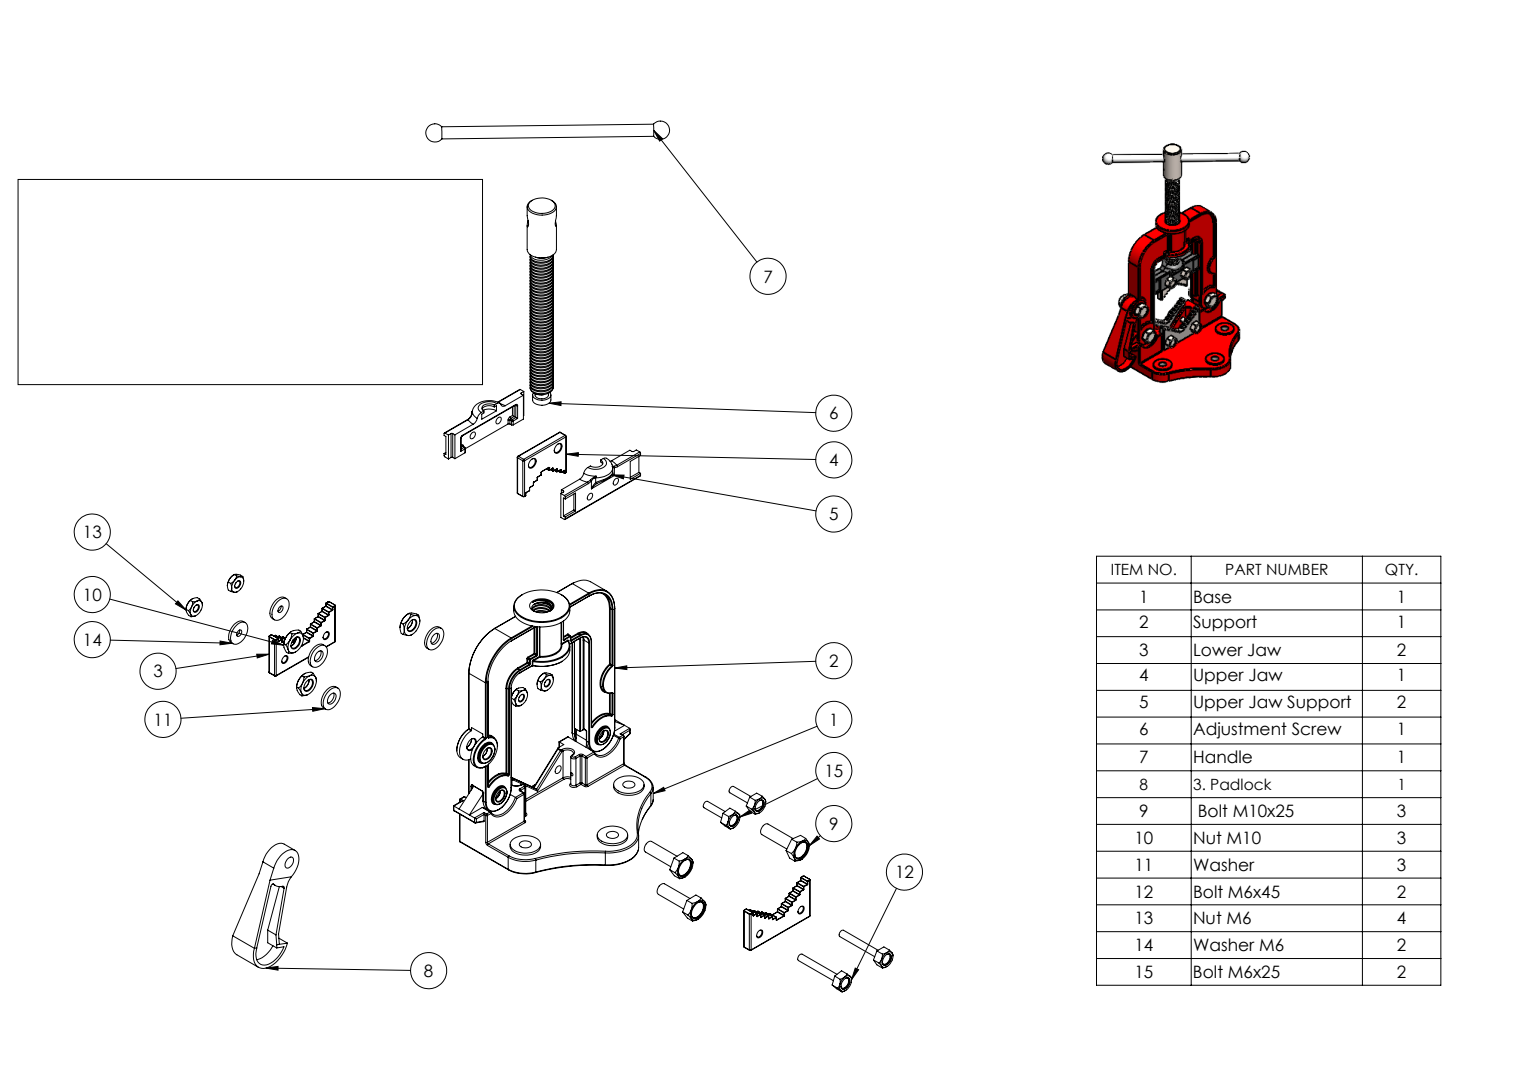
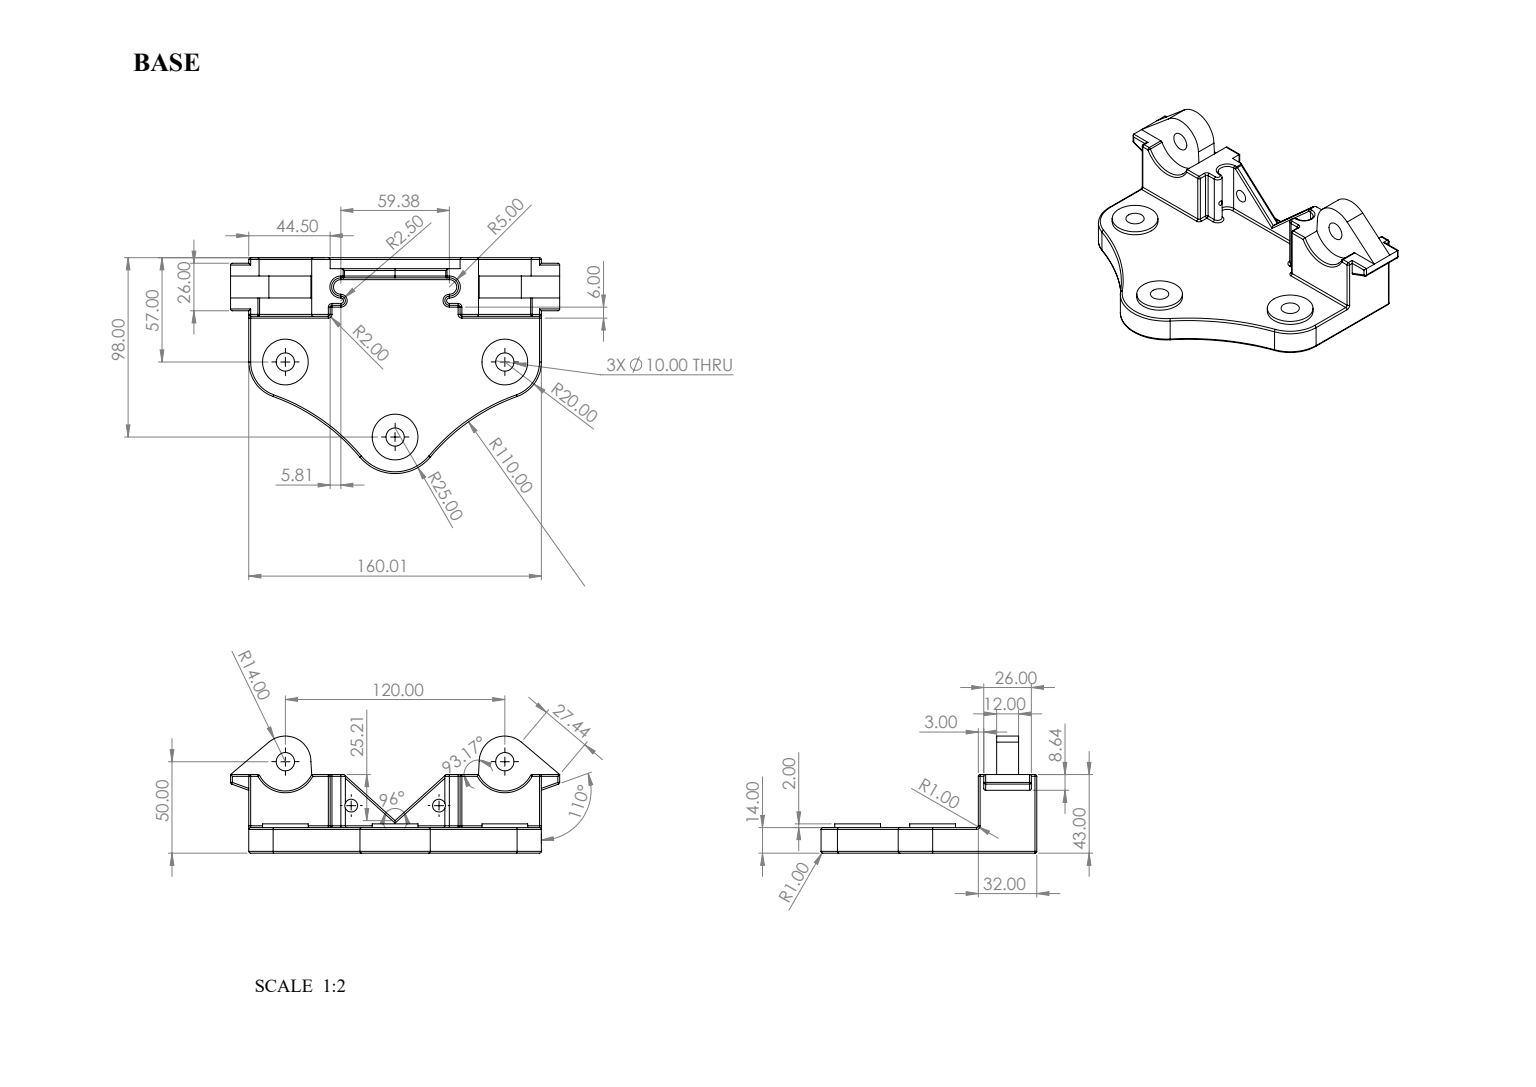
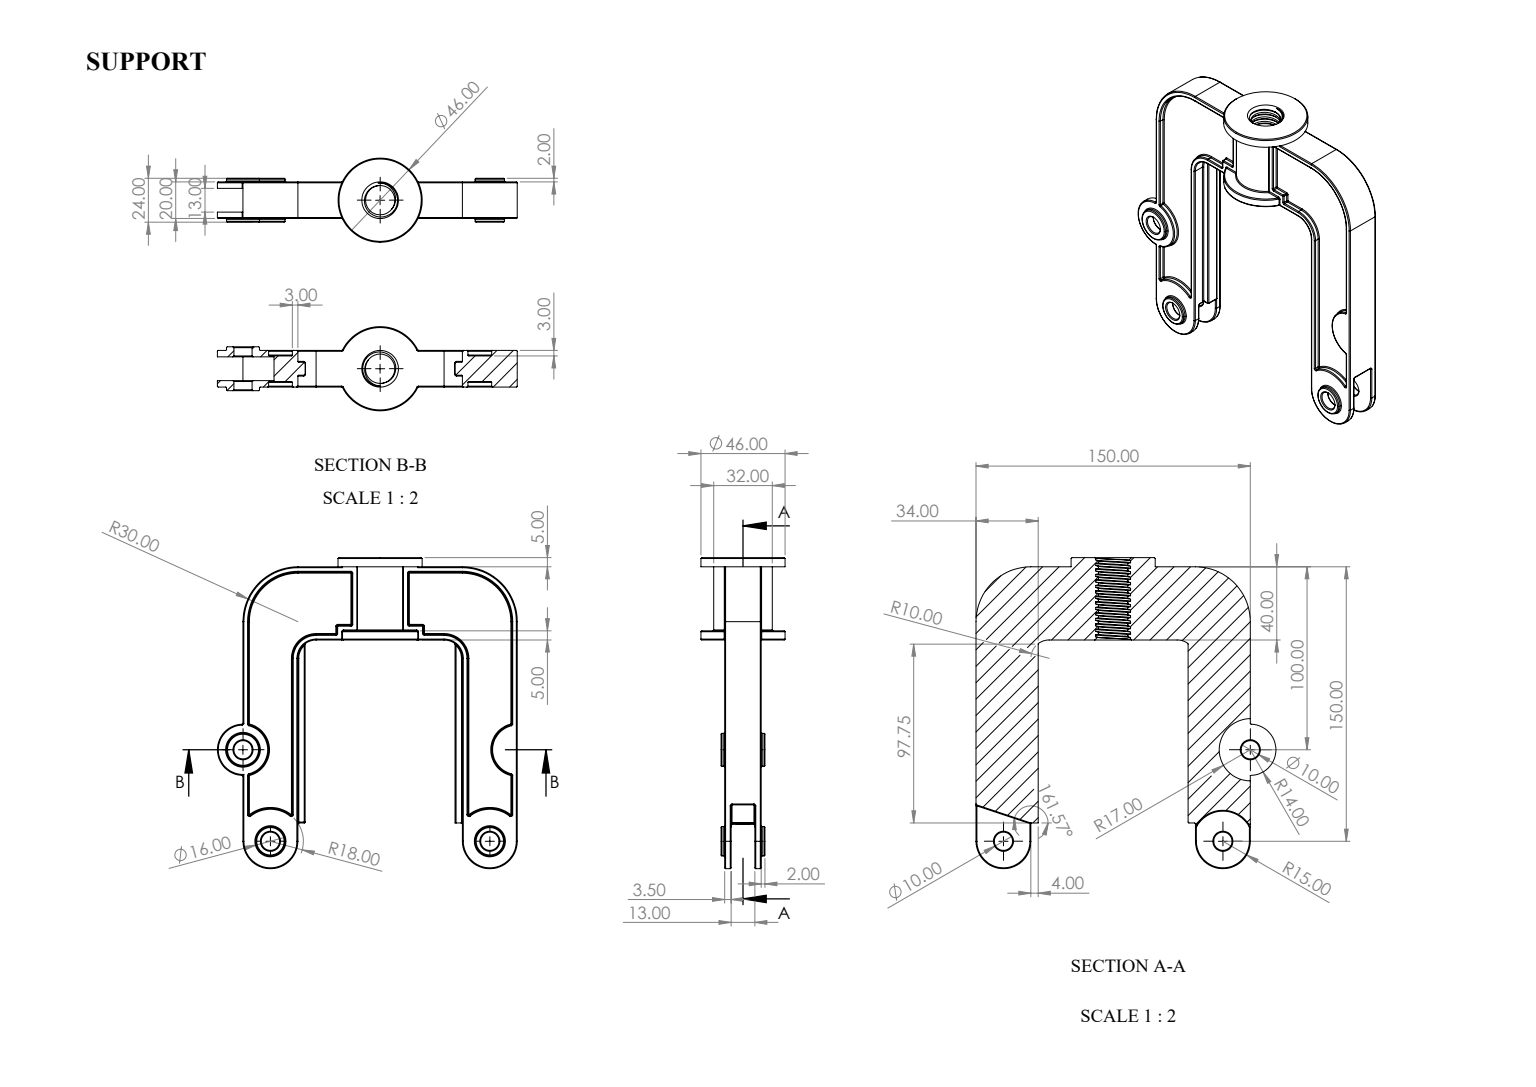
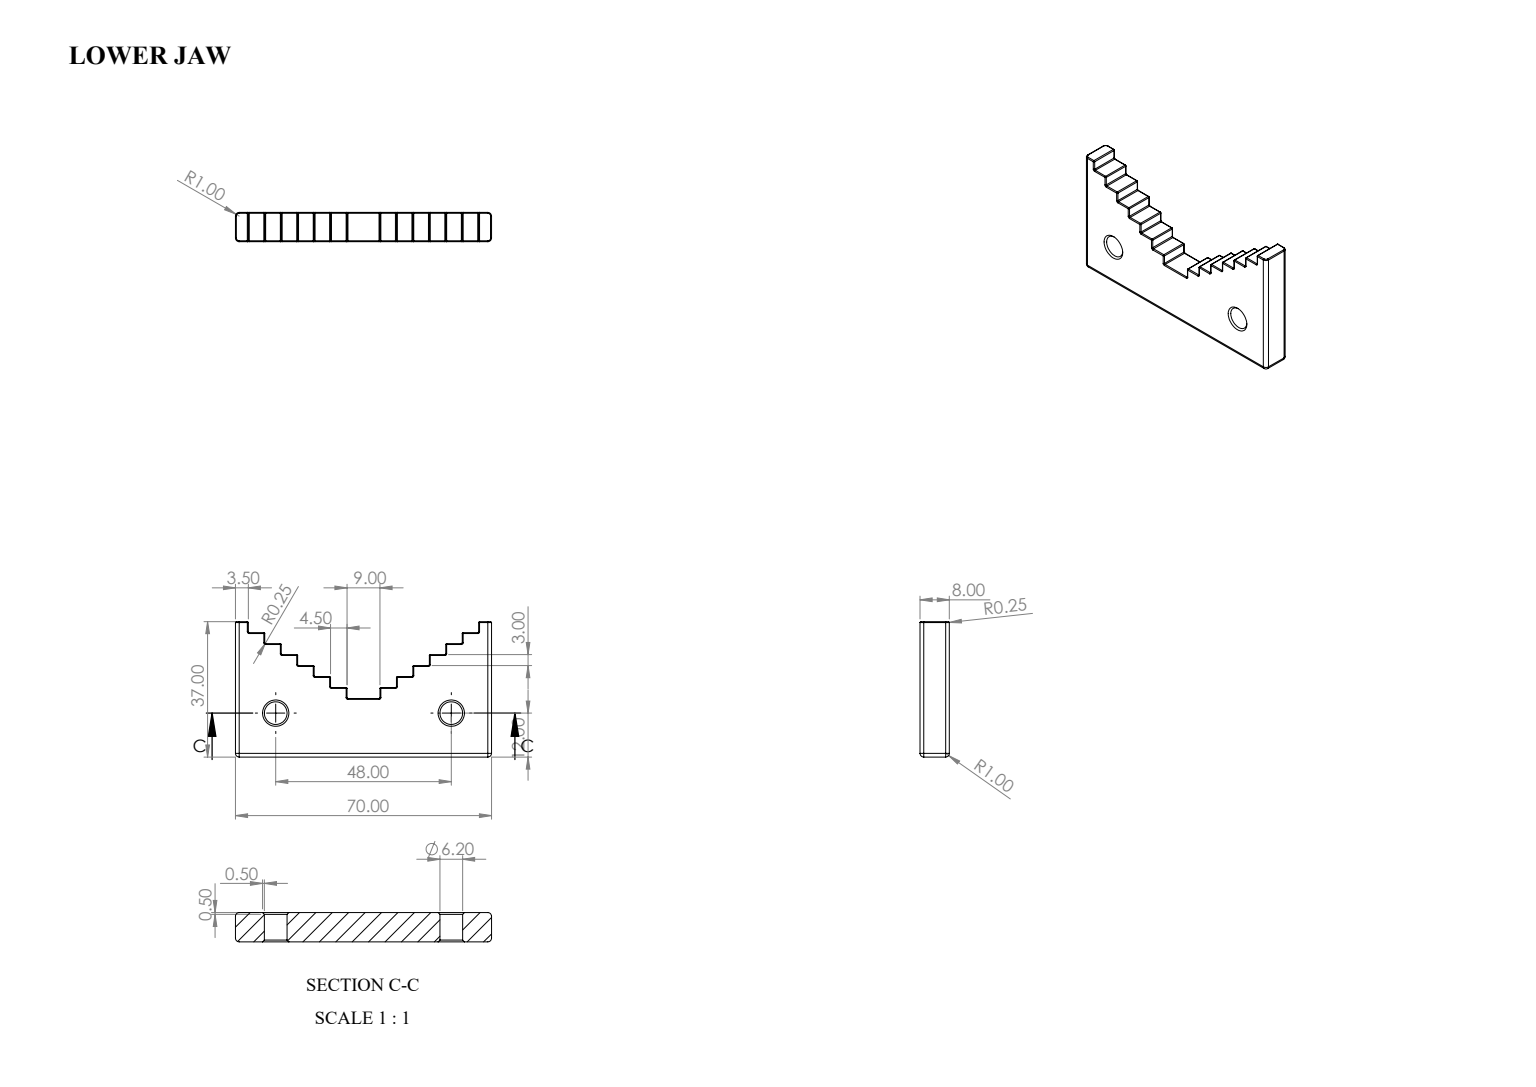
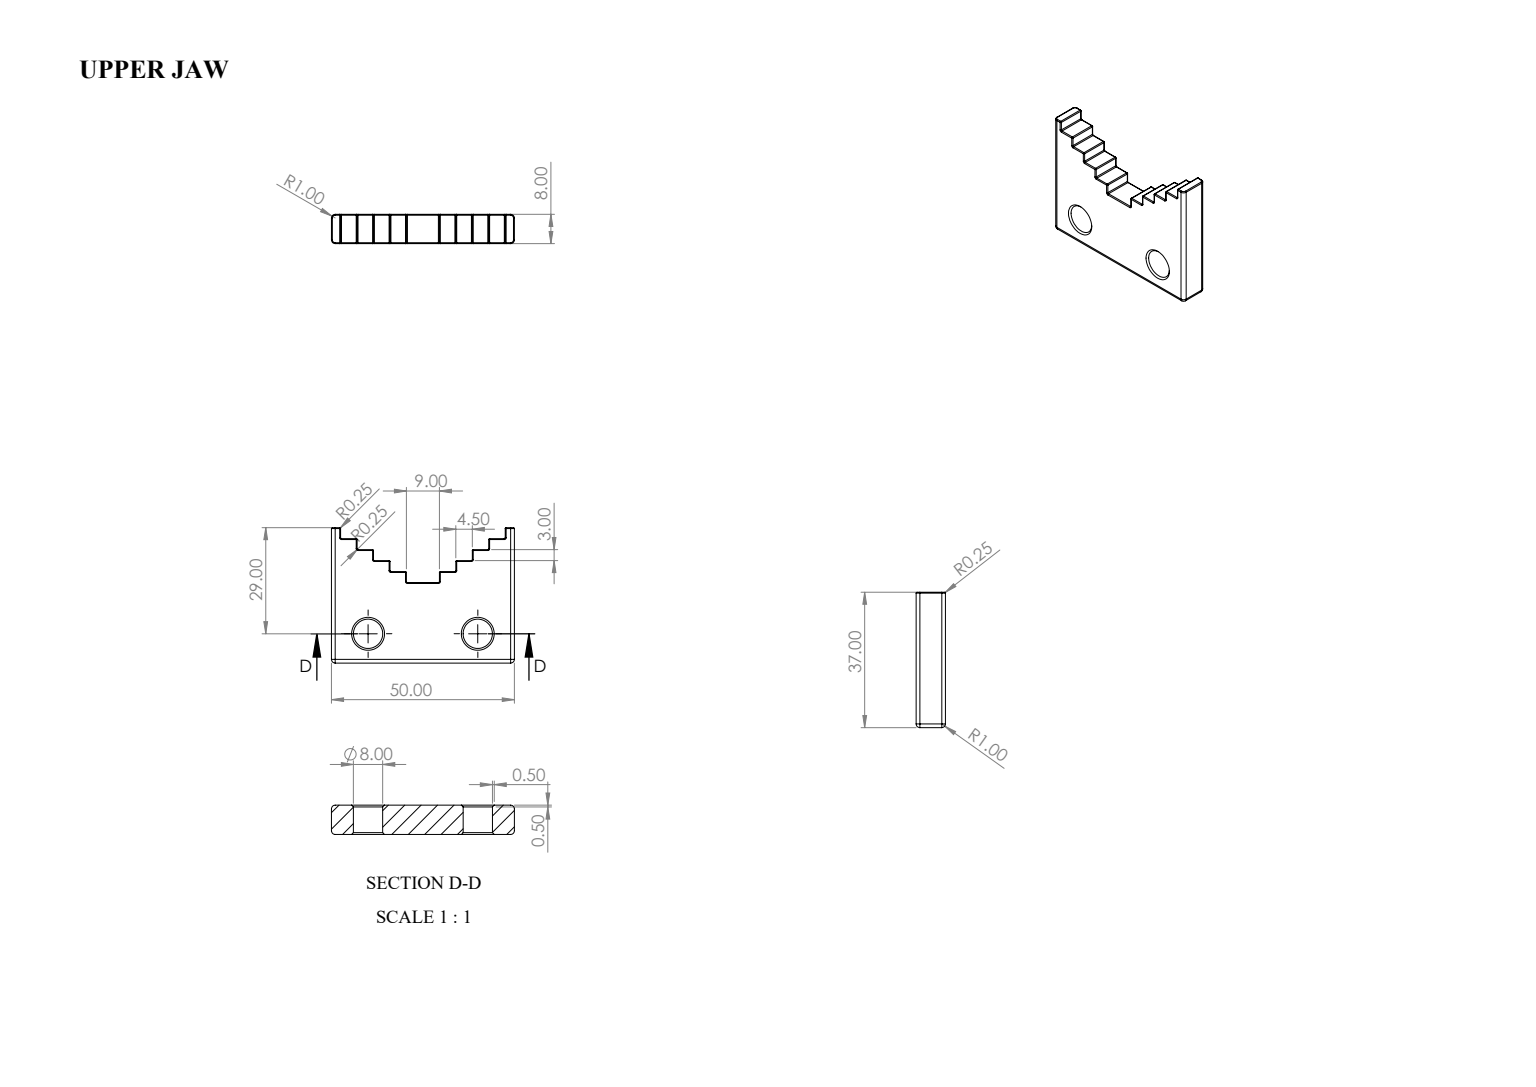
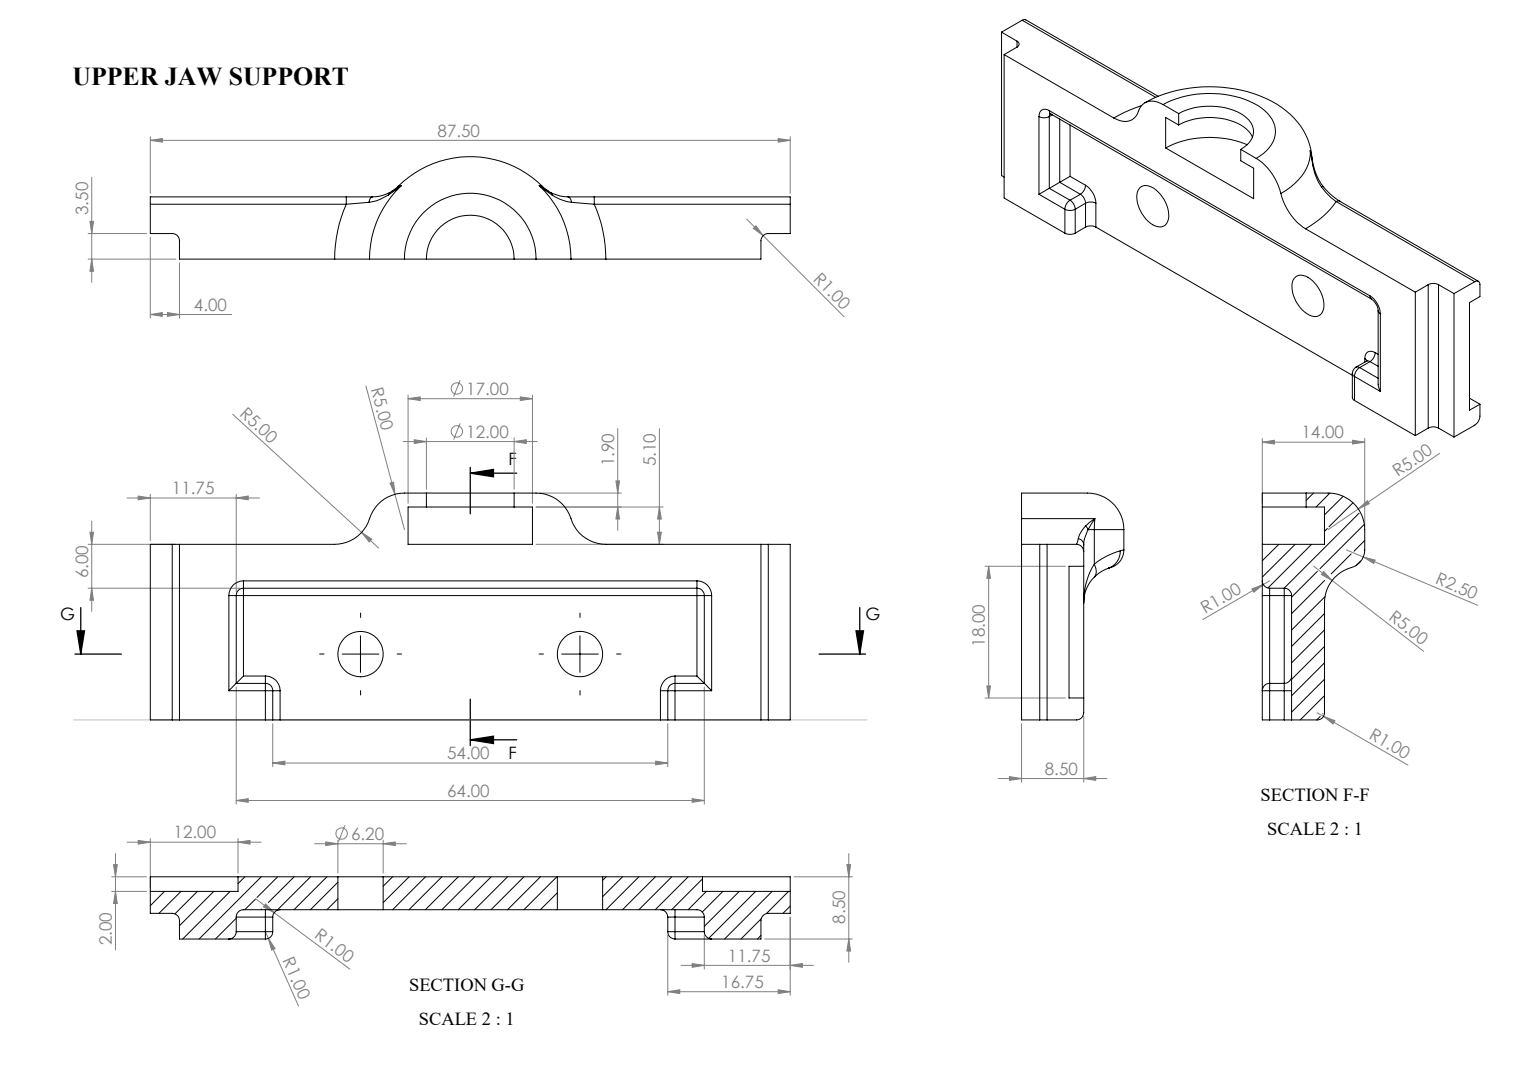
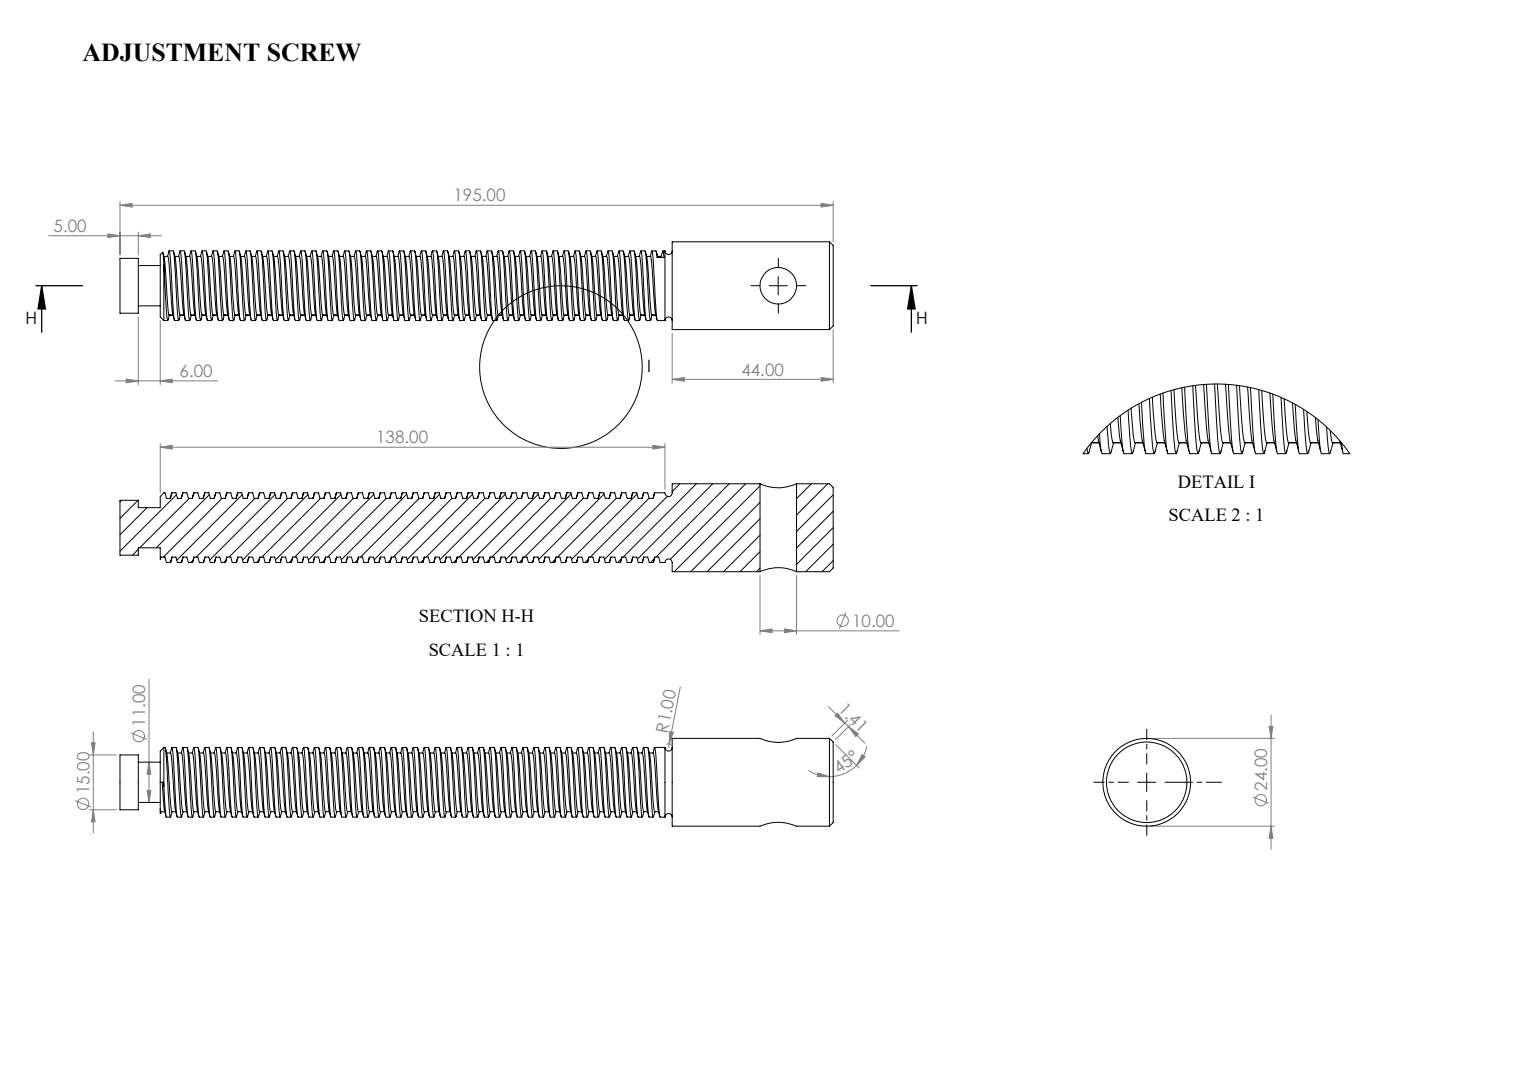
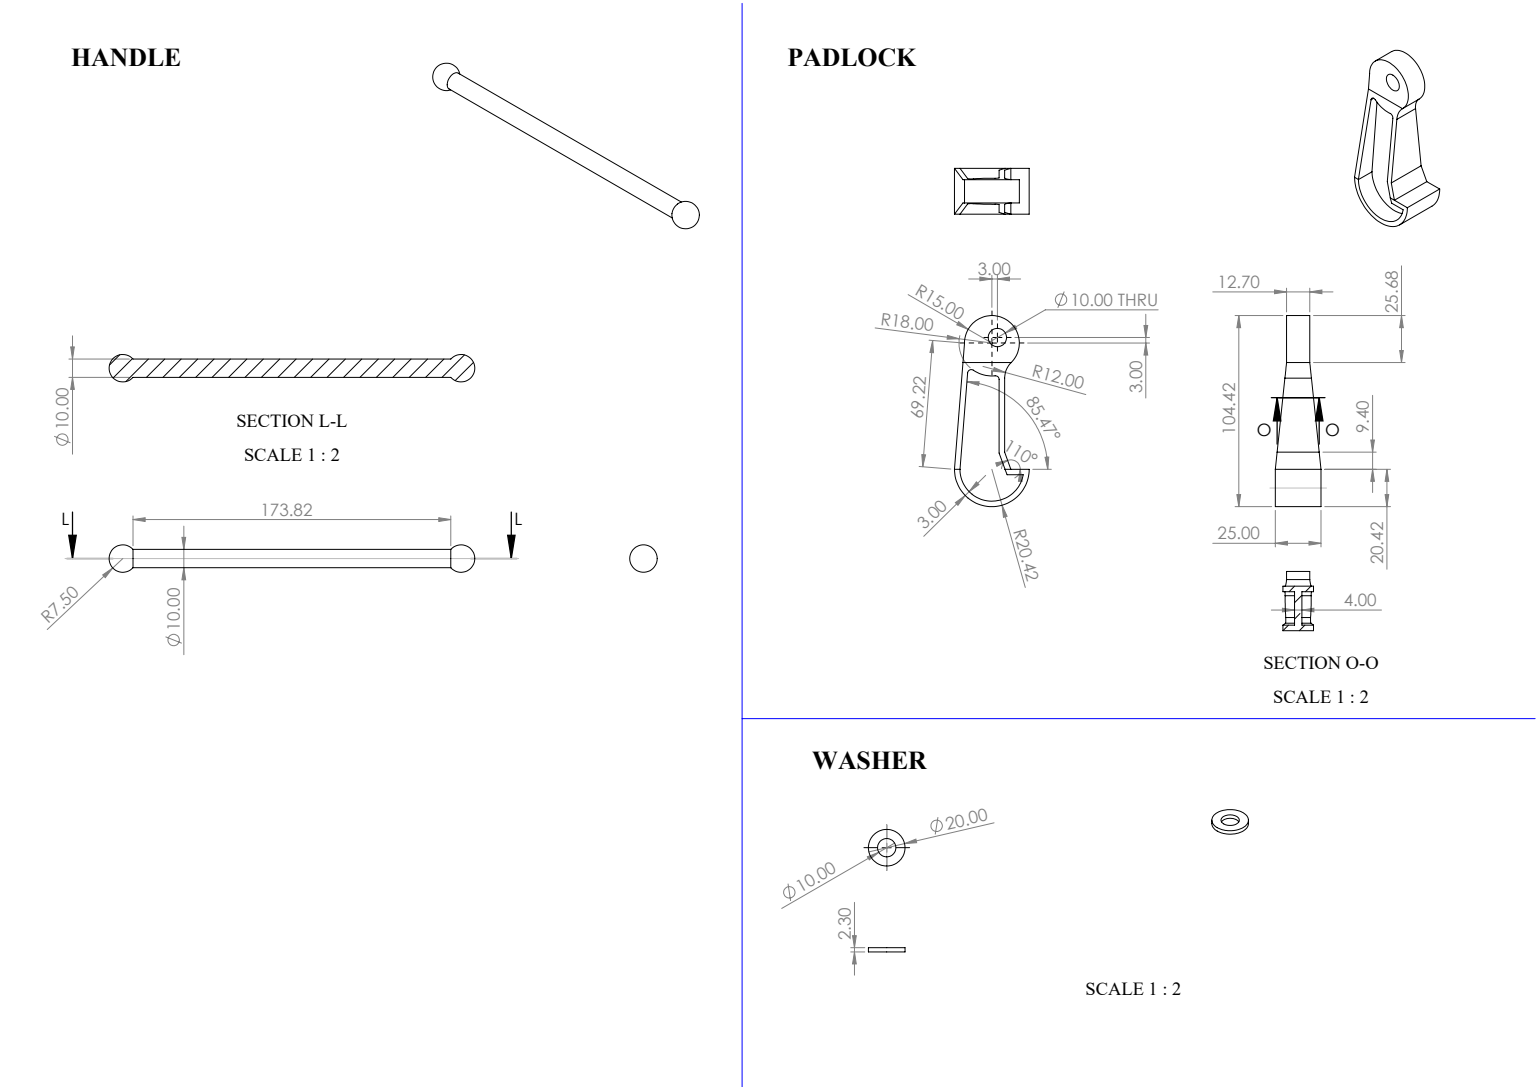
ISO-10303-21;
HEADER;
FILE_DESCRIPTION (('STEP AP214'),
    '1' );
FILE_NAME ('MAS-684',
    '2026-10-09T08:13:37',
    ( '' ),
    ( '' ),
    'SwSTEP 2.0',
    'SolidWorks 2021',
    '' );
FILE_SCHEMA (( 'AUTOMOTIVE_DESIGN' ));
ENDSEC;

DATA;
#1 = B_SPLINE_CURVE_WITH_KNOTS ( 'NONE', 3,
 ( #31451, #51902, #15336, #30765, #9698, #42087, #68086, #42425 ),
 .UNSPECIFIED., .F., .F.,
 ( 4, 2, 2, 4 ),
 ( 0.000000000000000000, 0.001617176559457151079, 0.002425764839185726510, 0.003234353118914302157 ),
 .UNSPECIFIED. ) ;
#2 = DIRECTION ( 'NONE',  ( 0.000000000000000000, -1.000000000000000000, 0.000000000000000000 ) ) ;
#3 = CIRCLE ( 'NONE', #24760, 5.000000000000004441 ) ;
#4 = EDGE_CURVE ( 'NONE', #67546, #44738, #50850, .T. ) ;
#5 = TOROIDAL_SURFACE ( 'NONE', #4527, 1.000000000000000000, 0.5000000000000000000 ) ;
#6 = DIRECTION ( 'NONE',  ( 1.000000000000000000, -0.000000000000000000, 0.000000000000000000 ) ) ;
#7 = CARTESIAN_POINT ( 'NONE',  ( 8.690363669209105524, -2.361802048420730493, 2.947848588679143234 ) ) ;
#8 =( LENGTH_UNIT ( ) NAMED_UNIT ( * ) SI_UNIT ( .MILLI., .METRE. ) );
#9 = ORIENTED_EDGE ( 'NONE', *, *, #4228, .F. ) ;
#10 = DIRECTION ( 'NONE',  ( 1.298988366203102052E-16, 0.05527174654752588928, 0.9984713486292864371 ) ) ;
#12 = EDGE_CURVE ( 'NONE', #66900, #26262, #59644, .T. ) ;
#11 = LINE ( 'NONE', #27826, #25683 ) ;
#13 = CARTESIAN_POINT ( 'NONE',  ( -99.50499999999996703, -6.826472737025115478, -4.959722759717899443 ) ) ;
#14 = ORIENTED_EDGE ( 'NONE', *, *, #46779, .F. ) ;
#15 = AXIS2_PLACEMENT_3D ( 'NONE', #14951, #52244, #34992 ) ;
#16 = PLANE ( 'NONE',  #47135 ) ;
#17 = CARTESIAN_POINT ( 'NONE',  ( -133.7070736234661865, -3.094860106618431139, -9.524999999999991473 ) ) ;
#18 = DIRECTION ( 'NONE',  ( 1.000000000000000000, 0.000000000000000000, 0.000000000000000000 ) ) ;
#19 = CARTESIAN_POINT ( 'NONE',  ( -65.45707362346617231, -9.058813317711329915, 2.943386871421371787 ) ) ;
#20 = PRESENTATION_LAYER_ASSIGNMENT (  '', '', ( #67473 ) ) ;
#21 = FACE_OUTER_BOUND ( 'NONE', #40498, .T. ) ;
#22 = ORIENTED_EDGE ( 'NONE', *, *, #11042, .T. ) ;
#23 = VECTOR ( 'NONE', #7321, 1000.000000000000000 ) ;
#25 = CARTESIAN_POINT ( 'NONE',  ( -71.49999999999998579, 64.07124727947029896, 7.000000000000000000 ) ) ;
#24 = CARTESIAN_POINT ( 'NONE',  ( -48.00000000000000000, 13.41640786499872284, -7.000000000000000000 ) ) ;
#26 = EDGE_CURVE ( 'NONE', #13502, #64475, #59831, .T. ) ;
#27 = CARTESIAN_POINT ( 'NONE',  ( -109.2549999999999955, -4.716976649647092401, 6.492361379858946790 ) ) ;
#28 = CARTESIAN_POINT ( 'NONE',  ( -5.598654528085806881, 124.7449999999999903, -7.705886871421374629 ) ) ;
#29 = CARTESIAN_POINT ( 'NONE',  ( -119.3949999999999676, -6.826472737025115478, -4.959722759717899443 ) ) ;
#30 = COLOUR_RGB ( '', 0.09019608, 0.27058824, 0.51372549) ;
#31 = DIRECTION ( 'NONE',  ( -9.376883653928687363E-17, -1.000000000000000000, 0.000000000000000000 ) ) ;
#32 = MECHANICAL_DESIGN_GEOMETRIC_PRESENTATION_REPRESENTATION (  '', ( #66376 ), #38375 ) ;
#34 = FACE_OUTER_BOUND ( 'NONE', #29836, .T. ) ;
#33 = DIRECTION ( 'NONE',  ( 0.000000000000000000, -0.000000000000000000, -1.000000000000000000 ) ) ;
#35 = EDGE_LOOP ( 'NONE', ( #36552, #43299, #63091, #34996 ) ) ;
#36 = CARTESIAN_POINT ( 'NONE',  ( -167.2429263765338305, 5.598654528085804216, 7.705886871421366635 ) ) ;
#37 =( LENGTH_UNIT ( ) NAMED_UNIT ( * ) SI_UNIT ( .MILLI., .METRE. ) );
#38 = CARTESIAN_POINT ( 'NONE',  ( -176.3949999999999818, -6.826472737025115478, -4.959722759717899443 ) ) ;
#39 = DIRECTION ( 'NONE',  ( -0.000000000000000000, 1.000000000000000000, -0.000000000000000000 ) ) ;
#40 = CARTESIAN_POINT ( 'NONE',  ( -47.09426399558999776, -13.61002330776443969, 0.8661849162379273714 ) ) ;
#41 = CARTESIAN_POINT ( 'NONE',  ( 39.74999999999999289, 18.74999999999997868, -3.750000000000000000 ) ) ;
#42 = CARTESIAN_POINT ( 'NONE',  ( 47.50000000000000000, 1.797044900979284448E-15, -9.500000000000000000 ) ) ;
#43 = ORIENTED_EDGE ( 'NONE', *, *, #36163, .F. ) ;
#44 = AXIS2_PLACEMENT_3D ( 'NONE', #13603, #53264, #52575 ) ;
#45 = CARTESIAN_POINT ( 'NONE',  ( -72.14292637653379359, 5.598654528085800663, -7.705886871421367523 ) ) ;
#46 = ADVANCED_FACE ( 'NONE', ( #69199 ), #64244, .F. ) ;
#47 = CARTESIAN_POINT ( 'NONE',  ( 5.000000000000000000, 6.123233995736766282E-16, 0.7500000000000000000 ) ) ;
#48 = FACE_OUTER_BOUND ( 'NONE', #30012, .T. ) ;
#49 = COLOUR_RGB ( '', 0.72549020, 0.75294118, 0.79215686) ;
#50 = VECTOR ( 'NONE', #19293, 1000.000000000000000 ) ;
#51 = CYLINDRICAL_SURFACE ( 'NONE', #37197, 1.000000000000000888 ) ;
#52 = CARTESIAN_POINT ( 'NONE',  ( -5.603568002170371543, -8.294335516573692502, 0.9848892659495209756 ) ) ;
#53 = CARTESIAN_POINT ( 'NONE',  ( -181.7050000000000125, 2.607480562269072433, 8.024999999999991473 ) ) ;
#54 = EDGE_LOOP ( 'NONE', ( #66784, #37211, #64174, #16099 ) ) ;
#55 = DIRECTION ( 'NONE',  ( 1.000000000000000000, -0.000000000000000000, -1.300977106640434891E-16 ) ) ;
#56 = FILL_AREA_STYLE ('',( #48034 ) ) ;
#57 = CIRCLE ( 'NONE', #46222, 13.49999999999999822 ) ;
#58 =( NAMED_UNIT ( * ) SI_UNIT ( $, .STERADIAN. ) SOLID_ANGLE_UNIT ( ) );
#59 = VECTOR ( 'NONE', #65967, 1000.000000000000000 ) ;
#60 = DIRECTION ( 'NONE',  ( 0.000000000000000000, 0.000000000000000000, 1.000000000000000000 ) ) ;
#61 = CARTESIAN_POINT ( 'NONE',  ( 2.607480562269071989, 140.7070736234661581, 8.025000000000002132 ) ) ;
#62 = AXIS2_PLACEMENT_3D ( 'NONE', #27613, #39267, #7568 ) ;
#63 = ORIENTED_EDGE ( 'NONE', *, *, #14885, .F. ) ;
#64 = DIRECTION ( 'NONE',  ( 0.000000000000000000, 0.000000000000000000, -1.000000000000000000 ) ) ;
#65 = CARTESIAN_POINT ( 'NONE',  ( -91.85499999999998977, 4.716976649647094177, 6.492361379858945902 ) ) ;
#66 = VECTOR ( 'NONE', #60751, 1000.000000000000000 ) ;
#67 = FILL_AREA_STYLE ('',( #15655 ) ) ;
#68 = EDGE_LOOP ( 'NONE', ( #29117, #12517, #42805, #36614 ) ) ;
#69 =( NAMED_UNIT ( * ) SI_UNIT ( $, .STERADIAN. ) SOLID_ANGLE_UNIT ( ) );
#70 = DIRECTION ( 'NONE',  ( -1.000000000000000000, 0.000000000000000000, 0.000000000000000000 ) ) ;
#71 =( NAMED_UNIT ( * ) SI_UNIT ( $, .STERADIAN. ) SOLID_ANGLE_UNIT ( ) );
#72 = ADVANCED_FACE ( 'NONE', ( #68858 ), #63563, .T. ) ;
#73 = FACE_OUTER_BOUND ( 'NONE', #54146, .T. ) ;
#74 = ORIENTED_EDGE ( 'NONE', *, *, #39587, .T. ) ;
#75 = SURFACE_SIDE_STYLE ('',( #32169 ) ) ;
#76 = CARTESIAN_POINT ( 'NONE',  ( -65.54499999999998749, -7.632228543268600340, -2.479861379858950166 ) ) ;
#77 = EDGE_LOOP ( 'NONE', ( #67985, #68623, #51580, #57239 ) ) ;
#78 = VECTOR ( 'NONE', #42057, 1000.000000000000000 ) ;
#79 = SURFACE_STYLE_FILL_AREA ( #11398 ) ;
#80 = LINE ( 'NONE', #20219, #38004 ) ;
#81 = CARTESIAN_POINT ( 'NONE',  ( 2.999999999999990230, 5.000000000000000000, 37.00402776293829277 ) ) ;
#82 = ORIENTED_EDGE ( 'NONE', *, *, #21496, .T. ) ;
#83 = SURFACE_STYLE_FILL_AREA ( #58559 ) ;
#84 = EDGE_LOOP ( 'NONE', ( #18925, #54897, #57059, #45162 ) ) ;
#85 = CIRCLE ( 'NONE', #4622, 3.000000000000000444 ) ;
#87 = ADVANCED_FACE ( 'NONE', ( #15409 ), #58281, .T. ) ;
#86 =( LENGTH_UNIT ( ) NAMED_UNIT ( * ) SI_UNIT ( .MILLI., .METRE. ) );
#88 = CARTESIAN_POINT ( 'NONE',  ( -127.2550000000000097, -4.716976649647092401, 6.492361379858946790 ) ) ;
#89 = ORIENTED_EDGE ( 'NONE', *, *, #8280, .T. ) ;
#90 = CARTESIAN_POINT ( 'NONE',  ( 31.64575850060272089, 42.77450856510287025, -45.47201648568074006 ) ) ;
#91 = EDGE_LOOP ( 'NONE', ( #34667, #18919, #19506, #38504 ) ) ;
#92 = DIRECTION ( 'NONE',  ( 0.000000000000000000, 0.000000000000000000, -1.000000000000000000 ) ) ;
#93 = CARTESIAN_POINT ( 'NONE',  ( 71.50000000000000000, 14.49137674618942562, -7.000000000000000000 ) ) ;
#94 = DIRECTION ( 'NONE',  ( 1.000000000000000000, 0.000000000000000000, 0.000000000000000000 ) ) ;
#95 = CARTESIAN_POINT ( 'NONE',  ( -162.5070736234661979, 8.102448949553176405, 5.886773742842740909 ) ) ;
#96 = EDGE_CURVE ( 'NONE', #24376, #48365, #62535, .T. ) ;
#97 = CARTESIAN_POINT ( 'NONE',  ( 3.094860106618431583, 126.0949999999999847, 9.525000000000000355 ) ) ;
#98 =( BOUNDED_CURVE ( )  B_SPLINE_CURVE ( 2, ( #68533, #63250, #15098, #47110, #57988, #9804, #31215, #52708, #25942 ),
 .UNSPECIFIED., .F., .F. ) 
 B_SPLINE_CURVE_WITH_KNOTS ( ( 3, 2, 2, 2, 3 ),
 ( 0.01408042836260392332, 0.01521739130434775211, 0.01739130434782587206, 0.01956521739130399548, 0.02173913043478211196 ),
 .UNSPECIFIED. ) 
 CURVE ( )  GEOMETRIC_REPRESENTATION_ITEM ( )  RATIONAL_B_SPLINE_CURVE ( ( 0.9755800536518706156, 0.9744024134823617844, 1.000000000000000000, 0.9510565162951535312, 1.000000000000000000, 0.9510565162951535312, 1.000000000000000000, 0.9510565162951647444, 0.9999999999999887867 ) ) 
 REPRESENTATION_ITEM ( '' )  );
#99 = CARTESIAN_POINT ( 'NONE',  ( -92.45707362346617231, -9.058813317711329915, 2.943386871421371787 ) ) ;
#100 = AXIS2_PLACEMENT_3D ( 'NONE', #41019, #61382, #57148 ) ;
#101 = EDGE_CURVE ( 'NONE', #11552, #53103, #65288, .T. ) ;
#102 = VECTOR ( 'NONE', #57920, 1000.000000000000000 ) ;
#103 = CARTESIAN_POINT ( 'NONE',  ( 0.000000000000000000, 154.4258142642185305, -9.450814264218562855 ) ) ;
#104 = ORIENTED_EDGE ( 'NONE', *, *, #55820, .T. ) ;
#107 = STYLED_ITEM ( 'NONE', ( #51157 ), #11664 ) ;
#106 = SURFACE_STYLE_USAGE ( .BOTH. , #32519 ) ;
#105 = CARTESIAN_POINT ( 'NONE',  ( 15.98999599679679839, 118.4999999999999716, -9.500000000000000000 ) ) ;
#108 = EDGE_CURVE ( 'NONE', #11830, #36200, #38610, .T. ) ;
#109 = CARTESIAN_POINT ( 'NONE',  ( -139.8550000000000182, 4.716976649647094177, 6.492361379858945902 ) ) ;
#110 = CARTESIAN_POINT ( 'NONE',  ( -86.15707362346617515, -9.058813317711329915, -2.943386871421370898 ) ) ;
#111 = COLOUR_RGB ( '', 0.31764706, 0.68627451, 0.89019608) ;
#112 = CARTESIAN_POINT ( 'NONE',  ( -141.5950000000000273, 2.607480562269073321, 8.024999999999991473 ) ) ;
#113 = CARTESIAN_POINT ( 'NONE',  ( -142.0449999999999875, 7.632228543268600340, 2.479861379858949277 ) ) ;
#114 = MECHANICAL_DESIGN_GEOMETRIC_PRESENTATION_REPRESENTATION (  '', ( #15946 ), #36167 ) ;
#115 = ORIENTED_EDGE ( 'NONE', *, *, #22584, .F. ) ;
#116 = AXIS2_PLACEMENT_3D ( 'NONE', #7910, #46285, #57492 ) ;
#117 = CARTESIAN_POINT ( 'NONE',  ( 44.47787316461994322, 9.825957721539964496, -3.000913084730224334 ) ) ;
#118 = LINE ( 'NONE', #36494, #27806 ) ;
#119 = SURFACE_STYLE_USAGE ( .BOTH. , #59618 ) ;
#120 = UNCERTAINTY_MEASURE_WITH_UNIT (LENGTH_MEASURE( 1.000000000000000082E-05 ), #23829, 'distance_accuracy_value', 'NONE');
#121 = CARTESIAN_POINT ( 'NONE',  ( -52.85499999999998266, 4.716976649647094177, 6.492361379858945902 ) ) ;
#122 = CARTESIAN_POINT ( 'NONE',  ( -74.50000000000000000, 7.768687147774684831, 6.500000000000000000 ) ) ;
#123 = CIRCLE ( 'NONE', #49622, 13.99999999999999822 ) ;
#124 = CARTESIAN_POINT ( 'NONE',  ( -56.24499999999999034, -4.716976649647093289, -6.492361379858945902 ) ) ;
#125 = TOROIDAL_SURFACE ( 'NONE', #45179, 0.5000000000000000000, 0.2500000000000000000 ) ;
#126 = CARTESIAN_POINT ( 'NONE',  ( 3.094860106618435136, 161.4050000000000296, -9.525000000000000355 ) ) ;
#127 = DIRECTION ( 'NONE',  ( -1.189524669241239115E-16, -1.000000000000000000, -0.000000000000000000 ) ) ;
#128 = AXIS2_PLACEMENT_3D ( 'NONE', #2627, #68021, #19809 ) ;
#129 = CARTESIAN_POINT ( 'NONE',  ( -5.603096392576914830, -1.514639124457109354, 8.295152368350901639 ) ) ;
#130 = UNCERTAINTY_MEASURE_WITH_UNIT (LENGTH_MEASURE( 1.000000000000000082E-05 ), #4411, 'distance_accuracy_value', 'NONE');
#131 = CARTESIAN_POINT ( 'NONE',  ( -108.1429263765338078, 5.598654528085800663, -7.705886871421367523 ) ) ;
#132 = DIRECTION ( 'NONE',  ( -5.775339657480442461E-17, 1.000000000000000000, 4.528264053928432625E-17 ) ) ;
#133 = FILL_AREA_STYLE_COLOUR ( '', #46192 ) ;
#134 = VECTOR ( 'NONE', #49583, 1000.000000000000000 ) ;
#135 = CARTESIAN_POINT ( 'NONE',  ( -89.30707362346616662, -10.01517768586948698, 6.132527647946031529E-16 ) ) ;
#136 = DIRECTION ( 'NONE',  ( -1.000000000000000000, 0.000000000000000000, 0.000000000000000000 ) ) ;
#137 = AXIS2_PLACEMENT_3D ( 'NONE', #11267, #39426, #17620 ) ;
#138 = CYLINDRICAL_SURFACE ( 'NONE', #6916, 0.2500000000000002220 ) ;
#139 = DIRECTION ( 'NONE',  ( -1.000000000000000000, 0.000000000000000000, 0.000000000000000000 ) ) ;
#140 =( NAMED_UNIT ( * ) PLANE_ANGLE_UNIT ( ) SI_UNIT ( $, .RADIAN. ) );
#141 = ORIENTED_EDGE ( 'NONE', *, *, #12867, .F. ) ;
#142 = DIRECTION ( 'NONE',  ( 0.000000000000000000, -1.000000000000000000, 0.000000000000000000 ) ) ;
#143 = CARTESIAN_POINT ( 'NONE',  ( -8.437984349512095861, 109.8070736234661666, -5.166775262442723748E-16 ) ) ;
#144 = AXIS2_PLACEMENT_3D ( 'NONE', #47269, #4995, #63405 ) ;
#145 = AXIS2_PLACEMENT_3D ( 'NONE', #37722, #53827, #52228 ) ;
#146 = CARTESIAN_POINT ( 'NONE',  ( 75.00000000000000000, 19.97932849626359442, -6.162720495828226674 ) ) ;
#147 = VECTOR ( 'NONE', #29815, 1000.000000000000000 ) ;
#148 = FILL_AREA_STYLE ('',( #5466 ) ) ;
#149 = VERTEX_POINT ( 'NONE', #38256 ) ;
#150 = ORIENTED_EDGE ( 'NONE', *, *, #13034, .F. ) ;
#151 = DIRECTION ( 'NONE',  ( -1.000000000000000000, 0.000000000000000000, 0.000000000000000000 ) ) ;
#152 =( NAMED_UNIT ( * ) SI_UNIT ( $, .STERADIAN. ) SOLID_ANGLE_UNIT ( ) );
#153 = PLANE ( 'NONE',  #33814 ) ;
#154 = ORIENTED_EDGE ( 'NONE', *, *, #42387, .F. ) ;
#155 = CARTESIAN_POINT ( 'NONE',  ( -9.058813317711338797, 132.4549999999999841, 2.943386871421373563 ) ) ;
#156 =( LENGTH_UNIT ( ) NAMED_UNIT ( * ) SI_UNIT ( .MILLI., .METRE. ) );
#157 = EDGE_CURVE ( 'NONE', #21970, #6242, #4359, .T. ) ;
#158 = AXIS2_PLACEMENT_3D ( 'NONE', #18232, #49917, #34060 ) ;
#159 = LINE ( 'NONE', #54035, #22728 ) ;
#160 = CARTESIAN_POINT ( 'NONE',  ( -103.0449999999999875, 7.632228543268600340, 2.479861379858949277 ) ) ;
#161 = ORIENTED_EDGE ( 'NONE', *, *, #21267, .T. ) ;
#162 = EDGE_CURVE ( 'NONE', #36655, #50552, #43525, .T. ) ;
#163 =( GEOMETRIC_REPRESENTATION_CONTEXT ( 3 ) GLOBAL_UNCERTAINTY_ASSIGNED_CONTEXT ( ( #7392 ) ) GLOBAL_UNIT_ASSIGNED_CONTEXT ( ( #22652, #18065, #24030 ) ) REPRESENTATION_CONTEXT ( 'NONE', 'WORKASPACE' ) );
#164 = SPHERICAL_SURFACE ( 'NONE', #64743, 0.2500000000000000000 ) ;
#165 = CARTESIAN_POINT ( 'NONE',  ( -60.00000000000000000, -2.024042244987997205E-14, -11.50000000000000000 ) ) ;
#166 = ORIENTED_EDGE ( 'NONE', *, *, #34857, .T. ) ;
#167 = CARTESIAN_POINT ( 'NONE',  ( 98.00000000000000000, 5.000000000000000000, 0.000000000000000000 ) ) ;
#168 = SURFACE_STYLE_FILL_AREA ( #63900 ) ;
#169 = EDGE_CURVE ( 'NONE', #40912, #47500, #6890, .T. ) ;
#170 =( LENGTH_UNIT ( ) NAMED_UNIT ( * ) SI_UNIT ( .MILLI., .METRE. ) );
#171 =( GEOMETRIC_REPRESENTATION_CONTEXT ( 3 ) GLOBAL_UNCERTAINTY_ASSIGNED_CONTEXT ( ( #48298 ) ) GLOBAL_UNIT_ASSIGNED_CONTEXT ( ( #9974, #68031, #14535 ) ) REPRESENTATION_CONTEXT ( 'NONE', 'WORKASPACE' ) );
#172 = FACE_OUTER_BOUND ( 'NONE', #8225, .T. ) ;
#173 = EDGE_CURVE ( 'NONE', #4422, #21622, #52492, .T. ) ;
#174 = VECTOR ( 'NONE', #68890, 1000.000000000000114 ) ;
#175 = ADVANCED_BREP_SHAPE_REPRESENTATION ( '', ( #4071, #42840 ), #64177 ) ;
#176 = CARTESIAN_POINT ( 'NONE',  ( 20.03861782943699765, 115.4999999895429994, -10.00000000000000000 ) ) ;
#177 = EDGE_CURVE ( 'NONE', #27373, #65754, #48012, .T. ) ;
#178 = ORIENTED_EDGE ( 'NONE', *, *, #22736, .F. ) ;
#179 = CARTESIAN_POINT ( 'NONE',  ( -165.8070736234661808, 10.01517768586948698, -1.839758294383808966E-15 ) ) ;
#180 = PLANE ( 'NONE',  #48189 ) ;
#181 = DIRECTION ( 'NONE',  ( -1.000000000000000000, 0.000000000000000000, 0.000000000000000000 ) ) ;
#182 = CARTESIAN_POINT ( 'NONE',  ( 57.00000000000000000, 16.00000000000000000, 47.50402776293824303 ) ) ;
#183 = DIRECTION ( 'NONE',  ( -1.000000000000000000, -0.000000000000000000, -0.000000000000000000 ) ) ;
#184 = CARTESIAN_POINT ( 'NONE',  ( 7.249999999999999112, 8.878689293818310074E-16, 0.7500000000000000000 ) ) ;
#185 = DIRECTION ( 'NONE',  ( -1.000000000000000000, 0.000000000000000000, 0.000000000000000000 ) ) ;
#186 = EDGE_CURVE ( 'NONE', #21243, #60834, #11121, .T. ) ;
#187 = DIRECTION ( 'NONE',  ( -1.445602896647337931E-16, 1.000000000000000000, 0.000000000000000000 ) ) ;
#188 = CARTESIAN_POINT ( 'NONE',  ( -9.827790563157511022E-16, 121.4429263765338050, 8.025000000000000355 ) ) ;
#189 = CARTESIAN_POINT ( 'NONE',  ( -2.652578976365682184, 154.0340937016761984, 8.678865135533699871 ) ) ;
#190 = ORIENTED_EDGE ( 'NONE', *, *, #17439, .F. ) ;
#191 = AXIS2_PLACEMENT_3D ( 'NONE', #1829, #61641, #18072 ) ;
#192 = ORIENTED_EDGE ( 'NONE', *, *, #68046, .T. ) ;
#193 = CARTESIAN_POINT ( 'NONE',  ( -49.55707362346617373, -1.166476076187852838E-15, -9.524999999999991473 ) ) ;
#194 = FACE_BOUND ( 'NONE', #69314, .T. ) ;
#195 = DIRECTION ( 'NONE',  ( 1.000000000000000000, 0.000000000000000000, 0.000000000000000000 ) ) ;
#196 = SURFACE_STYLE_USAGE ( .BOTH. , #38639 ) ;
#197 = VERTEX_POINT ( 'NONE', #32571 ) ;
#198 = SURFACE_SIDE_STYLE ('',( #59328 ) ) ;
#199 = CARTESIAN_POINT ( 'NONE',  ( -166.1049999999999898, -6.826472737025115478, 4.959722759717900331 ) ) ;
#200 = CARTESIAN_POINT ( 'NONE',  ( 52.99999999999999289, 27.99999999999998579, 3.750000000000000000 ) ) ;
#201 = CARTESIAN_POINT ( 'NONE',  ( -147.5070736234661695, 8.102448949553176405, 5.886773742842740909 ) ) ;
#202 = CARTESIAN_POINT ( 'NONE',  ( -176.6949999999999363, -8.437984349512085203, 5.166775262442717831E-16 ) ) ;
#203 = CARTESIAN_POINT ( 'NONE',  ( -162.8949999999999534, 6.826472737025115478, 4.959722759717899443 ) ) ;
#204 = EDGE_LOOP ( 'NONE', ( #41831, #44506, #36977, #5553, #63644 ) ) ;
#205 = FILL_AREA_STYLE_COLOUR ( '', #39242 ) ;
#206 = CARTESIAN_POINT ( 'NONE',  ( -83.60499999999998977, 6.826472737025113702, -4.959722759717902107 ) ) ;
#207 = CARTESIAN_POINT ( 'NONE',  ( 98.00000000000000000, 16.00000000000000000, 0.000000000000000000 ) ) ;
#208 = SURFACE_STYLE_USAGE ( .BOTH. , #48512 ) ;
#209 = AXIS2_PLACEMENT_3D ( 'NONE', #26533, #25492, #41365 ) ;
#210 = CARTESIAN_POINT ( 'NONE',  ( -75.01496064257371188, 35.97861232747153082, -9.531191624918911032 ) ) ;
#211 = CARTESIAN_POINT ( 'NONE',  ( -76.94499999999997897, -9.827790563157499189E-16, -8.024999999999991473 ) ) ;
#212 = CARTESIAN_POINT ( 'NONE',  ( 9.058813317711338797, 133.9549999999999841, -2.943386871421372675 ) ) ;
#213 = PRESENTATION_LAYER_ASSIGNMENT (  '', '', ( #51963 ) ) ;
#214 = CARTESIAN_POINT ( 'NONE',  ( 8.082903768654762899, -1.269775441351268174E-15, 1.082903768654759125 ) ) ;
#215 = DIRECTION ( 'NONE',  ( 4.336808689941999001E-16, -1.000000000000000000, -0.000000000000000000 ) ) ;
#216 = DIRECTION ( 'NONE',  ( 1.000000000000000000, 0.000000000000000000, -0.000000000000000000 ) ) ;
#217 = UNCERTAINTY_MEASURE_WITH_UNIT (LENGTH_MEASURE( 1.000000000000000082E-05 ), #32735, 'distance_accuracy_value', 'NONE');
#218 = EDGE_CURVE ( 'NONE', #1575, #11319, #54033, .T. ) ;
#219 =( LENGTH_UNIT ( ) NAMED_UNIT ( * ) SI_UNIT ( .MILLI., .METRE. ) );
#220 = ORIENTED_EDGE ( 'NONE', *, *, #67345, .F. ) ;
#221 = CARTESIAN_POINT ( 'NONE',  ( -71.75000000000000000, -3.000000000000000000, 19.00000000000000000 ) ) ;
#222 =( LENGTH_UNIT ( ) NAMED_UNIT ( * ) SI_UNIT ( .MILLI., .METRE. ) );
#223 = COLOUR_RGB ( '', 0.09019608, 0.27058824, 0.51372549) ;
#224 = DIRECTION ( 'NONE',  ( -0.000000000000000000, 0.000000000000000000, -1.000000000000000000 ) ) ;
#225 = AXIS2_PLACEMENT_3D ( 'NONE', #1591, #39312, #61408 ) ;
#226 = CARTESIAN_POINT ( 'NONE',  ( -9.827790563157511022E-16, 137.5570736234661808, 8.025000000000000355 ) ) ;
#227 = ORIENTED_EDGE ( 'NONE', *, *, #43634, .F. ) ;
#228 = ORIENTED_EDGE ( 'NONE', *, *, #50580, .F. ) ;
#229 = CARTESIAN_POINT ( 'NONE',  ( -6.826472737025120807, 135.9929263765338021, 4.959722759717906548 ) ) ;
#230 = DIRECTION ( 'NONE',  ( 1.000000000000000000, -1.189524669241239115E-16, -0.000000000000000000 ) ) ;
#231 = AXIS2_PLACEMENT_3D ( 'NONE', #66179, #33824, #22947 ) ;
#232 = AXIS2_PLACEMENT_3D ( 'NONE', #24788, #2610, #8300 ) ;
#233 = DIRECTION ( 'NONE',  ( -0.000000000000000000, 1.000000000000000000, -0.000000000000000000 ) ) ;
#234 = CARTESIAN_POINT ( 'NONE',  ( 0.000000000000000000, 0.9999999999999991118, 79.00402776293826435 ) ) ;
#235 = STYLED_ITEM ( 'NONE', ( #26376 ), #25017 ) ;
#236 = DIRECTION ( 'NONE',  ( 0.000000000000000000, 0.000000000000000000, -1.000000000000000000 ) ) ;
#237 = CARTESIAN_POINT ( 'NONE',  ( 7.632228543268607446, 140.0429263765338135, 2.479861379858954606 ) ) ;
#238 = ORIENTED_EDGE ( 'NONE', *, *, #66575, .F. ) ;
#239 = CARTESIAN_POINT ( 'NONE',  ( -116.0049999999999955, 6.826472737025115478, 4.959722759717899443 ) ) ;
#240 = ORIENTED_EDGE ( 'NONE', *, *, #61435, .F. ) ;
#241 = CARTESIAN_POINT ( 'NONE',  ( 32.00000000000001421, 42.00000000000000000, 45.61250543006183022 ) ) ;
#242 = CARTESIAN_POINT ( 'NONE',  ( -45.00000000000000000, 99.99999999999992895, 9.500000000000000000 ) ) ;
#243 = EDGE_CURVE ( 'NONE', #42679, #46237, #35432, .T. ) ;
#244 = ORIENTED_EDGE ( 'NONE', *, *, #29335, .T. ) ;
#245 = DIRECTION ( 'NONE',  ( 0.000000000000000000, 0.000000000000000000, 1.000000000000000000 ) ) ;
#246 = VERTEX_POINT ( 'NONE', #61384 ) ;
#247 = VECTOR ( 'NONE', #43567, 1000.000000000000000 ) ;
#248 = AXIS2_PLACEMENT_3D ( 'NONE', #65963, #7915, #18135 ) ;
#249 = PRESENTATION_STYLE_ASSIGNMENT (( #27017 ) ) ;
#250 = CARTESIAN_POINT ( 'NONE',  ( -5.598654528085806881, 154.7450000000000045, -7.705886871421374629 ) ) ;
#251 = CARTESIAN_POINT ( 'NONE',  ( -10.11618306975752368, 54.14354156754873060, -6.790106699912857202 ) ) ;
#252 = ADVANCED_FACE ( 'NONE', ( #46303 ), #29740, .T. ) ;
#253 = ORIENTED_EDGE ( 'NONE', *, *, #40055, .T. ) ;
#254 = AXIS2_PLACEMENT_3D ( 'NONE', #63574, #19953, #15420 ) ;
#255 = FACE_OUTER_BOUND ( 'NONE', #52685, .T. ) ;
#256 = CARTESIAN_POINT ( 'NONE',  ( 6.062177826491067734, 2.500000000000000000, 3.500000000000000000 ) ) ;
#257 = ORIENTED_EDGE ( 'NONE', *, *, #41024, .T. ) ;
#258 = CARTESIAN_POINT ( 'NONE',  ( 6.826472737025121695, 125.4929263765338021, -4.959722759717905660 ) ) ;
#259 = FACE_OUTER_BOUND ( 'NONE', #25224, .T. ) ;
#260 = CARTESIAN_POINT ( 'NONE',  ( -47.75707362346617657, -5.598654528085801552, 7.705886871421367523 ) ) ;
#261 = STYLED_ITEM ( 'NONE', ( #11744 ), #23739 ) ;
#262 = SURFACE_STYLE_FILL_AREA ( #59071 ) ;
#263 = CYLINDRICAL_SURFACE ( 'NONE', #24226, 0.5000000000000004441 ) ;
#264 = ORIENTED_EDGE ( 'NONE', *, *, #62719, .T. ) ;
#265 = PRESENTATION_LAYER_ASSIGNMENT (  '', '', ( #48688 ) ) ;
#266 = CARTESIAN_POINT ( 'NONE',  ( -9.250000000000003553, 25.24999999999998934, -4.000000000000000000 ) ) ;
#267 = EDGE_CURVE ( 'NONE', #53683, #25670, #29372, .T. ) ;
#268 = ORIENTED_EDGE ( 'NONE', *, *, #5778, .F. ) ;
#269 = PRESENTATION_STYLE_ASSIGNMENT (( #22843 ) ) ;
#270 = SURFACE_SIDE_STYLE ('',( #10898 ) ) ;
#271 = CARTESIAN_POINT ( 'NONE',  ( -141.6550000000000011, -7.632228543268600340, -2.479861379858950166 ) ) ;
#272 = AXIS2_PLACEMENT_3D ( 'NONE', #51746, #29926, #40167 ) ;
#273 = CYLINDRICAL_SURFACE ( 'NONE', #56704, 18.00000000000000355 ) ;
#274 = CARTESIAN_POINT ( 'NONE',  ( 4.041451884327377897, -1.417096231345241097, 7.000000000000000888 ) ) ;
#275 = UNCERTAINTY_MEASURE_WITH_UNIT (LENGTH_MEASURE( 1.000000000000000082E-05 ), #13075, 'distance_accuracy_value', 'NONE');
#276 = MECHANICAL_DESIGN_GEOMETRIC_PRESENTATION_REPRESENTATION (  '', ( #28426 ), #30651 ) ;
#277 = CARTESIAN_POINT ( 'NONE',  ( -106.6429263765338078, -5.598654528085801552, 7.705886871421367523 ) ) ;
#278 = EDGE_CURVE ( 'NONE', #12588, #35727, #7038, .T. ) ;
#279 =( LENGTH_UNIT ( ) NAMED_UNIT ( * ) SI_UNIT ( .MILLI., .METRE. ) );
#280 = CARTESIAN_POINT ( 'NONE',  ( 41.47746817312157219, 107.6230562796895072, 3.580135233560061803 ) ) ;
#281 = ORIENTED_EDGE ( 'NONE', *, *, #65356, .T. ) ;
#282 = ORIENTED_EDGE ( 'NONE', *, *, #38883, .T. ) ;
#283 = CARTESIAN_POINT ( 'NONE',  ( -44.99928864675339923, 9.682073287424886487, 3.525366027039916528 ) ) ;
#284 = MECHANICAL_DESIGN_GEOMETRIC_PRESENTATION_REPRESENTATION (  '', ( #21680 ), #66580 ) ;
#285 = DIRECTION ( 'NONE',  ( -0.000000000000000000, -1.000000000000000000, -0.000000000000000000 ) ) ;
#286 = MECHANICAL_DESIGN_GEOMETRIC_PRESENTATION_REPRESENTATION (  '', ( #23945 ), #46493 ) ;
#287 = CARTESIAN_POINT ( 'NONE',  ( -55.55499999999999261, 0.000000000000000000, 8.024999999999991473 ) ) ;
#288 = ORIENTED_EDGE ( 'NONE', *, *, #20970, .T. ) ;
#289 = DIRECTION ( 'NONE',  ( 1.000000000000000000, 0.000000000000000000, -0.000000000000000000 ) ) ;
#290 = CARTESIAN_POINT ( 'NONE',  ( 57.00000000000000000, 5.000000000000000000, -60.00402776293827145 ) ) ;
#291 = CARTESIAN_POINT ( 'NONE',  ( 0.000000000000000000, 21.74999999999998224, 3.750000000000000000 ) ) ;
#292 = DIRECTION ( 'NONE',  ( 0.000000000000000000, 0.000000000000000000, 1.000000000000000000 ) ) ;
#293 = FACE_OUTER_BOUND ( 'NONE', #40694, .T. ) ;
#294 = ORIENTED_EDGE ( 'NONE', *, *, #44539, .F. ) ;
#295 = AXIS2_PLACEMENT_3D ( 'NONE', #291, #21821, #59418 ) ;
#296 = DIRECTION ( 'NONE',  ( -0.000000000000000000, 1.000000000000000000, -0.000000000000000000 ) ) ;
#297 = CARTESIAN_POINT ( 'NONE',  ( -195.0000000000000000, 0.000000000000000000, 9.524999999999991473 ) ) ;
#298 = DIRECTION ( 'NONE',  ( 0.000000000000000000, 0.000000000000000000, 1.000000000000000000 ) ) ;
#299 = CARTESIAN_POINT ( 'NONE',  ( 4.716976649647096842, 125.8570736234661496, 6.492361379858953896 ) ) ;
#300 = CARTESIAN_POINT ( 'NONE',  ( -111.1449999999999960, -4.716976649647092401, 6.492361379858946790 ) ) ;
#301 = CARTESIAN_POINT ( 'NONE',  ( 5.598654528085805993, 112.3549999999999898, 7.705886871421374629 ) ) ;
#302 = CARTESIAN_POINT ( 'NONE',  ( -91.79500000000000171, 2.607480562269068880, -8.024999999999993250 ) ) ;
#303 = CARTESIAN_POINT ( 'NONE',  ( 9.250000000000003553, 27.99999999999998934, -3.750000000000000000 ) ) ;
#304 =( GEOMETRIC_REPRESENTATION_CONTEXT ( 3 ) GLOBAL_UNCERTAINTY_ASSIGNED_CONTEXT ( ( #58594 ) ) GLOBAL_UNIT_ASSIGNED_CONTEXT ( ( #4162, #68574, #20369 ) ) REPRESENTATION_CONTEXT ( 'NONE', 'WORKASPACE' ) );
#306 = CIRCLE ( 'NONE', #39710, 0.2500000000000002220 ) ;
#305 = AXIS2_PLACEMENT_3D ( 'NONE', #48367, #58534, #16691 ) ;
#307 = CYLINDRICAL_SURFACE ( 'NONE', #23624, 13.99999999999999822 ) ;
#308 = CARTESIAN_POINT ( 'NONE',  ( -4.041451884327380562, 1.417096231345237545, -7.000000000000003553 ) ) ;
#309 = UNCERTAINTY_MEASURE_WITH_UNIT (LENGTH_MEASURE( 1.000000000000000082E-05 ), #35446, 'distance_accuracy_value', 'NONE');
#310 = ADVANCED_FACE ( 'NONE', ( #67035 ), #58895, .T. ) ;
#311 = STYLED_ITEM ( 'NONE', ( #371 ), #47003 ) ;
#312 = ORIENTED_EDGE ( 'NONE', *, *, #24526, .F. ) ;
#313 = CARTESIAN_POINT ( 'NONE',  ( -124.3429263765337964, -9.058813317711329915, 2.943386871421371787 ) ) ;
#314 = CARTESIAN_POINT ( 'NONE',  ( -149.0949999999999704, -2.607480562269071545, -8.024999999999991473 ) ) ;
#315 = FACE_OUTER_BOUND ( 'NONE', #23935, .T. ) ;
#316 = CIRCLE ( 'NONE', #9392, 2.000000000000001776 ) ;
#317 = FACE_OUTER_BOUND ( 'NONE', #34215, .T. ) ;
#318 = CARTESIAN_POINT ( 'NONE',  ( -75.75000000000000000, -0.9999999999999995559, 5.000000000000001776 ) ) ;
#319 = ORIENTED_EDGE ( 'NONE', *, *, #13976, .T. ) ;
#320 = VERTEX_POINT ( 'NONE', #28678 ) ;
#321 =( GEOMETRIC_REPRESENTATION_CONTEXT ( 3 ) GLOBAL_UNCERTAINTY_ASSIGNED_CONTEXT ( ( #54569 ) ) GLOBAL_UNIT_ASSIGNED_CONTEXT ( ( #7356, #56918, #50953 ) ) REPRESENTATION_CONTEXT ( 'NONE', 'WORKASPACE' ) );
#322 = CARTESIAN_POINT ( 'NONE',  ( -47.54356174116917089, -13.47739874223435486, 2.712348457220761677 ) ) ;
#323 = CARTESIAN_POINT ( 'NONE',  ( -43.75000000000000000, 4.336808689942018722E-16, -5.099999999999999645 ) ) ;
#324 = ADVANCED_FACE ( 'NONE', ( #66322 ), #18147, .F. ) ;
#325 = DIRECTION ( 'NONE',  ( 0.000000000000000000, 0.000000000000000000, -1.000000000000000000 ) ) ;
#326 = CARTESIAN_POINT ( 'NONE',  ( -45.84245570871746622, 9.151528339695964576, 6.292049778185707432 ) ) ;
#327 = CARTESIAN_POINT ( 'NONE',  ( -129.6570736234661751, 9.058813317711329915, 2.943386871421369566 ) ) ;
#328 = AXIS2_PLACEMENT_3D ( 'NONE', #15577, #26444, #22218 ) ;
#329 = LINE ( 'NONE', #43015, #27426 ) ;
#330 = VERTEX_POINT ( 'NONE', #26529 ) ;
#331 = CARTESIAN_POINT ( 'NONE',  ( -138.2049999999999557, -2.607480562269071545, -8.024999999999991473 ) ) ;
#332 = EDGE_CURVE ( 'NONE', #19277, #32327, #42649, .T. ) ;
#333 = CIRCLE ( 'NONE', #2606, 13.50000000000000178 ) ;
#334 = EDGE_CURVE ( 'NONE', #46687, #29083, #34195, .T. ) ;
#335 = EDGE_LOOP ( 'NONE', ( #46322, #25808, #46956, #19729 ) ) ;
#336 = SURFACE_STYLE_USAGE ( .BOTH. , #31016 ) ;
#337 = LINE ( 'NONE', #47253, #45614 ) ;
#338 = EDGE_LOOP ( 'NONE', ( #32374, #30973 ) ) ;
#339 = CARTESIAN_POINT ( 'NONE',  ( -22.75000000000000711, 37.00000000000000000, -3.750000000000000000 ) ) ;
#340 = CARTESIAN_POINT ( 'NONE',  ( -1.166476076187854022E-15, 134.9449999999999932, 9.525000000000000355 ) ) ;
#341 = ORIENTED_EDGE ( 'NONE', *, *, #5446, .F. ) ;
#342 = AXIS2_PLACEMENT_3D ( 'NONE', #10777, #58965, #31869 ) ;
#343 = SURFACE_STYLE_FILL_AREA ( #48645 ) ;
#345 = EDGE_CURVE ( 'NONE', #35189, #45655, #41362, .T. ) ;
#344 = CARTESIAN_POINT ( 'NONE',  ( 9.058813317711337021, 130.6550000000000011, 2.943386871421375783 ) ) ;
#346 = CARTESIAN_POINT ( 'NONE',  ( -60.65499999999998693, -7.632228543268600340, -2.479861379858950166 ) ) ;
#347 = CARTESIAN_POINT ( 'NONE',  ( -124.4949999999999761, 6.826472737025113702, -4.959722759717902107 ) ) ;
#348 = CARTESIAN_POINT ( 'NONE',  ( -15.48999599679678951, 117.4999999999999716, -10.00000000000000000 ) ) ;
#349 = ORIENTED_EDGE ( 'NONE', *, *, #57912, .F. ) ;
#350 = CARTESIAN_POINT ( 'NONE',  ( 5.598654528085805993, 148.3549999999999898, 7.705886871421374629 ) ) ;
#351 = CARTESIAN_POINT ( 'NONE',  ( -74.99999999999998579, 119.9999999999997726, 9.500000000000000000 ) ) ;
#352 = UNCERTAINTY_MEASURE_WITH_UNIT (LENGTH_MEASURE( 1.000000000000000082E-05 ), #2968, 'distance_accuracy_value', 'NONE');
#353 = CARTESIAN_POINT ( 'NONE',  ( -69.50000000000000000, 50.00000000000000000, -12.00000000000000000 ) ) ;
#354 = EDGE_CURVE ( 'NONE', #25360, #68588, #1, .T. ) ;
#355 = MECHANICAL_DESIGN_GEOMETRIC_PRESENTATION_REPRESENTATION (  '', ( #14033 ), #16160 ) ;
#356 = SURFACE_SIDE_STYLE ('',( #48656 ) ) ;
#357 = FILL_AREA_STYLE ('',( #26774 ) ) ;
#358 = FILL_AREA_STYLE_COLOUR ( '', #9295 ) ;
#359 = EDGE_CURVE ( 'NONE', #40324, #25898, #56986, .T. ) ;
#360 = VERTEX_POINT ( 'NONE', #25837 ) ;
#361 = STYLED_ITEM ( 'NONE', ( #59359 ), #48177 ) ;
#362 = AXIS2_PLACEMENT_3D ( 'NONE', #9506, #4167, #25641 ) ;
#363 =( NAMED_UNIT ( * ) PLANE_ANGLE_UNIT ( ) SI_UNIT ( $, .RADIAN. ) );
#364 = DIRECTION ( 'NONE',  ( 1.000000000000000000, 0.000000000000000000, 0.000000000000000000 ) ) ;
#365 = CARTESIAN_POINT ( 'NONE',  ( -170.4549999999999841, 7.632228543268599452, -2.479861379858951942 ) ) ;
#366 = ORIENTED_EDGE ( 'NONE', *, *, #63470, .F. ) ;
#367 = SURFACE_STYLE_FILL_AREA ( #58828 ) ;
#368 = UNCERTAINTY_MEASURE_WITH_UNIT (LENGTH_MEASURE( 1.000000000000000082E-05 ), #47808, 'distance_accuracy_value', 'NONE');
#369 = VECTOR ( 'NONE', #21449, 1000.000000000000114 ) ;
#370 = FILL_AREA_STYLE ('',( #16639 ) ) ;
#371 = PRESENTATION_STYLE_ASSIGNMENT (( #36383 ) ) ;
#372 = CARTESIAN_POINT ( 'NONE',  ( -20.42000000000000881, 0.000000000000000000, -12.50000000000000000 ) ) ;
#373 = VERTEX_POINT ( 'NONE', #69120 ) ;
#374 = DIRECTION ( 'NONE',  ( -1.000000000000000000, -0.000000000000000000, -0.000000000000000000 ) ) ;
#375 = CARTESIAN_POINT ( 'NONE',  ( -88.85499999999998977, 4.716976649647094177, 6.492361379858945902 ) ) ;
#377 = ORIENTED_EDGE ( 'NONE', *, *, #6524, .T. ) ;
#376 = AXIS2_PLACEMENT_3D ( 'NONE', #14154, #19764, #67612 ) ;
#378 = CARTESIAN_POINT ( 'NONE',  ( -46.25707362346617657, 5.598654528085800663, -7.705886871421367523 ) ) ;
#379 = CARTESIAN_POINT ( 'NONE',  ( 71.99999999999998579, 63.67479433117734544, -9.500000000000000000 ) ) ;
#380 =( GEOMETRIC_REPRESENTATION_CONTEXT ( 3 ) GLOBAL_UNCERTAINTY_ASSIGNED_CONTEXT ( ( #3120 ) ) GLOBAL_UNIT_ASSIGNED_CONTEXT ( ( #49416, #10736, #5098 ) ) REPRESENTATION_CONTEXT ( 'NONE', 'WORKASPACE' ) );
#381 = EDGE_CURVE ( 'NONE', #57733, #8059, #64170, .T. ) ;
#382 = DIRECTION ( 'NONE',  ( -0.000000000000000000, 1.000000000000000000, -0.000000000000000000 ) ) ;
#383 = CARTESIAN_POINT ( 'NONE',  ( -63.50707362346616947, 8.102448949553176405, 5.886773742842740909 ) ) ;
#384 = SURFACE_SIDE_STYLE ('',( #16992 ) ) ;
#385 = AXIS2_PLACEMENT_3D ( 'NONE', #51419, #38910, #35597 ) ;
#386 = ORIENTED_EDGE ( 'NONE', *, *, #25244, .T. ) ;
#387 = FILL_AREA_STYLE_COLOUR ( '', #30374 ) ;
#389 = DIRECTION ( 'NONE',  ( -0.000000000000000000, 1.000000000000000000, -0.000000000000000000 ) ) ;
#388 = SURFACE_SIDE_STYLE ('',( #27504 ) ) ;
#390 =( GEOMETRIC_REPRESENTATION_CONTEXT ( 3 ) GLOBAL_UNCERTAINTY_ASSIGNED_CONTEXT ( ( #37775 ) ) GLOBAL_UNIT_ASSIGNED_CONTEXT ( ( #23177, #45009, #60773 ) ) REPRESENTATION_CONTEXT ( 'NONE', 'WORKASPACE' ) );
#391 = CIRCLE ( 'NONE', #1543, 2.499999999999998668 ) ;
#392 = CARTESIAN_POINT ( 'NONE',  ( -102.5049999999999955, -6.826472737025115478, -4.959722759717899443 ) ) ;
#393 = CARTESIAN_POINT ( 'NONE',  ( 10.01517768586949231, 132.6949999999999363, 1.839758294383810543E-15 ) ) ;
#394 = CARTESIAN_POINT ( 'NONE',  ( -115.0449999999999875, 7.632228543268600340, 2.479861379858949277 ) ) ;
#395 = PRESENTATION_LAYER_ASSIGNMENT (  '', '', ( #8301 ) ) ;
#396 = FILL_AREA_STYLE_COLOUR ( '', #24610 ) ;
#398 = CARTESIAN_POINT ( 'NONE',  ( -153.6570736234661751, 9.058813317711329915, 2.943386871421369566 ) ) ;
#397 = LINE ( 'NONE', #21925, #57054 ) ;
#399 = AXIS2_PLACEMENT_3D ( 'NONE', #50431, #30330, #39914 ) ;
#400 = CARTESIAN_POINT ( 'NONE',  ( -161.3929263765337794, 8.102448949553176405, 5.886773742842740909 ) ) ;
#401 = CARTESIAN_POINT ( 'NONE',  ( -174.2949999999999591, -2.607480562269069768, 8.024999999999991473 ) ) ;
#402 = VECTOR ( 'NONE', #43226, 1000.000000000000000 ) ;
#403 = SURFACE_STYLE_FILL_AREA ( #27517 ) ;
#405 = DIRECTION ( 'NONE',  ( -0.000000000000000000, 1.000000000000000000, -0.000000000000000000 ) ) ;
#404 = COLOUR_RGB ( '', 0.72549020, 0.75294118, 0.79215686) ;
#406 = ORIENTED_EDGE ( 'NONE', *, *, #2305, .T. ) ;
#407 = CARTESIAN_POINT ( 'NONE',  ( 15.98999599679679839, 118.4999999999999716, 9.500000000000000000 ) ) ;
#408 = VERTEX_POINT ( 'NONE', #20929 ) ;
#409 = CARTESIAN_POINT ( 'NONE',  ( -74.39292637653380780, 8.102448949553176405, 5.886773742842740909 ) ) ;
#410 = ITEM_DEFINED_TRANSFORMATION ( 'NONE', 'NONE', #22560,  #42840 ) ;
#411 = DIRECTION ( 'NONE',  ( 1.000000000000000000, 2.116950682547968038E-14, 0.000000000000000000 ) ) ;
#412 = DIRECTION ( 'NONE',  ( 0.000000000000000000, -0.000000000000000000, 1.000000000000000000 ) ) ;
#413 = ADVANCED_FACE ( 'NONE', ( #42770 ), #52941, .F. ) ;
#414 = DIRECTION ( 'NONE',  ( -1.000000000000000000, 0.000000000000000000, 0.000000000000000000 ) ) ;
#415 =( LENGTH_UNIT ( ) NAMED_UNIT ( * ) SI_UNIT ( .MILLI., .METRE. ) );
#416 = CARTESIAN_POINT ( 'NONE',  ( -7.566679973970432016, -4.894125840469273570, -1.768604793866979108E-15 ) ) ;
#417 = VERTEX_POINT ( 'NONE', #64528 ) ;
#418 = CARTESIAN_POINT ( 'NONE',  ( -177.2050000000000125, -2.607480562269071545, -8.024999999999991473 ) ) ;
#419 = ADVANCED_FACE ( 'NONE', ( #59216 ), #27553, .F. ) ;
#420 = AXIS2_PLACEMENT_3D ( 'NONE', #64761, #28836, #27779 ) ;
#421 = ORIENTED_EDGE ( 'NONE', *, *, #43281, .T. ) ;
#422 = DIRECTION ( 'NONE',  ( 1.000000000000000000, 0.000000000000000000, 0.000000000000000000 ) ) ;
#423 = DIRECTION ( 'NONE',  ( -1.000000000000000000, -0.000000000000000000, -0.000000000000000000 ) ) ;
#424 = DIRECTION ( 'NONE',  ( 1.000000000000000000, 0.000000000000000000, 0.000000000000000000 ) ) ;
#425 = DIRECTION ( 'NONE',  ( -1.000000000000000000, 0.000000000000000000, 0.000000000000000000 ) ) ;
#426 = AXIS2_PLACEMENT_3D ( 'NONE', #33230, #23025, #2543 ) ;
#427 =( BOUNDED_SURFACE ( )  B_SPLINE_SURFACE ( 3, 2, ( 
 ( #49244, #43328, #49944 ),
 ( #55178, #22502, #32695 ),
 ( #44001, #54149, #283 ),
 ( #65414, #17262, #38724 ),
 ( #17597, #60131, #11944 ),
 ( #54828, #22857, #44353 ),
 ( #65756, #39063, #13666 ),
 ( #39400, #66088, #40781 ) ),
 .UNSPECIFIED., .F., .F., .F. ) 
 B_SPLINE_SURFACE_WITH_KNOTS ( ( 4, 2, 2, 4 ),
 ( 3, 3 ),
 ( 0.003346294263012634333, 0.003496419684072975091, 0.003646545105133316284, 0.003946795947253998668 ),
 ( 0.000000000000000000, 1.000000000000000000 ),
 .UNSPECIFIED. ) 
 GEOMETRIC_REPRESENTATION_ITEM ( )  RATIONAL_B_SPLINE_SURFACE ( (
 ( 1.000000000000000000, 0.2907356542125085763, 1.000000000000000000),
 ( 1.000000000000000000, 0.3025307796950364447, 1.000000000000000000),
 ( 1.000000000000000000, 0.3140637513638668277, 1.000000000000000000),
 ( 1.000000000000000000, 0.3350422074605917677, 1.000000000000000000),
 ( 1.000000000000000000, 0.3444808824053638974, 1.000000000000000000),
 ( 1.000000000000000000, 0.3678721613322129547, 1.000000000000000000),
 ( 1.000000000000000000, 0.3767760736214396111, 1.000000000000000000),
 ( 1.000000000000000000, 0.3766558475679890328, 1.000000000000000000) ) ) 
 REPRESENTATION_ITEM ( '' )  SURFACE ( )  );
#428 = CARTESIAN_POINT ( 'NONE',  ( -7.632228543268607446, 139.6570736234661467, -2.479861379858953718 ) ) ;
#429 = ORIENTED_EDGE ( 'NONE', *, *, #23613, .F. ) ;
#430 = CARTESIAN_POINT ( 'NONE',  ( -96.80499999999999261, -8.437984349512086979, 5.166775262442717831E-16 ) ) ;
#431 = AXIS2_PLACEMENT_3D ( 'NONE', #40119, #61508, #29524 ) ;
#432 = UNCERTAINTY_MEASURE_WITH_UNIT (LENGTH_MEASURE( 1.000000000000000082E-05 ), #8140, 'distance_accuracy_value', 'NONE');
#433 = DIRECTION ( 'NONE',  ( 0.000000000000000000, 0.000000000000000000, 1.000000000000000000 ) ) ;
#434 = ORIENTED_EDGE ( 'NONE', *, *, #4204, .F. ) ;
#435 = CARTESIAN_POINT ( 'NONE',  ( -92.00707362346615525, -8.102448949553174629, -5.886773742842741797 ) ) ;
#436 = EDGE_CURVE ( 'NONE', #66069, #10730, #32165, .T. ) ;
#437 = AXIS2_PLACEMENT_3D ( 'NONE', #17639, #69690, #49288 ) ;
#438 = CARTESIAN_POINT ( 'NONE',  ( -126.8929263765338220, -8.102448949553174629, -5.886773742842741797 ) ) ;
#439 = CARTESIAN_POINT ( 'NONE',  ( 61.74999999999998579, 30.74999999999999289, -4.000000000000000000 ) ) ;
#440 = ORIENTED_EDGE ( 'NONE', *, *, #34479, .T. ) ;
#441 = CARTESIAN_POINT ( 'NONE',  ( 1.000000000000000000, 14.00000000000000000, -79.00402776293826435 ) ) ;
#442 = CARTESIAN_POINT ( 'NONE',  ( -59.24499999999999034, -4.716976649647093289, -6.492361379858945902 ) ) ;
#443 = VERTEX_POINT ( 'NONE', #33210 ) ;
#444 = PRESENTATION_LAYER_ASSIGNMENT (  '', '', ( #30821 ) ) ;
#445 = AXIS2_PLACEMENT_3D ( 'NONE', #1315, #50606, #28423 ) ;
#446 = DIRECTION ( 'NONE',  ( 0.000000000000000000, 0.000000000000000000, 1.000000000000000000 ) ) ;
#447 = CARTESIAN_POINT ( 'NONE',  ( -139.2570736234661695, 5.598654528085800663, -7.705886871421367523 ) ) ;
#448 = ORIENTED_EDGE ( 'NONE', *, *, #48910, .F. ) ;
#449 = PRESENTATION_STYLE_ASSIGNMENT (( #6812 ) ) ;
#450 = CARTESIAN_POINT ( 'NONE',  ( -195.0000000000000000, 0.000000000000000000, 0.000000000000000000 ) ) ;
#451 = ORIENTED_EDGE ( 'NONE', *, *, #12857, .T. ) ;
#452 = DIRECTION ( 'NONE',  ( -1.000000000000000000, 0.000000000000000000, 0.000000000000000000 ) ) ;
#453 = CARTESIAN_POINT ( 'NONE',  ( -117.8050000000000068, -8.437984349512085203, 5.166775262442717831E-16 ) ) ;
#454 = VERTEX_POINT ( 'NONE', #6800 ) ;
#455 = EDGE_CURVE ( 'NONE', #58809, #68764, #43475, .T. ) ;
#456 = LINE ( 'NONE', #49090, #15967 ) ;
#457 = SURFACE_SIDE_STYLE ('',( #43491 ) ) ;
#458 =( LENGTH_UNIT ( ) NAMED_UNIT ( * ) SI_UNIT ( .MILLI., .METRE. ) );
#459 = AXIS2_PLACEMENT_3D ( 'NONE', #49067, #22282, #38157 ) ;
#460 = CIRCLE ( 'NONE', #48869, 0.2500000000000002220 ) ;
#461 = CARTESIAN_POINT ( 'NONE',  ( -159.5070736234661979, 8.102448949553176405, 5.886773742842740909 ) ) ;
#462 = EDGE_CURVE ( 'NONE', #45832, #24916, #21603, .T. ) ;
#463 = CARTESIAN_POINT ( 'NONE',  ( 5.598654528085809545, 136.1449999999999818, -7.705886871421373741 ) ) ;
#464 = CARTESIAN_POINT ( 'NONE',  ( -99.05707362346618083, 0.000000000000000000, 9.524999999999991473 ) ) ;
#465 = PRESENTATION_STYLE_ASSIGNMENT (( #5780 ) ) ;
#466 = EDGE_LOOP ( 'NONE', ( #50263, #33098, #39209, #1885 ) ) ;
#467 =( NAMED_UNIT ( * ) PLANE_ANGLE_UNIT ( ) SI_UNIT ( $, .RADIAN. ) );
#468 =( NAMED_UNIT ( * ) SI_UNIT ( $, .STERADIAN. ) SOLID_ANGLE_UNIT ( ) );
#469 = FACE_OUTER_BOUND ( 'NONE', #45688, .T. ) ;
#470 = CIRCLE ( 'NONE', #10679, 0.5000000000000004441 ) ;
#471 = CARTESIAN_POINT ( 'NONE',  ( -144.9550000000000125, -7.632228543268599452, 2.479861379858951054 ) ) ;
#472 = DIRECTION ( 'NONE',  ( 0.000000000000000000, 0.000000000000000000, -1.000000000000000000 ) ) ;
#473 = CARTESIAN_POINT ( 'NONE',  ( 75.00000000000000000, -2.215169945516535778E-14, -9.500000000000000000 ) ) ;
#474 = CARTESIAN_POINT ( 'NONE',  ( -144.4449999999999932, 0.000000000000000000, 8.024999999999991473 ) ) ;
#475 = AXIS2_PLACEMENT_3D ( 'NONE', #59190, #10003, #26823 ) ;
#476 = CARTESIAN_POINT ( 'NONE',  ( -136.6449999999999818, 4.716976649647091513, -6.492361379858946790 ) ) ;
#477 = EDGE_LOOP ( 'NONE', ( #1632, #5095, #61496, #50075 ) ) ;
#478 = TOROIDAL_SURFACE ( 'NONE', #19609, 27.49999999999999645, 0.5000000000000000000 ) ;
#479 = SURFACE_STYLE_USAGE ( .BOTH. , #37889 ) ;
#480 = CIRCLE ( 'NONE', #20796, 0.5000000000000004441 ) ;
#481 = CARTESIAN_POINT ( 'NONE',  ( -50.45499999999996987, 7.632228543268599452, -2.479861379858951942 ) ) ;
#482 = CARTESIAN_POINT ( 'NONE',  ( -57.59499999999998465, 2.607480562269073321, 8.024999999999991473 ) ) ;
#483 = PRESENTATION_STYLE_ASSIGNMENT (( #53340 ) ) ;
#484 = CARTESIAN_POINT ( 'NONE',  ( 4.000000000000002665, 38.70020753820971748, -89.00000000000000000 ) ) ;
#485 = EDGE_CURVE ( 'NONE', #67224, #42847, #8634, .T. ) ;
#486 = CARTESIAN_POINT ( 'NONE',  ( -103.1929263765338192, -10.01517768586948698, 6.132527647946031529E-16 ) ) ;
#487 = DIRECTION ( 'NONE',  ( -1.066927527481589776E-15, 0.9999999056890690463, -0.0004343061746624778119 ) ) ;
#488 = CIRCLE ( 'NONE', #21959, 112.9999999999981526 ) ;
#489 = SURFACE_SIDE_STYLE ('',( #28657 ) ) ;
#490 = AXIS2_PLACEMENT_3D ( 'NONE', #45726, #67139, #13310 ) ;
#491 = CARTESIAN_POINT ( 'NONE',  ( 4.250000000000001776, 21.99999999999998579, -3.750000000000000000 ) ) ;
#492 = SURFACE_SIDE_STYLE ('',( #43527 ) ) ;
#493 = CIRCLE ( 'NONE', #39921, 0.5000000000000004441 ) ;
#494 = DIRECTION ( 'NONE',  ( -1.000000000000000000, 0.000000000000000000, 0.000000000000000000 ) ) ;
#495 = EDGE_CURVE ( 'NONE', #60866, #33108, #37843, .T. ) ;
#496 = EDGE_LOOP ( 'NONE', ( #21915, #36794, #9814, #1766 ) ) ;
#497 = CARTESIAN_POINT ( 'NONE',  ( 0.000000000000000000, -3.000000000000000000, 7.000000000000001776 ) ) ;
#498 = SURFACE_STYLE_FILL_AREA ( #48799 ) ;
#499 = ORIENTED_EDGE ( 'NONE', *, *, #68459, .T. ) ;
#500 = MECHANICAL_DESIGN_GEOMETRIC_PRESENTATION_REPRESENTATION (  '', ( #7305 ), #9589 ) ;
#501 = EDGE_CURVE ( 'NONE', #29891, #48746, #14250, .T. ) ;
#502 = CARTESIAN_POINT ( 'NONE',  ( 8.437984349512095861, 114.3070736234661666, 1.550032578732817026E-15 ) ) ;
#503 =( LENGTH_UNIT ( ) NAMED_UNIT ( * ) SI_UNIT ( .MILLI., .METRE. ) );
#504 = DIRECTION ( 'NONE',  ( -0.000000000000000000, 1.000000000000000000, -0.000000000000000000 ) ) ;
#505 = DIRECTION ( 'NONE',  ( 1.000000000000000000, 0.000000000000000000, 0.000000000000000000 ) ) ;
#506 = ORIENTED_EDGE ( 'NONE', *, *, #15438, .F. ) ;
#507 = ORIENTED_EDGE ( 'NONE', *, *, #36909, .F. ) ;
#508 = ADVANCED_FACE ( 'NONE', ( #27196 ), #65200, .F. ) ;
#509 = CARTESIAN_POINT ( 'NONE',  ( 0.000000000000000000, 1.000000000000000222, 3.000000000000000000 ) ) ;
#510 = VECTOR ( 'NONE', #3553, 1000.000000000000000 ) ;
#511 = FILL_AREA_STYLE_COLOUR ( '', #37228 ) ;
#512 = ORIENTED_EDGE ( 'NONE', *, *, #8696, .F. ) ;
#513 = CARTESIAN_POINT ( 'NONE',  ( -10.01517768586949231, 126.3049999999999784, -6.132527647946036459E-16 ) ) ;
#514 = CARTESIAN_POINT ( 'NONE',  ( 10.00000000000000178, 43.00000000000000000, -90.00000000000000000 ) ) ;
#515 = CIRCLE ( 'NONE', #57891, 0.2500000000000002220 ) ;
#516 = CARTESIAN_POINT ( 'NONE',  ( 6.826472737025121695, 149.4929263765338021, -4.959722759717905660 ) ) ;
#517 = CARTESIAN_POINT ( 'NONE',  ( -90.44499999999997897, 0.000000000000000000, 8.024999999999991473 ) ) ;
#518 = ORIENTED_EDGE ( 'NONE', *, *, #44832, .T. ) ;
#519 =( BOUNDED_CURVE ( )  B_SPLINE_CURVE ( 3, ( #46857, #68263, #20043, #8814 ),
 .UNSPECIFIED., .F., .F. ) 
 B_SPLINE_CURVE_WITH_KNOTS ( ( 4, 4 ),
 ( 4.712388980384689674, 6.283185307179586232 ),
 .UNSPECIFIED. ) 
 CURVE ( )  GEOMETRIC_REPRESENTATION_ITEM ( )  RATIONAL_B_SPLINE_CURVE ( ( 1.000000000000000000, 0.8047378541243649375, 0.8047378541243649375, 1.000000000000000000 ) ) 
 REPRESENTATION_ITEM ( '' )  );
#520 = FILL_AREA_STYLE ('',( #23094 ) ) ;
#521 = CYLINDRICAL_SURFACE ( 'NONE', #54220, 0.2500000000000002220 ) ;
#522 = ORIENTED_EDGE ( 'NONE', *, *, #64472, .T. ) ;
#523 = CARTESIAN_POINT ( 'NONE',  ( -175.4929263765337737, -8.102448949553174629, 5.886773742842742685 ) ) ;
#524 = SURFACE_STYLE_FILL_AREA ( #22748 ) ;
#525 = CARTESIAN_POINT ( 'NONE',  ( 6.418790567836331284, -2.882328613363594361, 0.02778322089669375133 ) ) ;
#526 = CYLINDRICAL_SURFACE ( 'NONE', #25539, 8.025000000000000355 ) ;
#527 = ORIENTED_EDGE ( 'NONE', *, *, #58530, .F. ) ;
#528 = DIRECTION ( 'NONE',  ( 1.000000000000000000, 0.000000000000000000, 0.000000000000000000 ) ) ;
#529 = VERTEX_POINT ( 'NONE', #11740 ) ;
#530 = CARTESIAN_POINT ( 'NONE',  ( -68.49999999999998579, -1.919947267060472329E-14, -10.49999999999999822 ) ) ;
#531 = DIRECTION ( 'NONE',  ( 0.000000000000000000, 1.000000000000000000, 0.000000000000000000 ) ) ;
#532 = CARTESIAN_POINT ( 'NONE',  ( 44.97237157117557871, 9.999999999999980460, 3.164074568774512652 ) ) ;
#533 = SURFACE_STYLE_USAGE ( .BOTH. , #23107 ) ;
#534 = DIRECTION ( 'NONE',  ( 0.000000000000000000, 0.000000000000000000, -1.000000000000000000 ) ) ;
#535 = CARTESIAN_POINT ( 'NONE',  ( 24.21231517720798010, 113.4999999999999858, 10.00000000000000000 ) ) ;
#536 = AXIS2_PLACEMENT_3D ( 'NONE', #63748, #14905, #19454 ) ;
#537 = CIRCLE ( 'NONE', #69160, 1.000000000000000888 ) ;
#538 = CARTESIAN_POINT ( 'NONE',  ( 6.999798566743343997, 9.396926207859090496, -11.50901484383455120 ) ) ;
#539 = CARTESIAN_POINT ( 'NONE',  ( -115.4929263765338021, -8.102448949553174629, 5.886773742842742685 ) ) ;
#540 = ORIENTED_EDGE ( 'NONE', *, *, #37095, .F. ) ;
#541 = CARTESIAN_POINT ( 'NONE',  ( -161.5429263765338135, 9.058813317711329915, 2.943386871421369566 ) ) ;
#542 = CARTESIAN_POINT ( 'NONE',  ( 0.000000000000000000, 109.9999999999999858, 0.000000000000000000 ) ) ;
#543 = SURFACE_SIDE_STYLE ('',( #44265 ) ) ;
#544 = STYLED_ITEM ( 'NONE', ( #19652 ), #63859 ) ;
#545 = ORIENTED_EDGE ( 'NONE', *, *, #1842, .F. ) ;
#546 = FILL_AREA_STYLE ('',( #7873 ) ) ;
#547 = CARTESIAN_POINT ( 'NONE',  ( -171.0549999999999784, -9.827790563157499189E-16, -8.024999999999991473 ) ) ;
#548 = DIRECTION ( 'NONE',  ( 0.000000000000000000, 0.000000000000000000, -1.000000000000000000 ) ) ;
#549 = DIRECTION ( 'NONE',  ( -1.000000000000000000, 0.000000000000000000, 0.000000000000000000 ) ) ;
#550 = CARTESIAN_POINT ( 'NONE',  ( -171.1449999999999818, -4.716976649647092401, 6.492361379858946790 ) ) ;
#551 = STYLED_ITEM ( 'NONE', ( #61712 ), #49528 ) ;
#552 = CIRCLE ( 'NONE', #64648, 1.000000000000000888 ) ;
#553 = CARTESIAN_POINT ( 'NONE',  ( -166.7949999999999875, 2.607480562269069324, -8.024999999999993250 ) ) ;
#554 = ORIENTED_EDGE ( 'NONE', *, *, #7703, .F. ) ;
#555 = DIRECTION ( 'NONE',  ( 0.000000000000000000, 1.000000000000000000, 0.000000000000000000 ) ) ;
#556 = LINE ( 'NONE', #57031, #55928 ) ;
#557 = LINE ( 'NONE', #64975, #11108 ) ;
#558 =( NAMED_UNIT ( * ) SI_UNIT ( $, .STERADIAN. ) SOLID_ANGLE_UNIT ( ) );
#559 = CARTESIAN_POINT ( 'NONE',  ( -79.85499999999997556, 4.716976649647094177, 6.492361379858945902 ) ) ;
#560 = CARTESIAN_POINT ( 'NONE',  ( -195.0000000000000000, 0.000000000000000000, 0.000000000000000000 ) ) ;
#561 = CARTESIAN_POINT ( 'NONE',  ( 24.58105220659400203, 26.69229804232007197, 27.43511223479084293 ) ) ;
#562 = CARTESIAN_POINT ( 'NONE',  ( 57.00000000000000000, 16.00000000000000000, -60.00402776293825724 ) ) ;
#563 = VECTOR ( 'NONE', #25648, 1000.000000000000000 ) ;
#564 = CARTESIAN_POINT ( 'NONE',  ( -85.49499999999999034, 6.826472737025113702, -4.959722759717902107 ) ) ;
#565 = CARTESIAN_POINT ( 'NONE',  ( 9.058813317711337021, 136.6550000000000011, 2.943386871421375783 ) ) ;
#566 = DIRECTION ( 'NONE',  ( 0.000000000000000000, 1.000000000000000000, 0.000000000000000000 ) ) ;
#567 = AXIS2_PLACEMENT_3D ( 'NONE', #40858, #31645, #58735 ) ;
#568 = EDGE_CURVE ( 'NONE', #2804, #25571, #6450, .T. ) ;
#569 = FILL_AREA_STYLE ('',( #28734 ) ) ;
#570 = EDGE_CURVE ( 'NONE', #54537, #8864, #15015, .T. ) ;
#571 = PRESENTATION_STYLE_ASSIGNMENT (( #38313 ) ) ;
#572 = DIRECTION ( 'NONE',  ( 1.000000000000000000, 0.000000000000000000, 0.000000000000000000 ) ) ;
#573 = ORIENTED_EDGE ( 'NONE', *, *, #64148, .T. ) ;
#574 = STYLED_ITEM ( 'NONE', ( #44469 ), #32799 ) ;
#575 = CARTESIAN_POINT ( 'NONE',  ( 31.00000000000001421, 15.00000000000000000, 35.50000000000000000 ) ) ;
#576 = DIRECTION ( 'NONE',  ( 1.000000000000000000, 0.000000000000000000, 0.000000000000000000 ) ) ;
#577 = EDGE_CURVE ( 'NONE', #48904, #13709, #23970, .T. ) ;
#578 = EDGE_CURVE ( 'NONE', #68782, #823, #306, .T. ) ;
#579 = EDGE_CURVE ( 'NONE', #15724, #20480, #67919, .T. ) ;
#580 = FACE_OUTER_BOUND ( 'NONE', #29985, .T. ) ;
#581 = SURFACE_STYLE_USAGE ( .BOTH. , #6263 ) ;
#582 = VERTEX_POINT ( 'NONE', #12774 ) ;
#583 = VERTEX_POINT ( 'NONE', #9173 ) ;
#584 = CARTESIAN_POINT ( 'NONE',  ( -34.99999999999999289, 99.99999999999998579, -9.500000000000000000 ) ) ;
#585 = ADVANCED_FACE ( 'NONE', ( #60599 ), #66238, .T. ) ;
#586 = CIRCLE ( 'NONE', #9675, 14.49999999999999822 ) ;
#587 = EDGE_CURVE ( 'NONE', #62302, #51825, #44499, .T. ) ;
#588 = CARTESIAN_POINT ( 'NONE',  ( -195.0000000000000000, 0.000000000000000000, 0.000000000000000000 ) ) ;
#589 = DIRECTION ( 'NONE',  ( -2.312964634635740689E-15, 1.000000000000000000, -0.000000000000000000 ) ) ;
#590 = ORIENTED_EDGE ( 'NONE', *, *, #62902, .T. ) ;
#591 = CARTESIAN_POINT ( 'NONE',  ( -112.2549999999999955, -4.716976649647092401, 6.492361379858946790 ) ) ;
#592 = EDGE_LOOP ( 'NONE', ( #33276, #36266, #62240, #1238 ) ) ;
#593 = CIRCLE ( 'NONE', #44497, 0.2500000000000002220 ) ;
#594 =( LENGTH_UNIT ( ) NAMED_UNIT ( * ) SI_UNIT ( .MILLI., .METRE. ) );
#595 = LINE ( 'NONE', #31625, #55701 ) ;
#596 = ORIENTED_EDGE ( 'NONE', *, *, #59481, .F. ) ;
#597 = LINE ( 'NONE', #54114, #32415 ) ;
#598 = FACE_OUTER_BOUND ( 'NONE', #29023, .T. ) ;
#599 = VERTEX_POINT ( 'NONE', #55698 ) ;
#600 =( GEOMETRIC_REPRESENTATION_CONTEXT ( 3 ) GLOBAL_UNCERTAINTY_ASSIGNED_CONTEXT ( ( #58099 ) ) GLOBAL_UNIT_ASSIGNED_CONTEXT ( ( #44153, #38168, #38862 ) ) REPRESENTATION_CONTEXT ( 'NONE', 'WORKASPACE' ) );
#601 = AXIS2_PLACEMENT_3D ( 'NONE', #12597, #1301, #1663 ) ;
#602 =( GEOMETRIC_REPRESENTATION_CONTEXT ( 3 ) GLOBAL_UNCERTAINTY_ASSIGNED_CONTEXT ( ( #27133 ) ) GLOBAL_UNIT_ASSIGNED_CONTEXT ( ( #69280, #58715, #31973 ) ) REPRESENTATION_CONTEXT ( 'NONE', 'WORKASPACE' ) );
#603 = DIRECTION ( 'NONE',  ( -1.000000000000000000, 0.000000000000000000, 0.000000000000000000 ) ) ;
#604 = ORIENTED_EDGE ( 'NONE', *, *, #23658, .F. ) ;
#605 = ORIENTED_EDGE ( 'NONE', *, *, #66146, .T. ) ;
#606 = CARTESIAN_POINT ( 'NONE',  ( -118.4070736234669710, 3.094860106605118233, -9.525000000009663736 ) ) ;
#607 = DIRECTION ( 'NONE',  ( 0.000000000000000000, 0.000000000000000000, -1.000000000000000000 ) ) ;
#608 = DIRECTION ( 'NONE',  ( -1.000000000000000000, -0.000000000000000000, -0.000000000000000000 ) ) ;
#609 = EDGE_LOOP ( 'NONE', ( #63299, #42577, #64965, #23489 ) ) ;
#610 = CARTESIAN_POINT ( 'NONE',  ( 7.632228543268607446, 140.0429263765338135, 2.479861379858954606 ) ) ;
#611 = CARTESIAN_POINT ( 'NONE',  ( -53.60138881051016568, -9.947368421052628307, -2.000000000000000000 ) ) ;
#612 = CARTESIAN_POINT ( 'NONE',  ( -22.25000000000000711, 33.74999999999999289, -3.750000000000000000 ) ) ;
#613 = CARTESIAN_POINT ( 'NONE',  ( 60.00000000000000000, 1.797044900979284448E-15, -10.00000000000000000 ) ) ;
#614 = VECTOR ( 'NONE', #3377, 1000.000000000000000 ) ;
#615 = PRESENTATION_STYLE_ASSIGNMENT (( #48916 ) ) ;
#616 = ORIENTED_EDGE ( 'NONE', *, *, #63159, .F. ) ;
#617 = DIRECTION ( 'NONE',  ( 1.000000000000000000, 0.000000000000000000, 0.000000000000000000 ) ) ;
#618 = VERTEX_POINT ( 'NONE', #65903 ) ;
#619 = CARTESIAN_POINT ( 'NONE',  ( -50.24292637653379501, 5.598654528085804216, 7.705886871421366635 ) ) ;
#620 = AXIS2_PLACEMENT_3D ( 'NONE', #68621, #62294, #58074 ) ;
#621 = DIRECTION ( 'NONE',  ( 1.000000000000000000, 0.000000000000000000, 0.000000000000000000 ) ) ;
#622 = DIRECTION ( 'NONE',  ( 0.000000000000000000, 1.712231188808094676E-15, 1.000000000000000000 ) ) ;
#623 = FACE_OUTER_BOUND ( 'NONE', #46827, .T. ) ;
#624 = CARTESIAN_POINT ( 'NONE',  ( -140.4549999999999841, 7.632228543268599452, -2.479861379858951942 ) ) ;
#625 = CARTESIAN_POINT ( 'NONE',  ( -6.887213563469350319, -2.329718218673038077, -6.070996185493596542 ) ) ;
#626 = CARTESIAN_POINT ( 'NONE',  ( 3.000000000000000444, 3.673940397442059868E-16, 7.500000000000000000 ) ) ;
#627 = PRESENTATION_LAYER_ASSIGNMENT (  '', '', ( #4029 ) ) ;
#628 = DIRECTION ( 'NONE',  ( 0.000000000000000000, 0.000000000000000000, 1.000000000000000000 ) ) ;
#629 = FILL_AREA_STYLE ('',( #37340 ) ) ;
#630 = CARTESIAN_POINT ( 'NONE',  ( 40.99999999999998579, 107.7459666924148252, 2.999999999999999556 ) ) ;
#631 = VERTEX_POINT ( 'NONE', #30590 ) ;
#632 = ORIENTED_EDGE ( 'NONE', *, *, #3874, .T. ) ;
#633 = FILL_AREA_STYLE_COLOUR ( '', #8694 ) ;
#634 = CARTESIAN_POINT ( 'NONE',  ( -58.10499999999999687, -6.826472737025115478, 4.959722759717900331 ) ) ;
#635 = EDGE_LOOP ( 'NONE', ( #19968, #33329, #40400, #68725 ) ) ;
#636 = PRESENTATION_STYLE_ASSIGNMENT (( #5968 ) ) ;
#637 =( NAMED_UNIT ( * ) SI_UNIT ( $, .STERADIAN. ) SOLID_ANGLE_UNIT ( ) );
#638 = DIRECTION ( 'NONE',  ( -1.000000000000000000, 0.000000000000000000, 0.000000000000000000 ) ) ;
#639 = CARTESIAN_POINT ( 'NONE',  ( 73.01088739851485343, 5.000000000000000000, 65.71817553072288831 ) ) ;
#640 = SPHERICAL_SURFACE ( 'NONE', #63217, 0.2500000000000000000 ) ;
#641 = CARTESIAN_POINT ( 'NONE',  ( -96.44292637653380496, -1.166476076187852838E-15, -9.524999999999991473 ) ) ;
#642 = ORIENTED_EDGE ( 'NONE', *, *, #21432, .T. ) ;
#643 = CARTESIAN_POINT ( 'NONE',  ( 26.25000000000001066, 18.74999999999997868, -3.750000000000000000 ) ) ;
#644 = DIRECTION ( 'NONE',  ( -0.000000000000000000, -0.000000000000000000, -1.000000000000000000 ) ) ;
#645 = PLANE ( 'NONE',  #55065 ) ;
#646 = ADVANCED_FACE ( 'NONE', ( #52096 ), #14421, .T. ) ;
#647 = CARTESIAN_POINT ( 'NONE',  ( -106.3449999999999989, 7.632228543268599452, -2.479861379858951942 ) ) ;
#648 = CARTESIAN_POINT ( 'NONE',  ( -9.058813317711338797, 158.3449999999999989, 2.943386871421373563 ) ) ;
#649 = CARTESIAN_POINT ( 'NONE',  ( -87.59499999999999886, 2.607480562269073321, 8.024999999999991473 ) ) ;
#650 = CARTESIAN_POINT ( 'NONE',  ( -9.827790563157511022E-16, 113.5570736234661666, 8.025000000000000355 ) ) ;
#651 = EDGE_CURVE ( 'NONE', #30219, #13126, #54768, .T. ) ;
#652 = AXIS2_PLACEMENT_3D ( 'NONE', #67205, #12333, #13740 ) ;
#653 = DIRECTION ( 'NONE',  ( 0.000000000000000000, 0.000000000000000000, 1.000000000000000000 ) ) ;
#654 = CARTESIAN_POINT ( 'NONE',  ( -13.50000000000000355, 28.24999999999998934, -4.000000000000000000 ) ) ;
#655 = ADVANCED_FACE ( 'NONE', ( #2147 ), #7166, .F. ) ;
#656 = CARTESIAN_POINT ( 'NONE',  ( 0.000000000000000000, -2.500000000000000000, 0.000000000000000000 ) ) ;
#657 = EDGE_LOOP ( 'NONE', ( #60359, #62367, #34898 ) ) ;
#658 = CARTESIAN_POINT ( 'NONE',  ( -125.9929263765338021, 8.102448949553171076, -5.886773742842744461 ) ) ;
#659 = CARTESIAN_POINT ( 'NONE',  ( -143.9950000000000045, -6.826472737025115478, 4.959722759717900331 ) ) ;
#660 = CARTESIAN_POINT ( 'NONE',  ( 60.00000000000000000, 1.797044900979284448E-15, 6.500000000000000000 ) ) ;
#661 =( GEOMETRIC_REPRESENTATION_CONTEXT ( 3 ) GLOBAL_UNCERTAINTY_ASSIGNED_CONTEXT ( ( #46852 ) ) GLOBAL_UNIT_ASSIGNED_CONTEXT ( ( #30764, #11314, #10968 ) ) REPRESENTATION_CONTEXT ( 'NONE', 'WORKASPACE' ) );
#662 = ADVANCED_FACE ( 'NONE', ( #5583 ), #47541, .F. ) ;
#663 = FILL_AREA_STYLE ('',( #53838 ) ) ;
#664 = ORIENTED_EDGE ( 'NONE', *, *, #56214, .F. ) ;
#665 = EDGE_LOOP ( 'NONE', ( #49715, #50790 ) ) ;
#666 = LINE ( 'NONE', #54539, #66260 ) ;
#667 = EDGE_CURVE ( 'NONE', #26396, #31733, #51240, .T. ) ;
#668 = CYLINDRICAL_SURFACE ( 'NONE', #49557, 1.000000000000000000 ) ;
#669 = CARTESIAN_POINT ( 'NONE',  ( -60.14292637653380069, 5.598654528085800663, -7.705886871421367523 ) ) ;
#670 = CARTESIAN_POINT ( 'NONE',  ( -23.71231517720798010, 117.4999999999999716, 9.500000000000000000 ) ) ;
#671 = SURFACE_SIDE_STYLE ('',( #26751 ) ) ;
#672 = ORIENTED_EDGE ( 'NONE', *, *, #13406, .T. ) ;
#673 = CARTESIAN_POINT ( 'NONE',  ( -136.5549999999999784, 0.000000000000000000, 8.024999999999991473 ) ) ;
#674 = ORIENTED_EDGE ( 'NONE', *, *, #55012, .F. ) ;
#675 = ORIENTED_EDGE ( 'NONE', *, *, #6557, .F. ) ;
#676 = CARTESIAN_POINT ( 'NONE',  ( 0.000000000000000000, 152.9429263765338192, -8.025000000000000355 ) ) ;
#677 = ORIENTED_EDGE ( 'NONE', *, *, #58749, .T. ) ;
#678 = CARTESIAN_POINT ( 'NONE',  ( 0.000000000000000000, 2.500000000000000000, 0.000000000000000000 ) ) ;
#679 = CARTESIAN_POINT ( 'NONE',  ( -1.166476076187854022E-15, 128.9449999999999648, 9.525000000000000355 ) ) ;
#680 = FACE_OUTER_BOUND ( 'NONE', #24766, .T. ) ;
#681 = VERTEX_POINT ( 'NONE', #58733 ) ;
#682 = CARTESIAN_POINT ( 'NONE',  ( -94.70707362346726654, -3.094860106636581509, -9.524999999986803800 ) ) ;
#683 = CARTESIAN_POINT ( 'NONE',  ( -3.094860106618434248, 126.9049999999999869, 9.525000000000000355 ) ) ;
#684 = CARTESIAN_POINT ( 'NONE',  ( -55.25499999999999545, -4.716976649647092401, 6.492361379858946790 ) ) ;
#685 = CARTESIAN_POINT ( 'NONE',  ( -119.5449999999999875, -7.632228543268600340, -2.479861379858950166 ) ) ;
#686 = CARTESIAN_POINT ( 'NONE',  ( 8.750000000000001776, 24.74999999999998579, -3.750000000000000000 ) ) ;
#687 = ORIENTED_EDGE ( 'NONE', *, *, #50668, .F. ) ;
#688 = CARTESIAN_POINT ( 'NONE',  ( 9.058813317711337021, 154.6549999999999727, 2.943386871421375783 ) ) ;
#689 = CARTESIAN_POINT ( 'NONE',  ( 20.00000000000001776, 15.00000000000000000, 29.68999999999999417 ) ) ;
#690 = COLOUR_RGB ( '', 0.40784314, 0.44705882, 0.49803922) ;
#691 = FILL_AREA_STYLE ('',( #44075 ) ) ;
#692 = DIRECTION ( 'NONE',  ( -0.000000000000000000, 0.000000000000000000, -1.000000000000000000 ) ) ;
#693 = AXIS2_PLACEMENT_3D ( 'NONE', #42691, #64090, #15943 ) ;
#694 = CYLINDRICAL_SURFACE ( 'NONE', #40795, 9.524999999999991473 ) ;
#695 = COLOUR_RGB ( '', 0.66274510, 0.83137255, 0.94901961) ;
#696 = ORIENTED_EDGE ( 'NONE', *, *, #23588, .F. ) ;
#697 = CARTESIAN_POINT ( 'NONE',  ( -33.26980702001004175, -9.137952730708951421, -3.992206423873327914 ) ) ;
#698 = CARTESIAN_POINT ( 'NONE',  ( 34.99999999999999289, 99.99999999999997158, -4.000000000000000000 ) ) ;
#699 = CARTESIAN_POINT ( 'NONE',  ( -174.5049999999999955, -6.826472737025115478, -4.959722759717899443 ) ) ;
#700 = ORIENTED_EDGE ( 'NONE', *, *, #2572, .T. ) ;
#701 = CARTESIAN_POINT ( 'NONE',  ( 1.518239866961975881, 111.9742333516235959, -7.925161578318684619 ) ) ;
#702 = EDGE_CURVE ( 'NONE', #13056, #23284, #24257, .T. ) ;
#703 =( LENGTH_UNIT ( ) NAMED_UNIT ( * ) SI_UNIT ( .MILLI., .METRE. ) );
#704 = CARTESIAN_POINT ( 'NONE',  ( 9.566487832665400148, -1.863712308906143811, 1.430357023834058161 ) ) ;
#705 = ORIENTED_EDGE ( 'NONE', *, *, #22573, .F. ) ;
#706 =( NAMED_UNIT ( * ) PLANE_ANGLE_UNIT ( ) SI_UNIT ( $, .RADIAN. ) );
#707 = B_SPLINE_CURVE_WITH_KNOTS ( 'NONE', 3,
 ( #58669, #36586, #58006, #10500 ),
 .UNSPECIFIED., .F., .F.,
 ( 4, 4 ),
 ( -1.393623722524901192E-05, 0.002366665958592541717 ),
 .UNSPECIFIED. ) ;
#708 = AXIS2_PLACEMENT_3D ( 'NONE', #33466, #2431, #60873 ) ;
#709 = FACE_OUTER_BOUND ( 'NONE', #7778, .T. ) ;
#710 = CARTESIAN_POINT ( 'NONE',  ( -84.50499999999999545, -6.826472737025115478, -4.959722759717899443 ) ) ;
#711 = EDGE_LOOP ( 'NONE', ( #27099, #281, #7477, #38071, #31799, #34233, #57951, #19950, #23018, #67509, #55080, #10516, #52770, #24683, #63743, #40061, #46422, #12294, #62526, #64426 ) ) ;
#712 =( NAMED_UNIT ( * ) PLANE_ANGLE_UNIT ( ) SI_UNIT ( $, .RADIAN. ) );
#713 = CARTESIAN_POINT ( 'NONE',  ( -31.74882385472577084, -8.677117902359153589, -1.656194935354385001 ) ) ;
#714 = CARTESIAN_POINT ( 'NONE',  ( 2.607480562268988500, 143.7070736234661581, 8.025000000000062528 ) ) ;
#715 = CARTESIAN_POINT ( 'NONE',  ( -64.55707362346618083, -1.166476076187852838E-15, -9.524999999999991473 ) ) ;
#716 = CARTESIAN_POINT ( 'NONE',  ( -4.250000000000001776, 21.99999999999998579, 3.750000000000000000 ) ) ;
#717 = ORIENTED_EDGE ( 'NONE', *, *, #61031, .T. ) ;
#719 = CYLINDRICAL_SURFACE ( 'NONE', #3216, 0.5000000000000004441 ) ;
#718 = SURFACE_STYLE_USAGE ( .BOTH. , #388 ) ;
#720 = ADVANCED_FACE ( 'NONE', ( #53122 ), #26361, .T. ) ;
#721 = CARTESIAN_POINT ( 'NONE',  ( -100.5549999999999926, 0.000000000000000000, 8.024999999999991473 ) ) ;
#722 = EDGE_CURVE ( 'NONE', #61387, #65027, #68863, .T. ) ;
#723 = CARTESIAN_POINT ( 'NONE',  ( 8.102448949553183510, 129.9950000000000045, -5.886773742842746238 ) ) ;
#724 = CARTESIAN_POINT ( 'NONE',  ( -120.1449999999999818, -4.716976649647092401, 6.492361379858946790 ) ) ;
#725 = DIRECTION ( 'NONE',  ( 0.000000000000000000, 0.000000000000000000, 1.000000000000000000 ) ) ;
#727 = LINE ( 'NONE', #38132, #38212 ) ;
#726 = LINE ( 'NONE', #12376, #44759 ) ;
#728 = EDGE_CURVE ( 'NONE', #56584, #51279, #30456, .T. ) ;
#729 = CARTESIAN_POINT ( 'NONE',  ( -151.1929263765337907, -10.01517768586948698, 6.132527647946031529E-16 ) ) ;
#730 = FILL_AREA_STYLE ('',( #12736 ) ) ;
#731 = CARTESIAN_POINT ( 'NONE',  ( -172.1949999999999648, 8.437984349512085203, -1.550032578732815448E-15 ) ) ;
#732 = ADVANCED_FACE ( 'NONE', ( #34413 ), #28058, .F. ) ;
#733 = VECTOR ( 'NONE', #5421, 1000.000000000000000 ) ;
#734 = CARTESIAN_POINT ( 'NONE',  ( -6.826472737025120807, 148.5070736234661410, -4.959722759717907437 ) ) ;
#735 = EDGE_CURVE ( 'NONE', #36722, #13211, #28412, .T. ) ;
#736 = CARTESIAN_POINT ( 'NONE',  ( -45.13832304515305083, -13.94474245745556473, 2.675331246431452925 ) ) ;
#737 = VERTEX_POINT ( 'NONE', #928 ) ;
#738 = ORIENTED_EDGE ( 'NONE', *, *, #6575, .F. ) ;
#739 = CARTESIAN_POINT ( 'NONE',  ( -68.24292637653380211, 5.598654528085804216, 7.705886871421366635 ) ) ;
#740 = SURFACE_SIDE_STYLE ('',( #49709 ) ) ;
#741 = ADVANCED_FACE ( 'NONE', ( #50258 ), #13012, .T. ) ;
#742 = CARTESIAN_POINT ( 'NONE',  ( 34.99999999999999289, 99.99999999999997158, 9.500000000000000000 ) ) ;
#743 = CARTESIAN_POINT ( 'NONE',  ( -25.00000000000000355, 36.75000000000000000, -3.000000000000000000 ) ) ;
#744 = CARTESIAN_POINT ( 'NONE',  ( -7.794228634059950700, -4.500000000000003553, 0.000000000000000000 ) ) ;
#745 = CARTESIAN_POINT ( 'NONE',  ( 3.673940397442060361E-16, -1.999999999999999556, -3.000000000000000444 ) ) ;
#746 = ORIENTED_EDGE ( 'NONE', *, *, #25332, .F. ) ;
#747 = CARTESIAN_POINT ( 'NONE',  ( -165.5049999999999955, -6.826472737025113702, -4.959722759717900331 ) ) ;
#748 = ORIENTED_EDGE ( 'NONE', *, *, #23356, .F. ) ;
#749 = DIRECTION ( 'NONE',  ( 0.000000000000000000, -1.000000000000000000, 0.000000000000000000 ) ) ;
#750 = SURFACE_SIDE_STYLE ('',( #61895 ) ) ;
#751 =( NAMED_UNIT ( * ) PLANE_ANGLE_UNIT ( ) SI_UNIT ( $, .RADIAN. ) );
#752 = CARTESIAN_POINT ( 'NONE',  ( -2.607480562269073765, 151.2070736234661581, -8.025000000000000355 ) ) ;
#753 = ORIENTED_EDGE ( 'NONE', *, *, #45483, .T. ) ;
#754 = DIRECTION ( 'NONE',  ( 0.000000000000000000, 0.000000000000000000, 1.000000000000000000 ) ) ;
#755 = CARTESIAN_POINT ( 'NONE',  ( -81.80499999999996419, -8.437984349512086979, 5.166775262442717831E-16 ) ) ;
#756 = CARTESIAN_POINT ( 'NONE',  ( 10.00000000000001776, 17.04554193418302788, 0.6691306063588585706 ) ) ;
#757 = ORIENTED_EDGE ( 'NONE', *, *, #23978, .T. ) ;
#758 =( NAMED_UNIT ( * ) PLANE_ANGLE_UNIT ( ) SI_UNIT ( $, .RADIAN. ) );
#759 =( NAMED_UNIT ( * ) SI_UNIT ( $, .STERADIAN. ) SOLID_ANGLE_UNIT ( ) );
#760 =( LENGTH_UNIT ( ) NAMED_UNIT ( * ) SI_UNIT ( .MILLI., .METRE. ) );
#761 =( NAMED_UNIT ( * ) PLANE_ANGLE_UNIT ( ) SI_UNIT ( $, .RADIAN. ) );
#762 = ORIENTED_EDGE ( 'NONE', *, *, #11363, .F. ) ;
#763 = CARTESIAN_POINT ( 'NONE',  ( -62.24499999999998323, -4.716976649647093289, -6.492361379858945902 ) ) ;
#764 = ORIENTED_EDGE ( 'NONE', *, *, #13916, .F. ) ;
#765 = DIRECTION ( 'NONE',  ( 0.8946296187927070820, 0.000000000000000000, -0.4468085106382997385 ) ) ;
#766 = EDGE_CURVE ( 'NONE', #54457, #36334, #60105, .T. ) ;
#767 = LINE ( 'NONE', #44165, #46999 ) ;
#768 = CARTESIAN_POINT ( 'NONE',  ( -45.00000000000000000, 8.189706559487571980, -5.659622407587006521 ) ) ;
#769 = ORIENTED_EDGE ( 'NONE', *, *, #2609, .T. ) ;
#770 = CARTESIAN_POINT ( 'NONE',  ( -74.50000000000000000, 7.768687147774684831, 6.999999999999999112 ) ) ;
#771 =( NAMED_UNIT ( * ) SI_UNIT ( $, .STERADIAN. ) SOLID_ANGLE_UNIT ( ) );
#772 = ORIENTED_EDGE ( 'NONE', *, *, #14294, .T. ) ;
#773 = COLOUR_RGB ( '', 0.31764706, 0.68627451, 0.89019608) ;
#774 = CARTESIAN_POINT ( 'NONE',  ( 45.00000000000000000, 10.69371294329215516, -6.262534692517951029 ) ) ;
#775 = DIRECTION ( 'NONE',  ( 0.000000000000000000, 0.000000000000000000, 1.000000000000000000 ) ) ;
#776 = CARTESIAN_POINT ( 'NONE',  ( -117.3549999999999898, -4.716976649647093289, -6.492361379858945902 ) ) ;
#777 = ORIENTED_EDGE ( 'NONE', *, *, #69425, .F. ) ;
#778 = PRESENTATION_STYLE_ASSIGNMENT (( #43137 ) ) ;
#779 = CARTESIAN_POINT ( 'NONE',  ( -30.38025804287905629, -8.499999999999996447, -2.000000000000000000 ) ) ;
#780 = CARTESIAN_POINT ( 'NONE',  ( -147.2070736234661865, 3.094860106618433360, 9.524999999999991473 ) ) ;
#781 = CARTESIAN_POINT ( 'NONE',  ( -5.598654528085808657, 134.6449999999999818, 7.705886871421373741 ) ) ;
#782 = CARTESIAN_POINT ( 'NONE',  ( -94.10707362346613536, 8.102448949553171076, -5.886773742842744461 ) ) ;
#783 = ADVANCED_FACE ( 'NONE', ( #49924 ), #48915, .T. ) ;
#784 = CARTESIAN_POINT ( 'NONE',  ( 22.00000000000002132, 42.00000000000000000, -29.68999999999999417 ) ) ;
#785 = ORIENTED_EDGE ( 'NONE', *, *, #43825, .T. ) ;
#786 =( LENGTH_UNIT ( ) NAMED_UNIT ( * ) SI_UNIT ( .MILLI., .METRE. ) );
#787 =( GEOMETRIC_REPRESENTATION_CONTEXT ( 3 ) GLOBAL_UNCERTAINTY_ASSIGNED_CONTEXT ( ( #12911 ) ) GLOBAL_UNIT_ASSIGNED_CONTEXT ( ( #5440, #36832, #37544 ) ) REPRESENTATION_CONTEXT ( 'NONE', 'WORKASPACE' ) );
#789 = SURFACE_SIDE_STYLE ('',( #20956 ) ) ;
#788 = PRESENTATION_STYLE_ASSIGNMENT (( #17764 ) ) ;
#790 = CONICAL_SURFACE ( 'NONE', #40211, 5.500000000000005329, 0.7853981633974309595 ) ;
#791 = EDGE_CURVE ( 'NONE', #1837, #31530, #38921, .T. ) ;
#792 = CARTESIAN_POINT ( 'NONE',  ( -128.1550000000000011, 7.632228543268600340, 2.479861379858949277 ) ) ;
#793 = CARTESIAN_POINT ( 'NONE',  ( -163.9429263765338192, 0.000000000000000000, 9.524999999999991473 ) ) ;
#794 = ADVANCED_FACE ( 'NONE', ( #22135 ), #59760, .T. ) ;
#795 = CARTESIAN_POINT ( 'NONE',  ( -147.2929263765342682, 3.094860106610630712, -9.525000000005659828 ) ) ;
#796 = FILL_AREA_STYLE_COLOUR ( '', #11802 ) ;
#797 = CARTESIAN_POINT ( 'NONE',  ( -147.1450000000000102, -4.716976649647092401, 6.492361379858946790 ) ) ;
#798 = CARTESIAN_POINT ( 'NONE',  ( -128.9950000000000045, -6.826472737025113702, 4.959722759717902107 ) ) ;
#799 = EDGE_LOOP ( 'NONE', ( #22119, #68329, #5663, #61545 ) ) ;
#800 = CARTESIAN_POINT ( 'NONE',  ( 45.00000000000000000, 10.69371294336137801, -4.000000000000001776 ) ) ;
#801 = EDGE_CURVE ( 'NONE', #31294, #36166, #8564, .T. ) ;
#802 =( LENGTH_UNIT ( ) NAMED_UNIT ( * ) SI_UNIT ( .MILLI., .METRE. ) );
#803 = UNCERTAINTY_MEASURE_WITH_UNIT (LENGTH_MEASURE( 1.000000000000000082E-05 ), #47965, 'distance_accuracy_value', 'NONE');
#804 = CARTESIAN_POINT ( 'NONE',  ( -180.7429263765338021, -5.598654528085803328, -7.705886871421366635 ) ) ;
#805 = SHAPE_REPRESENTATION_RELATIONSHIP ( 'NONE' , 'NONE' ,  #40670, #34624 ) ;
#806 = CARTESIAN_POINT ( 'NONE',  ( -59.84499999999998465, -7.632228543268599452, 2.479861379858951054 ) ) ;
#807 = EDGE_CURVE ( 'NONE', #48124, #69054, #39378, .T. ) ;
#808 = FILL_AREA_STYLE_COLOUR ( '', #61266 ) ;
#809 = CARTESIAN_POINT ( 'NONE',  ( 4.716976649647096842, 152.8570736234661638, 6.492361379858953896 ) ) ;
#810 = CARTESIAN_POINT ( 'NONE',  ( -56.89247722676302033, -8.499999999999992895, -0.08128311974370756865 ) ) ;
#811 = CARTESIAN_POINT ( 'NONE',  ( -76.40707362346616094, 3.094860106618428031, -9.524999999999993250 ) ) ;
#813 =( BOUNDED_CURVE ( )  B_SPLINE_CURVE ( 2, ( #63359, #19750, #9216, #41245, #67966, #8856, #68296, #24330, #46539, #57038, #30276 ),
 .UNSPECIFIED., .F., .F. ) 
 B_SPLINE_CURVE_WITH_KNOTS ( ( 3, 2, 2, 2, 2, 3 ),
 ( 0.6470588235294120194, 0.6529411764705884691, 0.6588235294117649188, 0.6647058823529413685, 0.6705882352941178182, 0.6764705882352943789 ),
 .UNSPECIFIED. ) 
 CURVE ( )  GEOMETRIC_REPRESENTATION_ITEM ( )  RATIONAL_B_SPLINE_CURVE ( ( 0.9999999999999981126, 0.9510565162951554186, 1.000000000000000000, 0.9510565162951535312, 1.000000000000000000, 0.9510565162951535312, 1.000000000000000000, 0.9510565162951535312, 1.000000000000000000, 0.9510565162951516438, 1.000000000000001776 ) ) 
 REPRESENTATION_ITEM ( '' )  );
#812 = CARTESIAN_POINT ( 'NONE',  ( -104.3929263765338078, 8.102448949553176405, 5.886773742842740909 ) ) ;
#814 = DIRECTION ( 'NONE',  ( -1.000000000000000000, -1.067062355321543253E-15, -3.102125002257870873E-16 ) ) ;
#815 = DIRECTION ( 'NONE',  ( 1.000000000000000000, 0.000000000000000000, 0.000000000000000000 ) ) ;
#816 = CIRCLE ( 'NONE', #58197, 1.000000000000000888 ) ;
#817 = CYLINDRICAL_SURFACE ( 'NONE', #68549, 8.025000000000000355 ) ;
#818 = DIRECTION ( 'NONE',  ( 0.000000000000000000, 0.000000000000000000, -1.000000000000000000 ) ) ;
#819 = STYLED_ITEM ( 'NONE', ( #43125 ), #50506 ) ;
#820 = CIRCLE ( 'NONE', #40245, 0.4999999999999994449 ) ;
#821 = DIRECTION ( 'NONE',  ( 0.000000000000000000, 1.000000000000000000, -0.000000000000000000 ) ) ;
#822 = EDGE_CURVE ( 'NONE', #3091, #51817, #9685, .T. ) ;
#823 = VERTEX_POINT ( 'NONE', #49569 ) ;
#824 = SURFACE_STYLE_FILL_AREA ( #32223 ) ;
#825 = DIRECTION ( 'NONE',  ( -1.000000000000000000, 0.000000000000000000, 0.000000000000000000 ) ) ;
#826 = ORIENTED_EDGE ( 'NONE', *, *, #29866, .F. ) ;
#827 = CARTESIAN_POINT ( 'NONE',  ( 57.00000000000000000, 16.00000000000000000, -65.00402776293825013 ) ) ;
#828 = COLOUR_RGB ( '', 0.09019608, 0.27058824, 0.51372549) ;
#829 = EDGE_CURVE ( 'NONE', #11857, #12490, #26513, .T. ) ;
#830 = CARTESIAN_POINT ( 'NONE',  ( 6.826472737025119919, 123.0070736234661695, 4.959722759717908325 ) ) ;
#831 = DIRECTION ( 'NONE',  ( 0.000000000000000000, -1.000000000000000000, 0.000000000000000000 ) ) ;
#832 = CARTESIAN_POINT ( 'NONE',  ( 74.65811388300841145, 19.88603796100278487, -6.000000000000000000 ) ) ;
#833 = AXIS2_PLACEMENT_3D ( 'NONE', #13505, #64129, #9660 ) ;
#834 = EDGE_LOOP ( 'NONE', ( #4085, #26069, #55060, #50281 ) ) ;
#835 = VERTEX_POINT ( 'NONE', #28774 ) ;
#836 = CARTESIAN_POINT ( 'NONE',  ( 15.98999599679679839, 146.4999999999999716, 7.000000000000000000 ) ) ;
#837 = EDGE_LOOP ( 'NONE', ( #3899, #15136, #7179, #58174 ) ) ;
#838 = DIRECTION ( 'NONE',  ( -0.000000000000000000, -0.000000000000000000, -1.000000000000000000 ) ) ;
#839 = DIRECTION ( 'NONE',  ( -0.000000000000000000, 1.000000000000000000, -0.000000000000000000 ) ) ;
#840 = LINE ( 'NONE', #28680, #24983 ) ;
#841 = CARTESIAN_POINT ( 'NONE',  ( -86.99499999999997613, -6.826472737025115478, 4.959722759717900331 ) ) ;
#842 = ORIENTED_EDGE ( 'NONE', *, *, #45785, .F. ) ;
#843 = CARTESIAN_POINT ( 'NONE',  ( 8.209205615337721085, 153.6217806035195110, -2.745863952952167342 ) ) ;
#844 = DIRECTION ( 'NONE',  ( 0.000000000000000000, 0.000000000000000000, 1.000000000000000000 ) ) ;
#845 = DIRECTION ( 'NONE',  ( 1.000000000000000000, 0.000000000000000000, -0.000000000000000000 ) ) ;
#846 = AXIS2_PLACEMENT_3D ( 'NONE', #22168, #7704, #65057 ) ;
#847 = EDGE_LOOP ( 'NONE', ( #26581, #32418, #27548, #41432 ) ) ;
#848 = CARTESIAN_POINT ( 'NONE',  ( 2.607480562269076430, 161.7929263765338135, -8.025000000000000355 ) ) ;
#849 = VERTEX_POINT ( 'NONE', #14704 ) ;
#850 = EDGE_CURVE ( 'NONE', #23192, #29847, #37737, .T. ) ;
#851 = CARTESIAN_POINT ( 'NONE',  ( -7.766391886667105560, 1.733608113333017453, -0.5482146608018624301 ) ) ;
#852 = ORIENTED_EDGE ( 'NONE', *, *, #10725, .F. ) ;
#853 = CARTESIAN_POINT ( 'NONE',  ( 72.49999999999998579, 64.07124727947029896, -10.00000000000000000 ) ) ;
#854 = CARTESIAN_POINT ( 'NONE',  ( 0.000000000000000000, 0.000000000000000000, 79.00402776293826435 ) ) ;
#855 = SURFACE_STYLE_FILL_AREA ( #64264 ) ;
#856 = CIRCLE ( 'NONE', #40278, 16.44999999999999218 ) ;
#857 = CARTESIAN_POINT ( 'NONE',  ( -179.7570736234661979, -5.598654528085801552, 7.705886871421367523 ) ) ;
#858 = CARTESIAN_POINT ( 'NONE',  ( -75.00000000000000000, 7.768687147774688384, -6.999999999999999112 ) ) ;
#859 = STYLED_ITEM ( 'NONE', ( #4112 ), #4071 ) ;
#860 = ADVANCED_FACE ( 'NONE', ( #67456 ), #46041, .T. ) ;
#861 = CARTESIAN_POINT ( 'NONE',  ( -3.535366420403587284, 9.000000000000008882, 0.6617903051486830890 ) ) ;
#862 = CARTESIAN_POINT ( 'NONE',  ( -115.0429263765338135, -9.058813317711329915, -2.943386871421370898 ) ) ;
#863 = ORIENTED_EDGE ( 'NONE', *, *, #33369, .F. ) ;
#864 = MECHANICAL_DESIGN_GEOMETRIC_PRESENTATION_REPRESENTATION (  '', ( #31253 ), #48145 ) ;
#865 = CARTESIAN_POINT ( 'NONE',  ( -162.2929263765340977, 3.094860106613655404, -9.525000000003460698 ) ) ;
#866 = STYLED_ITEM ( 'NONE', ( #49101 ), #66381 ) ;
#867 = CARTESIAN_POINT ( 'NONE',  ( 36.00000000000002842, 5.000000000000000000, -32.00402776293825724 ) ) ;
#868 = CARTESIAN_POINT ( 'NONE',  ( 16.00000000000001776, 42.00000000000000000, 29.68999999999999417 ) ) ;
#869 = ORIENTED_EDGE ( 'NONE', *, *, #37055, .F. ) ;
#870 =( NAMED_UNIT ( * ) PLANE_ANGLE_UNIT ( ) SI_UNIT ( $, .RADIAN. ) );
#871 = EDGE_CURVE ( 'NONE', #17912, #22405, #53502, .T. ) ;
#872 = CARTESIAN_POINT ( 'NONE',  ( -158.6050000000000182, 6.826472737025113702, -4.959722759717902107 ) ) ;
#873 = DIRECTION ( 'NONE',  ( -1.000000000000000000, -0.000000000000000000, -0.000000000000000000 ) ) ;
#874 = CARTESIAN_POINT ( 'NONE',  ( -183.9431579317532055, -8.604615092590435665, -0.1013726718049147574 ) ) ;
#875 = CARTESIAN_POINT ( 'NONE',  ( -172.6449999999999818, 4.716976649647091513, -6.492361379858946790 ) ) ;
#876 = AXIS2_PLACEMENT_3D ( 'NONE', #62738, #3624, #19840 ) ;
#877 = CARTESIAN_POINT ( 'NONE',  ( -170.9950000000000045, -6.826472737025113702, 4.959722759717902107 ) ) ;
#878 = ORIENTED_EDGE ( 'NONE', *, *, #36806, .F. ) ;
#879 = VECTOR ( 'NONE', #31549, 1000.000000000000000 ) ;
#880 = CARTESIAN_POINT ( 'NONE',  ( -90.29292637653378506, 3.094860106618428031, -9.524999999999993250 ) ) ;
#881 = DIRECTION ( 'NONE',  ( 1.000000000000000000, 0.000000000000000000, 0.000000000000000000 ) ) ;
#882 = CARTESIAN_POINT ( 'NONE',  ( -86.15499999999998693, 7.632228543268600340, 2.479861379858949277 ) ) ;
#883 = CARTESIAN_POINT ( 'NONE',  ( 24.29181562774721215, 24.88364009055414883, 27.31771990072506640 ) ) ;
#885 = LINE ( 'NONE', #28364, #23641 ) ;
#884 = AXIS2_PLACEMENT_3D ( 'NONE', #23527, #66093, #8054 ) ;
#886 = EDGE_CURVE ( 'NONE', #36075, #3129, #2705, .T. ) ;
#887 = CARTESIAN_POINT ( 'NONE',  ( -85.19499999999999318, 8.437984349512086979, -1.550032578732815448E-15 ) ) ;
#888 = CARTESIAN_POINT ( 'NONE',  ( -8.102448949553181734, 138.6049999999999329, 5.886773742842747126 ) ) ;
#889 = CARTESIAN_POINT ( 'NONE',  ( -134.1570736234661751, -9.058813317711329915, -2.943386871421370898 ) ) ;
#890 = CARTESIAN_POINT ( 'NONE',  ( 7.186760109404651153, 154.4703037126919867, 6.248938465618627980 ) ) ;
#891 = UNCERTAINTY_MEASURE_WITH_UNIT (LENGTH_MEASURE( 1.000000000000000082E-05 ), #17075, 'distance_accuracy_value', 'NONE');
#892 = DIRECTION ( 'NONE',  ( 1.000000000000000000, -0.000000000000000000, 0.000000000000000000 ) ) ;
#893 = ORIENTED_EDGE ( 'NONE', *, *, #58691, .T. ) ;
#894 = CARTESIAN_POINT ( 'NONE',  ( 14.09999999999999609, 11.99999999999999289, 3.500000000000004885 ) ) ;
#895 = CARTESIAN_POINT ( 'NONE',  ( -51.44292637653380496, -1.166476076187852838E-15, -9.524999999999991473 ) ) ;
#896 = AXIS2_PLACEMENT_3D ( 'NONE', #40176, #45807, #61574 ) ;
#897 = DIRECTION ( 'NONE',  ( 0.000000000000000000, 0.000000000000000000, 1.000000000000000000 ) ) ;
#898 = ORIENTED_EDGE ( 'NONE', *, *, #4253, .T. ) ;
#899 = MECHANICAL_DESIGN_GEOMETRIC_PRESENTATION_REPRESENTATION (  '', ( #50407 ), #5477 ) ;
#900 = ORIENTED_EDGE ( 'NONE', *, *, #28247, .T. ) ;
#901 = CYLINDRICAL_SURFACE ( 'NONE', #61063, 5.000000000000004441 ) ;
#902 = CYLINDRICAL_SURFACE ( 'NONE', #35389, 1.000000000000000888 ) ;
#903 = COLOUR_RGB ( '', 0.31764706, 0.68627451, 0.89019608) ;
#904 =( BOUNDED_CURVE ( )  B_SPLINE_CURVE ( 3, ( #64172, #16030, #47011, #64538 ),
 .UNSPECIFIED., .F., .F. ) 
 B_SPLINE_CURVE_WITH_KNOTS ( ( 4, 4 ),
 ( 0.000000000000000000, 1.570796326794899223 ),
 .UNSPECIFIED. ) 
 CURVE ( )  GEOMETRIC_REPRESENTATION_ITEM ( )  RATIONAL_B_SPLINE_CURVE ( ( 1.000000000000000000, 0.8047378541243643824, 0.8047378541243643824, 1.000000000000000000 ) ) 
 REPRESENTATION_ITEM ( '' )  );
#905 = MECHANICAL_DESIGN_GEOMETRIC_PRESENTATION_REPRESENTATION (  '', ( #66119 ), #43731 ) ;
#906 = DIRECTION ( 'NONE',  ( 0.000000000000000000, -1.000000000000000000, 0.000000000000000000 ) ) ;
#907 =( GEOMETRIC_REPRESENTATION_CONTEXT ( 3 ) GLOBAL_UNCERTAINTY_ASSIGNED_CONTEXT ( ( #51593 ) ) GLOBAL_UNIT_ASSIGNED_CONTEXT ( ( #5704, #16660, #55985 ) ) REPRESENTATION_CONTEXT ( 'NONE', 'WORKASPACE' ) );
#908 = EDGE_LOOP ( 'NONE', ( #67803, #57612, #55838, #66761 ) ) ;
#909 = CARTESIAN_POINT ( 'NONE',  ( -115.5549999999999926, 0.000000000000000000, 8.024999999999991473 ) ) ;
#910 = EDGE_LOOP ( 'NONE', ( #58286, #13364, #33728, #51994 ) ) ;
#911 = SURFACE_STYLE_FILL_AREA ( #38685 ) ;
#912 = CARTESIAN_POINT ( 'NONE',  ( 1.000000000000000000, 1.000000000000000222, 3.000000000000000000 ) ) ;
#913 = ORIENTED_EDGE ( 'NONE', *, *, #57118, .F. ) ;
#914 = CARTESIAN_POINT ( 'NONE',  ( -57.14292637653378648, 5.598654528085800663, -7.705886871421367523 ) ) ;
#915 = CARTESIAN_POINT ( 'NONE',  ( -6.938426666069064552, -2.291132984336068379, 1.982292489777641720 ) ) ;
#916 = EDGE_LOOP ( 'NONE', ( #4799, #6621, #31272, #29643 ) ) ;
#917 = AXIS2_PLACEMENT_3D ( 'NONE', #37172, #21275, #37530 ) ;
#918 = LINE ( 'NONE', #66052, #53474 ) ;
#919 = CARTESIAN_POINT ( 'NONE',  ( 10.01517768586949231, 156.6949999999999932, 1.839758294383810543E-15 ) ) ;
#920 = CARTESIAN_POINT ( 'NONE',  ( 0.000000000000000000, 0.000000000000000000, 12.50000000000000000 ) ) ;
#921 = ORIENTED_EDGE ( 'NONE', *, *, #6986, .F. ) ;
#922 = ORIENTED_EDGE ( 'NONE', *, *, #54460, .T. ) ;
#923 = CARTESIAN_POINT ( 'NONE',  ( 32.00000000000002132, 15.00000000000000000, 79.00402776293823592 ) ) ;
#924 = CARTESIAN_POINT ( 'NONE',  ( -8.246138225238285102, -2.499999999999994671, -3.717269627651451191 ) ) ;
#925 = EDGE_LOOP ( 'NONE', ( #34844, #14529, #43213, #21160 ) ) ;
#926 = CARTESIAN_POINT ( 'NONE',  ( -2.607480562269073765, 132.0929263765338249, -8.025000000000000355 ) ) ;
#927 = CARTESIAN_POINT ( 'NONE',  ( 45.50000000000000000, -1.469576158976824618E-14, 10.00000000000000000 ) ) ;
#928 = CARTESIAN_POINT ( 'NONE',  ( -12.74999999999999822, -4.000000000000000000, 7.000000000000001776 ) ) ;
#929 = CARTESIAN_POINT ( 'NONE',  ( 12.00000000000001776, 14.00000000000000000, 29.68999999999999417 ) ) ;
#930 = DIRECTION ( 'NONE',  ( 1.000000000000000000, 0.000000000000000000, 0.000000000000000000 ) ) ;
#931 = ORIENTED_EDGE ( 'NONE', *, *, #25197, .F. ) ;
#932 = ADVANCED_FACE ( 'NONE', ( #19253 ), #67118, .F. ) ;
#933 = DIRECTION ( 'NONE',  ( -0.000000000000000000, -0.000000000000000000, -1.000000000000000000 ) ) ;
#934 = ORIENTED_EDGE ( 'NONE', *, *, #5792, .T. ) ;
#935 = CARTESIAN_POINT ( 'NONE',  ( -53.39292637653380069, 8.102448949553176405, 5.886773742842740909 ) ) ;
#936 =( LENGTH_UNIT ( ) NAMED_UNIT ( * ) SI_UNIT ( .MILLI., .METRE. ) );
#937 = DIRECTION ( 'NONE',  ( -1.000000000000000000, -0.000000000000000000, -0.000000000000000000 ) ) ;
#938 = CARTESIAN_POINT ( 'NONE',  ( -158.9070736234665162, -3.094860106613422257, 9.525000000003631229 ) ) ;
#939 = CARTESIAN_POINT ( 'NONE',  ( -138.6550000000000011, -7.632228543268600340, -2.479861379858950166 ) ) ;
#940 =( LENGTH_UNIT ( ) NAMED_UNIT ( * ) SI_UNIT ( .MILLI., .METRE. ) );
#941 = UNCERTAINTY_MEASURE_WITH_UNIT (LENGTH_MEASURE( 1.000000000000000082E-05 ), #61585, 'distance_accuracy_value', 'NONE');
#942 = ORIENTED_EDGE ( 'NONE', *, *, #69657, .F. ) ;
#943 = AXIS2_PLACEMENT_3D ( 'NONE', #27160, #59885, #725 ) ;
#944 = CARTESIAN_POINT ( 'NONE',  ( 41.61212508608636540, 107.5086115709064956, 4.000000005149253468 ) ) ;
#945 = ORIENTED_EDGE ( 'NONE', *, *, #68006, .F. ) ;
#946 = EDGE_LOOP ( 'NONE', ( #19427, #8776, #15362 ) ) ;
#947 = CARTESIAN_POINT ( 'NONE',  ( -17.41059898028469277, 6.938893903907228378E-15, 12.50000000000000000 ) ) ;
#948 = MECHANICAL_DESIGN_GEOMETRIC_PRESENTATION_REPRESENTATION (  '', ( #61662 ), #15669 ) ;
#949 = CARTESIAN_POINT ( 'NONE',  ( -51.50707362346618368, 8.102448949553176405, 5.886773742842740909 ) ) ;
#950 = CARTESIAN_POINT ( 'NONE',  ( -52.85499999999998266, 4.716976649647094177, 6.492361379858945902 ) ) ;
#951 = ORIENTED_EDGE ( 'NONE', *, *, #31614, .F. ) ;
#952 = CARTESIAN_POINT ( 'NONE',  ( -20.57648123223228254, 154.9999999999999716, -10.27659574468085069 ) ) ;
#953 = ADVANCED_FACE ( 'NONE', ( #51633 ), #51996, .T. ) ;
#954 = FILL_AREA_STYLE ('',( #63683 ) ) ;
#955 = CARTESIAN_POINT ( 'NONE',  ( 44.50000000000000000, 99.99999999999998579, -3.500000000000000000 ) ) ;
#956 = EDGE_CURVE ( 'NONE', #7813, #35108, #56198, .T. ) ;
#957 = AXIS2_PLACEMENT_3D ( 'NONE', #20614, #36831, #10071 ) ;
#958 = AXIS2_PLACEMENT_3D ( 'NONE', #57886, #42783, #47358 ) ;
#959 = ADVANCED_FACE ( 'NONE', ( #41450 ), #57247, .F. ) ;
#960 = DIRECTION ( 'NONE',  ( 1.000000000000000000, 0.000000000000000000, 0.000000000000000000 ) ) ;
#961 = PLANE ( 'NONE',  #9583 ) ;
#962 = AXIS2_PLACEMENT_3D ( 'NONE', #56401, #8236, #63071 ) ;
#963 = ORIENTED_EDGE ( 'NONE', *, *, #66472, .F. ) ;
#964 = AXIS2_PLACEMENT_3D ( 'NONE', #69437, #21227, #422 ) ;
#965 = EDGE_CURVE ( 'NONE', #65527, #64066, #10468, .T. ) ;
#966 = FACE_OUTER_BOUND ( 'NONE', #59717, .T. ) ;
#967 = CARTESIAN_POINT ( 'NONE',  ( 31.00000000000000355, 50.00000000000000000, -60.00000000000000711 ) ) ;
#968 = CARTESIAN_POINT ( 'NONE',  ( -79.55707362346616662, -1.166476076187852838E-15, -9.524999999999991473 ) ) ;
#969 =( GEOMETRIC_REPRESENTATION_CONTEXT ( 3 ) GLOBAL_UNCERTAINTY_ASSIGNED_CONTEXT ( ( #46175 ) ) GLOBAL_UNIT_ASSIGNED_CONTEXT ( ( #23556, #2764, #12655 ) ) REPRESENTATION_CONTEXT ( 'NONE', 'WORKASPACE' ) );
#970 = CYLINDRICAL_SURFACE ( 'NONE', #33737, 0.2500000000000002220 ) ;
#971 = ADVANCED_FACE ( 'NONE', ( #15752 ), #57965, .T. ) ;
#972 = CARTESIAN_POINT ( 'NONE',  ( -113.2449999999999903, -4.716976649647093289, -6.492361379858945902 ) ) ;
#973 = CARTESIAN_POINT ( 'NONE',  ( 5.598654528085809545, 160.1449999999999818, -7.705886871421373741 ) ) ;
#974 = CARTESIAN_POINT ( 'NONE',  ( -81.29499999999998749, -2.607480562269069768, 8.024999999999991473 ) ) ;
#975 = PRESENTATION_LAYER_ASSIGNMENT (  '', '', ( #51578 ) ) ;
#976 = DIRECTION ( 'NONE',  ( 0.000000000000000000, 0.000000000000000000, -1.000000000000000000 ) ) ;
#977 = UNCERTAINTY_MEASURE_WITH_UNIT (LENGTH_MEASURE( 1.000000000000000082E-05 ), #63393, 'distance_accuracy_value', 'NONE');
#978 = CIRCLE ( 'NONE', #69598, 3.000000000000000444 ) ;
#980 = SURFACE_STYLE_FILL_AREA ( #27768 ) ;
#979 =( REPRESENTATION_RELATIONSHIP ('NONE','NONE', #5102, #67568 ) REPRESENTATION_RELATIONSHIP_WITH_TRANSFORMATION ( #5376 )SHAPE_REPRESENTATION_RELATIONSHIP( ) );
#981 = EDGE_LOOP ( 'NONE', ( #30979, #51142, #59233 ) ) ;
#982 = CARTESIAN_POINT ( 'NONE',  ( -125.8429263765337964, 9.058813317711329915, -2.943386871421373119 ) ) ;
#983 = DIRECTION ( 'NONE',  ( 1.000000000000000000, 0.000000000000000000, 0.000000000000000000 ) ) ;
#984 = CARTESIAN_POINT ( 'NONE',  ( -148.7950000000000159, 2.607480562269068880, -8.024999999999993250 ) ) ;
#985 = DIRECTION ( 'NONE',  ( 0.000000000000000000, 1.000000000000000000, -0.000000000000000000 ) ) ;
#986 = CIRCLE ( 'NONE', #40403, 0.2500000000000002220 ) ;
#987 = CARTESIAN_POINT ( 'NONE',  ( -195.0000000000000000, 0.000000000000000000, 0.000000000000000000 ) ) ;
#988 = CARTESIAN_POINT ( 'NONE',  ( 4.500000000000002665, 22.24999999999998579, 4.000000000000000000 ) ) ;
#989 = ORIENTED_EDGE ( 'NONE', *, *, #32331, .T. ) ;
#990 = ORIENTED_EDGE ( 'NONE', *, *, #25548, .F. ) ;
#991 = PRESENTATION_LAYER_ASSIGNMENT (  '', '', ( #22417 ) ) ;
#992 = PRESENTATION_LAYER_ASSIGNMENT (  '', '', ( #63982 ) ) ;
#993 = CARTESIAN_POINT ( 'NONE',  ( 74.89452121010485541, 0.000000000000000000, -66.39042820928574429 ) ) ;
#994 = CIRCLE ( 'NONE', #49400, 9.524999999999991473 ) ;
#995 =( NAMED_UNIT ( * ) PLANE_ANGLE_UNIT ( ) SI_UNIT ( $, .RADIAN. ) );
#996 = CARTESIAN_POINT ( 'NONE',  ( 31.00000000000000000, 42.00000000000000000, -79.00402776293826435 ) ) ;
#997 = CARTESIAN_POINT ( 'NONE',  ( -50.30707362346617373, -10.01517768586948698, 6.132527647946031529E-16 ) ) ;
#998 = COLOUR_RGB ( '', 0.40784314, 0.44705882, 0.49803922) ;
#999 = DIRECTION ( 'NONE',  ( 0.000000000000000000, 0.000000000000000000, 1.000000000000000000 ) ) ;
#1000 = EDGE_LOOP ( 'NONE', ( #21761, #35276, #54792, #50255 ) ) ;
#1001 = CARTESIAN_POINT ( 'NONE',  ( -145.7050000000000125, 2.607480562269072433, 8.024999999999991473 ) ) ;
#1002 = ORIENTED_EDGE ( 'NONE', *, *, #18036, .T. ) ;
#1003 = ORIENTED_EDGE ( 'NONE', *, *, #1274, .T. ) ;
#1004 = CARTESIAN_POINT ( 'NONE',  ( 22.00000000000000711, 50.00000000000000000, -46.00000000000000000 ) ) ;
#1005 = CARTESIAN_POINT ( 'NONE',  ( 6.123233995736766282E-16, -1.999999999999995337, -5.000000000000000000 ) ) ;
#1006 = ORIENTED_EDGE ( 'NONE', *, *, #6104, .T. ) ;
#1007 = PRESENTATION_LAYER_ASSIGNMENT (  '', '', ( #54996 ) ) ;
#1008 = TOROIDAL_SURFACE ( 'NONE', #8984, 0.7500000000000000000, 0.2500000000000000000 ) ;
#1009 = CARTESIAN_POINT ( 'NONE',  ( -55.09946728320541354, -8.921903058037614187, -1.645666659141976407 ) ) ;
#1010 = CIRCLE ( 'NONE', #35957, 1.000000000000000000 ) ;
#1011 = CARTESIAN_POINT ( 'NONE',  ( -10.01517768586949231, 128.1950000000000216, -6.132527647946036459E-16 ) ) ;
#1012 = VERTEX_POINT ( 'NONE', #58990 ) ;
#1013 = DIRECTION ( 'NONE',  ( 0.000000000000000000, 0.000000000000000000, 1.000000000000000000 ) ) ;
#1014 = CARTESIAN_POINT ( 'NONE',  ( 3.094860106618431583, 130.2049999999999841, 9.525000000000000355 ) ) ;
#1015 = CARTESIAN_POINT ( 'NONE',  ( -55.55499999999999261, 0.000000000000000000, 8.024999999999991473 ) ) ;
#1016 = CARTESIAN_POINT ( 'NONE',  ( -118.0450000000000017, 7.632228543268600340, 2.479861379858949277 ) ) ;
#1017 = MECHANICAL_DESIGN_GEOMETRIC_PRESENTATION_REPRESENTATION (  '', ( #69588 ), #41554 ) ;
#1018 = CARTESIAN_POINT ( 'NONE',  ( -53.26511667252331250, -9.007918291183415249, 5.430249810268242605 ) ) ;
#1019 = ORIENTED_EDGE ( 'NONE', *, *, #17957, .F. ) ;
#1020 = CARTESIAN_POINT ( 'NONE',  ( -9.058813317711338797, 159.4549999999999841, 2.943386871421373563 ) ) ;
#1021 = DIRECTION ( 'NONE',  ( -0.000000000000000000, -0.000000000000000000, -1.000000000000000000 ) ) ;
#1022 = UNCERTAINTY_MEASURE_WITH_UNIT (LENGTH_MEASURE( 1.000000000000000082E-05 ), #27650, 'distance_accuracy_value', 'NONE');
#1023 = AXIS2_PLACEMENT_3D ( 'NONE', #41776, #45999, #51959 ) ;
#1024 =( NAMED_UNIT ( * ) PLANE_ANGLE_UNIT ( ) SI_UNIT ( $, .RADIAN. ) );
#1025 = CARTESIAN_POINT ( 'NONE',  ( 6.330869393641158638, 43.00000000000000000, 28.38386403503541899 ) ) ;
#1026 = CARTESIAN_POINT ( 'NONE',  ( 0.000000000000000000, 2.299999999999999822, 0.000000000000000000 ) ) ;
#1027 = ADVANCED_FACE ( 'NONE', ( #10803 ), #9781, .T. ) ;
#1028 = CARTESIAN_POINT ( 'NONE',  ( 20.71231517720798010, 109.9999999999999858, 9.500000000000000000 ) ) ;
#1029 = EDGE_LOOP ( 'NONE', ( #6531, #47187, #15663, #64925, #17552 ) ) ;
#1030 = AXIS2_PLACEMENT_3D ( 'NONE', #28182, #1061, #1427 ) ;
#1031 = LINE ( 'NONE', #22576, #25461 ) ;
#1032 = FACE_OUTER_BOUND ( 'NONE', #23249, .T. ) ;
#1033 = CARTESIAN_POINT ( 'NONE',  ( -172.8550000000000182, 4.716976649647094177, 6.492361379858945902 ) ) ;
#1034 = VERTEX_POINT ( 'NONE', #15419 ) ;
#1035 = CARTESIAN_POINT ( 'NONE',  ( 62.24999999999998579, 33.99999999999999289, -3.750000000000000000 ) ) ;
#1036 = UNCERTAINTY_MEASURE_WITH_UNIT (LENGTH_MEASURE( 1.000000000000000082E-05 ), #23838, 'distance_accuracy_value', 'NONE');
#1037 = PRESENTATION_LAYER_ASSIGNMENT (  '', '', ( #31420 ) ) ;
#1038 = EDGE_CURVE ( 'NONE', #30672, #41120, #15077, .T. ) ;
#1039 = COLOUR_RGB ( '', 0.31764706, 0.68627451, 0.89019608) ;
#1040 = FACE_OUTER_BOUND ( 'NONE', #32390, .T. ) ;
#1041 =( NAMED_UNIT ( * ) PLANE_ANGLE_UNIT ( ) SI_UNIT ( $, .RADIAN. ) );
#1042 =( NAMED_UNIT ( * ) SI_UNIT ( $, .STERADIAN. ) SOLID_ANGLE_UNIT ( ) );
#1043 = CARTESIAN_POINT ( 'NONE',  ( 179.4361977533490347, 0.9999999999999991118, -103.7004518695263044 ) ) ;
#1044 = VERTEX_POINT ( 'NONE', #36876 ) ;
#1045 = AXIS2_PLACEMENT_3D ( 'NONE', #18634, #23539, #28450 ) ;
#1046 = EDGE_CURVE ( 'NONE', #39125, #41202, #52649, .T. ) ;
#1047 = SURFACE_SIDE_STYLE ('',( #65491 ) ) ;
#1048 = CARTESIAN_POINT ( 'NONE',  ( -82.55499999999999261, 0.000000000000000000, 8.024999999999991473 ) ) ;
#1049 = ORIENTED_EDGE ( 'NONE', *, *, #65191, .F. ) ;
#1050 = DIRECTION ( 'NONE',  ( 0.000000000000000000, 0.000000000000000000, 1.000000000000000000 ) ) ;
#1051 = EDGE_CURVE ( 'NONE', #31668, #16942, #44246, .T. ) ;
#1052 = AXIS2_PLACEMENT_3D ( 'NONE', #6461, #27897, #49403 ) ;
#1053 = COLOUR_RGB ( '', 0.66274510, 0.83137255, 0.94901961) ;
#1054 = FILL_AREA_STYLE_COLOUR ( '', #68815 ) ;
#1055 = DIRECTION ( 'NONE',  ( 0.000000000000000000, 0.000000000000000000, -1.000000000000000000 ) ) ;
#1056 = CARTESIAN_POINT ( 'NONE',  ( -57.05707362346618083, 0.000000000000000000, 9.524999999999991473 ) ) ;
#1057 = EDGE_CURVE ( 'NONE', #33883, #50178, #6563, .T. ) ;
#1058 =( NAMED_UNIT ( * ) PLANE_ANGLE_UNIT ( ) SI_UNIT ( $, .RADIAN. ) );
#1059 = ORIENTED_EDGE ( 'NONE', *, *, #66159, .T. ) ;
#1060 = PRESENTATION_STYLE_ASSIGNMENT (( #22250 ) ) ;
#1061 = DIRECTION ( 'NONE',  ( -0.000000000000000000, -1.000000000000000000, -0.000000000000000000 ) ) ;
#1062 = CARTESIAN_POINT ( 'NONE',  ( -100.7049999999999841, 2.607480562269073321, 8.024999999999991473 ) ) ;
#1063 = CARTESIAN_POINT ( 'NONE',  ( 5.598654528085809545, 127.1449999999999818, -7.705886871421373741 ) ) ;
#1064 = CARTESIAN_POINT ( 'NONE',  ( -115.1949999999999932, 8.437984349512085203, -1.550032578732815448E-15 ) ) ;
#1065 = AXIS2_PLACEMENT_3D ( 'NONE', #36610, #68921, #58024 ) ;
#1066 = AXIS2_PLACEMENT_3D ( 'NONE', #10576, #69647, #37700 ) ;
#1067 = CARTESIAN_POINT ( 'NONE',  ( -71.49999999999998579, 119.9999999999997868, -7.500000000000000000 ) ) ;
#1068 = CIRCLE ( 'NONE', #41598, 3.499999999999997780 ) ;
#1069 = CARTESIAN_POINT ( 'NONE',  ( -18.30291578181160972, 11.39569540983528206, -3.767653220740891484 ) ) ;
#1070 = CARTESIAN_POINT ( 'NONE',  ( -152.8429263765337964, 9.058813317711329915, -2.943386871421373119 ) ) ;
#1071 =( NAMED_UNIT ( * ) PLANE_ANGLE_UNIT ( ) SI_UNIT ( $, .RADIAN. ) );
#1072 = CARTESIAN_POINT ( 'NONE',  ( -172.4950000000000045, 6.826472737025113702, -4.959722759717902107 ) ) ;
#1073 = CARTESIAN_POINT ( 'NONE',  ( 39.74999999999999289, 18.99999999999997868, 4.000000000000000000 ) ) ;
#1074 = VECTOR ( 'NONE', #4879, 1000.000000000000000 ) ;
#1075 = CIRCLE ( 'NONE', #56169, 4.750000000000000000 ) ;
#1076 = CARTESIAN_POINT ( 'NONE',  ( 7.335726704534227594, 5.294148637306920868, 0.03572125916566718656 ) ) ;
#1077 = ORIENTED_EDGE ( 'NONE', *, *, #50915, .F. ) ;
#1078 = DIRECTION ( 'NONE',  ( 0.000000000000000000, 1.000000000000000000, 0.000000000000000000 ) ) ;
#1079 = DIRECTION ( 'NONE',  ( 0.000000000000000000, -1.000000000000000000, 0.000000000000000000 ) ) ;
#1080 = ORIENTED_EDGE ( 'NONE', *, *, #9314, .F. ) ;
#1081 = CARTESIAN_POINT ( 'NONE',  ( -70.64292637653379359, -5.598654528085801552, 7.705886871421367523 ) ) ;
#1082 = AXIS2_PLACEMENT_3D ( 'NONE', #60399, #892, #22438 ) ;
#1083 = CARTESIAN_POINT ( 'NONE',  ( -45.91547277936962246, 9.430195807687217879, 6.039758700367571898 ) ) ;
#1084 = CARTESIAN_POINT ( 'NONE',  ( -195.0000000000000000, 0.000000000000000000, 0.000000000000000000 ) ) ;
#1085 = EDGE_CURVE ( 'NONE', #61213, #35189, #33302, .T. ) ;
#1086 =( GEOMETRIC_REPRESENTATION_CONTEXT ( 3 ) GLOBAL_UNCERTAINTY_ASSIGNED_CONTEXT ( ( #3714 ) ) GLOBAL_UNIT_ASSIGNED_CONTEXT ( ( #68652, #21846, #44387 ) ) REPRESENTATION_CONTEXT ( 'NONE', 'WORKASPACE' ) );
#1087 = CARTESIAN_POINT ( 'NONE',  ( 27.00000000000001776, 42.00000000000000000, 34.49999999999999289 ) ) ;
#1088 = CARTESIAN_POINT ( 'NONE',  ( 16.00000000000001776, 42.00000000000000000, 29.68999999999999417 ) ) ;
#1089 = CARTESIAN_POINT ( 'NONE',  ( 39.74999999999999289, 18.74999999999997868, 3.750000000000000000 ) ) ;
#1090 = STYLED_ITEM ( 'NONE', ( #6246 ), #69414 ) ;
#1091 = FILL_AREA_STYLE ('',( #65180 ) ) ;
#1092 = ORIENTED_EDGE ( 'NONE', *, *, #60276, .T. ) ;
#1093 = CARTESIAN_POINT ( 'NONE',  ( -171.3550000000000182, -4.716976649647093289, -6.492361379858945902 ) ) ;
#1094 = VERTEX_POINT ( 'NONE', #11133 ) ;
#1095 = LINE ( 'NONE', #22635, #20169 ) ;
#1096 = DIRECTION ( 'NONE',  ( 1.000000000000000000, 0.000000000000000000, 0.000000000000000000 ) ) ;
#1097 =( NAMED_UNIT ( * ) SI_UNIT ( $, .STERADIAN. ) SOLID_ANGLE_UNIT ( ) );
#1098 = PLANE ( 'NONE',  #39875 ) ;
#1099 = FACE_BOUND ( 'NONE', #16181, .T. ) ;
#1100 = CARTESIAN_POINT ( 'NONE',  ( -9.827790563157511022E-16, 149.5570736234661524, 8.025000000000000355 ) ) ;
#1101 = ORIENTED_EDGE ( 'NONE', *, *, #12298, .T. ) ;
#1102 = AXIS2_PLACEMENT_3D ( 'NONE', #7032, #1705, #66107 ) ;
#1103 = CARTESIAN_POINT ( 'NONE',  ( 2.607480562268992941, 137.7929263765338419, -8.025000000000060751 ) ) ;
#1104 = STYLED_ITEM ( 'NONE', ( #33830 ), #11987 ) ;
#1105 = CARTESIAN_POINT ( 'NONE',  ( -84.80499999999999261, -8.437984349512086979, 5.166775262442717831E-16 ) ) ;
#1106 = UNCERTAINTY_MEASURE_WITH_UNIT (LENGTH_MEASURE( 1.000000000000000082E-05 ), #415, 'distance_accuracy_value', 'NONE');
#1107 = FILL_AREA_STYLE ('',( #61306 ) ) ;
#1108 = FILL_AREA_STYLE ('',( #53945 ) ) ;
#1109 = ADVANCED_FACE ( 'NONE', ( #28690 ), #54044, .F. ) ;
#1110 = CARTESIAN_POINT ( 'NONE',  ( -169.9429263765337907, 0.000000000000000000, 9.524999999999991473 ) ) ;
#1111 = ADVANCED_FACE ( 'NONE', ( #48830 ), #43796, .F. ) ;
#1112 = FACE_OUTER_BOUND ( 'NONE', #40591, .T. ) ;
#1113 = DIRECTION ( 'NONE',  ( -0.000000000000000000, -0.000000000000000000, -1.000000000000000000 ) ) ;
#1114 = CARTESIAN_POINT ( 'NONE',  ( 20.57648123223228254, 110.4999999999999858, -10.27659574468085069 ) ) ;
#1115 = ORIENTED_EDGE ( 'NONE', *, *, #63135, .T. ) ;
#1116 = DIRECTION ( 'NONE',  ( -0.000000000000000000, -0.000000000000000000, 1.000000000000000000 ) ) ;
#1117 = CARTESIAN_POINT ( 'NONE',  ( 82.09357085539578236, 5.000000000000000000, 37.00402776293825724 ) ) ;
#1118 = CARTESIAN_POINT ( 'NONE',  ( -64.94499999999999318, -9.827790563157499189E-16, -8.024999999999991473 ) ) ;
#1120 = ORIENTED_EDGE ( 'NONE', *, *, #30649, .T. ) ;
#1119 = STYLED_ITEM ( 'NONE', ( #55497 ), #34613 ) ;
#1121 = SURFACE_STYLE_USAGE ( .BOTH. , #5755 ) ;
#1122 = EDGE_CURVE ( 'NONE', #7643, #49707, #24655, .T. ) ;
#1123 = PRESENTATION_LAYER_ASSIGNMENT (  '', '', ( #23790 ) ) ;
#1124 = FILL_AREA_STYLE ('',( #6457 ) ) ;
#1125 = CARTESIAN_POINT ( 'NONE',  ( -45.00000000000000000, 9.708372675170615196, -6.000000000000000888 ) ) ;
#1126 = CIRCLE ( 'NONE', #57335, 12.50000000000001066 ) ;
#1127 = ORIENTED_EDGE ( 'NONE', *, *, #27155, .F. ) ;
#1128 =( LENGTH_UNIT ( ) NAMED_UNIT ( * ) SI_UNIT ( .MILLI., .METRE. ) );
#1129 = ORIENTED_EDGE ( 'NONE', *, *, #69485, .F. ) ;
#1130 = CARTESIAN_POINT ( 'NONE',  ( 44.99999999999999289, 9.639620389971918613, -6.500000000000007105 ) ) ;
#1131 = CARTESIAN_POINT ( 'NONE',  ( 0.000000000000000000, 111.9999999999999858, 0.000000000000000000 ) ) ;
#1132 = CARTESIAN_POINT ( 'NONE',  ( -117.0549999999999926, -9.827790563157499189E-16, -8.024999999999991473 ) ) ;
#1133 = ORIENTED_EDGE ( 'NONE', *, *, #57435, .T. ) ;
#1134 = CARTESIAN_POINT ( 'NONE',  ( -57.58629378005873889, -7.761720733523185700, -0.7755720678490086728 ) ) ;
#1135 = CARTESIAN_POINT ( 'NONE',  ( -72.59292637653379643, -3.094860106618431139, -9.524999999999991473 ) ) ;
#1136 = ADVANCED_FACE ( 'NONE', ( #6215 ), #44928, .F. ) ;
#1137 =( NAMED_UNIT ( * ) SI_UNIT ( $, .STERADIAN. ) SOLID_ANGLE_UNIT ( ) );
#1138 = DIRECTION ( 'NONE',  ( 0.000000000000000000, 1.000000000000000000, -0.000000000000000000 ) ) ;
#1139 = SURFACE_SIDE_STYLE ('',( #43493 ) ) ;
#1140 = CARTESIAN_POINT ( 'NONE',  ( -149.9070736234661183, -3.094860106618429807, 9.524999999999991473 ) ) ;
#1141 = AXIS2_PLACEMENT_3D ( 'NONE', #3631, #7905, #30372 ) ;
#1142 = CARTESIAN_POINT ( 'NONE',  ( 5.598654528085809545, 130.1449999999999818, -7.705886871421373741 ) ) ;
#1143 = CARTESIAN_POINT ( 'NONE',  ( -97.85707362346616378, -5.598654528085803328, -7.705886871421366635 ) ) ;
#1144 = PRODUCT_DEFINITION_FORMATION_WITH_SPECIFIED_SOURCE ( 'ANY', '', #64784, .NOT_KNOWN. ) ;
#1145 = EDGE_CURVE ( 'NONE', #47531, #52271, #24448, .T. ) ;
#1146 = DIRECTION ( 'NONE',  ( 1.000000000000000000, 1.601283208593975100E-14, 0.000000000000000000 ) ) ;
#1147 = VERTEX_POINT ( 'NONE', #23771 ) ;
#1148 = STYLED_ITEM ( 'NONE', ( #50817 ), #55567 ) ;
#1149 = CARTESIAN_POINT ( 'NONE',  ( -15.98999599679679839, 118.4999999999999716, 7.000000000000000000 ) ) ;
#1150 = CARTESIAN_POINT ( 'NONE',  ( -130.1049999999999898, -6.826472737025115478, 4.959722759717900331 ) ) ;
#1151 = CARTESIAN_POINT ( 'NONE',  ( -164.3929263765337794, 8.102448949553176405, 5.886773742842740909 ) ) ;
#1152 = CARTESIAN_POINT ( 'NONE',  ( -146.9929263765338021, 8.102448949553172852, -5.886773742842744461 ) ) ;
#1153 = SURFACE_STYLE_FILL_AREA ( #7207 ) ;
#1154 = CARTESIAN_POINT ( 'NONE',  ( -143.0949999999999704, -2.607480562269071545, -8.024999999999991473 ) ) ;
#1155 = CARTESIAN_POINT ( 'NONE',  ( -133.3449999999999989, 7.632228543268599452, -2.479861379858951942 ) ) ;
#1156 = VECTOR ( 'NONE', #44633, 1000.000000000000000 ) ;
#1157 = EDGE_LOOP ( 'NONE', ( #14111, #36056 ) ) ;
#1158 = CARTESIAN_POINT ( 'NONE',  ( 8.000000000000035527, 5.000000000000000000, -77.00402776293825013 ) ) ;
#1159 = CARTESIAN_POINT ( 'NONE',  ( -5.000000000000000000, 0.000000000000000000, 0.2499999999999941436 ) ) ;
#1160 = SURFACE_STYLE_USAGE ( .BOTH. , #38912 ) ;
#1161 = COLOUR_RGB ( '', 0.66274510, 0.83137255, 0.94901961) ;
#1163 = CIRCLE ( 'NONE', #40576, 0.2500000000000002220 ) ;
#1162 = CARTESIAN_POINT ( 'NONE',  ( -1.387778780781445676E-14, 17.78868675966041835, 1.540743955509788682E-30 ) ) ;
#1164 = CARTESIAN_POINT ( 'NONE',  ( -48.50499999999998835, -6.826472737025115478, -4.959722759717899443 ) ) ;
#1165 = CARTESIAN_POINT ( 'NONE',  ( -54.44499999999999318, 0.000000000000000000, 8.024999999999991473 ) ) ;
#1166 =( GEOMETRIC_REPRESENTATION_CONTEXT ( 3 ) GLOBAL_UNCERTAINTY_ASSIGNED_CONTEXT ( ( #48224 ) ) GLOBAL_UNIT_ASSIGNED_CONTEXT ( ( #19992, #41496, #14751 ) ) REPRESENTATION_CONTEXT ( 'NONE', 'WORKASPACE' ) );
#1167 = DIRECTION ( 'NONE',  ( -0.000000000000000000, 0.000000000000000000, -1.000000000000000000 ) ) ;
#1168 = LINE ( 'NONE', #22705, #15247 ) ;
#1169 = AXIS2_PLACEMENT_3D ( 'NONE', #11637, #23568, #65083 ) ;
#1170 = FILL_AREA_STYLE_COLOUR ( '', #43640 ) ;
#1171 = CARTESIAN_POINT ( 'NONE',  ( -60.00000000000000000, -2.024042244987997205E-14, 12.00000000000000000 ) ) ;
#1172 = COLOUR_RGB ( '', 0.31764706, 0.68627451, 0.89019608) ;
#1173 = CARTESIAN_POINT ( 'NONE',  ( -95.69292637653379074, 10.01517768586948698, -1.839758294383808571E-15 ) ) ;
#1174 = PRODUCT_CONTEXT ( 'NONE', #31147, 'mechanical' ) ;
#1175 = DIRECTION ( 'NONE',  ( 1.300977106640434891E-16, -0.000000000000000000, 1.000000000000000000 ) ) ;
#1176 = CYLINDRICAL_SURFACE ( 'NONE', #1141, 0.5000000000000004441 ) ;
#1177 = ADVANCED_FACE ( 'NONE', ( #61050 ), #66333, .F. ) ;
#1178 = VECTOR ( 'NONE', #18203, 1000.000000000000000 ) ;
#1179 = CARTESIAN_POINT ( 'NONE',  ( -48.50000000000000000, 14.49137674618942562, -7.500000000000000000 ) ) ;
#1180 = CARTESIAN_POINT ( 'NONE',  ( -100.2570736234661695, 5.598654528085800663, -7.705886871421367523 ) ) ;
#1181 = MECHANICAL_DESIGN_GEOMETRIC_PRESENTATION_REPRESENTATION (  '', ( #46236 ), #52936 ) ;
#1182 = FACE_OUTER_BOUND ( 'NONE', #23963, .T. ) ;
#1183 = ORIENTED_EDGE ( 'NONE', *, *, #62423, .F. ) ;
#1184 = DIRECTION ( 'NONE',  ( -0.000000000000000000, 0.000000000000000000, 1.000000000000000000 ) ) ;
#1185 = CARTESIAN_POINT ( 'NONE',  ( 1.000000000000000000, 1.000000000000000222, 3.000000000000000000 ) ) ;
#1186 = ORIENTED_EDGE ( 'NONE', *, *, #33909, .F. ) ;
#1187 = DIRECTION ( 'NONE',  ( -1.000000000000000000, 0.000000000000000000, 0.000000000000000000 ) ) ;
#1188 = AXIS2_PLACEMENT_3D ( 'NONE', #63108, #10004, #20185 ) ;
#1189 = CARTESIAN_POINT ( 'NONE',  ( -7.632228543268607446, 127.6570736234661467, -2.479861379858953718 ) ) ;
#1190 = PRODUCT_DEFINITION ( 'UNKNOWN', '', #57360, #55755 ) ;
#1191 = ADVANCED_FACE ( 'NONE', ( #19171 ), #67357, .T. ) ;
#1192 = CARTESIAN_POINT ( 'NONE',  ( 34.99999999999992895, 110.4999999999999858, -10.00000000000000000 ) ) ;
#1193 = ADVANCED_FACE ( 'NONE', ( #3310, #15668 ), #63497, .T. ) ;
#1194 = DIRECTION ( 'NONE',  ( 0.000000000000000000, 0.000000000000000000, 1.000000000000000000 ) ) ;
#1195 = MECHANICAL_DESIGN_GEOMETRIC_PRESENTATION_REPRESENTATION (  '', ( #1148 ), #28191 ) ;
#1196 = AXIS2_PLACEMENT_3D ( 'NONE', #18355, #29584, #13059 ) ;
#1197 = FILL_AREA_STYLE ('',( #27959 ) ) ;
#1198 = VERTEX_POINT ( 'NONE', #42101 ) ;
#1199 = ORIENTED_EDGE ( 'NONE', *, *, #53541, .F. ) ;
#1200 = SURFACE_STYLE_USAGE ( .BOTH. , #54373 ) ;
#1201 = EDGE_CURVE ( 'NONE', #34141, #63720, #44903, .T. ) ;
#1202 = ORIENTED_EDGE ( 'NONE', *, *, #65528, .F. ) ;
#1203 = EDGE_CURVE ( 'NONE', #56838, #56593, #54978, .T. ) ;
#1204 = DIRECTION ( 'NONE',  ( 1.000000000000000000, 0.000000000000000000, 0.000000000000000000 ) ) ;
#1205 = CARTESIAN_POINT ( 'NONE',  ( -94.55707362346616662, -1.166476076187852838E-15, -9.524999999999991473 ) ) ;
#1206 = AXIS2_PLACEMENT_3D ( 'NONE', #46550, #19759, #14477 ) ;
#1207 = CARTESIAN_POINT ( 'NONE',  ( 2.607480562269034241, 134.7929263765338135, -8.025000000000032330 ) ) ;
#1208 = CARTESIAN_POINT ( 'NONE',  ( -94.34499999999998465, 7.632228543268599452, -2.479861379858951942 ) ) ;
#1209 = ORIENTED_EDGE ( 'NONE', *, *, #62339, .F. ) ;
#1210 = CARTESIAN_POINT ( 'NONE',  ( -195.0000000000000000, 0.000000000000000000, 0.000000000000000000 ) ) ;
#1211 = EDGE_CURVE ( 'NONE', #8109, #66508, #33662, .T. ) ;
#1212 = PRESENTATION_LAYER_ASSIGNMENT (  '', '', ( #41744 ) ) ;
#1213 = CARTESIAN_POINT ( 'NONE',  ( 17.25000000000000711, 25.24999999999998224, 3.750000000000000000 ) ) ;
#1214 = ORIENTED_EDGE ( 'NONE', *, *, #14225, .F. ) ;
#1215 = DIRECTION ( 'NONE',  ( 0.000000000000000000, 0.000000000000000000, 1.000000000000000000 ) ) ;
#1216 =( NAMED_UNIT ( * ) PLANE_ANGLE_UNIT ( ) SI_UNIT ( $, .RADIAN. ) );
#1217 = EDGE_CURVE ( 'NONE', #56763, #41176, #14618, .T. ) ;
#1218 = AXIS2_PLACEMENT_3D ( 'NONE', #48330, #21556, #43071 ) ;
#1219 = DIRECTION ( 'NONE',  ( -0.000000000000000000, -1.000000000000000000, -0.000000000000000000 ) ) ;
#1220 = ORIENTED_EDGE ( 'NONE', *, *, #65094, .T. ) ;
#1221 = COLOUR_RGB ( '', 0.72549020, 0.75294118, 0.79215686) ;
#1222 = ORIENTED_EDGE ( 'NONE', *, *, #587, .F. ) ;
#1223 = DIRECTION ( 'NONE',  ( 1.224646799147353207E-16, 1.000000000000000000, -0.000000000000000000 ) ) ;
#1224 = DIRECTION ( 'NONE',  ( -1.000000000000000000, 0.000000000000000000, 0.000000000000000000 ) ) ;
#1225 = DIRECTION ( 'NONE',  ( -1.000000000000000000, -0.000000000000000000, -0.000000000000000000 ) ) ;
#1226 = CARTESIAN_POINT ( 'NONE',  ( -5.710692600061824997, -2.499999999999999112, 4.108790270285303414 ) ) ;
#1227 = DIRECTION ( 'NONE',  ( -0.000000000000000000, -0.000000000000000000, -1.000000000000000000 ) ) ;
#1228 = CARTESIAN_POINT ( 'NONE',  ( 60.00000000000000000, 1.797044900979284448E-15, -7.000000000000000888 ) ) ;
#1229 = COLOUR_RGB ( '', 0.66274510, 0.83137255, 0.94901961) ;
#1230 =( NAMED_UNIT ( * ) PLANE_ANGLE_UNIT ( ) SI_UNIT ( $, .RADIAN. ) );
#1231 = CARTESIAN_POINT ( 'NONE',  ( -8.440061761865273127, 153.6413859836615359, 2.039925464057752880 ) ) ;
#1232 = ORIENTED_EDGE ( 'NONE', *, *, #57235, .T. ) ;
#1233 = CIRCLE ( 'NONE', #28222, 7.500000000000000000 ) ;
#1234 = SURFACE_STYLE_FILL_AREA ( #22069 ) ;
#1235 = DIRECTION ( 'NONE',  ( 1.000000000000000000, 0.000000000000000000, 0.000000000000000000 ) ) ;
#1236 = CARTESIAN_POINT ( 'NONE',  ( -148.8570736234661638, -5.598654528085803328, -7.705886871421366635 ) ) ;
#1237 = CYLINDRICAL_SURFACE ( 'NONE', #33201, 0.5000000000000004441 ) ;
#1238 = ORIENTED_EDGE ( 'NONE', *, *, #36509, .F. ) ;
#1239 = CARTESIAN_POINT ( 'NONE',  ( -157.7049999999999557, 2.607480562269073321, 8.024999999999991473 ) ) ;
#1240 = DIRECTION ( 'NONE',  ( 0.000000000000000000, 0.000000000000000000, -1.000000000000000000 ) ) ;
#1241 = DIRECTION ( 'NONE',  ( -0.000000000000000000, -1.000000000000000000, -0.000000000000000000 ) ) ;
#1242 = AXIS2_PLACEMENT_3D ( 'NONE', #13763, #56679, #8505 ) ;
#1243 = CARTESIAN_POINT ( 'NONE',  ( -169.6449999999999818, 4.716976649647091513, -6.492361379858946790 ) ) ;
#1244 = CARTESIAN_POINT ( 'NONE',  ( -156.4449999999999932, 0.000000000000000000, 8.024999999999991473 ) ) ;
#1245 = EDGE_CURVE ( 'NONE', #9552, #29900, #12302, .T. ) ;
#1246 =( BOUNDED_CURVE ( )  B_SPLINE_CURVE ( 2, ( #14281, #8668, #68114, #46334, #52297, #62798, #40698, #62111, #14641, #9015, #35747 ),
 .UNSPECIFIED., .F., .F. ) 
 B_SPLINE_CURVE_WITH_KNOTS ( ( 3, 2, 2, 2, 2, 3 ),
 ( 0.7391304347826086474, 0.7413043478260870067, 0.7434782608695652550, 0.7456521739130435034, 0.7478260869565217517, 0.7500000000000000000 ),
 .UNSPECIFIED. ) 
 CURVE ( )  GEOMETRIC_REPRESENTATION_ITEM ( )  RATIONAL_B_SPLINE_CURVE ( ( 1.000000000000000000, 0.9510565162951535312, 1.000000000000000000, 0.9510565162951535312, 1.000000000000000000, 0.9510565162951535312, 1.000000000000000000, 0.9510565162951535312, 1.000000000000000000, 0.9510565162951535312, 1.000000000000000000 ) ) 
 REPRESENTATION_ITEM ( '' )  );
#1247 = ORIENTED_EDGE ( 'NONE', *, *, #15835, .T. ) ;
#1248 = AXIS2_PLACEMENT_3D ( 'NONE', #67127, #50957, #2716 ) ;
#1249 = CARTESIAN_POINT ( 'NONE',  ( 44.83562443654408725, 9.945208145515103126, 3.584089800673137205 ) ) ;
#1250 = LINE ( 'NONE', #60055, #46266 ) ;
#1251 = CARTESIAN_POINT ( 'NONE',  ( -68.90499999999997272, 2.607480562269068880, -8.024999999999993250 ) ) ;
#1252 = CARTESIAN_POINT ( 'NONE',  ( -35.35889534745761864, -11.21033625376975529, 1.846521352861608012 ) ) ;
#1253 = MECHANICAL_DESIGN_GEOMETRIC_PRESENTATION_REPRESENTATION (  '', ( #11456 ), #65392 ) ;
#1254 =( NAMED_UNIT ( * ) PLANE_ANGLE_UNIT ( ) SI_UNIT ( $, .RADIAN. ) );
#1255 = CARTESIAN_POINT ( 'NONE',  ( -74.69499999999995055, -8.437984349512086979, 5.166775262442717831E-16 ) ) ;
#1256 = CARTESIAN_POINT ( 'NONE',  ( -5.598654528085806881, 137.8549999999999898, -7.705886871421374629 ) ) ;
#1257 = CARTESIAN_POINT ( 'NONE',  ( 6.418790567836331284, -2.882328613363594361, 0.02778322089669375133 ) ) ;
#1258 =( GEOMETRIC_REPRESENTATION_CONTEXT ( 3 ) GLOBAL_UNCERTAINTY_ASSIGNED_CONTEXT ( ( #60738 ) ) GLOBAL_UNIT_ASSIGNED_CONTEXT ( ( #46100, #63287, #19676 ) ) REPRESENTATION_CONTEXT ( 'NONE', 'WORKASPACE' ) );
#1259 = CARTESIAN_POINT ( 'NONE',  ( 57.00000000000000000, 14.00000000000000000, 79.00402776293826435 ) ) ;
#1260 = SURFACE_STYLE_USAGE ( .BOTH. , #49535 ) ;
#1262 = ORIENTED_EDGE ( 'NONE', *, *, #38969, .F. ) ;
#1261 = CIRCLE ( 'NONE', #100, 4.999999999999997335 ) ;
#1263 = FILL_AREA_STYLE ('',( #17201 ) ) ;
#1264 = AXIS2_PLACEMENT_3D ( 'NONE', #69527, #68504, #26267 ) ;
#1265 = MECHANICAL_DESIGN_GEOMETRIC_PRESENTATION_REPRESENTATION (  '', ( #37346 ), #6794 ) ;
#1266 =( NAMED_UNIT ( * ) SI_UNIT ( $, .STERADIAN. ) SOLID_ANGLE_UNIT ( ) );
#1267 = TOROIDAL_SURFACE ( 'NONE', #6956, 4.750000000000000000, 0.2500000000000000000 ) ;
#1268 = CARTESIAN_POINT ( 'NONE',  ( 57.00000000000000000, 14.00000000000000000, -79.00402776293826435 ) ) ;
#1269 = ORIENTED_EDGE ( 'NONE', *, *, #12536, .F. ) ;
#1270 = VERTEX_POINT ( 'NONE', #47359 ) ;
#1271 = DIRECTION ( 'NONE',  ( 1.000000000000000000, -0.000000000000000000, -0.000000000000000000 ) ) ;
#1272 = PRESENTATION_LAYER_ASSIGNMENT (  '', '', ( #15946 ) ) ;
#1273 =( GEOMETRIC_REPRESENTATION_CONTEXT ( 3 ) GLOBAL_UNCERTAINTY_ASSIGNED_CONTEXT ( ( #62316 ) ) GLOBAL_UNIT_ASSIGNED_CONTEXT ( ( #32324, #36270, #26006 ) ) REPRESENTATION_CONTEXT ( 'NONE', 'WORKASPACE' ) );
#1274 = EDGE_CURVE ( 'NONE', #33237, #54480, #4739, .T. ) ;
#1275 = SURFACE_STYLE_USAGE ( .BOTH. , #28387 ) ;
#1276 = DIRECTION ( 'NONE',  ( -1.000000000000000000, 0.000000000000000000, 0.000000000000000000 ) ) ;
#1277 = LINE ( 'NONE', #49203, #61033 ) ;
#1278 = VERTEX_POINT ( 'NONE', #20585 ) ;
#1279 = CARTESIAN_POINT ( 'NONE',  ( -113.0049999999999812, 6.826472737025115478, 4.959722759717899443 ) ) ;
#1280 = ORIENTED_EDGE ( 'NONE', *, *, #13683, .F. ) ;
#1281 = EDGE_CURVE ( 'NONE', #34416, #38988, #39322, .T. ) ;
#1282 = VECTOR ( 'NONE', #24541, 1000.000000000000000 ) ;
#1283 = EDGE_LOOP ( 'NONE', ( #11813, #37848, #54579, #36242 ) ) ;
#1284 = DIRECTION ( 'NONE',  ( 1.000000000000000000, 0.000000000000000000, 0.000000000000000000 ) ) ;
#1285 = CARTESIAN_POINT ( 'NONE',  ( -68.90707362346616094, -3.094860106618429807, 9.524999999999991473 ) ) ;
#1286 = VERTEX_POINT ( 'NONE', #41726 ) ;
#1287 = AXIS2_PLACEMENT_3D ( 'NONE', #47917, #10571, #69642 ) ;
#1288 = DIRECTION ( 'NONE',  ( 0.000000000000000000, 1.000000000000000000, 0.000000000000000000 ) ) ;
#1289 = CARTESIAN_POINT ( 'NONE',  ( 8.102448949553183510, 156.9949999999999761, -5.886773742842746238 ) ) ;
#1290 = DIRECTION ( 'NONE',  ( 0.000000000000000000, 0.000000000000000000, -1.000000000000000000 ) ) ;
#1291 = ORIENTED_EDGE ( 'NONE', *, *, #47372, .F. ) ;
#1292 = ORIENTED_EDGE ( 'NONE', *, *, #37976, .F. ) ;
#1293 = AXIS2_PLACEMENT_3D ( 'NONE', #38188, #59591, #65571 ) ;
#1294 = CARTESIAN_POINT ( 'NONE',  ( -7.315997198399062817, 110.4999999999999716, -6.115009789855206712 ) ) ;
#1295 =( NAMED_UNIT ( * ) PLANE_ANGLE_UNIT ( ) SI_UNIT ( $, .RADIAN. ) );
#1296 = DIRECTION ( 'NONE',  ( 1.000000000000000000, 0.000000000000000000, 0.000000000000000000 ) ) ;
#1297 = DIRECTION ( 'NONE',  ( 0.000000000000000000, 0.000000000000000000, -1.000000000000000000 ) ) ;
#1298 = ORIENTED_EDGE ( 'NONE', *, *, #53745, .F. ) ;
#1299 = CARTESIAN_POINT ( 'NONE',  ( 2.607480562269071989, 136.5929263765338249, 8.025000000000002132 ) ) ;
#1300 = CARTESIAN_POINT ( 'NONE',  ( 22.75000000000000711, 36.75000000000000000, -3.750000000000000000 ) ) ;
#1301 = DIRECTION ( 'NONE',  ( -0.000000000000000000, 0.000000000000000000, -1.000000000000000000 ) ) ;
#1302 = AXIS2_PLACEMENT_3D ( 'NONE', #29668, #24371, #46230 ) ;
#1303 = EDGE_CURVE ( 'NONE', #9072, #69035, #35880, .T. ) ;
#1304 = CARTESIAN_POINT ( 'NONE',  ( -104.0929263765348054, 3.094860106635372698, 9.524999999987684873 ) ) ;
#1305 = FACE_OUTER_BOUND ( 'NONE', #25216, .T. ) ;
#1306 = VERTEX_POINT ( 'NONE', #14990 ) ;
#1307 = DIRECTION ( 'NONE',  ( 0.000000000000000000, 0.6691306063588592368, 0.7431448254773934670 ) ) ;
#1308 = ORIENTED_EDGE ( 'NONE', *, *, #5446, .T. ) ;
#1309 =( LENGTH_UNIT ( ) NAMED_UNIT ( * ) SI_UNIT ( .MILLI., .METRE. ) );
#1310 = CYLINDRICAL_SURFACE ( 'NONE', #5308, 1.000000000000000888 ) ;
#1311 = CARTESIAN_POINT ( 'NONE',  ( 33.00000000000000000, 13.00000000000000178, -80.00402776293826435 ) ) ;
#1312 = CARTESIAN_POINT ( 'NONE',  ( -195.0000000000000000, 0.000000000000000000, 0.000000000000000000 ) ) ;
#1314 = CARTESIAN_POINT ( 'NONE',  ( -133.1050000000000182, -6.826472737025115478, 4.959722759717900331 ) ) ;
#1313 = PRESENTATION_LAYER_ASSIGNMENT (  '', '', ( #12609 ) ) ;
#1315 = CARTESIAN_POINT ( 'NONE',  ( -15.00000000000000000, 8.000000000000000000, -4.000000000000000000 ) ) ;
#1316 = DIRECTION ( 'NONE',  ( 1.000000000000000000, -0.000000000000000000, 0.000000000000000000 ) ) ;
#1317 = ORIENTED_EDGE ( 'NONE', *, *, #27225, .T. ) ;
#1318 =( GEOMETRIC_REPRESENTATION_CONTEXT ( 3 ) GLOBAL_UNCERTAINTY_ASSIGNED_CONTEXT ( ( #10073 ) ) GLOBAL_UNIT_ASSIGNED_CONTEXT ( ( #1753, #7084, #39471 ) ) REPRESENTATION_CONTEXT ( 'NONE', 'WORKASPACE' ) );
#1319 = DIRECTION ( 'NONE',  ( -1.000000000000000000, 0.000000000000000000, 0.000000000000000000 ) ) ;
#1320 = CARTESIAN_POINT ( 'NONE',  ( 0.9115210089146362771, 9.000000000000010658, 3.505587024369798722E-15 ) ) ;
#1321 = CARTESIAN_POINT ( 'NONE',  ( -45.00000000000000000, 9.708372675170618749, -6.000000000000000000 ) ) ;
#1322 = ORIENTED_EDGE ( 'NONE', *, *, #36239, .F. ) ;
#1323 = STYLED_ITEM ( 'NONE', ( #8302 ), #23504 ) ;
#1324 = VERTEX_POINT ( 'NONE', #9349 ) ;
#1325 = DIRECTION ( 'NONE',  ( -1.300977106640434891E-16, 0.000000000000000000, -1.000000000000000000 ) ) ;
#1326 = CARTESIAN_POINT ( 'NONE',  ( 0.000000000000000000, 87.30187232391182306, 8.025000000000000355 ) ) ;
#1327 = CARTESIAN_POINT ( 'NONE',  ( -57.95499999999997698, -7.632228543268599452, 2.479861379858951054 ) ) ;
#1328 = ORIENTED_EDGE ( 'NONE', *, *, #29654, .T. ) ;
#1329 = FILL_AREA_STYLE ('',( #60802 ) ) ;
#1330 = AXIS2_PLACEMENT_3D ( 'NONE', #45095, #48989, #61227 ) ;
#1331 = CARTESIAN_POINT ( 'NONE',  ( 1.401671290772265266, 7.000000000000007105, 0.1093172352041303641 ) ) ;
#1332 = CIRCLE ( 'NONE', #28318, 8.524999999999977263 ) ;
#1333 = DIRECTION ( 'NONE',  ( -1.000000000000000000, 0.000000000000000000, -0.000000000000000000 ) ) ;
#1334 = ADVANCED_FACE ( 'NONE', ( #63825 ), #59512, .T. ) ;
#1335 = CARTESIAN_POINT ( 'NONE',  ( -129.2929263765344956, 3.094860106606730721, -9.525000000008491341 ) ) ;
#1336 = ORIENTED_EDGE ( 'NONE', *, *, #9744, .F. ) ;
#1337 = CARTESIAN_POINT ( 'NONE',  ( -58.75000000000000000, -8.499999999999992895, 11.89999999999999680 ) ) ;
#1338 = DIRECTION ( 'NONE',  ( 0.000000000000000000, 0.000000000000000000, 1.000000000000000000 ) ) ;
#1339 = SURFACE_SIDE_STYLE ('',( #32034 ) ) ;
#1340 = DIRECTION ( 'NONE',  ( -1.000000000000000000, 1.224646799147349509E-16, 0.000000000000000000 ) ) ;
#1341 = PRESENTATION_STYLE_ASSIGNMENT (( #44369 ) ) ;
#1342 = CONICAL_SURFACE ( 'NONE', #66540, 5.499999999999976907, 0.7853981633974309595 ) ;
#1343 = CARTESIAN_POINT ( 'NONE',  ( -105.8949999999999818, 6.826472737025115478, 4.959722759717899443 ) ) ;
#1344 = CARTESIAN_POINT ( 'NONE',  ( -8.102448949553181734, 111.0049999999999955, -5.886773742842749790 ) ) ;
#1345 = CARTESIAN_POINT ( 'NONE',  ( -79.94499999999999318, -9.827790563157499189E-16, -8.024999999999991473 ) ) ;
#1346 = AXIS2_PLACEMENT_3D ( 'NONE', #38983, #42884, #22765 ) ;
#1347 = DIRECTION ( 'NONE',  ( -1.000000000000000000, 7.709882115452469292E-16, 0.000000000000000000 ) ) ;
#1348 = DIRECTION ( 'NONE',  ( -0.000000000000000000, -0.000000000000000000, 1.000000000000000000 ) ) ;
#1349 =( NAMED_UNIT ( * ) SI_UNIT ( $, .STERADIAN. ) SOLID_ANGLE_UNIT ( ) );
#1350 = DIRECTION ( 'NONE',  ( -1.000000000000000000, 0.000000000000000000, 0.000000000000000000 ) ) ;
#1351 =( BOUNDED_CURVE ( )  B_SPLINE_CURVE ( 2, ( #31554, #16113, #4825, #37593, #63906, #32255, #25576, #47091, #26277, #68515, #20312 ),
 .UNSPECIFIED., .F., .F. ) 
 B_SPLINE_CURVE_WITH_KNOTS ( ( 3, 2, 2, 2, 2, 3 ),
 ( 0.8695652173913043237, 0.8717391304347825720, 0.8739130434782608203, 0.8760869565217391797, 0.8782608695652174280, 0.8804347826086956763 ),
 .UNSPECIFIED. ) 
 CURVE ( )  GEOMETRIC_REPRESENTATION_ITEM ( )  RATIONAL_B_SPLINE_CURVE ( ( 1.000000000000000000, 0.9510565162951535312, 1.000000000000000000, 0.9510565162951535312, 1.000000000000000000, 0.9510565162951535312, 1.000000000000000000, 0.9510565162951535312, 1.000000000000000000, 0.9510565162951535312, 1.000000000000000000 ) ) 
 REPRESENTATION_ITEM ( '' )  );
#1352 = AXIS2_PLACEMENT_3D ( 'NONE', #3507, #4216, #14826 ) ;
#1353 = DIRECTION ( 'NONE',  ( -0.000000000000000000, 1.000000000000000000, -0.000000000000000000 ) ) ;
#1354 = DIRECTION ( 'NONE',  ( -0.000000000000000000, -1.000000000000000000, 0.000000000000000000 ) ) ;
#1355 = VERTEX_POINT ( 'NONE', #52277 ) ;
#1357 =( GEOMETRIC_REPRESENTATION_CONTEXT ( 3 ) GLOBAL_UNCERTAINTY_ASSIGNED_CONTEXT ( ( #38268 ) ) GLOBAL_UNIT_ASSIGNED_CONTEXT ( ( #67368, #13909, #8640 ) ) REPRESENTATION_CONTEXT ( 'NONE', 'WORKASPACE' ) );
#1356 = CARTESIAN_POINT ( 'NONE',  ( -120.1429263765338078, 5.598654528085800663, -7.705886871421367523 ) ) ;
#1358 = CARTESIAN_POINT ( 'NONE',  ( -135.4449999999999932, 0.000000000000000000, 8.024999999999991473 ) ) ;
#1359 = SURFACE_SIDE_STYLE ('',( #45067 ) ) ;
#1360 = CIRCLE ( 'NONE', #37436, 16.94999999999999218 ) ;
#1361 = ADVANCED_FACE ( 'NONE', ( #17064 ), #27566, .T. ) ;
#1362 = CARTESIAN_POINT ( 'NONE',  ( -48.14499999999999602, -4.716976649647092401, 6.492361379858946790 ) ) ;
#1363 = SURFACE_SIDE_STYLE ('',( #6684 ) ) ;
#1364 = ORIENTED_EDGE ( 'NONE', *, *, #65878, .T. ) ;
#1366 = ORIENTED_EDGE ( 'NONE', *, *, #32459, .F. ) ;
#1365 = CIRCLE ( 'NONE', #55345, 0.5000000000000004441 ) ;
#1367 = CARTESIAN_POINT ( 'NONE',  ( 22.99999999999995026, 5.000000000000000000, 77.00402776293825013 ) ) ;
#1368 = DIRECTION ( 'NONE',  ( 0.000000000000000000, 1.000000000000000000, 0.000000000000000000 ) ) ;
#1369 = MECHANICAL_DESIGN_GEOMETRIC_PRESENTATION_REPRESENTATION (  '', ( #7050 ), #50843 ) ;
#1370 = FACE_BOUND ( 'NONE', #12312, .T. ) ;
#1371 = DIRECTION ( 'NONE',  ( -0.000000000000000000, -1.000000000000000000, 0.000000000000000000 ) ) ;
#1372 = DIRECTION ( 'NONE',  ( -0.7071067811865487940, 0.000000000000000000, 0.7071067811865463515 ) ) ;
#1373 = CYLINDRICAL_SURFACE ( 'NONE', #20731, 4.999999999999997335 ) ;
#1374 = VERTEX_POINT ( 'NONE', #64865 ) ;
#1375 = CARTESIAN_POINT ( 'NONE',  ( -140.0049999999999670, 6.826472737025115478, 4.959722759717899443 ) ) ;
#1376 = ORIENTED_EDGE ( 'NONE', *, *, #28257, .T. ) ;
#1377 = EDGE_CURVE ( 'NONE', #47061, #49280, #37856, .T. ) ;
#1378 = EDGE_LOOP ( 'NONE', ( #57692, #3735, #67885, #29980 ) ) ;
#1379 = FILL_AREA_STYLE_COLOUR ( '', #46788 ) ;
#1380 = AXIS2_PLACEMENT_3D ( 'NONE', #55149, #60428, #12235 ) ;
#1381 = ORIENTED_EDGE ( 'NONE', *, *, #57111, .F. ) ;
#1382 = PRODUCT_DEFINITION_SHAPE ( 'NONE', 'NONE',  #69711 ) ;
#1383 = CARTESIAN_POINT ( 'NONE',  ( -55.32330819037883174, -8.822438139991119144, -1.968259336913087409 ) ) ;
#1385 = ADVANCED_FACE ( 'NONE', ( #43805 ), #11752, .T. ) ;
#1384 = CIRCLE ( 'NONE', #58745, 0.5000000000000004441 ) ;
#1386 = SURFACE_STYLE_USAGE ( .BOTH. , #39807 ) ;
#1387 = CARTESIAN_POINT ( 'NONE',  ( 9.058813317711337021, 129.5449999999999875, 2.943386871421375783 ) ) ;
#1388 = DIRECTION ( 'NONE',  ( 0.000000000000000000, 0.000000000000000000, 1.000000000000000000 ) ) ;
#1389 = AXIS2_PLACEMENT_3D ( 'NONE', #58474, #53213, #1407 ) ;
#1390 = ORIENTED_EDGE ( 'NONE', *, *, #3863, .F. ) ;
#1391 = CARTESIAN_POINT ( 'NONE',  ( 179.4361977533490347, 5.000000000000000000, -103.7004518695263044 ) ) ;
#1393 = ADVANCED_FACE ( 'NONE', ( #12430 ), #49750, .T. ) ;
#1392 = CARTESIAN_POINT ( 'NONE',  ( -10.01517768586949408, 126.3049999999999784, -6.132527647946036459E-16 ) ) ;
#1394 = CARTESIAN_POINT ( 'NONE',  ( -53.45499999999997698, 7.632228543268599452, -2.479861379858951942 ) ) ;
#1395 = CARTESIAN_POINT ( 'NONE',  ( 66.49999999999998579, 33.99999999999999289, 4.000000000000000000 ) ) ;
#1396 = ORIENTED_EDGE ( 'NONE', *, *, #47139, .F. ) ;
#1397 = CARTESIAN_POINT ( 'NONE',  ( -3.094860106618434248, 153.9049999999999443, 9.525000000000000355 ) ) ;
#1398 = CARTESIAN_POINT ( 'NONE',  ( 3.249999999999998668, 36.74999999999999289, -3.750000000000000000 ) ) ;
#1399 = CARTESIAN_POINT ( 'NONE',  ( 1.000000000000000000, 36.74999999999999289, -3.750000000000000000 ) ) ;
#1400 = CIRCLE ( 'NONE', #49772, 8.999999999999994671 ) ;
#1401 = ADVANCED_FACE ( 'NONE', ( #54310 ), #49085, .T. ) ;
#1402 = COLOUR_RGB ( '', 0.40784314, 0.44705882, 0.49803922) ;
#1403 = PRESENTATION_STYLE_ASSIGNMENT (( #49658 ) ) ;
#1404 = FILL_AREA_STYLE_COLOUR ( '', #32070 ) ;
#1405 = VECTOR ( 'NONE', #56854, 1000.000000000000000 ) ;
#1406 = VERTEX_POINT ( 'NONE', #6134 ) ;
#1407 = DIRECTION ( 'NONE',  ( -1.000000000000000000, 0.000000000000000000, 0.000000000000000000 ) ) ;
#1408 = VERTEX_POINT ( 'NONE', #12088 ) ;
#1409 =( NAMED_UNIT ( * ) SI_UNIT ( $, .STERADIAN. ) SOLID_ANGLE_UNIT ( ) );
#1410 = FILL_AREA_STYLE_COLOUR ( '', #38556 ) ;
#1411 = CARTESIAN_POINT ( 'NONE',  ( -174.8050000000000068, -8.437984349512085203, 5.166775262442717831E-16 ) ) ;
#1412 = ORIENTED_EDGE ( 'NONE', *, *, #31186, .T. ) ;
#1413 = FILL_AREA_STYLE_COLOUR ( '', #18303 ) ;
#1414 = CARTESIAN_POINT ( 'NONE',  ( -183.9999999999998863, -8.156250775944638320, 1.871348862729520279 ) ) ;
#1415 = FILL_AREA_STYLE_COLOUR ( '', #31002 ) ;
#1416 = VERTEX_POINT ( 'NONE', #11404 ) ;
#1417 = EDGE_LOOP ( 'NONE', ( #28875, #48706, #35094, #7610 ) ) ;
#1418 = CARTESIAN_POINT ( 'NONE',  ( -45.03917211512175811, 8.121391520911325657, -3.616130125723889144 ) ) ;
#1419 = CARTESIAN_POINT ( 'NONE',  ( -81.80499999999996419, -8.437984349512085203, 5.166775262442717831E-16 ) ) ;
#1420 = EDGE_LOOP ( 'NONE', ( #65933, #39551, #7020, #26468 ) ) ;
#1421 = AXIS2_PLACEMENT_3D ( 'NONE', #7959, #45967, #55799 ) ;
#1422 = CARTESIAN_POINT ( 'NONE',  ( -44.99999999999977973, 146.9999999999999716, 7.000000000000000000 ) ) ;
#1423 = DIRECTION ( 'NONE',  ( 1.000000000000000000, 0.000000000000000000, 0.000000000000000000 ) ) ;
#1424 = COLOUR_RGB ( '', 0.66274510, 0.83137255, 0.94901961) ;
#1425 = CARTESIAN_POINT ( 'NONE',  ( 23.21231517720797655, 117.4999999999999716, 10.00000000000000000 ) ) ;
#1426 = ORIENTED_EDGE ( 'NONE', *, *, #62891, .F. ) ;
#1427 = DIRECTION ( 'NONE',  ( 0.000000000000000000, 0.000000000000000000, -1.000000000000000000 ) ) ;
#1428 = CARTESIAN_POINT ( 'NONE',  ( 3.094860106618435136, 127.2949999999999875, -9.525000000000000355 ) ) ;
#1429 = CARTESIAN_POINT ( 'NONE',  ( -110.6949999999999932, -8.437984349512085203, 5.166775262442717831E-16 ) ) ;
#1430 = CIRCLE ( 'NONE', #65510, 0.5000000000000004441 ) ;
#1431 =( NAMED_UNIT ( * ) SI_UNIT ( $, .STERADIAN. ) SOLID_ANGLE_UNIT ( ) );
#1433 = CARTESIAN_POINT ( 'NONE',  ( -18.76049541207539306, 11.53663499276287752, -3.311062927408552792 ) ) ;
#1432 = DIRECTION ( 'NONE',  ( -1.000000000000000000, 0.000000000000000000, 0.000000000000000000 ) ) ;
#1434 = CARTESIAN_POINT ( 'NONE',  ( -150.7429263765338021, -5.598654528085803328, -7.705886871421366635 ) ) ;
#1435 = VECTOR ( 'NONE', #40829, 1000.000000000000000 ) ;
#1436 = CARTESIAN_POINT ( 'NONE',  ( -175.0450000000000159, 7.632228543268600340, 2.479861379858949277 ) ) ;
#1437 =( GEOMETRIC_REPRESENTATION_CONTEXT ( 3 ) GLOBAL_UNCERTAINTY_ASSIGNED_CONTEXT ( ( #62085 ) ) GLOBAL_UNIT_ASSIGNED_CONTEXT ( ( #52179, #58131, #19436 ) ) REPRESENTATION_CONTEXT ( 'NONE', 'WORKASPACE' ) );
#1438 = AXIS2_PLACEMENT_3D ( 'NONE', #23559, #55221, #1717 ) ;
#1439 = CARTESIAN_POINT ( 'NONE',  ( -136.9429263765338192, 0.000000000000000000, 9.524999999999991473 ) ) ;
#1440 = EDGE_CURVE ( 'NONE', #65459, #13986, #26856, .T. ) ;
#1441 = CARTESIAN_POINT ( 'NONE',  ( 74.99999999999998579, 50.00000000000000000, 7.500000000000000000 ) ) ;
#1442 = VERTEX_POINT ( 'NONE', #1488 ) ;
#1443 = DIRECTION ( 'NONE',  ( -0.000000000000000000, -0.000000000000000000, -1.000000000000000000 ) ) ;
#1444 = ORIENTED_EDGE ( 'NONE', *, *, #61752, .T. ) ;
#1445 = CARTESIAN_POINT ( 'NONE',  ( -68.69292637653381917, 10.01517768586948698, -1.839758294383808571E-15 ) ) ;
#1447 = EDGE_CURVE ( 'NONE', #42847, #7443, #5760, .T. ) ;
#1446 = SURFACE_STYLE_USAGE ( .BOTH. , #740 ) ;
#1448 = FILL_AREA_STYLE_COLOUR ( '', #19215 ) ;
#1449 = CIRCLE ( 'NONE', #48762, 0.5000000000000004441 ) ;
#1450 = ADVANCED_FACE ( 'NONE', ( #44513 ), #56041, .F. ) ;
#1451 = FILL_AREA_STYLE ('',( #21946 ) ) ;
#1452 = EDGE_CURVE ( 'NONE', #47861, #21323, #48748, .T. ) ;
#1453 = CARTESIAN_POINT ( 'NONE',  ( -87.50000000000000000, -8.499999999999989342, 23.00000000000000000 ) ) ;
#1454 = VERTEX_POINT ( 'NONE', #13840 ) ;
#1455 = CARTESIAN_POINT ( 'NONE',  ( -166.2549999999999955, -4.716976649647092401, 6.492361379858946790 ) ) ;
#1456 = VECTOR ( 'NONE', #66838, 1000.000000000000000 ) ;
#1457 = ADVANCED_FACE ( 'NONE', ( #2536 ), #45872, .F. ) ;
#1458 = ORIENTED_EDGE ( 'NONE', *, *, #68873, .F. ) ;
#1459 = FACE_OUTER_BOUND ( 'NONE', #69682, .T. ) ;
#1461 = ADVANCED_FACE ( 'NONE', ( #29307 ), #50107, .T. ) ;
#1460 = DIRECTION ( 'NONE',  ( 0.000000000000000000, 0.000000000000000000, -1.000000000000000000 ) ) ;
#1462 = FACE_OUTER_BOUND ( 'NONE', #20819, .T. ) ;
#1463 = TOROIDAL_SURFACE ( 'NONE', #36424, 10.49999999999999822, 0.5000000000000000000 ) ;
#1464 = EDGE_CURVE ( 'NONE', #31245, #59005, #62374, .T. ) ;
#1465 = CARTESIAN_POINT ( 'NONE',  ( -13.23915246117191025, 52.65078610323165265, 12.50000000000000000 ) ) ;
#1466 = CARTESIAN_POINT ( 'NONE',  ( -4.716976649647098618, 155.2570736234661695, 6.492361379858953008 ) ) ;
#1467 = COLOUR_RGB ( '', 0.08235294, 0.09019608, 0.10196078) ;
#1468 = EDGE_LOOP ( 'NONE', ( #7591, #12251 ) ) ;
#1469 = MECHANICAL_DESIGN_GEOMETRIC_PRESENTATION_REPRESENTATION (  '', ( #16174 ), #3746 ) ;
#1471 = EDGE_CURVE ( 'NONE', #62435, #36781, #56877, .T. ) ;
#1470 = CARTESIAN_POINT ( 'NONE',  ( -195.0000000000000000, 0.000000000000000000, 9.524999999999991473 ) ) ;
#1472 = CARTESIAN_POINT ( 'NONE',  ( -81.95499999999998408, -7.632228543268599452, 2.479861379858951054 ) ) ;
#1473 =( LENGTH_UNIT ( ) NAMED_UNIT ( * ) SI_UNIT ( .MILLI., .METRE. ) );
#1474 = LINE ( 'NONE', #45858, #51256 ) ;
#1475 = CARTESIAN_POINT ( 'NONE',  ( 3.851859888774471706E-31, -8.500000000000000000, 0.000000000000000000 ) ) ;
#1476 = EDGE_LOOP ( 'NONE', ( #27866, #33163, #13088, #60927 ) ) ;
#1478 = DIRECTION ( 'NONE',  ( 0.000000000000000000, -1.000000000000000000, 0.000000000000000000 ) ) ;
#1477 = AXIS2_PLACEMENT_3D ( 'NONE', #12607, #18245, #55875 ) ;
#1479 = CARTESIAN_POINT ( 'NONE',  ( -60.89499999999999602, 6.826472737025116366, 4.959722759717898555 ) ) ;
#1480 = ORIENTED_EDGE ( 'NONE', *, *, #10436, .F. ) ;
#1481 = DIRECTION ( 'NONE',  ( 0.000000000000000000, 0.000000000000000000, 1.000000000000000000 ) ) ;
#1482 = VECTOR ( 'NONE', #10807, 1000.000000000000000 ) ;
#1483 = DIRECTION ( 'NONE',  ( -0.000000000000000000, -1.000000000000000000, -0.000000000000000000 ) ) ;
#1484 = CARTESIAN_POINT ( 'NONE',  ( -45.00000000000000000, 8.747695062214377870, -6.883368695987051034 ) ) ;
#1485 = COLOUR_RGB ( '', 0.40784314, 0.44705882, 0.49803922) ;
#1486 = ORIENTED_EDGE ( 'NONE', *, *, #61250, .F. ) ;
#1487 = CARTESIAN_POINT ( 'NONE',  ( -55.79499999999998039, 2.607480562269069324, -8.024999999999993250 ) ) ;
#1488 = CARTESIAN_POINT ( 'NONE',  ( 36.00000000000002842, 0.000000000000000000, -32.00402776293825724 ) ) ;
#1489 = ORIENTED_EDGE ( 'NONE', *, *, #35919, .F. ) ;
#1490 = CIRCLE ( 'NONE', #62198, 0.5000000000000003331 ) ;
#1491 = CIRCLE ( 'NONE', #40906, 16.50000000000000000 ) ;
#1492 = CARTESIAN_POINT ( 'NONE',  ( -71.99999999999998579, 64.07124727947029896, 9.500000000000000000 ) ) ;
#1493 = CARTESIAN_POINT ( 'NONE',  ( -110.0049999999999955, 6.826472737025116366, 4.959722759717898555 ) ) ;
#1494 = EDGE_LOOP ( 'NONE', ( #28905, #64829, #57228, #9435, #16796, #47009, #29650 ) ) ;
#1495 = DIRECTION ( 'NONE',  ( -1.000000000000000000, 0.000000000000000000, 0.000000000000000000 ) ) ;
#1496 = CARTESIAN_POINT ( 'NONE',  ( 35.99999999999999289, 5.000000000000000000, 32.00402776293825724 ) ) ;
#1497 = DIRECTION ( 'NONE',  ( 0.000000000000000000, 0.000000000000000000, 1.000000000000000000 ) ) ;
#1498 = CARTESIAN_POINT ( 'NONE',  ( -153.9570736234661581, 9.058813317711329915, -2.943386871421373119 ) ) ;
#1499 = PRESENTATION_LAYER_ASSIGNMENT (  '', '', ( #4919 ) ) ;
#1500 = B_SPLINE_CURVE_WITH_KNOTS ( 'NONE', 3,
 ( #35780, #67431, #52658, #4427, #25900, #19931, #18879, #68144 ),
 .UNSPECIFIED., .F., .F.,
 ( 4, 2, 2, 4 ),
 ( 0.004228133357766588295, 0.005276243923116606498, 0.006324354488466623833, 0.008420575619166661974 ),
 .UNSPECIFIED. ) ;
#1501 = DIRECTION ( 'NONE',  ( -1.000000000000000000, 1.445602896647339656E-16, -0.000000000000000000 ) ) ;
#1502 = CARTESIAN_POINT ( 'NONE',  ( 0.000000000000000000, 133.4449999999999932, -9.525000000000000355 ) ) ;
#1503 = CARTESIAN_POINT ( 'NONE',  ( -81.20707362346617231, 3.094860106618433360, 9.524999999999991473 ) ) ;
#1504 = EDGE_CURVE ( 'NONE', #34547, #21325, #2896, .T. ) ;
#1505 = MECHANICAL_DESIGN_GEOMETRIC_PRESENTATION_REPRESENTATION (  '', ( #55485 ), #10565 ) ;
#1506 = CARTESIAN_POINT ( 'NONE',  ( -96.44292637653380496, -1.166476076187852838E-15, -9.524999999999991473 ) ) ;
#1507 = ORIENTED_EDGE ( 'NONE', *, *, #64505, .T. ) ;
#1508 = CARTESIAN_POINT ( 'NONE',  ( 3.999798566743339556, 8.867945265733707672, 12.50000000000000000 ) ) ;
#1510 = SURFACE_STYLE_FILL_AREA ( #66989 ) ;
#1509 = PLANE ( 'NONE',  #68354 ) ;
#1511 = CARTESIAN_POINT ( 'NONE',  ( 0.2500000000000000000, 36.74999999999999289, 3.000000000000000000 ) ) ;
#1512 = CARTESIAN_POINT ( 'NONE',  ( -128.4549999999999841, 7.632228543268599452, -2.479861379858951942 ) ) ;
#1513 = DIRECTION ( 'NONE',  ( 0.000000000000000000, 0.000000000000000000, -1.000000000000000000 ) ) ;
#1514 = DIRECTION ( 'NONE',  ( -0.000000000000000000, -0.000000000000000000, 1.000000000000000000 ) ) ;
#1515 =( LENGTH_UNIT ( ) NAMED_UNIT ( * ) SI_UNIT ( .MILLI., .METRE. ) );
#1516 = CARTESIAN_POINT ( 'NONE',  ( -139.1950000000000216, 8.437984349512085203, -1.550032578732815448E-15 ) ) ;
#1517 = AXIS2_PLACEMENT_3D ( 'NONE', #21312, #42154, #46736 ) ;
#1518 = MECHANICAL_DESIGN_GEOMETRIC_PRESENTATION_REPRESENTATION (  '', ( #62224 ), #67871 ) ;
#1519 = CARTESIAN_POINT ( 'NONE',  ( -130.4950000000000045, 6.826472737025113702, -4.959722759717902107 ) ) ;
#1520 = EDGE_LOOP ( 'NONE', ( #57365, #40556, #39529, #17385 ) ) ;
#1521 = LINE ( 'NONE', #7548, #63948 ) ;
#1522 = DIRECTION ( 'NONE',  ( 1.156482317317870344E-15, -1.000000000000000000, -0.000000000000000000 ) ) ;
#1523 = UNCERTAINTY_MEASURE_WITH_UNIT (LENGTH_MEASURE( 1.000000000000000082E-05 ), #37418, 'distance_accuracy_value', 'NONE');
#1524 = CARTESIAN_POINT ( 'NONE',  ( -48.65499999999997272, -7.632228543268600340, -2.479861379858950166 ) ) ;
#1525 = CARTESIAN_POINT ( 'NONE',  ( -58.04499999999998749, 7.632228543268600340, 2.479861379858949277 ) ) ;
#1526 = STYLED_ITEM ( 'NONE', ( #69011 ), #38236 ) ;
#1527 = EDGE_CURVE ( 'NONE', #61621, #8720, #51254, .T. ) ;
#1528 = CARTESIAN_POINT ( 'NONE',  ( -24.21231517720798010, 112.4999999999999858, -10.00000000000000000 ) ) ;
#1529 = CARTESIAN_POINT ( 'NONE',  ( 35.99999999999999289, 0.000000000000000000, -29.00402776293825724 ) ) ;
#1530 =( GEOMETRIC_REPRESENTATION_CONTEXT ( 3 ) GLOBAL_UNCERTAINTY_ASSIGNED_CONTEXT ( ( #1022 ) ) GLOBAL_UNIT_ASSIGNED_CONTEXT ( ( #27650, #5492, #59675 ) ) REPRESENTATION_CONTEXT ( 'NONE', 'WORKASPACE' ) );
#1531 = DIRECTION ( 'NONE',  ( 1.000000000000000000, 0.000000000000000000, 0.000000000000000000 ) ) ;
#1532 = FILL_AREA_STYLE_COLOUR ( '', #19254 ) ;
#1533 = PRODUCT_DEFINITION_CONTEXT ( 'detailed design', #65785, 'design' ) ;
#1534 = CARTESIAN_POINT ( 'NONE',  ( -99.59292637653381064, -3.094860106618431139, -9.524999999999991473 ) ) ;
#1535 = PRODUCT_CONTEXT ( 'NONE', #25304, 'mechanical' ) ;
#1536 = STYLED_ITEM ( 'NONE', ( #12096 ), #56123 ) ;
#1538 = ADVANCED_FACE ( 'NONE', ( #20505 ), #57449, .T. ) ;
#1537 = FILL_AREA_STYLE ('',( #50151 ) ) ;
#1539 =( LENGTH_UNIT ( ) NAMED_UNIT ( * ) SI_UNIT ( .MILLI., .METRE. ) );
#1540 = STYLED_ITEM ( 'NONE', ( #33585 ), #31183 ) ;
#1541 = DIRECTION ( 'NONE',  ( 0.000000000000000000, 0.000000000000000000, -1.000000000000000000 ) ) ;
#1542 = FACE_OUTER_BOUND ( 'NONE', #12338, .T. ) ;
#1543 = AXIS2_PLACEMENT_3D ( 'NONE', #26249, #49714, #27534 ) ;
#1544 = SPHERICAL_SURFACE ( 'NONE', #65316, 0.2500000000000000000 ) ;
#1545 = VERTEX_POINT ( 'NONE', #47649 ) ;
#1546 = FILL_AREA_STYLE_COLOUR ( '', #12747 ) ;
#1547 = ADVANCED_FACE ( 'NONE', ( #20862 ), #47907, .T. ) ;
#1548 = CARTESIAN_POINT ( 'NONE',  ( -15.48999599679679662, 146.4999999999999716, -7.500000000000000000 ) ) ;
#1549 = ORIENTED_EDGE ( 'NONE', *, *, #58572, .F. ) ;
#1550 =( NAMED_UNIT ( * ) SI_UNIT ( $, .STERADIAN. ) SOLID_ANGLE_UNIT ( ) );
#1551 = CIRCLE ( 'NONE', #19577, 111.0000000000000142 ) ;
#1552 = CARTESIAN_POINT ( 'NONE',  ( -4.716976649647098618, 128.2570736234661695, 6.492361379858953008 ) ) ;
#1553 = VECTOR ( 'NONE', #47217, 1000.000000000000000 ) ;
#1554 =( GEOMETRIC_REPRESENTATION_CONTEXT ( 3 ) GLOBAL_UNCERTAINTY_ASSIGNED_CONTEXT ( ( #62966 ) ) GLOBAL_UNIT_ASSIGNED_CONTEXT ( ( #48576, #59403, #49235 ) ) REPRESENTATION_CONTEXT ( 'NONE', 'WORKASPACE' ) );
#1556 = EDGE_CURVE ( 'NONE', #50331, #65395, #9628, .T. ) ;
#1555 = LINE ( 'NONE', #34318, #59 ) ;
#1557 = CARTESIAN_POINT ( 'NONE',  ( 0.000000000000000000, -2.500000000000000000, 0.000000000000000000 ) ) ;
#1558 = ORIENTED_EDGE ( 'NONE', *, *, #27850, .F. ) ;
#1559 = CARTESIAN_POINT ( 'NONE',  ( -115.8570736234661780, -5.598654528085803328, -7.705886871421366635 ) ) ;
#1560 = TOROIDAL_SURFACE ( 'NONE', #6083, 13.49999999999999822, 0.5000000000000000000 ) ;
#1561 = DIRECTION ( 'NONE',  ( 0.9968761159932768567, -0.07898106964430656740, 0.000000000000000000 ) ) ;
#1562 = ORIENTED_EDGE ( 'NONE', *, *, #47547, .T. ) ;
#1563 = CARTESIAN_POINT ( 'NONE',  ( -93.35707362346617799, 5.598654528085804216, 7.705886871421366635 ) ) ;
#1564 = CIRCLE ( 'NONE', #40982, 5.000000000000004441 ) ;
#1565 = DIRECTION ( 'NONE',  ( -1.000000000000000000, 0.000000000000000000, 0.000000000000000000 ) ) ;
#1566 = CARTESIAN_POINT ( 'NONE',  ( -93.44499999999999318, 0.000000000000000000, 8.024999999999991473 ) ) ;
#1567 = VERTEX_POINT ( 'NONE', #30335 ) ;
#1568 = CARTESIAN_POINT ( 'NONE',  ( -20.46001754528041161, 114.7916627990982192, -10.31416700829639588 ) ) ;
#1569 = FACE_OUTER_BOUND ( 'NONE', #46402, .T. ) ;
#1570 =( LENGTH_UNIT ( ) NAMED_UNIT ( * ) SI_UNIT ( .MILLI., .METRE. ) );
#1571 = ORIENTED_EDGE ( 'NONE', *, *, #19374, .T. ) ;
#1572 = CARTESIAN_POINT ( 'NONE',  ( 2.607480562269071989, 160.5929263765337964, 8.025000000000002132 ) ) ;
#1573 = DIRECTION ( 'NONE',  ( 0.000000000000000000, 0.000000000000000000, 1.000000000000000000 ) ) ;
#1574 = VECTOR ( 'NONE', #46104, 1000.000000000000000 ) ;
#1575 = VERTEX_POINT ( 'NONE', #63749 ) ;
#1576 = CARTESIAN_POINT ( 'NONE',  ( -6.062177826491070398, 2.500000000000000000, -3.499999999999998224 ) ) ;
#1577 = VERTEX_POINT ( 'NONE', #26111 ) ;
#1578 = CARTESIAN_POINT ( 'NONE',  ( -137.0929263765344217, 3.094860106628584351, 9.524999999992617816 ) ) ;
#1579 = CARTESIAN_POINT ( 'NONE',  ( 10.99999999999999645, 11.99999999999999289, 3.500000000000004885 ) ) ;
#1580 = CARTESIAN_POINT ( 'NONE',  ( -1.908195823574483386E-14, 24.74999999999996803, 4.000000000000000000 ) ) ;
#1581 = DIRECTION ( 'NONE',  ( -1.000000000000000000, 0.000000000000000000, -0.000000000000000000 ) ) ;
#1582 = CARTESIAN_POINT ( 'NONE',  ( -176.7570736234661695, -5.598654528085801552, 7.705886871421367523 ) ) ;
#1583 = DIRECTION ( 'NONE',  ( 0.000000000000000000, -1.000000000000000000, 0.000000000000000000 ) ) ;
#1584 = DIRECTION ( 'NONE',  ( 0.07854820085872894764, 0.9914125719358882760, 0.1045528208578022367 ) ) ;
#1585 = PRESENTATION_LAYER_ASSIGNMENT (  '', '', ( #69049 ) ) ;
#1586 = CARTESIAN_POINT ( 'NONE',  ( -113.3070736234661666, -10.01517768586948698, 6.132527647946031529E-16 ) ) ;
#1587 = EDGE_CURVE ( 'NONE', #66764, #12604, #46944, .T. ) ;
#1588 = CARTESIAN_POINT ( 'NONE',  ( -1.805736402306164390, 9.000000000000007105, 0.1687517039304846367 ) ) ;
#1589 = CARTESIAN_POINT ( 'NONE',  ( 39.24999999999999289, 16.24999999999997513, -4.000000000000000000 ) ) ;
#1590 = ORIENTED_EDGE ( 'NONE', *, *, #7241, .T. ) ;
#1591 = CARTESIAN_POINT ( 'NONE',  ( -23.21231517720797655, 117.4999999999999716, -7.500000000000000000 ) ) ;
#1592 = DIRECTION ( 'NONE',  ( 0.000000000000000000, 0.000000000000000000, -1.000000000000000000 ) ) ;
#1593 = CARTESIAN_POINT ( 'NONE',  ( -34.99999999999992895, 112.9999999999999858, -7.500000000000000000 ) ) ;
#1594 = DIRECTION ( 'NONE',  ( 0.000000000000000000, 0.000000000000000000, -1.000000000000000000 ) ) ;
#1595 = VERTEX_POINT ( 'NONE', #46600 ) ;
#1596 = CARTESIAN_POINT ( 'NONE',  ( -160.4049999999999727, -2.607480562269069768, 8.024999999999991473 ) ) ;
#1597 = DIRECTION ( 'NONE',  ( 1.000000000000000000, -0.000000000000000000, -0.000000000000000000 ) ) ;
#1598 = CARTESIAN_POINT ( 'NONE',  ( -183.9007312495837425, -8.565707761958867295, -1.052177752376815212 ) ) ;
#1599 = CARTESIAN_POINT ( 'NONE',  ( -176.8449999999999989, -7.632228543268599452, 2.479861379858951054 ) ) ;
#1600 = CARTESIAN_POINT ( 'NONE',  ( -156.5949999999999704, 2.607480562269072433, 8.024999999999991473 ) ) ;
#1601 = ORIENTED_EDGE ( 'NONE', *, *, #20283, .F. ) ;
#1602 = AXIS2_PLACEMENT_3D ( 'NONE', #64294, #16145, #53733 ) ;
#1603 = DIRECTION ( 'NONE',  ( -1.000000000000000000, -0.000000000000000000, -0.000000000000000000 ) ) ;
#1604 = AXIS2_PLACEMENT_3D ( 'NONE', #45387, #50619, #61489 ) ;
#1605 = CARTESIAN_POINT ( 'NONE',  ( 44.97464006314717722, 9.991546687716530428, 3.784415753861383180 ) ) ;
#1606 = DIRECTION ( 'NONE',  ( -0.000000000000000000, 1.000000000000000000, -0.000000000000000000 ) ) ;
#1607 = CARTESIAN_POINT ( 'NONE',  ( -77.60499999999996135, 6.826472737025113702, -4.959722759717902107 ) ) ;
#1608 = CARTESIAN_POINT ( 'NONE',  ( -38.76790784220121111, -11.41832517657503487, 3.451608923803376250 ) ) ;
#1609 = EDGE_CURVE ( 'NONE', #36722, #59012, #4024, .T. ) ;
#1610 = AXIS2_PLACEMENT_3D ( 'NONE', #32355, #32704, #38392 ) ;
#1611 = CARTESIAN_POINT ( 'NONE',  ( -74.54499999999998749, -7.632228543268600340, -2.479861379858950166 ) ) ;
#1612 = EDGE_CURVE ( 'NONE', #51275, #57245, #37073, .T. ) ;
#1613 = CARTESIAN_POINT ( 'NONE',  ( 8.102448949553183510, 149.1049999999999898, -5.886773742842746238 ) ) ;
#1614 = CARTESIAN_POINT ( 'NONE',  ( -0.7087670488506461197, 2.466410156631503092, -7.000000000000004441 ) ) ;
#1615 = CIRCLE ( 'NONE', #33116, 8.000000000000000000 ) ;
#1616 =( GEOMETRIC_REPRESENTATION_CONTEXT ( 3 ) GLOBAL_UNCERTAINTY_ASSIGNED_CONTEXT ( ( #47498 ) ) GLOBAL_UNIT_ASSIGNED_CONTEXT ( ( #59921, #33874, #38861 ) ) REPRESENTATION_CONTEXT ( 'NONE', 'WORKASPACE' ) );
#1617 = VECTOR ( 'NONE', #37214, 1000.000000000000000 ) ;
#1618 = CARTESIAN_POINT ( 'NONE',  ( 6.669484432089998194, 154.4410788397644296, 6.756431230636611218 ) ) ;
#1619 = UNCERTAINTY_MEASURE_WITH_UNIT (LENGTH_MEASURE( 1.000000000000000082E-05 ), #22366, 'distance_accuracy_value', 'NONE');
#1620 = SURFACE_STYLE_FILL_AREA ( #39684 ) ;
#1621 = DIRECTION ( 'NONE',  ( -1.000000000000000000, 0.000000000000000000, 0.000000000000000000 ) ) ;
#1622 = EDGE_CURVE ( 'NONE', #27240, #5819, #10310, .T. ) ;
#1623 =( NAMED_UNIT ( * ) PLANE_ANGLE_UNIT ( ) SI_UNIT ( $, .RADIAN. ) );
#1624 = FILL_AREA_STYLE ('',( #50225 ) ) ;
#1625 = AXIS2_PLACEMENT_3D ( 'NONE', #5260, #1583, #17827 ) ;
#1626 = EDGE_CURVE ( 'NONE', #10996, #37203, #42701, .T. ) ;
#1627 = PRESENTATION_LAYER_ASSIGNMENT (  '', '', ( #38788 ) ) ;
#1628 = CARTESIAN_POINT ( 'NONE',  ( -72.49999999999998579, 119.9999999999997868, 10.00000000000000000 ) ) ;
#1629 =( GEOMETRIC_REPRESENTATION_CONTEXT ( 3 ) GLOBAL_UNCERTAINTY_ASSIGNED_CONTEXT ( ( #55915 ) ) GLOBAL_UNIT_ASSIGNED_CONTEXT ( ( #24364, #66237, #23005 ) ) REPRESENTATION_CONTEXT ( 'NONE', 'WORKASPACE' ) );
#1630 = CARTESIAN_POINT ( 'NONE',  ( -119.2429263765338021, 5.598654528085804216, 7.705886871421366635 ) ) ;
#1631 = EDGE_CURVE ( 'NONE', #16182, #69681, #26785, .T. ) ;
#1632 = ORIENTED_EDGE ( 'NONE', *, *, #18041, .F. ) ;
#1633 = ORIENTED_EDGE ( 'NONE', *, *, #46764, .T. ) ;
#1634 =( LENGTH_UNIT ( ) NAMED_UNIT ( * ) SI_UNIT ( .MILLI., .METRE. ) );
#1636 = CARTESIAN_POINT ( 'NONE',  ( -133.2570736234661695, 5.598654528085800663, -7.705886871421367523 ) ) ;
#1635 = CIRCLE ( 'NONE', #50027, 13.99999999999999822 ) ;
#1637 = AXIS2_PLACEMENT_3D ( 'NONE', #41069, #3710, #52317 ) ;
#1638 = EDGE_CURVE ( 'NONE', #24543, #61513, #25382, .T. ) ;
#1639 =( LENGTH_UNIT ( ) NAMED_UNIT ( * ) SI_UNIT ( .MILLI., .METRE. ) );
#1640 = DIRECTION ( 'NONE',  ( 0.000000000000000000, -1.000000000000000000, 0.000000000000000000 ) ) ;
#1641 =( BOUNDED_SURFACE ( )  B_SPLINE_SURFACE ( 3, 2, ( 
 ( #832, #59649, #11466 ),
 ( #38942, #48455, #54708 ),
 ( #5828, #146, #21676 ),
 ( #32938, #6514, #43196 ),
 ( #64601, #27957, #16448 ),
 ( #49466, #65630, #55058 ),
 ( #40659, #8633, #34319 ),
 ( #18820, #56455, #30063 ),
 ( #12853, #3292, #55772 ),
 ( #2601, #45254, #45610 ) ),
 .UNSPECIFIED., .F., .F., .F. ) 
 B_SPLINE_SURFACE_WITH_KNOTS ( ( 4, 2, 2, 2, 4 ),
 ( 3, 3 ),
 ( 3.141592653589793116, 3.534291735288517255, 3.926990816987241395, 4.319689898685965090, 4.712388980384689674 ),
 ( 0.000000000000000000, 1.000000000000000000 ),
 .UNSPECIFIED. ) 
 GEOMETRIC_REPRESENTATION_ITEM ( )  RATIONAL_B_SPLINE_SURFACE ( (
 ( 1.000000000000000000, 0.8112421851755602376, 1.000000000000000000),
 ( 1.000000000000000000, 0.8112499556556433955, 1.000000000000000000),
 ( 1.000000000000000000, 0.8087168080150066718, 1.000000000000000000),
 ( 1.000000000000000000, 0.7988629633398904861, 1.000000000000000000),
 ( 1.000000000000000000, 0.7915339219236784407, 1.000000000000000000),
 ( 1.000000000000000000, 0.7728233248393433508, 1.000000000000000000),
 ( 1.000000000000000000, 0.7614408922480963016, 1.000000000000000000),
 ( 1.000000000000000000, 0.7359001690392014128, 1.000000000000000000),
 ( 1.000000000000000000, 0.7217502572879682665, 1.000000000000000000),
 ( 1.000000000000000000, 0.7071067811865475727, 1.000000000000000000) ) ) 
 REPRESENTATION_ITEM ( '' )  SURFACE ( )  );
#1642 = DIRECTION ( 'NONE',  ( 0.000000000000000000, 0.000000000000000000, -1.000000000000000000 ) ) ;
#1643 = CARTESIAN_POINT ( 'NONE',  ( 71.74137931034481142, 36.89918356738973415, -10.00000000000000000 ) ) ;
#1644 = ORIENTED_EDGE ( 'NONE', *, *, #8589, .T. ) ;
#1645 = CARTESIAN_POINT ( 'NONE',  ( -113.3049999999999784, 8.437984349512086979, -1.550032578732815448E-15 ) ) ;
#1646 = ORIENTED_EDGE ( 'NONE', *, *, #26508, .F. ) ;
#1647 =( LENGTH_UNIT ( ) NAMED_UNIT ( * ) SI_UNIT ( .MILLI., .METRE. ) );
#1648 = DIRECTION ( 'NONE',  ( 1.000000000000000000, 0.000000000000000000, -0.000000000000000000 ) ) ;
#1649 = ORIENTED_EDGE ( 'NONE', *, *, #32637, .T. ) ;
#1650 = DIRECTION ( 'NONE',  ( -1.000000000000000000, -7.709882115452468306E-16, 0.000000000000000000 ) ) ;
#1651 = LINE ( 'NONE', #60764, #28776 ) ;
#1652 = VERTEX_POINT ( 'NONE', #54585 ) ;
#1653 = DIRECTION ( 'NONE',  ( -1.000000000000000000, 0.000000000000000000, 0.000000000000000000 ) ) ;
#1654 = EDGE_LOOP ( 'NONE', ( #63446, #32269, #54881, #12806 ) ) ;
#1655 = EDGE_LOOP ( 'NONE', ( #19080, #40394, #14488, #19156 ) ) ;
#1656 = AXIS2_PLACEMENT_3D ( 'NONE', #868, #6233, #22410 ) ;
#1657 = CARTESIAN_POINT ( 'NONE',  ( -74.42859372179059108, 8.073499555448577780, -6.500000000000000888 ) ) ;
#1658 = DIRECTION ( 'NONE',  ( -0.2503800040544290062, 0.000000000000000000, -0.9681476403781109630 ) ) ;
#1659 = SURFACE_STYLE_USAGE ( .BOTH. , #60434 ) ;
#1660 = VERTEX_POINT ( 'NONE', #43729 ) ;
#1661 = CARTESIAN_POINT ( 'NONE',  ( -6.826472737025120807, 132.3929263765338362, -4.959722759717907437 ) ) ;
#1662 = DIRECTION ( 'NONE',  ( 0.000000000000000000, 0.000000000000000000, -1.000000000000000000 ) ) ;
#1663 = DIRECTION ( 'NONE',  ( 0.000000000000000000, 1.000000000000000000, 0.000000000000000000 ) ) ;
#1664 = EDGE_LOOP ( 'NONE', ( #14425, #17146, #44162, #32760 ) ) ;
#1665 = DIRECTION ( 'NONE',  ( 0.000000000000000000, 0.000000000000000000, -1.000000000000000000 ) ) ;
#1666 = ORIENTED_EDGE ( 'NONE', *, *, #5331, .T. ) ;
#1667 = CYLINDRICAL_SURFACE ( 'NONE', #31576, 1.000000000000000888 ) ;
#1668 = TOROIDAL_SURFACE ( 'NONE', #28618, 8.499999999999998224, 0.5000000000000000000 ) ;
#1669 = DIRECTION ( 'NONE',  ( 1.000000000000000000, 0.000000000000000000, 0.000000000000000000 ) ) ;
#1670 = CARTESIAN_POINT ( 'NONE',  ( 4.041451884327379673, -7.000000000000002665, 7.500000000000000000 ) ) ;
#1671 = CARTESIAN_POINT ( 'NONE',  ( -129.8050000000000068, -8.437984349512085203, 5.166775262442717831E-16 ) ) ;
#1672 = SURFACE_STYLE_FILL_AREA ( #29489 ) ;
#1673 = FILL_AREA_STYLE ('',( #34756 ) ) ;
#1674 = EDGE_LOOP ( 'NONE', ( #43799, #46856, #2229, #60113 ) ) ;
#1675 = ADVANCED_FACE ( 'NONE', ( #48314 ), #22028, .T. ) ;
#1676 = CARTESIAN_POINT ( 'NONE',  ( -40.66823730937047543, -13.67203837763575436, 0.8500273690653776804 ) ) ;
#1677 = CARTESIAN_POINT ( 'NONE',  ( -157.7929263765340977, -3.094860106612715711, 9.525000000004141043 ) ) ;
#1678 = CARTESIAN_POINT ( 'NONE',  ( -45.00000000000000000, 7.768687147774684831, -6.999999999999999112 ) ) ;
#1679 = ORIENTED_EDGE ( 'NONE', *, *, #11278, .T. ) ;
#1680 = VERTEX_POINT ( 'NONE', #372 ) ;
#1681 = DIRECTION ( 'NONE',  ( -1.000000000000000000, 0.000000000000000000, 0.000000000000000000 ) ) ;
#1682 = DIRECTION ( 'NONE',  ( -0.000000000000000000, 0.000000000000000000, -1.000000000000000000 ) ) ;
#1683 = CARTESIAN_POINT ( 'NONE',  ( -50.45499999999996987, 7.632228543268599452, -2.479861379858951942 ) ) ;
#1685 = EDGE_LOOP ( 'NONE', ( #59397, #57758, #23436, #341 ) ) ;
#1684 = AXIS2_PLACEMENT_3D ( 'NONE', #54632, #6442, #1096 ) ;
#1686 = DIRECTION ( 'NONE',  ( 0.000000000000000000, 1.000000000000000000, 0.000000000000000000 ) ) ;
#1687 =( NAMED_UNIT ( * ) SI_UNIT ( $, .STERADIAN. ) SOLID_ANGLE_UNIT ( ) );
#1688 = DIRECTION ( 'NONE',  ( 0.000000000000000000, 0.000000000000000000, 1.000000000000000000 ) ) ;
#1689 = TOROIDAL_SURFACE ( 'NONE', #36598, 9.499999999999996447, 0.5000000000000000000 ) ;
#1690 = AXIS2_PLACEMENT_3D ( 'NONE', #2054, #13035, #33454 ) ;
#1691 = ORIENTED_EDGE ( 'NONE', *, *, #43453, .F. ) ;
#1692 = SURFACE_STYLE_FILL_AREA ( #49957 ) ;
#1693 = EDGE_CURVE ( 'NONE', #63720, #28531, #45617, .T. ) ;
#1694 = SURFACE_SIDE_STYLE ('',( #54512 ) ) ;
#1695 = VECTOR ( 'NONE', #24083, 1000.000000000000000 ) ;
#1696 = DIRECTION ( 'NONE',  ( 0.7071067811865352493, 8.659560562354781249E-17, -0.7071067811865597852 ) ) ;
#1697 = LINE ( 'NONE', #55562, #35972 ) ;
#1698 = EDGE_CURVE ( 'NONE', #34648, #11331, #27618, .T. ) ;
#1699 = EDGE_CURVE ( 'NONE', #24423, #69362, #16641, .T. ) ;
#1700 = CARTESIAN_POINT ( 'NONE',  ( -97.49499999999999034, 6.826472737025113702, -4.959722759717902107 ) ) ;
#1701 = EDGE_CURVE ( 'NONE', #44158, #54061, #62331, .T. ) ;
#1702 = CARTESIAN_POINT ( 'NONE',  ( 9.058813317711337021, 115.6549999999999869, 2.943386871421375783 ) ) ;
#1703 = CARTESIAN_POINT ( 'NONE',  ( -80.99499999999999034, -6.826472737025115478, 4.959722759717900331 ) ) ;
#1704 = SURFACE_SIDE_STYLE ('',( #19304 ) ) ;
#1705 = DIRECTION ( 'NONE',  ( 0.000000000000000000, -1.000000000000000000, -0.000000000000000000 ) ) ;
#1706 = CYLINDRICAL_SURFACE ( 'NONE', #4736, 0.2500000000000002220 ) ;
#1707 = UNCERTAINTY_MEASURE_WITH_UNIT (LENGTH_MEASURE( 1.000000000000000082E-05 ), #61396, 'distance_accuracy_value', 'NONE');
#1708 = CIRCLE ( 'NONE', #23156, 0.5000000000000004441 ) ;
#1709 = CYLINDRICAL_SURFACE ( 'NONE', #68980, 0.5000000000000004441 ) ;
#1710 = ORIENTED_EDGE ( 'NONE', *, *, #3780, .F. ) ;
#1711 = CARTESIAN_POINT ( 'NONE',  ( -125.2429263765338021, 5.598654528085804216, 7.705886871421366635 ) ) ;
#1712 = CARTESIAN_POINT ( 'NONE',  ( 0.000000000000000000, 0.000000000000000000, 0.000000000000000000 ) ) ;
#1713 = CARTESIAN_POINT ( 'NONE',  ( -140.9949999999999193, -6.826472737025115478, 4.959722759717900331 ) ) ;
#1714 = SURFACE_SIDE_STYLE ('',( #49980 ) ) ;
#1715 = ADVANCED_FACE ( 'NONE', ( #22942 ), #38109, .F. ) ;
#1716 = VECTOR ( 'NONE', #36325, 1000.000000000000000 ) ;
#1717 = DIRECTION ( 'NONE',  ( -1.000000000000000000, 0.000000000000000000, 0.000000000000000000 ) ) ;
#1718 = AXIS2_PLACEMENT_3D ( 'NONE', #43200, #48810, #44230 ) ;
#1719 = DIRECTION ( 'NONE',  ( 1.000000000000000000, 0.000000000000000000, 0.000000000000000000 ) ) ;
#1720 = EDGE_LOOP ( 'NONE', ( #55191, #20863, #22219, #51454 ) ) ;
#1721 = VERTEX_POINT ( 'NONE', #11327 ) ;
#1722 = COLOUR_RGB ( '', 0.40784314, 0.44705882, 0.49803922) ;
#1723 = DIRECTION ( 'NONE',  ( -0.000000000000000000, -0.000000000000000000, -1.000000000000000000 ) ) ;
#1724 = CARTESIAN_POINT ( 'NONE',  ( 71.49999999999998579, 64.07124727947029896, 7.500000000000000000 ) ) ;
#1725 = LINE ( 'NONE', #54872, #40584 ) ;
#1726 = CARTESIAN_POINT ( 'NONE',  ( -51.50000000000000000, -2.024042244987997205E-14, 10.50000000000000000 ) ) ;
#1727 = CARTESIAN_POINT ( 'NONE',  ( -7.440601873764707719, -1.112499515747335854, 0.4948905776603325646 ) ) ;
#1728 = SPHERICAL_SURFACE ( 'NONE', #52931, 0.5000000000000000000 ) ;
#1729 = ORIENTED_EDGE ( 'NONE', *, *, #50153, .T. ) ;
#1730 = CARTESIAN_POINT ( 'NONE',  ( -143.4550000000000125, 7.632228543268599452, -2.479861379858951942 ) ) ;
#1731 = VERTEX_POINT ( 'NONE', #33480 ) ;
#1732 = STYLED_ITEM ( 'NONE', ( #50330 ), #39268 ) ;
#1733 = EDGE_CURVE ( 'NONE', #6729, #52429, #35213, .T. ) ;
#1734 = ORIENTED_EDGE ( 'NONE', *, *, #43890, .T. ) ;
#1735 = CARTESIAN_POINT ( 'NONE',  ( -0.4882456337924103162, 152.9710135830613069, -8.025000000000005684 ) ) ;
#1736 = DIRECTION ( 'NONE',  ( -0.8660254037844385966, -0.5000000000000002220, 0.000000000000000000 ) ) ;
#1737 = ORIENTED_EDGE ( 'NONE', *, *, #52562, .F. ) ;
#1738 = AXIS2_PLACEMENT_3D ( 'NONE', #27033, #21799, #43312 ) ;
#1739 = AXIS2_PLACEMENT_3D ( 'NONE', #15953, #4662, #41642 ) ;
#1740 = LINE ( 'NONE', #30843, #5683 ) ;
#1741 = ADVANCED_FACE ( 'NONE', ( #28162 ), #27492, .F. ) ;
#1742 = FACE_OUTER_BOUND ( 'NONE', #52453, .T. ) ;
#1743 = CARTESIAN_POINT ( 'NONE',  ( 8.102448949553181734, 132.3949999999999534, 5.886773742842750679 ) ) ;
#1744 = ORIENTED_EDGE ( 'NONE', *, *, #38315, .T. ) ;
#1745 = CARTESIAN_POINT ( 'NONE',  ( -8.102448949553179958, 141.0049999999999670, -5.886773742842749790 ) ) ;
#1746 = CARTESIAN_POINT ( 'NONE',  ( -58.10499999999998977, -6.826472737025113702, 4.959722759717902107 ) ) ;
#1747 = CARTESIAN_POINT ( 'NONE',  ( 44.99999999999998579, 119.9999999999999716, 10.00000000000000000 ) ) ;
#1748 = VERTEX_POINT ( 'NONE', #50030 ) ;
#1749 = CARTESIAN_POINT ( 'NONE',  ( 0.000000000000000000, 161.5550000000000068, -9.525000000000000355 ) ) ;
#1750 = DIRECTION ( 'NONE',  ( 1.000000000000000000, -0.000000000000000000, 0.000000000000000000 ) ) ;
#1751 = UNCERTAINTY_MEASURE_WITH_UNIT (LENGTH_MEASURE( 1.000000000000000082E-05 ), #36044, 'distance_accuracy_value', 'NONE');
#1752 = DIRECTION ( 'NONE',  ( 0.000000000000000000, -1.000000000000000000, 0.000000000000000000 ) ) ;
#1753 =( LENGTH_UNIT ( ) NAMED_UNIT ( * ) SI_UNIT ( .MILLI., .METRE. ) );
#1754 = PRESENTATION_STYLE_ASSIGNMENT (( #22929 ) ) ;
#1755 = ORIENTED_EDGE ( 'NONE', *, *, #50050, .F. ) ;
#1756 = ORIENTED_EDGE ( 'NONE', *, *, #7312, .F. ) ;
#1757 = DIRECTION ( 'NONE',  ( -0.000000000000000000, -1.000000000000000000, 0.000000000000000000 ) ) ;
#1758 = CARTESIAN_POINT ( 'NONE',  ( -74.99999999999998579, 119.9999999999997726, -9.500000000000000000 ) ) ;
#1759 = SURFACE_SIDE_STYLE ('',( #50022 ) ) ;
#1760 = CARTESIAN_POINT ( 'NONE',  ( -164.7549999999999955, 4.716976649647091513, -6.492361379858946790 ) ) ;
#1761 = ORIENTED_EDGE ( 'NONE', *, *, #46779, .T. ) ;
#1762 = UNCERTAINTY_MEASURE_WITH_UNIT (LENGTH_MEASURE( 1.000000000000000082E-05 ), #2360, 'distance_accuracy_value', 'NONE');
#1763 = AXIS2_PLACEMENT_3D ( 'NONE', #60378, #40701, #63172 ) ;
#1764 = CARTESIAN_POINT ( 'NONE',  ( 48.50000000000000000, 99.99999999999998579, 7.500000000000000000 ) ) ;
#1765 = DIRECTION ( 'NONE',  ( 0.5000000000000001110, 0.8660254037844384856, 0.000000000000000000 ) ) ;
#1766 = ORIENTED_EDGE ( 'NONE', *, *, #12022, .F. ) ;
#1767 = ORIENTED_EDGE ( 'NONE', *, *, #3874, .F. ) ;
#1768 = DIRECTION ( 'NONE',  ( 0.7071067811865474617, 0.000000000000000000, 0.7071067811865474617 ) ) ;
#1769 = CYLINDRICAL_SURFACE ( 'NONE', #53748, 9.524999999999991473 ) ;
#1770 = CARTESIAN_POINT ( 'NONE',  ( -82.25499999999998124, -4.716976649647092401, 6.492361379858946790 ) ) ;
#1771 = ORIENTED_EDGE ( 'NONE', *, *, #28441, .T. ) ;
#1772 = PRESENTATION_STYLE_ASSIGNMENT (( #8156 ) ) ;
#1773 = EDGE_CURVE ( 'NONE', #32850, #4180, #8147, .T. ) ;
#1774 = CARTESIAN_POINT ( 'NONE',  ( -150.0570736234661808, 0.000000000000000000, 9.524999999999991473 ) ) ;
#1775 =( BOUNDED_CURVE ( )  B_SPLINE_CURVE ( 2, ( #49571, #53783, #43311, #60108, #6619, #11923, #21433, #64352, #17240, #11226, #16201 ),
 .UNSPECIFIED., .F., .F. ) 
 B_SPLINE_CURVE_WITH_KNOTS ( ( 3, 2, 2, 2, 2, 3 ),
 ( 0.2647058823529411242, 0.2705882352941175739, 0.2764705882352940791, 0.2823529411764705843, 0.2882352941176470340, 0.2941176470588235392 ),
 .UNSPECIFIED. ) 
 CURVE ( )  GEOMETRIC_REPRESENTATION_ITEM ( )  RATIONAL_B_SPLINE_CURVE ( ( 1.000000000000000666, 0.9510565162951531981, 1.000000000000000000, 0.9510565162951535312, 1.000000000000000000, 0.9510565162951535312, 1.000000000000000000, 0.9510565162951535312, 1.000000000000000000, 0.9510565162951535312, 1.000000000000000000 ) ) 
 REPRESENTATION_ITEM ( '' )  );
#1776 = EDGE_CURVE ( 'NONE', #32384, #10461, #7100, .T. ) ;
#1777 = CARTESIAN_POINT ( 'NONE',  ( -75.00000000000000000, 8.841134989787066800, -6.848475133234801504 ) ) ;
#1778 = ORIENTED_EDGE ( 'NONE', *, *, #49397, .T. ) ;
#1779 = DIRECTION ( 'NONE',  ( 1.000000000000000000, 0.000000000000000000, 0.000000000000000000 ) ) ;
#1781 = FILL_AREA_STYLE ('',( #28545 ) ) ;
#1780 = CARTESIAN_POINT ( 'NONE',  ( -52.55707362346618083, -1.166476076187852838E-15, -9.524999999999991473 ) ) ;
#1782 = AXIS2_PLACEMENT_3D ( 'NONE', #26676, #58364, #37307 ) ;
#1783 = ADVANCED_FACE ( 'NONE', ( #39485 ), #63546, .T. ) ;
#1784 = CARTESIAN_POINT ( 'NONE',  ( 3.094860106618435136, 130.2949999999999591, -9.525000000000000355 ) ) ;
#1785 = CARTESIAN_POINT ( 'NONE',  ( -107.2449999999999903, -4.716976649647093289, -6.492361379858945902 ) ) ;
#1786 = CARTESIAN_POINT ( 'NONE',  ( 26.00000000000001776, -3.148064030671221758, -29.68999999999999417 ) ) ;
#1788 = CARTESIAN_POINT ( 'NONE',  ( -19.48793012548083325, 11.79525974137268562, 2.228109774474827276 ) ) ;
#1787 = CARTESIAN_POINT ( 'NONE',  ( -33.13898406348611303, -9.269969315817824906, -2.682282538649360504 ) ) ;
#1789 = CARTESIAN_POINT ( 'NONE',  ( -152.2429263765338021, 5.598654528085804216, 7.705886871421366635 ) ) ;
#1790 = CARTESIAN_POINT ( 'NONE',  ( -165.1449999999999818, -4.716976649647092401, 6.492361379858946790 ) ) ;
#1791 = ADVANCED_FACE ( 'NONE', ( #23614 ), #55969, .F. ) ;
#1792 = CYLINDRICAL_SURFACE ( 'NONE', #51211, 5.000000000000011546 ) ;
#1793 = CARTESIAN_POINT ( 'NONE',  ( 57.00000000000000000, 14.00000000000000000, 60.00402776293827145 ) ) ;
#1794 = ORIENTED_EDGE ( 'NONE', *, *, #4602, .F. ) ;
#1795 = DIRECTION ( 'NONE',  ( -2.478176394252586564E-16, 0.000000000000000000, -1.000000000000000000 ) ) ;
#1796 = EDGE_LOOP ( 'NONE', ( #11898, #17901, #30240, #23916 ) ) ;
#1797 = CARTESIAN_POINT ( 'NONE',  ( -64.64292637653379359, -5.598654528085801552, 7.705886871421367523 ) ) ;
#1798 = DIRECTION ( 'NONE',  ( 0.000000000000000000, 0.000000000000000000, 1.000000000000000000 ) ) ;
#1799 = CARTESIAN_POINT ( 'NONE',  ( 3.249999999999999112, 34.24999999999998579, -4.000000000000000000 ) ) ;
#1800 = FACE_BOUND ( 'NONE', #63024, .T. ) ;
#1801 = DIRECTION ( 'NONE',  ( -1.000000000000000000, 0.000000000000000000, 0.000000000000000000 ) ) ;
#1802 = AXIS2_PLACEMENT_3D ( 'NONE', #26945, #38281, #12170 ) ;
#1803 = ORIENTED_EDGE ( 'NONE', *, *, #14374, .T. ) ;
#1804 = CARTESIAN_POINT ( 'NONE',  ( -169.8550000000000182, 4.716976649647094177, 6.492361379858945902 ) ) ;
#1805 = ORIENTED_EDGE ( 'NONE', *, *, #57852, .F. ) ;
#1806 = DIRECTION ( 'NONE',  ( -1.000000000000000000, 0.000000000000000000, 0.000000000000000000 ) ) ;
#1807 = AXIS2_PLACEMENT_3D ( 'NONE', #58819, #22571, #64084 ) ;
#1808 = SURFACE_STYLE_USAGE ( .BOTH. , #12757 ) ;
#1809 = CARTESIAN_POINT ( 'NONE',  ( 2.607480562269071989, 155.7070736234661297, 8.025000000000002132 ) ) ;
#1810 = ORIENTED_EDGE ( 'NONE', *, *, #45487, .T. ) ;
#1811 = DIRECTION ( 'NONE',  ( 0.000000000000000000, 0.000000000000000000, -1.000000000000000000 ) ) ;
#1812 =( NAMED_UNIT ( * ) PLANE_ANGLE_UNIT ( ) SI_UNIT ( $, .RADIAN. ) );
#1813 = CARTESIAN_POINT ( 'NONE',  ( -82.55499999999999261, 0.000000000000000000, 8.024999999999991473 ) ) ;
#1814 = DIRECTION ( 'NONE',  ( 1.000000000000000000, 0.000000000000000000, 0.000000000000000000 ) ) ;
#1815 = CARTESIAN_POINT ( 'NONE',  ( 8.102448949553183510, 131.1049999999999898, -5.886773742842746238 ) ) ;
#1816 = UNCERTAINTY_MEASURE_WITH_UNIT (LENGTH_MEASURE( 1.000000000000000082E-05 ), #38811, 'distance_accuracy_value', 'NONE');
#1817 = DIRECTION ( 'NONE',  ( 0.000000000000000000, 0.000000000000000000, 1.000000000000000000 ) ) ;
#1818 = SURFACE_STYLE_USAGE ( .BOTH. , #39901 ) ;
#1819 =( GEOMETRIC_REPRESENTATION_CONTEXT ( 3 ) GLOBAL_UNCERTAINTY_ASSIGNED_CONTEXT ( ( #30589 ) ) GLOBAL_UNIT_ASSIGNED_CONTEXT ( ( #44578, #59656, #11474 ) ) REPRESENTATION_CONTEXT ( 'NONE', 'WORKASPACE' ) );
#1820 = CARTESIAN_POINT ( 'NONE',  ( -127.0429263765337993, -9.058813317711329915, -2.943386871421370898 ) ) ;
#1821 = CARTESIAN_POINT ( 'NONE',  ( -112.9429263765338050, 0.000000000000000000, 9.524999999999991473 ) ) ;
#1822 = SURFACE_SIDE_STYLE ('',( #39904 ) ) ;
#1823 = CARTESIAN_POINT ( 'NONE',  ( -112.5570736234661808, -1.166476076187852838E-15, -9.524999999999991473 ) ) ;
#1824 = ORIENTED_EDGE ( 'NONE', *, *, #60940, .F. ) ;
#1825 = SURFACE_SIDE_STYLE ('',( #7509 ) ) ;
#1826 = PRESENTATION_STYLE_ASSIGNMENT (( #35294 ) ) ;
#1827 = CARTESIAN_POINT ( 'NONE',  ( -53.84499999999997755, -7.632228543268599452, 2.479861379858951054 ) ) ;
#1828 = VERTEX_POINT ( 'NONE', #24633 ) ;
#1829 = CARTESIAN_POINT ( 'NONE',  ( 0.000000000000000000, -2.500000000000000000, 0.000000000000000000 ) ) ;
#1830 = LINE ( 'NONE', #54984, #13241 ) ;
#1831 = CARTESIAN_POINT ( 'NONE',  ( -45.00000000000000000, 8.062885781073932279, -5.999999999999994671 ) ) ;
#1832 = DIRECTION ( 'NONE',  ( 0.000000000000000000, 0.000000000000000000, -1.000000000000000000 ) ) ;
#1833 = EDGE_LOOP ( 'NONE', ( #2523, #16517, #30246, #42888 ) ) ;
#1834 = CARTESIAN_POINT ( 'NONE',  ( -48.09626709540965095, -13.32227690487224692, 2.730064154176659041 ) ) ;
#1835 = CARTESIAN_POINT ( 'NONE',  ( -49.04499999999998039, 7.632228543268600340, 2.479861379858949277 ) ) ;
#1836 = CARTESIAN_POINT ( 'NONE',  ( 10.00000000000001954, 42.00000000000000000, 28.38386403503541899 ) ) ;
#1837 = VERTEX_POINT ( 'NONE', #17677 ) ;
#1838 = CARTESIAN_POINT ( 'NONE',  ( -75.00000000000000000, 9.371995676438187317, 6.584629826274253084 ) ) ;
#1839 = CARTESIAN_POINT ( 'NONE',  ( -114.6549999999999869, -7.632228543268600340, -2.479861379858950166 ) ) ;
#1840 = ORIENTED_EDGE ( 'NONE', *, *, #16931, .T. ) ;
#1841 = CARTESIAN_POINT ( 'NONE',  ( -4.716976649647097730, 118.3570736234661638, -6.492361379858953896 ) ) ;
#1842 = EDGE_CURVE ( 'NONE', #17714, #62163, #39146, .T. ) ;
#1843 =( NAMED_UNIT ( * ) SI_UNIT ( $, .STERADIAN. ) SOLID_ANGLE_UNIT ( ) );
#1844 = FACE_OUTER_BOUND ( 'NONE', #6899, .T. ) ;
#1845 = CARTESIAN_POINT ( 'NONE',  ( -154.1070736234661922, 8.102448949553171076, -5.886773742842744461 ) ) ;
#1846 = CARTESIAN_POINT ( 'NONE',  ( 57.00000000000000000, 5.000000000000000000, 77.00402776293825013 ) ) ;
#1847 = CARTESIAN_POINT ( 'NONE',  ( -9.058813317711337021, 143.0449999999999875, -2.943386871421374895 ) ) ;
#1848 = CARTESIAN_POINT ( 'NONE',  ( -87.20707362346618652, 3.094860106618433360, 9.524999999999991473 ) ) ;
#1849 = CARTESIAN_POINT ( 'NONE',  ( -54.73148258177910463, -9.107254030097818642, -1.999999999999995781 ) ) ;
#1850 = ORIENTED_EDGE ( 'NONE', *, *, #31656, .T. ) ;
#1851 = EDGE_CURVE ( 'NONE', #21243, #7407, #37805, .T. ) ;
#1852 = CARTESIAN_POINT ( 'NONE',  ( -9.250000000000003553, 25.24999999999998934, 4.000000000000000000 ) ) ;
#1853 = MECHANICAL_DESIGN_GEOMETRIC_PRESENTATION_REPRESENTATION (  '', ( #45784 ), #19877 ) ;
#1854 = CARTESIAN_POINT ( 'NONE',  ( -126.5049999999999528, -6.826472737025115478, -4.959722759717899443 ) ) ;
#1855 = EDGE_CURVE ( 'NONE', #49204, #16450, #7425, .T. ) ;
#1856 = LINE ( 'NONE', #54338, #19580 ) ;
#1857 = VECTOR ( 'NONE', #11669, 1000.000000000000000 ) ;
#1858 = DIRECTION ( 'NONE',  ( -0.000000000000000000, 1.000000000000000000, 0.000000000000000000 ) ) ;
#1859 = CARTESIAN_POINT ( 'NONE',  ( -132.5949999999999989, 2.607480562269073321, 8.024999999999991473 ) ) ;
#1860 = EDGE_CURVE ( 'NONE', #23940, #51066, #49036, .T. ) ;
#1861 = AXIS2_PLACEMENT_3D ( 'NONE', #1210, #22048, #4910 ) ;
#1862 = CARTESIAN_POINT ( 'NONE',  ( -127.7949999999999875, 2.607480562269069324, -8.024999999999993250 ) ) ;
#1863 = EDGE_CURVE ( 'NONE', #47273, #12421, #35916, .T. ) ;
#1864 = DIRECTION ( 'NONE',  ( 0.7071067811865447972, 0.000000000000000000, 0.7071067811865502373 ) ) ;
#1865 = ORIENTED_EDGE ( 'NONE', *, *, #14226, .T. ) ;
#1866 = LINE ( 'NONE', #23724, #57215 ) ;
#1867 = FILL_AREA_STYLE ('',( #38215 ) ) ;
#1868 = ADVANCED_FACE ( 'NONE', ( #10223 ), #41222, .F. ) ;
#1869 = CARTESIAN_POINT ( 'NONE',  ( -183.0000000000000000, 0.000000000000000000, 9.524999999999991473 ) ) ;
#1870 = CARTESIAN_POINT ( 'NONE',  ( -183.4429263765338192, -1.166476076187852838E-15, -9.524999999999991473 ) ) ;
#1871 = CARTESIAN_POINT ( 'NONE',  ( -47.24499999999998323, -4.716976649647093289, -6.492361379858945902 ) ) ;
#1872 = CARTESIAN_POINT ( 'NONE',  ( 44.99999999999977263, 147.4999999999999716, 10.00000000000000000 ) ) ;
#1873 = CARTESIAN_POINT ( 'NONE',  ( -102.3570736234661780, 5.598654528085804216, 7.705886871421366635 ) ) ;
#1874 = CARTESIAN_POINT ( 'NONE',  ( -33.89861118948982721, -9.947368421052626530, 2.722470280083843619 ) ) ;
#1875 = CARTESIAN_POINT ( 'NONE',  ( -75.75000000000000000, -0.9999999999999995559, 20.00000000000000000 ) ) ;
#1876 = CARTESIAN_POINT ( 'NONE',  ( -76.25707362346616947, 5.598654528085800663, -7.705886871421367523 ) ) ;
#1877 = CARTESIAN_POINT ( 'NONE',  ( -92.84292637653379643, 9.058813317711329915, -2.943386871421373119 ) ) ;
#1878 = APPLICATION_PROTOCOL_DEFINITION ( 'draft international standard', 'automotive_design', 1998, #29818 ) ;
#1879 = CARTESIAN_POINT ( 'NONE',  ( -163.4070736234664309, 3.094860106614563122, -9.525000000002803446 ) ) ;
#1880 = DIRECTION ( 'NONE',  ( 0.000000000000000000, -0.000000000000000000, -1.000000000000000000 ) ) ;
#1881 = DIRECTION ( 'NONE',  ( 0.000000000000000000, 0.000000000000000000, -1.000000000000000000 ) ) ;
#1882 =( LENGTH_UNIT ( ) NAMED_UNIT ( * ) SI_UNIT ( .MILLI., .METRE. ) );
#1883 = ORIENTED_EDGE ( 'NONE', *, *, #45933, .F. ) ;
#1884 = FACE_OUTER_BOUND ( 'NONE', #26846, .T. ) ;
#1885 = ORIENTED_EDGE ( 'NONE', *, *, #17807, .F. ) ;
#1886 = CARTESIAN_POINT ( 'NONE',  ( -23.21231517720797655, 118.4999999999999716, -7.500000000000000000 ) ) ;
#1887 = CARTESIAN_POINT ( 'NONE',  ( 8.437984349512095861, 120.3070736234661382, 1.550032578732817026E-15 ) ) ;
#1888 = CARTESIAN_POINT ( 'NONE',  ( 20.83091330386927353, 149.9514755777528023, 9.751095921151032186 ) ) ;
#1889 = AXIS2_PLACEMENT_3D ( 'NONE', #49833, #7264, #6904 ) ;
#1890 = ORIENTED_EDGE ( 'NONE', *, *, #42040, .T. ) ;
#1891 = VECTOR ( 'NONE', #60717, 1000.000000000000000 ) ;
#1892 = DIRECTION ( 'NONE',  ( 0.000000000000000000, 0.000000000000000000, -1.000000000000000000 ) ) ;
#1893 = PRESENTATION_STYLE_ASSIGNMENT (( #50170 ) ) ;
#1894 = CARTESIAN_POINT ( 'NONE',  ( 7.632228543268607446, 150.1570736234661751, 2.479861379858954606 ) ) ;
#1895 = PRESENTATION_LAYER_ASSIGNMENT (  '', '', ( #16609 ) ) ;
#1896 =( NAMED_UNIT ( * ) PLANE_ANGLE_UNIT ( ) SI_UNIT ( $, .RADIAN. ) );
#1897 =( NAMED_UNIT ( * ) PLANE_ANGLE_UNIT ( ) SI_UNIT ( $, .RADIAN. ) );
#1898 = CARTESIAN_POINT ( 'NONE',  ( -91.04499999999998749, 7.632228543268600340, 2.479861379858949277 ) ) ;
#1899 = ORIENTED_EDGE ( 'NONE', *, *, #69263, .T. ) ;
#1900 = CARTESIAN_POINT ( 'NONE',  ( 0.000000000000000000, 154.4258142642185305, -9.450814264218562855 ) ) ;
#1901 = CARTESIAN_POINT ( 'NONE',  ( 1.000000000000000000, 43.00000000000000000, -74.38749456993816978 ) ) ;
#1902 = ORIENTED_EDGE ( 'NONE', *, *, #30713, .F. ) ;
#1903 = SURFACE_SIDE_STYLE ('',( #5848 ) ) ;
#1904 = VECTOR ( 'NONE', #13869, 1000.000000000000000 ) ;
#1905 = VECTOR ( 'NONE', #66420, 1000.000000000000000 ) ;
#1906 = FACE_OUTER_BOUND ( 'NONE', #44768, .T. ) ;
#1907 = ORIENTED_EDGE ( 'NONE', *, *, #2071, .T. ) ;
#1909 = ORIENTED_EDGE ( 'NONE', *, *, #66811, .F. ) ;
#1908 = ADVANCED_FACE ( 'NONE', ( #63674 ), #26026, .T. ) ;
#1910 = CYLINDRICAL_SURFACE ( 'NONE', #12487, 5.000000000000000000 ) ;
#1911 = CYLINDRICAL_SURFACE ( 'NONE', #25691, 0.5000000000000004441 ) ;
#1912 = CARTESIAN_POINT ( 'NONE',  ( 13.75000000000000533, 30.99999999999999289, 3.750000000000000000 ) ) ;
#1913 = CARTESIAN_POINT ( 'NONE',  ( -176.9070736234661751, -3.094860106618429807, 9.524999999999991473 ) ) ;
#1914 = B_SPLINE_CURVE_WITH_KNOTS ( 'NONE', 3,
 ( #36287, #52107, #26018, #25672, #3859, #53132, #47552, #25341 ),
 .UNSPECIFIED., .F., .F.,
 ( 4, 2, 2, 4 ),
 ( 2.544316211732959925E-07, 0.002094919859796807744, 0.003142252573884623743, 0.004189585287972440175 ),
 .UNSPECIFIED. ) ;
#1915 = LINE ( 'NONE', #39647, #67942 ) ;
#1916 = EDGE_CURVE ( 'NONE', #24423, #11684, #20782, .T. ) ;
#1917 = CARTESIAN_POINT ( 'NONE',  ( -117.2070736234661723, 3.094860106618433360, 9.524999999999991473 ) ) ;
#1918 =( REPRESENTATION_RELATIONSHIP ('NONE','NONE', #5102, #12274 ) REPRESENTATION_RELATIONSHIP_WITH_TRANSFORMATION ( #10002 )SHAPE_REPRESENTATION_RELATIONSHIP( ) );
#1919 = CARTESIAN_POINT ( 'NONE',  ( -34.99999999999992895, 112.9999999999999858, 7.000000000000000000 ) ) ;
#1920 = ORIENTED_EDGE ( 'NONE', *, *, #55164, .T. ) ;
#1921 = CARTESIAN_POINT ( 'NONE',  ( -30.38025804287905629, -8.499999999999996447, 8.000000000000000000 ) ) ;
#1922 =( NAMED_UNIT ( * ) PLANE_ANGLE_UNIT ( ) SI_UNIT ( $, .RADIAN. ) );
#1923 = ORIENTED_EDGE ( 'NONE', *, *, #7630, .F. ) ;
#1924 = CARTESIAN_POINT ( 'NONE',  ( -159.0550000000000068, -9.827790563157499189E-16, -8.024999999999991473 ) ) ;
#1925 = CARTESIAN_POINT ( 'NONE',  ( -40.99999999999997868, 9.999999999999978684, -3.000000000000000444 ) ) ;
#1926 = CARTESIAN_POINT ( 'NONE',  ( -162.2949999999999875, -2.607480562269069768, 8.024999999999991473 ) ) ;
#1927 = EDGE_CURVE ( 'NONE', #35855, #21095, #41033, .T. ) ;
#1928 = CARTESIAN_POINT ( 'NONE',  ( -162.4449999999999932, 0.000000000000000000, 8.024999999999991473 ) ) ;
#1929 = EDGE_LOOP ( 'NONE', ( #2352, #3010, #34974, #11079 ) ) ;
#1930 = DIRECTION ( 'NONE',  ( 0.000000000000000000, 1.000000000000000000, 0.000000000000000000 ) ) ;
#1931 = DIRECTION ( 'NONE',  ( -0.000000000000000000, -0.000000000000000000, -1.000000000000000000 ) ) ;
#1932 = STYLED_ITEM ( 'NONE', ( #2654 ), #67274 ) ;
#1933 = EDGE_CURVE ( 'NONE', #67575, #60632, #52084, .T. ) ;
#1934 = LINE ( 'NONE', #19568, #57474 ) ;
#1935 = CARTESIAN_POINT ( 'NONE',  ( -74.75499999999998124, 4.716976649647091513, -6.492361379858946790 ) ) ;
#1936 = CARTESIAN_POINT ( 'NONE',  ( -37.05138327197616377, -10.73391388307777916, 3.833378626313314275 ) ) ;
#1937 = CARTESIAN_POINT ( 'NONE',  ( -23.71231517720798010, 113.4999999999999858, -7.500000000000000000 ) ) ;
#1938 = VECTOR ( 'NONE', #22305, 1000.000000000000000 ) ;
#1939 = CARTESIAN_POINT ( 'NONE',  ( -74.09499999999998465, -2.607480562269071545, -8.024999999999991473 ) ) ;
#1940 = CARTESIAN_POINT ( 'NONE',  ( -9.058813317711338797, 147.4550000000000125, 2.943386871421373563 ) ) ;
#1941 =( GEOMETRIC_REPRESENTATION_CONTEXT ( 3 ) GLOBAL_UNCERTAINTY_ASSIGNED_CONTEXT ( ( #64365 ) ) GLOBAL_UNIT_ASSIGNED_CONTEXT ( ( #6172, #65257, #12473 ) ) REPRESENTATION_CONTEXT ( 'NONE', 'WORKASPACE' ) );
#1942 = SURFACE_STYLE_USAGE ( .BOTH. , #50220 ) ;
#1943 = CARTESIAN_POINT ( 'NONE',  ( 0.2500000000000000000, 36.74999999999999289, -3.000000000000000000 ) ) ;
#1944 = SURFACE_SIDE_STYLE ('',( #33344 ) ) ;
#1945 = FACE_OUTER_BOUND ( 'NONE', #16092, .T. ) ;
#1946 =( GEOMETRIC_REPRESENTATION_CONTEXT ( 3 ) GLOBAL_UNCERTAINTY_ASSIGNED_CONTEXT ( ( #29065 ) ) GLOBAL_UNIT_ASSIGNED_CONTEXT ( ( #28549, #6078, #22259 ) ) REPRESENTATION_CONTEXT ( 'NONE', 'WORKASPACE' ) );
#1947 = DIRECTION ( 'NONE',  ( -0.9704308468600219006, 0.2413793103448194366, -0.000000000000000000 ) ) ;
#1948 = SURFACE_SIDE_STYLE ('',( #6585 ) ) ;
#1949 = DIRECTION ( 'NONE',  ( -1.274184670190250597E-16, 1.000000000000000000, 2.430666987508112707E-16 ) ) ;
#1950 = ORIENTED_EDGE ( 'NONE', *, *, #18817, .T. ) ;
#1951 = ORIENTED_EDGE ( 'NONE', *, *, #22847, .T. ) ;
#1952 = CARTESIAN_POINT ( 'NONE',  ( -60.65707362346617515, 9.058813317711329915, 2.943386871421369566 ) ) ;
#1953 = DIRECTION ( 'NONE',  ( -1.000000000000000000, 0.000000000000000000, -0.000000000000000000 ) ) ;
#1954 = EDGE_CURVE ( 'NONE', #68674, #68077, #15517, .T. ) ;
#1955 = CARTESIAN_POINT ( 'NONE',  ( -45.00000000000000000, 9.119539144243722362, 6.744166081069411511 ) ) ;
#1956 = LINE ( 'NONE', #44982, #13535 ) ;
#1957 = SURFACE_STYLE_FILL_AREA ( #50236 ) ;
#1958 = FILL_AREA_STYLE_COLOUR ( '', #16169 ) ;
#1959 = ORIENTED_EDGE ( 'NONE', *, *, #16549, .F. ) ;
#1960 = CARTESIAN_POINT ( 'NONE',  ( -100.4050000000000011, -2.607480562269069768, 8.024999999999991473 ) ) ;
#1961 = EDGE_LOOP ( 'NONE', ( #38716, #66795 ) ) ;
#1962 = CARTESIAN_POINT ( 'NONE',  ( 6.123233995736766282E-16, 0.000000000000000000, 5.000000000000000000 ) ) ;
#1963 = ORIENTED_EDGE ( 'NONE', *, *, #43566, .F. ) ;
#1964 = CARTESIAN_POINT ( 'NONE',  ( -10.01517768586949231, 111.3049999999999784, -6.132527647946036459E-16 ) ) ;
#1965 = DIRECTION ( 'NONE',  ( 1.000000000000000000, 0.000000000000000000, 0.000000000000000000 ) ) ;
#1966 = ORIENTED_EDGE ( 'NONE', *, *, #12053, .T. ) ;
#1967 = COLOUR_RGB ( '', 0.72549020, 0.75294118, 0.79215686) ;
#1968 = ORIENTED_EDGE ( 'NONE', *, *, #20890, .F. ) ;
#1969 = ORIENTED_EDGE ( 'NONE', *, *, #13332, .T. ) ;
#1970 = CARTESIAN_POINT ( 'NONE',  ( 12.75000000000000533, 27.99999999999998224, 4.000000000000000000 ) ) ;
#1971 =( NAMED_UNIT ( * ) PLANE_ANGLE_UNIT ( ) SI_UNIT ( $, .RADIAN. ) );
#1972 = CARTESIAN_POINT ( 'NONE',  ( -10.67562708368618551, -11.73435252745061774, -2.515260829213044058 ) ) ;
#1973 = CARTESIAN_POINT ( 'NONE',  ( -150.4429263765338192, -1.166476076187852838E-15, -9.524999999999991473 ) ) ;
#1974 = ORIENTED_EDGE ( 'NONE', *, *, #20335, .T. ) ;
#1975 = CARTESIAN_POINT ( 'NONE',  ( 7.632228543268608334, 131.3429263765338249, -2.479861379858951942 ) ) ;
#1976 = DIRECTION ( 'NONE',  ( 0.000000000000000000, 0.000000000000000000, 1.000000000000000000 ) ) ;
#1977 = SURFACE_STYLE_USAGE ( .BOTH. , #11922 ) ;
#1978 = MECHANICAL_DESIGN_GEOMETRIC_PRESENTATION_REPRESENTATION (  '', ( #28996 ), #50373 ) ;
#1979 = CIRCLE ( 'NONE', #8851, 1.000000000000000000 ) ;
#1980 = EDGE_CURVE ( 'NONE', #66411, #2325, #36526, .T. ) ;
#1981 = DIRECTION ( 'NONE',  ( 1.000000000000000000, 0.000000000000000000, 0.000000000000000000 ) ) ;
#1982 = FACE_OUTER_BOUND ( 'NONE', #67167, .T. ) ;
#1983 = EDGE_CURVE ( 'NONE', #60509, #45120, #1915, .T. ) ;
#1984 = ORIENTED_EDGE ( 'NONE', *, *, #37757, .F. ) ;
#1985 = ORIENTED_EDGE ( 'NONE', *, *, #53832, .T. ) ;
#1986 = DIRECTION ( 'NONE',  ( 1.000000000000000000, 7.703719777548942317E-32, 0.000000000000000000 ) ) ;
#1987 = CYLINDRICAL_SURFACE ( 'NONE', #47041, 1.000000000000000888 ) ;
#1988 = FILL_AREA_STYLE_COLOUR ( '', #62186 ) ;
#1989 = CARTESIAN_POINT ( 'NONE',  ( -135.0549999999999784, -9.827790563157499189E-16, -8.024999999999991473 ) ) ;
#1990 = FACE_OUTER_BOUND ( 'NONE', #59284, .T. ) ;
#1991 = SURFACE_SIDE_STYLE ('',( #17253 ) ) ;
#1992 = ORIENTED_EDGE ( 'NONE', *, *, #46091, .T. ) ;
#1993 = ADVANCED_FACE ( 'NONE', ( #15861 ), #23429, .F. ) ;
#1994 = CARTESIAN_POINT ( 'NONE',  ( -41.49999999999998579, 106.9282032302754999, 4.000000000000000000 ) ) ;
#1995 = CARTESIAN_POINT ( 'NONE',  ( 14.98999599679679662, 146.4999999999999716, 10.00000000000000000 ) ) ;
#1996 = DIRECTION ( 'NONE',  ( 1.000000000000000000, -0.000000000000000000, -1.300977106640434891E-16 ) ) ;
#1997 = ORIENTED_EDGE ( 'NONE', *, *, #11606, .T. ) ;
#1998 = VECTOR ( 'NONE', #11601, 1000.000000000000000 ) ;
#1999 = ORIENTED_EDGE ( 'NONE', *, *, #67741, .T. ) ;
#2000 = CYLINDRICAL_SURFACE ( 'NONE', #13705, 0.5000000000000004441 ) ;
#2001 = CARTESIAN_POINT ( 'NONE',  ( -30.38025804288019671, -8.499999999999996447, 0.06931351858043485747 ) ) ;
#2002 = CARTESIAN_POINT ( 'NONE',  ( -50.00499999999998835, 6.826472737025116366, 4.959722759717898555 ) ) ;
#2003 = ORIENTED_EDGE ( 'NONE', *, *, #7167, .T. ) ;
#2004 = CYLINDRICAL_SURFACE ( 'NONE', #18014, 5.000000000000000000 ) ;
#2005 = FACE_OUTER_BOUND ( 'NONE', #25769, .T. ) ;
#2006 = FILL_AREA_STYLE ('',( #54156 ) ) ;
#2007 = CARTESIAN_POINT ( 'NONE',  ( 4.041451884327376121, 7.000000000000007105, 1.082903768654759569 ) ) ;
#2008 = EDGE_CURVE ( 'NONE', #25443, #68774, #23034, .T. ) ;
#2009 = CARTESIAN_POINT ( 'NONE',  ( -182.0949999999999989, -2.607480562269071545, -8.024999999999991473 ) ) ;
#2010 = ORIENTED_EDGE ( 'NONE', *, *, #18790, .F. ) ;
#2011 = CARTESIAN_POINT ( 'NONE',  ( 33.00000000000000000, 15.00000000000000000, -79.00402776293826435 ) ) ;
#2012 = ADVANCED_FACE ( 'NONE', ( #59088 ), #33132, .T. ) ;
#2013 = CARTESIAN_POINT ( 'NONE',  ( -57.66974776420195781, -8.499999999999992895, 0.3730306325211200646 ) ) ;
#2014 = DIRECTION ( 'NONE',  ( -0.000000000000000000, -1.000000000000000000, 0.000000000000000000 ) ) ;
#2015 = CARTESIAN_POINT ( 'NONE',  ( 20.94636006565341191, 149.9999999999999716, 9.500000000000000000 ) ) ;
#2016 = AXIS2_PLACEMENT_3D ( 'NONE', #63589, #36894, #58653 ) ;
#2017 = CARTESIAN_POINT ( 'NONE',  ( -98.39499999999999602, -6.826472737025113702, -4.959722759717900331 ) ) ;
#2018 = CARTESIAN_POINT ( 'NONE',  ( 8.102448949553181734, 115.5049999999999812, 5.886773742842750679 ) ) ;
#2019 = CARTESIAN_POINT ( 'NONE',  ( -79.64499999999999602, 4.716976649647091513, -6.492361379858946790 ) ) ;
#2020 = CARTESIAN_POINT ( 'NONE',  ( 17.25000000000000711, 24.74999999999997868, -4.000000000000000000 ) ) ;
#2021 = VECTOR ( 'NONE', #11905, 1000.000000000000000 ) ;
#2022 = DIRECTION ( 'NONE',  ( -0.7071067811865426878, 0.000000000000000000, 0.7071067811865524577 ) ) ;
#2023 = DIRECTION ( 'NONE',  ( -1.000000000000000000, -0.000000000000000000, -0.000000000000000000 ) ) ;
#2024 = AXIS2_PLACEMENT_3D ( 'NONE', #3398, #36883, #47459 ) ;
#2025 = LINE ( 'NONE', #39780, #3909 ) ;
#2026 = ORIENTED_EDGE ( 'NONE', *, *, #15373, .T. ) ;
#2027 = CARTESIAN_POINT ( 'NONE',  ( -113.0929263765338106, 3.094860106618433360, 9.524999999999991473 ) ) ;
#2028 =( BOUNDED_CURVE ( )  B_SPLINE_CURVE ( 2, ( #895, #32636, #47235, #55123, #65351, #44297, #33003, #16846, #48526, #64672, #11535 ),
 .UNSPECIFIED., .F., .F. ) 
 B_SPLINE_CURVE_WITH_KNOTS ( ( 3, 2, 2, 2, 2, 3 ),
 ( 0.9673913043478260532, 0.9695652173913043015, 0.9717391304347826608, 0.9739130434782609091, 0.9760869565217391575, 0.9782608695652174058 ),
 .UNSPECIFIED. ) 
 CURVE ( )  GEOMETRIC_REPRESENTATION_ITEM ( )  RATIONAL_B_SPLINE_CURVE ( ( 1.000000000000000000, 0.9510565162951535312, 1.000000000000000000, 0.9510565162951535312, 1.000000000000000000, 0.9510565162951535312, 1.000000000000000000, 0.9510565162951535312, 1.000000000000000000, 0.9510565162951535312, 1.000000000000000000 ) ) 
 REPRESENTATION_ITEM ( '' )  );
#2029 = CARTESIAN_POINT ( 'NONE',  ( -139.7950000000000159, 2.607480562269068880, -8.024999999999993250 ) ) ;
#2030 = CARTESIAN_POINT ( 'NONE',  ( 22.99999999999998224, 5.000000000000000000, 72.00402776293825013 ) ) ;
#2031 = AXIS2_PLACEMENT_3D ( 'NONE', #59980, #64904, #28284 ) ;
#2032 = AXIS2_PLACEMENT_3D ( 'NONE', #2468, #7114, #12725 ) ;
#2033 = SURFACE_SIDE_STYLE ('',( #51696 ) ) ;
#2034 = SURFACE_STYLE_USAGE ( .BOTH. , #28831 ) ;
#2035 = CARTESIAN_POINT ( 'NONE',  ( -173.0929263765339670, 3.094860106620836326, 9.524999999998247091 ) ) ;
#2036 = ORIENTED_EDGE ( 'NONE', *, *, #45415, .F. ) ;
#2037 = AXIS2_PLACEMENT_3D ( 'NONE', #5373, #11359, #16676 ) ;
#2038 = ORIENTED_EDGE ( 'NONE', *, *, #18513, .F. ) ;
#2039 = DIRECTION ( 'NONE',  ( -0.000000000000000000, -0.000000000000000000, 1.000000000000000000 ) ) ;
#2040 = SURFACE_SIDE_STYLE ('',( #30561 ) ) ;
#2041 = EDGE_CURVE ( 'NONE', #69341, #849, #65697, .T. ) ;
#2042 = CYLINDRICAL_SURFACE ( 'NONE', #45127, 26.99999999999999645 ) ;
#2043 = AXIS2_PLACEMENT_3D ( 'NONE', #5876, #47475, #15779 ) ;
#2044 = CARTESIAN_POINT ( 'NONE',  ( 34.99999999999999289, 99.99999999999998579, 9.500000000000000000 ) ) ;
#2045 = CARTESIAN_POINT ( 'NONE',  ( -12.72792206135785698, 114.9999999999999574, -10.50000000000000000 ) ) ;
#2046 = EDGE_LOOP ( 'NONE', ( #10391, #5930, #64883, #11389 ) ) ;
#2047 = CARTESIAN_POINT ( 'NONE',  ( -135.9549999999999841, -7.632228543268599452, 2.479861379858951054 ) ) ;
#2048 = VERTEX_POINT ( 'NONE', #54736 ) ;
#2049 = EDGE_LOOP ( 'NONE', ( #54857, #54987, #54703, #56535 ) ) ;
#2050 =( NAMED_UNIT ( * ) PLANE_ANGLE_UNIT ( ) SI_UNIT ( $, .RADIAN. ) );
#2051 = SPHERICAL_SURFACE ( 'NONE', #28727, 0.5000000000000000000 ) ;
#2052 = VERTEX_POINT ( 'NONE', #11845 ) ;
#2053 = LINE ( 'NONE', #55942, #12463 ) ;
#2054 = CARTESIAN_POINT ( 'NONE',  ( -74.99999999999998579, 50.00000000000000000, 11.50000000000000000 ) ) ;
#2055 =( BOUNDED_CURVE ( )  B_SPLINE_CURVE ( 2, ( #5695, #21907, #48678, #43419, #6061 ),
 .UNSPECIFIED., .F., .F. ) 
 B_SPLINE_CURVE_WITH_KNOTS ( ( 3, 2, 3 ),
 ( 0.02072354678354213983, 0.02352941176470589243, 0.02941176470588238029 ),
 .UNSPECIFIED. ) 
 CURVE ( )  GEOMETRIC_REPRESENTATION_ITEM ( )  RATIONAL_B_SPLINE_CURVE ( ( 0.9755800536518703936, 0.9766541028127901924, 1.000000000000000000, 0.9510565162951533091, 1.000000000000000222 ) ) 
 REPRESENTATION_ITEM ( '' )  );
#2056 = CARTESIAN_POINT ( 'NONE',  ( 9.058813317711338797, 141.8449999999999989, -2.943386871421372675 ) ) ;
#2057 = DIRECTION ( 'NONE',  ( 0.000000000000000000, 0.000000000000000000, -1.000000000000000000 ) ) ;
#2058 = ORIENTED_EDGE ( 'NONE', *, *, #41906, .T. ) ;
#2059 = EDGE_CURVE ( 'NONE', #65559, #65056, #25221, .T. ) ;
#2060 = SURFACE_SIDE_STYLE ('',( #3114 ) ) ;
#2061 = CARTESIAN_POINT ( 'NONE',  ( 3.094860106618435136, 143.4050000000000011, -9.525000000000000355 ) ) ;
#2062 = CARTESIAN_POINT ( 'NONE',  ( -58.55499999999999261, 0.000000000000000000, 8.024999999999991473 ) ) ;
#2063 = FILL_AREA_STYLE ('',( #29197 ) ) ;
#2064 = ORIENTED_EDGE ( 'NONE', *, *, #14220, .T. ) ;
#2065 = CARTESIAN_POINT ( 'NONE',  ( 9.058813317711338797, 157.9549999999999841, -2.943386871421372675 ) ) ;
#2066 = LINE ( 'NONE', #55253, #51346 ) ;
#2067 = VECTOR ( 'NONE', #61071, 1000.000000000000000 ) ;
#2068 = ADVANCED_FACE ( 'NONE', ( #44939 ), #69638, .T. ) ;
#2069 = SURFACE_STYLE_FILL_AREA ( #2798 ) ;
#2070 = DIRECTION ( 'NONE',  ( 0.000000000000000000, 0.000000000000000000, 1.000000000000000000 ) ) ;
#2071 = EDGE_CURVE ( 'NONE', #6097, #12107, #64557, .T. ) ;
#2072 = VERTEX_POINT ( 'NONE', #6913 ) ;
#2073 = VECTOR ( 'NONE', #55391, 1000.000000000000000 ) ;
#2074 = PRESENTATION_STYLE_ASSIGNMENT (( #39474 ) ) ;
#2075 = ORIENTED_EDGE ( 'NONE', *, *, #11594, .T. ) ;
#2076 = FILL_AREA_STYLE_COLOUR ( '', #30282 ) ;
#2077 = TOROIDAL_SURFACE ( 'NONE', #23529, 13.49999999999999822, 0.5000000000000000000 ) ;
#2078 = CARTESIAN_POINT ( 'NONE',  ( 0.000000000000000000, 87.30187232391182306, 0.000000000000000000 ) ) ;
#2079 = CARTESIAN_POINT ( 'NONE',  ( -47.88739147232087134, -11.66012019292491608, 3.348867242218062312 ) ) ;
#2080 = CARTESIAN_POINT ( 'NONE',  ( -164.1550000000000011, 7.632228543268600340, 2.479861379858949277 ) ) ;
#2081 = ORIENTED_EDGE ( 'NONE', *, *, #41810, .T. ) ;
#2082 = FILL_AREA_STYLE ('',( #1413 ) ) ;
#2083 = AXIS2_PLACEMENT_3D ( 'NONE', #26863, #31824, #52958 ) ;
#2084 = ADVANCED_FACE ( 'NONE', ( #39306 ), #61184, .T. ) ;
#2085 = CYLINDRICAL_SURFACE ( 'NONE', #54345, 0.5000000000000004441 ) ;
#2086 = FILL_AREA_STYLE_COLOUR ( '', #60184 ) ;
#2087 = ORIENTED_EDGE ( 'NONE', *, *, #1211, .F. ) ;
#2088 = AXIS2_PLACEMENT_3D ( 'NONE', #37026, #10260, #26413 ) ;
#2090 = EDGE_CURVE ( 'NONE', #9321, #29580, #50189, .T. ) ;
#2089 = VERTEX_POINT ( 'NONE', #12173 ) ;
#2091 = LINE ( 'NONE', #62625, #46288 ) ;
#2092 = DIRECTION ( 'NONE',  ( -0.000000000000000000, -0.000000000000000000, -1.000000000000000000 ) ) ;
#2093 = CARTESIAN_POINT ( 'NONE',  ( -74.60500000000000398, 6.826472737025113702, -4.959722759717902107 ) ) ;
#2094 = EDGE_LOOP ( 'NONE', ( #31610, #22040, #48479, #53765, #19223, #15545, #17600, #48450 ) ) ;
#2095 = FILL_AREA_STYLE_COLOUR ( '', #56441 ) ;
#2096 = STYLED_ITEM ( 'NONE', ( #50046 ), #15066 ) ;
#2097 = CARTESIAN_POINT ( 'NONE',  ( 71.49999999999998579, 64.07124727947029896, -7.000000000000000000 ) ) ;
#2098 = FACE_OUTER_BOUND ( 'NONE', #34418, .T. ) ;
#2099 = MECHANICAL_DESIGN_GEOMETRIC_PRESENTATION_REPRESENTATION (  '', ( #61642 ), #29054 ) ;
#2100 = ORIENTED_EDGE ( 'NONE', *, *, #3711, .T. ) ;
#2101 = DIRECTION ( 'NONE',  ( 1.000000000000000000, 0.000000000000000000, -0.000000000000000000 ) ) ;
#2102 = VECTOR ( 'NONE', #54339, 1000.000000000000000 ) ;
#2104 =( NAMED_UNIT ( * ) PLANE_ANGLE_UNIT ( ) SI_UNIT ( $, .RADIAN. ) );
#2103 = DIRECTION ( 'NONE',  ( 1.000000000000000000, 7.709882115452468306E-16, -0.000000000000000000 ) ) ;
#2105 = CARTESIAN_POINT ( 'NONE',  ( 5.598654528085809545, 139.1449999999999818, -7.705886871421373741 ) ) ;
#2106 = CARTESIAN_POINT ( 'NONE',  ( -106.9449999999999790, -9.827790563157499189E-16, -8.024999999999991473 ) ) ;
#2107 = EDGE_CURVE ( 'NONE', #53683, #49361, #28699, .T. ) ;
#2109 = SURFACE_SIDE_STYLE ('',( #7802 ) ) ;
#2108 = CARTESIAN_POINT ( 'NONE',  ( 0.000000000000000000, 33.74999999999999289, 3.750000000000000000 ) ) ;
#2110 = CARTESIAN_POINT ( 'NONE',  ( -151.6429263765338078, -5.598654528085801552, 7.705886871421367523 ) ) ;
#2111 =( NAMED_UNIT ( * ) SI_UNIT ( $, .STERADIAN. ) SOLID_ANGLE_UNIT ( ) );
#2112 = CARTESIAN_POINT ( 'NONE',  ( -163.7950000000000159, 2.607480562269068880, -8.024999999999993250 ) ) ;
#2113 = VECTOR ( 'NONE', #3338, 1000.000000000000000 ) ;
#2114 = AXIS2_PLACEMENT_3D ( 'NONE', #67440, #45345, #41100 ) ;
#2115 = ORIENTED_EDGE ( 'NONE', *, *, #27930, .F. ) ;
#2116 = CARTESIAN_POINT ( 'NONE',  ( -6.826472737025120807, 129.3929263765338362, -4.959722759717907437 ) ) ;
#2117 = EDGE_LOOP ( 'NONE', ( #67842, #36360, #14328 ) ) ;
#2118 = CARTESIAN_POINT ( 'NONE',  ( -67.04292637653381348, -9.058813317711329915, -2.943386871421370898 ) ) ;
#2119 =( GEOMETRIC_REPRESENTATION_CONTEXT ( 3 ) GLOBAL_UNCERTAINTY_ASSIGNED_CONTEXT ( ( #18680 ) ) GLOBAL_UNIT_ASSIGNED_CONTEXT ( ( #52584, #42061, #3275 ) ) REPRESENTATION_CONTEXT ( 'NONE', 'WORKASPACE' ) );
#2120 = AXIS2_PLACEMENT_3D ( 'NONE', #24384, #41302, #36009 ) ;
#2121 = CARTESIAN_POINT ( 'NONE',  ( 0.000000000000000000, 110.4999999999999858, -9.525000000000000355 ) ) ;
#2122 = CARTESIAN_POINT ( 'NONE',  ( -142.9429263765337907, 0.000000000000000000, 9.524999999999991473 ) ) ;
#2123 = DIRECTION ( 'NONE',  ( -0.07898106964430649801, -0.9968761159932768567, -1.346643164337371088E-16 ) ) ;
#2124 = AXIS2_PLACEMENT_3D ( 'NONE', #34381, #27684, #22795 ) ;
#2125 = EDGE_LOOP ( 'NONE', ( #16141, #49060, #3649, #28198 ) ) ;
#2126 = CARTESIAN_POINT ( 'NONE',  ( -167.9050000000000011, 2.607480562269069324, -8.024999999999993250 ) ) ;
#2127 = ORIENTED_EDGE ( 'NONE', *, *, #52281, .T. ) ;
#2128 = FACE_OUTER_BOUND ( 'NONE', #19966, .T. ) ;
#2130 = EDGE_CURVE ( 'NONE', #64410, #66883, #18163, .T. ) ;
#2129 = DIRECTION ( 'NONE',  ( 0.000000000000000000, 0.000000000000000000, -1.000000000000000000 ) ) ;
#2131 =( GEOMETRIC_REPRESENTATION_CONTEXT ( 3 ) GLOBAL_UNCERTAINTY_ASSIGNED_CONTEXT ( ( #275 ) ) GLOBAL_UNIT_ASSIGNED_CONTEXT ( ( #13075, #2104, #12726 ) ) REPRESENTATION_CONTEXT ( 'NONE', 'WORKASPACE' ) );
#2132 = DIRECTION ( 'NONE',  ( 0.000000000000000000, 1.000000000000000000, -0.000000000000000000 ) ) ;
#2133 = CARTESIAN_POINT ( 'NONE',  ( 6.826472737025121695, 156.6070736234661638, -4.959722759717905660 ) ) ;
#2134 =( GEOMETRIC_REPRESENTATION_CONTEXT ( 3 ) GLOBAL_UNCERTAINTY_ASSIGNED_CONTEXT ( ( #22848 ) ) GLOBAL_UNIT_ASSIGNED_CONTEXT ( ( #12733, #39868, #7123 ) ) REPRESENTATION_CONTEXT ( 'NONE', 'WORKASPACE' ) );
#2135 = ORIENTED_EDGE ( 'NONE', *, *, #40737, .F. ) ;
#2136 = ADVANCED_FACE ( 'NONE', ( #45963 ), #8321, .F. ) ;
#2137 = CARTESIAN_POINT ( 'NONE',  ( -3.000000000000000000, -3.499999999999999556, 0.000000000000000000 ) ) ;
#2138 = CARTESIAN_POINT ( 'NONE',  ( 10.01517768586949408, 115.8049999999999784, 1.839758294383810543E-15 ) ) ;
#2139 = CARTESIAN_POINT ( 'NONE',  ( -84.35499999999998977, -4.716976649647093289, -6.492361379858945902 ) ) ;
#2140 = SURFACE_STYLE_USAGE ( .BOTH. , #7499 ) ;
#2141 = CARTESIAN_POINT ( 'NONE',  ( 3.094860106618431583, 130.2049999999999841, 9.525000000000000355 ) ) ;
#2142 = CIRCLE ( 'NONE', #15753, 0.5000000000000004441 ) ;
#2143 = FILL_AREA_STYLE_COLOUR ( '', #18399 ) ;
#2144 = EDGE_CURVE ( 'NONE', #3091, #11136, #51224, .T. ) ;
#2145 = CARTESIAN_POINT ( 'NONE',  ( 20.35445791815277161, 114.9981483343694748, 10.00000000000000000 ) ) ;
#2146 = DIRECTION ( 'NONE',  ( 0.000000000000000000, 0.000000000000000000, 1.000000000000000000 ) ) ;
#2147 = FACE_OUTER_BOUND ( 'NONE', #2966, .T. ) ;
#2148 = CARTESIAN_POINT ( 'NONE',  ( -112.7070736234670392, -3.094860106632951524, -9.524999999989441690 ) ) ;
#2149 = EDGE_LOOP ( 'NONE', ( #32277, #8973, #40586, #52611 ) ) ;
#2150 = DIRECTION ( 'NONE',  ( -0.000000000000000000, -0.000000000000000000, -1.000000000000000000 ) ) ;
#2152 = CARTESIAN_POINT ( 'NONE',  ( -50.09499999999996334, -2.607480562269071545, -8.024999999999991473 ) ) ;
#2151 = CIRCLE ( 'NONE', #56147, 0.5000000000000006661 ) ;
#2153 = ORIENTED_EDGE ( 'NONE', *, *, #63854, .F. ) ;
#2154 =( NAMED_UNIT ( * ) SI_UNIT ( $, .STERADIAN. ) SOLID_ANGLE_UNIT ( ) );
#2155 =( BOUNDED_CURVE ( )  B_SPLINE_CURVE ( 2, ( #60281, #50426, #37227, #18067, #55347, #38871, #58639, #10464, #7170, #39552, #6804 ),
 .UNSPECIFIED., .F., .F. ) 
 B_SPLINE_CURVE_WITH_KNOTS ( ( 3, 2, 2, 2, 2, 3 ),
 ( 0.3043478260869494356, 0.3065217391304276284, 0.3086956521739058212, 0.3108695652173840696, 0.3130434782608623179, 0.3152173913043405107 ),
 .UNSPECIFIED. ) 
 CURVE ( )  GEOMETRIC_REPRESENTATION_ITEM ( )  RATIONAL_B_SPLINE_CURVE ( ( 1.000000000000159872, 0.9510565162949935480, 1.000000000000000000, 0.9510565162951535312, 1.000000000000000000, 0.9510565162951535312, 1.000000000000000000, 0.9510565162951535312, 1.000000000000000000, 0.9510565162953185103, 0.9999999999998350209 ) ) 
 REPRESENTATION_ITEM ( '' )  );
#2156 = DIRECTION ( 'NONE',  ( 0.000000000000000000, 1.000000000000000000, 0.000000000000000000 ) ) ;
#2157 = CARTESIAN_POINT ( 'NONE',  ( 22.99999999999996447, 5.000000000000000000, -29.00402776293825369 ) ) ;
#2158 = CONICAL_SURFACE ( 'NONE', #40418, 4.000000000000000000, 0.7853981633974482790 ) ;
#2159 = DIRECTION ( 'NONE',  ( -1.000000000000000000, 0.000000000000000000, 0.000000000000000000 ) ) ;
#2160 = VERTEX_POINT ( 'NONE', #62102 ) ;
#2161 = CARTESIAN_POINT ( 'NONE',  ( -50.15331471893564697, -12.46732336030118482, 2.905981105417522858 ) ) ;
#2162 = CARTESIAN_POINT ( 'NONE',  ( -56.09499999999997044, -2.607480562269071545, -8.024999999999991473 ) ) ;
#2163 = ORIENTED_EDGE ( 'NONE', *, *, #27689, .T. ) ;
#2164 = EDGE_CURVE ( 'NONE', #42390, #22827, #66432, .T. ) ;
#2165 = CARTESIAN_POINT ( 'NONE',  ( -74.15772097241708138, 9.150846973920840455, 6.292314909082026730 ) ) ;
#2166 = CARTESIAN_POINT ( 'NONE',  ( -104.1549999999999869, 7.632228543268600340, 2.479861379858949277 ) ) ;
#2167 = EDGE_LOOP ( 'NONE', ( #50739, #59302, #68092, #56929, #49728 ) ) ;
#2168 = DIRECTION ( 'NONE',  ( 0.000000000000000000, 0.000000000000000000, -1.000000000000000000 ) ) ;
#2169 = AXIS2_PLACEMENT_3D ( 'NONE', #7764, #24622, #8816 ) ;
#2170 = LINE ( 'NONE', #6824, #63953 ) ;
#2171 = FACE_OUTER_BOUND ( 'NONE', #43803, .T. ) ;
#2172 = CONICAL_SURFACE ( 'NONE', #41544, 9.000000000000000000, 0.7853981633974500554 ) ;
#2173 = CARTESIAN_POINT ( 'NONE',  ( -154.7070736234661297, -3.094860106618431139, -9.524999999999991473 ) ) ;
#2174 = VECTOR ( 'NONE', #51707, 1000.000000000000000 ) ;
#2175 = DIRECTION ( 'NONE',  ( 0.000000000000000000, 0.000000000000000000, 1.000000000000000000 ) ) ;
#2176 = CARTESIAN_POINT ( 'NONE',  ( -1.166476076187854022E-15, 146.9449999999999932, 9.525000000000000355 ) ) ;
#2177 = CARTESIAN_POINT ( 'NONE',  ( -82.85707362346616378, -5.598654528085803328, -7.705886871421366635 ) ) ;
#2178 = COLOUR_RGB ( '', 0.08235294, 0.09019608, 0.10196078) ;
#2179 = CARTESIAN_POINT ( 'NONE',  ( -71.49999999999998579, 50.00000000000000000, 7.500000000000000000 ) ) ;
#2180 = EDGE_LOOP ( 'NONE', ( #39281, #38695, #64548, #13878, #24453 ) ) ;
#2181 = CIRCLE ( 'NONE', #42785, 1.000000000000000888 ) ;
#2182 = SURFACE_STYLE_FILL_AREA ( #38901 ) ;
#2184 = CARTESIAN_POINT ( 'NONE',  ( -24.21231517720798010, 113.4999999999999858, -9.500000000000000000 ) ) ;
#2183 = PRESENTATION_STYLE_ASSIGNMENT (( #50454 ) ) ;
#2185 = CARTESIAN_POINT ( 'NONE',  ( -134.0049999999999955, 6.826472737025116366, 4.959722759717898555 ) ) ;
#2186 = CARTESIAN_POINT ( 'NONE',  ( -164.0929263765340806, 3.094860106622937312, 9.524999999996721201 ) ) ;
#2187 = FACE_OUTER_BOUND ( 'NONE', #39719, .T. ) ;
#2188 = CARTESIAN_POINT ( 'NONE',  ( -3.094860106618434248, 113.7950000000000017, 9.525000000000000355 ) ) ;
#2189 = CARTESIAN_POINT ( 'NONE',  ( -134.5449999999999875, -7.632228543268600340, -2.479861379858950166 ) ) ;
#2190 = TOROIDAL_SURFACE ( 'NONE', #42791, 13.50000000000000178, 0.5000000000000000000 ) ;
#2191 = CARTESIAN_POINT ( 'NONE',  ( -128.8449999999999989, -7.632228543268599452, 2.479861379858951054 ) ) ;
#2192 = DIRECTION ( 'NONE',  ( -0.000000000000000000, -0.000000000000000000, -1.000000000000000000 ) ) ;
#2193 = EDGE_CURVE ( 'NONE', #11604, #10038, #2970, .T. ) ;
#2194 = VERTEX_POINT ( 'NONE', #29399 ) ;
#2195 = DIRECTION ( 'NONE',  ( -1.000000000000000000, -0.000000000000000000, -0.000000000000000000 ) ) ;
#2196 =( GEOMETRIC_REPRESENTATION_CONTEXT ( 3 ) GLOBAL_UNCERTAINTY_ASSIGNED_CONTEXT ( ( #57207 ) ) GLOBAL_UNIT_ASSIGNED_CONTEXT ( ( #30997, #57749, #47943 ) ) REPRESENTATION_CONTEXT ( 'NONE', 'WORKASPACE' ) );
#2197 = CARTESIAN_POINT ( 'NONE',  ( -15.98999599679679839, 146.9999999999999716, -7.000000000000000000 ) ) ;
#2198 = SURFACE_STYLE_FILL_AREA ( #39949 ) ;
#2199 = CARTESIAN_POINT ( 'NONE',  ( -177.1429263765338078, 5.598654528085800663, -7.705886871421367523 ) ) ;
#2200 = VECTOR ( 'NONE', #4405, 1000.000000000000000 ) ;
#2201 = CARTESIAN_POINT ( 'NONE',  ( -49.04499999999998039, 7.632228543268600340, 2.479861379858949277 ) ) ;
#2202 = DIRECTION ( 'NONE',  ( 0.000000000000000000, 0.000000000000000000, -1.000000000000000000 ) ) ;
#2203 = DIRECTION ( 'NONE',  ( 0.000000000000000000, 0.000000000000000000, -1.000000000000000000 ) ) ;
#2204 = FACE_OUTER_BOUND ( 'NONE', #25068, .T. ) ;
#2205 = CARTESIAN_POINT ( 'NONE',  ( 21.25000000000001066, 24.74999999999998224, -4.000000000000000000 ) ) ;
#2206 = AXIS2_PLACEMENT_3D ( 'NONE', #42196, #5501, #69549 ) ;
#2207 = CARTESIAN_POINT ( 'NONE',  ( -99.14292637653380780, 5.598654528085800663, -7.705886871421367523 ) ) ;
#2208 = SHAPE_DEFINITION_REPRESENTATION ( #19788, #14558 ) ;
#2209 = PLANE ( 'NONE',  #33470 ) ;
#2210 = DIRECTION ( 'NONE',  ( 0.000000000000000000, 0.000000000000000000, 1.000000000000000000 ) ) ;
#2211 = AXIS2_PLACEMENT_3D ( 'NONE', #39533, #13811, #7830 ) ;
#2212 = SURFACE_STYLE_USAGE ( .BOTH. , #38931 ) ;
#2213 = DIRECTION ( 'NONE',  ( 1.000000000000000000, 0.000000000000000000, 0.000000000000000000 ) ) ;
#2214 = ORIENTED_EDGE ( 'NONE', *, *, #4094, .F. ) ;
#2216 = EDGE_CURVE ( 'NONE', #34249, #13744, #2256, .T. ) ;
#2215 = CARTESIAN_POINT ( 'NONE',  ( 66.24999999999998579, 33.74999999999999289, -3.750000000000000000 ) ) ;
#2217 = CIRCLE ( 'NONE', #40487, 1.000000000000000888 ) ;
#2218 = CARTESIAN_POINT ( 'NONE',  ( -87.50000000000000000, -8.499999999999989342, 21.00000000000000000 ) ) ;
#2219 =( GEOMETRIC_REPRESENTATION_CONTEXT ( 3 ) GLOBAL_UNCERTAINTY_ASSIGNED_CONTEXT ( ( #3136 ) ) GLOBAL_UNIT_ASSIGNED_CONTEXT ( ( #12265, #65048, #59788 ) ) REPRESENTATION_CONTEXT ( 'NONE', 'WORKASPACE' ) );
#2220 = ORIENTED_EDGE ( 'NONE', *, *, #11023, .T. ) ;
#2221 = CARTESIAN_POINT ( 'NONE',  ( 44.25000000000000000, 21.74999999999998579, 3.750000000000000000 ) ) ;
#2222 = AXIS2_PLACEMENT_3D ( 'NONE', #12572, #11543, #1276 ) ;
#2223 = CARTESIAN_POINT ( 'NONE',  ( 6.826472737025119919, 120.0070736234661553, 4.959722759717908325 ) ) ;
#2225 =( GEOMETRIC_REPRESENTATION_CONTEXT ( 3 ) GLOBAL_UNCERTAINTY_ASSIGNED_CONTEXT ( ( #32772 ) ) GLOBAL_UNIT_ASSIGNED_CONTEXT ( ( #62827, #14308, #46728 ) ) REPRESENTATION_CONTEXT ( 'NONE', 'WORKASPACE' ) );
#2224 = LINE ( 'NONE', #8289, #34988 ) ;
#2226 = CARTESIAN_POINT ( 'NONE',  ( -60.00000000000000000, -2.024042244987997205E-14, 9.500000000000000000 ) ) ;
#2227 = VECTOR ( 'NONE', #29351, 1000.000000000000000 ) ;
#2228 = LINE ( 'NONE', #6884, #11765 ) ;
#2229 = ORIENTED_EDGE ( 'NONE', *, *, #50611, .F. ) ;
#2230 = EDGE_CURVE ( 'NONE', #18730, #36574, #67390, .T. ) ;
#2231 = CARTESIAN_POINT ( 'NONE',  ( -44.99999999999977973, 149.4999999999999716, 10.00000000000000000 ) ) ;
#2232 = CARTESIAN_POINT ( 'NONE',  ( 15.48999599679679662, 146.9999999999999716, 9.500000000000000000 ) ) ;
#2233 = CIRCLE ( 'NONE', #41670, 0.5000000000000004441 ) ;
#2234 = ADVANCED_FACE ( 'NONE', ( #8659 ), #45638, .T. ) ;
#2235 = CARTESIAN_POINT ( 'NONE',  ( 6.735557395310448926E-16, -2.500000000000000000, 5.500000000000005329 ) ) ;
#2236 = CARTESIAN_POINT ( 'NONE',  ( -85.49499999999999034, 6.826472737025113702, -4.959722759717902107 ) ) ;
#2237 = EDGE_LOOP ( 'NONE', ( #52641, #18976, #63639, #50020, #406, #65293 ) ) ;
#2238 = VECTOR ( 'NONE', #40361, 1000.000000000000000 ) ;
#2239 = AXIS2_PLACEMENT_3D ( 'NONE', #31507, #17114, #38229 ) ;
#2240 = EDGE_CURVE ( 'NONE', #40785, #2052, #51105, .T. ) ;
#2241 = UNCERTAINTY_MEASURE_WITH_UNIT (LENGTH_MEASURE( 1.000000000000000082E-05 ), #47721, 'distance_accuracy_value', 'NONE');
#2242 = ORIENTED_EDGE ( 'NONE', *, *, #45483, .F. ) ;
#2243 =( NAMED_UNIT ( * ) SI_UNIT ( $, .STERADIAN. ) SOLID_ANGLE_UNIT ( ) );
#2244 =( GEOMETRIC_REPRESENTATION_CONTEXT ( 3 ) GLOBAL_UNCERTAINTY_ASSIGNED_CONTEXT ( ( #18558 ) ) GLOBAL_UNIT_ASSIGNED_CONTEXT ( ( #33255, #6489, #27932 ) ) REPRESENTATION_CONTEXT ( 'NONE', 'WORKASPACE' ) );
#2245 = ADVANCED_FACE ( 'NONE', ( #19182 ), #21886, .T. ) ;
#2246 = DIRECTION ( 'NONE',  ( 1.000000000000000000, -5.782411586589331015E-16, 0.000000000000000000 ) ) ;
#2247 = ORIENTED_EDGE ( 'NONE', *, *, #44208, .F. ) ;
#2248 =( NAMED_UNIT ( * ) PLANE_ANGLE_UNIT ( ) SI_UNIT ( $, .RADIAN. ) );
#2249 = ORIENTED_EDGE ( 'NONE', *, *, #12851, .T. ) ;
#2250 = SURFACE_STYLE_FILL_AREA ( #39300 ) ;
#2251 = PRESENTATION_STYLE_ASSIGNMENT (( #17499 ) ) ;
#2252 = CARTESIAN_POINT ( 'NONE',  ( -60.00000000000000000, -2.024042244987997205E-14, -12.00000000000000000 ) ) ;
#2253 = LINE ( 'NONE', #23780, #38963 ) ;
#2254 = CARTESIAN_POINT ( 'NONE',  ( -175.2570736234661695, 5.598654528085800663, -7.705886871421367523 ) ) ;
#2255 = STYLED_ITEM ( 'NONE', ( #7634 ), #59871 ) ;
#2256 = LINE ( 'NONE', #24459, #37639 ) ;
#2257 = CARTESIAN_POINT ( 'NONE',  ( -9.058813317711338797, 113.3449999999999847, 2.943386871421373563 ) ) ;
#2258 = CARTESIAN_POINT ( 'NONE',  ( -115.7070736234661865, -3.094860106618431139, -9.524999999999991473 ) ) ;
#2259 = PRESENTATION_LAYER_ASSIGNMENT (  '', '', ( #34920 ) ) ;
#2260 = CARTESIAN_POINT ( 'NONE',  ( -195.0000000000000000, 1.166476076187852838E-15, -9.524999999999991473 ) ) ;
#2261 = AXIS2_PLACEMENT_3D ( 'NONE', #967, #65774, #49258 ) ;
#2262 = CARTESIAN_POINT ( 'NONE',  ( 4.000000000000030198, 43.00000000000000000, 79.00402776293826435 ) ) ;
#2263 = ORIENTED_EDGE ( 'NONE', *, *, #55554, .F. ) ;
#2264 = PLANE ( 'NONE',  #31213 ) ;
#2265 = DIRECTION ( 'NONE',  ( 1.000000000000000000, 0.000000000000000000, 0.000000000000000000 ) ) ;
#2266 = ORIENTED_EDGE ( 'NONE', *, *, #61589, .T. ) ;
#2267 = CARTESIAN_POINT ( 'NONE',  ( -161.0050000000000239, 6.826472737025116366, 4.959722759717898555 ) ) ;
#2268 = DIRECTION ( 'NONE',  ( 0.000000000000000000, 0.000000000000000000, -1.000000000000000000 ) ) ;
#2269 = CARTESIAN_POINT ( 'NONE',  ( -183.6553645613615231, -6.378555885439770812, -6.171192800300671522 ) ) ;
#2270 =( GEOMETRIC_REPRESENTATION_CONTEXT ( 3 ) GLOBAL_UNCERTAINTY_ASSIGNED_CONTEXT ( ( #49071 ) ) GLOBAL_UNIT_ASSIGNED_CONTEXT ( ( #27531, #28567, #28206 ) ) REPRESENTATION_CONTEXT ( 'NONE', 'WORKASPACE' ) );
#2271 = CARTESIAN_POINT ( 'NONE',  ( -160.9449999999999932, -9.827790563157499189E-16, -8.024999999999991473 ) ) ;
#2272 = CARTESIAN_POINT ( 'NONE',  ( -160.9449999999999932, -9.827790563157499189E-16, -8.024999999999991473 ) ) ;
#2273 = AXIS2_PLACEMENT_3D ( 'NONE', #57866, #19511, #68076 ) ;
#2274 = VERTEX_POINT ( 'NONE', #45287 ) ;
#2275 = VECTOR ( 'NONE', #13608, 1000.000000000000000 ) ;
#2276 = CARTESIAN_POINT ( 'NONE',  ( -8.252730563585677359, 3.705851362693089346, 0.03572125916567089887 ) ) ;
#2277 = LINE ( 'NONE', #19905, #15497 ) ;
#2278 = CARTESIAN_POINT ( 'NONE',  ( 53.24999999999999289, 27.99999999999998579, -3.750000000000000000 ) ) ;
#2279 = CARTESIAN_POINT ( 'NONE',  ( -76.40499999999995850, -2.607480562269069768, 8.024999999999991473 ) ) ;
#2280 = DIRECTION ( 'NONE',  ( 0.000000000000000000, 0.000000000000000000, -1.000000000000000000 ) ) ;
#2281 = LINE ( 'NONE', #29788, #48310 ) ;
#2282 = CARTESIAN_POINT ( 'NONE',  ( -74.39499999999998181, -6.826472737025113702, -4.959722759717900331 ) ) ;
#2283 = CARTESIAN_POINT ( 'NONE',  ( -9.058813317711337021, 147.1549999999999727, -2.943386871421374895 ) ) ;
#2284 = DIRECTION ( 'NONE',  ( 1.000000000000000000, 0.000000000000000000, 0.000000000000000000 ) ) ;
#2285 = CARTESIAN_POINT ( 'NONE',  ( -71.75000000000000000, -4.000000000000000000, 19.00000000000000000 ) ) ;
#2286 = UNCERTAINTY_MEASURE_WITH_UNIT (LENGTH_MEASURE( 1.000000000000000082E-05 ), #47305, 'distance_accuracy_value', 'NONE');
#2287 = DIRECTION ( 'NONE',  ( -1.000000000000000000, 0.000000000000000000, 0.000000000000000000 ) ) ;
#2288 = CARTESIAN_POINT ( 'NONE',  ( -195.0000000000000000, 0.000000000000000000, 9.524999999999991473 ) ) ;
#2289 = CARTESIAN_POINT ( 'NONE',  ( 2.128399401614408669E-13, 154.1464374838464266, 9.171437483846471395 ) ) ;
#2290 = MECHANICAL_DESIGN_GEOMETRIC_PRESENTATION_REPRESENTATION (  '', ( #46249 ), #23713 ) ;
#2291 = CARTESIAN_POINT ( 'NONE',  ( 8.252730563585672030, 2.464278740834330517, -3.705851362693084905 ) ) ;
#2292 = LINE ( 'NONE', #44971, #1178 ) ;
#2293 = EDGE_CURVE ( 'NONE', #27282, #51168, #34561, .T. ) ;
#2294 = DIRECTION ( 'NONE',  ( 0.000000000000000000, 0.000000000000000000, 1.000000000000000000 ) ) ;
#2295 = DIRECTION ( 'NONE',  ( -0.000000000000000000, -1.000000000000000000, 0.000000000000000000 ) ) ;
#2296 = ORIENTED_EDGE ( 'NONE', *, *, #43191, .F. ) ;
#2297 = ORIENTED_EDGE ( 'NONE', *, *, #15659, .F. ) ;
#2298 = AXIS2_PLACEMENT_3D ( 'NONE', #52152, #36331, #31336 ) ;
#2299 = EDGE_CURVE ( 'NONE', #59244, #60780, #66826, .T. ) ;
#2300 = ADVANCED_FACE ( 'NONE', ( #56014 ), #33198, .T. ) ;
#2301 = COLOUR_RGB ( '', 0.72549020, 0.75294118, 0.79215686) ;
#2302 = PRESENTATION_STYLE_ASSIGNMENT (( #24862 ) ) ;
#2303 = DIRECTION ( 'NONE',  ( 0.000000000000000000, 0.000000000000000000, -1.000000000000000000 ) ) ;
#2304 = CARTESIAN_POINT ( 'NONE',  ( 5.710692600061826774, -4.108790270285303414, 4.269046054161672230E-16 ) ) ;
#2305 = EDGE_CURVE ( 'NONE', #12184, #14271, #61069, .T. ) ;
#2306 = DIRECTION ( 'NONE',  ( 0.000000000000000000, 0.000000000000000000, -1.000000000000000000 ) ) ;
#2307 = ORIENTED_EDGE ( 'NONE', *, *, #53747, .T. ) ;
#2308 = VECTOR ( 'NONE', #50991, 1000.000000000000000 ) ;
#2309 = ORIENTED_EDGE ( 'NONE', *, *, #52854, .F. ) ;
#2310 = CYLINDRICAL_SURFACE ( 'NONE', #30887, 8.999999999999994671 ) ;
#2311 = SURFACE_STYLE_FILL_AREA ( #44316 ) ;
#2312 = ADVANCED_FACE ( 'NONE', ( #11730 ), #7157, .T. ) ;
#2313 = VERTEX_POINT ( 'NONE', #44818 ) ;
#2314 = CARTESIAN_POINT ( 'NONE',  ( 60.00000000000000000, 1.797044900979284448E-15, 12.00000000000000000 ) ) ;
#2315 = CARTESIAN_POINT ( 'NONE',  ( -144.5929263765343080, -3.094860106626901253, -9.524999999993836397 ) ) ;
#2316 = EDGE_LOOP ( 'NONE', ( #2064, #58531, #51021, #55262, #12760, #47189, #49016, #60845, #46783, #49150, #16273, #54383, #35609, #26887, #4168, #57985, #52372, #63290, #69459, #15058 ) ) ;
#2317 = STYLED_ITEM ( 'NONE', ( #33777 ), #21691 ) ;
#2318 = ADVANCED_FACE ( 'NONE', ( #65542 ), #54961, .F. ) ;
#2319 = CARTESIAN_POINT ( 'NONE',  ( 74.99999999999998579, 50.00000000000000000, 7.500000000000000000 ) ) ;
#2320 = AXIS2_PLACEMENT_3D ( 'NONE', #35367, #24430, #13187 ) ;
#2321 = CARTESIAN_POINT ( 'NONE',  ( -47.50000000000000000, 99.99999999999992895, -10.00000000000000000 ) ) ;
#2322 = CARTESIAN_POINT ( 'NONE',  ( -109.3449999999999847, 7.632228543268599452, -2.479861379858951942 ) ) ;
#2323 = ORIENTED_EDGE ( 'NONE', *, *, #64532, .T. ) ;
#2324 = CIRCLE ( 'NONE', #116, 8.500000000000007105 ) ;
#2325 = VERTEX_POINT ( 'NONE', #8204 ) ;
#2326 =( REPRESENTATION_RELATIONSHIP ('NONE','NONE', #5102, #14558 ) REPRESENTATION_RELATIONSHIP_WITH_TRANSFORMATION ( #56802 )SHAPE_REPRESENTATION_RELATIONSHIP( ) );
#2327 = CARTESIAN_POINT ( 'NONE',  ( -10.16375755832578776, -11.93254622256288577, 1.312058623809986502 ) ) ;
#2328 = EDGE_CURVE ( 'NONE', #65761, #408, #2513, .T. ) ;
#2329 = DIRECTION ( 'NONE',  ( 0.000000000000000000, 0.000000000000000000, 1.000000000000000000 ) ) ;
#2330 = ORIENTED_EDGE ( 'NONE', *, *, #34952, .F. ) ;
#2331 = CARTESIAN_POINT ( 'NONE',  ( -6.826472737025120807, 147.3929263765337794, -4.959722759717907437 ) ) ;
#2332 = CARTESIAN_POINT ( 'NONE',  ( 15.98999599679679839, 146.4999999999999716, 7.000000000000000000 ) ) ;
#2333 =( NAMED_UNIT ( * ) PLANE_ANGLE_UNIT ( ) SI_UNIT ( $, .RADIAN. ) );
#2334 = CIRCLE ( 'NONE', #61949, 0.5000000000000004441 ) ;
#2335 =( LENGTH_UNIT ( ) NAMED_UNIT ( * ) SI_UNIT ( .MILLI., .METRE. ) );
#2336 = ORIENTED_EDGE ( 'NONE', *, *, #42742, .F. ) ;
#2337 = CIRCLE ( 'NONE', #41712, 0.5000000000000004441 ) ;
#2338 = LINE ( 'NONE', #62863, #19512 ) ;
#2339 = ORIENTED_EDGE ( 'NONE', *, *, #33147, .T. ) ;
#2340 = FACE_OUTER_BOUND ( 'NONE', #59199, .T. ) ;
#2341 = DIRECTION ( 'NONE',  ( 0.000000000000000000, -1.000000000000000000, 0.000000000000000000 ) ) ;
#2342 = CARTESIAN_POINT ( 'NONE',  ( -8.690363669209109077, -2.947848588679142789, 0.1381979515792671198 ) ) ;
#2343 = CARTESIAN_POINT ( 'NONE',  ( -130.8549999999999898, 4.716976649647094177, 6.492361379858945902 ) ) ;
#2344 = FACE_OUTER_BOUND ( 'NONE', #23122, .T. ) ;
#2345 = DIRECTION ( 'NONE',  ( 1.000000000000000000, 0.000000000000000000, 0.000000000000000000 ) ) ;
#2346 = ORIENTED_EDGE ( 'NONE', *, *, #10261, .T. ) ;
#2347 = AXIS2_PLACEMENT_3D ( 'NONE', #43451, #65881, #11367 ) ;
#2348 = SURFACE_STYLE_USAGE ( .BOTH. , #46777 ) ;
#2349 = CARTESIAN_POINT ( 'NONE',  ( -47.09072696197004149, -13.61106737609491013, 0.8658857160018818000 ) ) ;
#2350 = CARTESIAN_POINT ( 'NONE',  ( 1.000000000000000000, 14.00000000000000533, 35.50000000000000000 ) ) ;
#2351 = CARTESIAN_POINT ( 'NONE',  ( -45.00000000000000000, 9.117000356772807734, -6.738247770644822054 ) ) ;
#2352 = ORIENTED_EDGE ( 'NONE', *, *, #23333, .T. ) ;
#2353 = PRESENTATION_LAYER_ASSIGNMENT (  '', '', ( #47411 ) ) ;
#2354 = ORIENTED_EDGE ( 'NONE', *, *, #62987, .F. ) ;
#2355 =( LENGTH_UNIT ( ) NAMED_UNIT ( * ) SI_UNIT ( .MILLI., .METRE. ) );
#2356 = CARTESIAN_POINT ( 'NONE',  ( -20.56536453975222756, 115.3173173917729173, 10.00000000000000000 ) ) ;
#2357 = FACE_OUTER_BOUND ( 'NONE', #8309, .T. ) ;
#2358 = CARTESIAN_POINT ( 'NONE',  ( -49.70499999999996987, 2.607480562269073321, 8.024999999999991473 ) ) ;
#2359 = ORIENTED_EDGE ( 'NONE', *, *, #20850, .F. ) ;
#2360 =( LENGTH_UNIT ( ) NAMED_UNIT ( * ) SI_UNIT ( .MILLI., .METRE. ) );
#2361 = CARTESIAN_POINT ( 'NONE',  ( -183.9550000000000125, -7.632228543268599452, 2.479861379858951054 ) ) ;
#2362 = CYLINDRICAL_SURFACE ( 'NONE', #40303, 9.524999999999991473 ) ;
#2363 = CARTESIAN_POINT ( 'NONE',  ( -60.05707362346616662, 0.000000000000000000, 9.524999999999991473 ) ) ;
#2364 = FACE_OUTER_BOUND ( 'NONE', #32171, .T. ) ;
#2365 = CARTESIAN_POINT ( 'NONE',  ( -60.00000000000000000, -2.024042244987997205E-14, -7.000000000000024869 ) ) ;
#2366 = ORIENTED_EDGE ( 'NONE', *, *, #2755, .F. ) ;
#2367 =( BOUNDED_CURVE ( )  B_SPLINE_CURVE ( 2, ( #19020, #13070, #23971, #7110, #34874, #34524, #8158, #19384, #46161, #51069, #1774 ),
 .UNSPECIFIED., .F., .F. ) 
 B_SPLINE_CURVE_WITH_KNOTS ( ( 3, 2, 2, 2, 2, 3 ),
 ( 0.2282608695652120212, 0.2304347826086902418, 0.2326086956521684346, 0.2347826086956466551, 0.2369565217391248479, 0.2391304347826030685 ),
 .UNSPECIFIED. ) 
 CURVE ( )  GEOMETRIC_REPRESENTATION_ITEM ( )  RATIONAL_B_SPLINE_CURVE ( ( 1.000000000000120570, 0.9510565162950328499, 1.000000000000000000, 0.9510565162951535312, 1.000000000000000000, 0.9510565162951535312, 1.000000000000000000, 0.9510565162951535312, 1.000000000000000000, 0.9510565162952804297, 0.9999999999998731015 ) ) 
 REPRESENTATION_ITEM ( '' )  );
#2368 = EDGE_CURVE ( 'NONE', #31733, #14584, #43166, .T. ) ;
#2369 = CARTESIAN_POINT ( 'NONE',  ( -162.0570736234661808, 0.000000000000000000, 9.524999999999991473 ) ) ;
#2370 = COLOUR_RGB ( '', 0.09019608, 0.27058824, 0.51372549) ;
#2371 = CARTESIAN_POINT ( 'NONE',  ( -98.45499999999998408, 7.632228543268599452, -2.479861379858951942 ) ) ;
#2372 = CARTESIAN_POINT ( 'NONE',  ( 8.706197787039554825, 154.4999999999999147, -3.888687344776530885 ) ) ;
#2373 = VECTOR ( 'NONE', #25912, 1000.000000000000000 ) ;
#2374 = CARTESIAN_POINT ( 'NONE',  ( -55.00000000000000000, -2.024042244987997205E-14, -12.00000000000000000 ) ) ;
#2375 = AXIS2_PLACEMENT_3D ( 'NONE', #25103, #46616, #57461 ) ;
#2376 = CARTESIAN_POINT ( 'NONE',  ( -102.7449999999999903, 4.716976649647094177, 6.492361379858945902 ) ) ;
#2377 = CARTESIAN_POINT ( 'NONE',  ( -9.058813317711337021, 114.1549999999999869, -2.943386871421374895 ) ) ;
#2378 = CARTESIAN_POINT ( 'NONE',  ( -76.64499999999999602, 4.716976649647091513, -6.492361379858946790 ) ) ;
#2379 =( GEOMETRIC_REPRESENTATION_CONTEXT ( 3 ) GLOBAL_UNCERTAINTY_ASSIGNED_CONTEXT ( ( #31444 ) ) GLOBAL_UNIT_ASSIGNED_CONTEXT ( ( #21067, #31965, #46829 ) ) REPRESENTATION_CONTEXT ( 'NONE', 'WORKASPACE' ) );
#2380 = CARTESIAN_POINT ( 'NONE',  ( 0.000000000000000000, 0.000000000000000000, 7.500000000000000000 ) ) ;
#2381 = AXIS2_PLACEMENT_3D ( 'NONE', #66229, #28220, #754 ) ;
#2382 = SURFACE_SIDE_STYLE ('',( #68217 ) ) ;
#2383 = UNCERTAINTY_MEASURE_WITH_UNIT (LENGTH_MEASURE( 1.000000000000000082E-05 ), #3755, 'distance_accuracy_value', 'NONE');
#2384 = VECTOR ( 'NONE', #67549, 1000.000000000000000 ) ;
#2385 = DIRECTION ( 'NONE',  ( -1.000000000000000000, 0.000000000000000000, 1.300977106640434644E-16 ) ) ;
#2386 = LINE ( 'NONE', #45418, #1456 ) ;
#2387 = VERTEX_POINT ( 'NONE', #18410 ) ;
#2388 = CARTESIAN_POINT ( 'NONE',  ( -115.3429263765337964, -9.058813317711329915, 2.943386871421371787 ) ) ;
#2389 =( NAMED_UNIT ( * ) PLANE_ANGLE_UNIT ( ) SI_UNIT ( $, .RADIAN. ) );
#2390 = CARTESIAN_POINT ( 'NONE',  ( -137.5449999999999875, -7.632228543268600340, -2.479861379858950166 ) ) ;
#2392 = CYLINDRICAL_SURFACE ( 'NONE', #48244, 8.025000000000000355 ) ;
#2391 = VECTOR ( 'NONE', #35253, 1000.000000000000000 ) ;
#2393 = VECTOR ( 'NONE', #37943, 1000.000000000000000 ) ;
#2394 = EDGE_CURVE ( 'NONE', #2414, #7688, #21767, .T. ) ;
#2395 = DIRECTION ( 'NONE',  ( 0.000000000000000000, 0.000000000000000000, -1.000000000000000000 ) ) ;
#2396 = AXIS2_PLACEMENT_3D ( 'NONE', #42704, #10, #26469 ) ;
#2397 = CARTESIAN_POINT ( 'NONE',  ( 0.000000000000000000, 2.299999999999999822, 0.000000000000000000 ) ) ;
#2398 = VERTEX_POINT ( 'NONE', #2137 ) ;
#2399 = VERTEX_POINT ( 'NONE', #46211 ) ;
#2400 = DIRECTION ( 'NONE',  ( 0.000000000000000000, 1.000000000000000000, 0.000000000000000000 ) ) ;
#2401 = CARTESIAN_POINT ( 'NONE',  ( 0.000000000000000000, 115.4999999999999574, 16.50000000000000000 ) ) ;
#2402 = EDGE_CURVE ( 'NONE', #40347, #32368, #52129, .T. ) ;
#2403 = AXIS2_PLACEMENT_3D ( 'NONE', #31743, #9970, #15606 ) ;
#2404 = DIRECTION ( 'NONE',  ( 0.000000000000000000, 0.000000000000000000, -1.000000000000000000 ) ) ;
#2405 = DIRECTION ( 'NONE',  ( 1.000000000000000000, 0.000000000000000000, 0.000000000000000000 ) ) ;
#2406 = LINE ( 'NONE', #13716, #62136 ) ;
#2407 = CARTESIAN_POINT ( 'NONE',  ( 0.000000000000000000, 0.000000000000000000, 0.2499999999999924227 ) ) ;
#2408 = ORIENTED_EDGE ( 'NONE', *, *, #26432, .F. ) ;
#2409 = CARTESIAN_POINT ( 'NONE',  ( -135.3549999999999898, -4.716976649647093289, -6.492361379858945902 ) ) ;
#2410 = VERTEX_POINT ( 'NONE', #61301 ) ;
#2411 = VERTEX_POINT ( 'NONE', #19433 ) ;
#2412 = CARTESIAN_POINT ( 'NONE',  ( -171.7429263765338305, -5.598654528085803328, -7.705886871421366635 ) ) ;
#2413 = CARTESIAN_POINT ( 'NONE',  ( -83.84292637653379643, 9.058813317711329915, -2.943386871421373119 ) ) ;
#2414 = VERTEX_POINT ( 'NONE', #40931 ) ;
#2415 = EDGE_CURVE ( 'NONE', #57518, #35469, #19497, .T. ) ;
#2416 = CIRCLE ( 'NONE', #29430, 22.50000000000000000 ) ;
#2417 = CARTESIAN_POINT ( 'NONE',  ( -102.2929263765348367, 3.094860106601218241, -9.525000000012498802 ) ) ;
#2418 = DIRECTION ( 'NONE',  ( 0.000000000000000000, 0.000000000000000000, 1.000000000000000000 ) ) ;
#2419 = CARTESIAN_POINT ( 'NONE',  ( 9.058813317711338797, 135.8449999999999989, -2.943386871421372675 ) ) ;
#2420 = DIRECTION ( 'NONE',  ( -0.000000000000000000, -1.000000000000000000, -0.000000000000000000 ) ) ;
#2421 = VERTEX_POINT ( 'NONE', #34234 ) ;
#2422 = VECTOR ( 'NONE', #46931, 1000.000000000000114 ) ;
#2423 = DIRECTION ( 'NONE',  ( 0.000000000000000000, 0.7431448254773944662, 0.6691306063588580155 ) ) ;
#2424 = CARTESIAN_POINT ( 'NONE',  ( -5.598654528085806881, 137.8549999999999898, -7.705886871421374629 ) ) ;
#2425 = CIRCLE ( 'NONE', #41751, 6.999999999999997335 ) ;
#2426 =( LENGTH_UNIT ( ) NAMED_UNIT ( * ) SI_UNIT ( .MILLI., .METRE. ) );
#2427 = ADVANCED_FACE ( 'NONE', ( #28925 ), #13816, .T. ) ;
#2428 = CARTESIAN_POINT ( 'NONE',  ( 57.24999999999999289, 28.24999999999998934, 4.000000000000000000 ) ) ;
#2429 = ORIENTED_EDGE ( 'NONE', *, *, #19167, .T. ) ;
#2430 = CARTESIAN_POINT ( 'NONE',  ( -4.716976649647097730, 117.2429263765338163, -6.492361379858953896 ) ) ;
#2431 = DIRECTION ( 'NONE',  ( -0.000000000000000000, -1.000000000000000000, -0.000000000000000000 ) ) ;
#2432 = UNCERTAINTY_MEASURE_WITH_UNIT (LENGTH_MEASURE( 1.000000000000000082E-05 ), #24097, 'distance_accuracy_value', 'NONE');
#2433 = AXIS2_PLACEMENT_3D ( 'NONE', #68780, #10385, #31108 ) ;
#2434 = CARTESIAN_POINT ( 'NONE',  ( -88.19292637653379074, -10.01517768586948698, 6.132527647946031529E-16 ) ) ;
#2435 = DIRECTION ( 'NONE',  ( -0.000000000000000000, 1.000000000000000000, -0.000000000000000000 ) ) ;
#2436 = DIRECTION ( 'NONE',  ( -0.5000000000000003331, -0.8660254037844384856, 0.000000000000000000 ) ) ;
#2437 = ORIENTED_EDGE ( 'NONE', *, *, #30727, .T. ) ;
#2438 = CIRCLE ( 'NONE', #59790, 10.00000000000000000 ) ;
#2439 =( LENGTH_UNIT ( ) NAMED_UNIT ( * ) SI_UNIT ( .MILLI., .METRE. ) );
#2440 = ORIENTED_EDGE ( 'NONE', *, *, #68940, .T. ) ;
#2441 = DIRECTION ( 'NONE',  ( 0.000000000000000000, -1.000000000000000000, 0.000000000000000000 ) ) ;
#2442 = CARTESIAN_POINT ( 'NONE',  ( -70.87837837837835764, 13.70805908423323949, 9.500000000000000000 ) ) ;
#2443 = CARTESIAN_POINT ( 'NONE',  ( -47.00571487472603138, -11.85301361210301607, 3.279042910798483312 ) ) ;
#2444 = CARTESIAN_POINT ( 'NONE',  ( -165.5049999999999955, -6.826472737025115478, -4.959722759717899443 ) ) ;
#2446 = ORIENTED_EDGE ( 'NONE', *, *, #61390, .T. ) ;
#2445 = AXIS2_PLACEMENT_3D ( 'NONE', #17055, #1478, #38537 ) ;
#2447 = SURFACE_STYLE_FILL_AREA ( #55267 ) ;
#2448 = UNCERTAINTY_MEASURE_WITH_UNIT (LENGTH_MEASURE( 1.000000000000000082E-05 ), #57735, 'distance_accuracy_value', 'NONE');
#2449 = AXIS2_PLACEMENT_3D ( 'NONE', #60100, #28770, #27718 ) ;
#2450 = DIRECTION ( 'NONE',  ( 1.000000000000000000, 0.000000000000000000, 0.000000000000000000 ) ) ;
#2451 = PRESENTATION_STYLE_ASSIGNMENT (( #29224 ) ) ;
#2452 = FILL_AREA_STYLE ('',( #12705 ) ) ;
#2453 = ORIENTED_EDGE ( 'NONE', *, *, #10095, .F. ) ;
#2454 = ORIENTED_EDGE ( 'NONE', *, *, #47966, .F. ) ;
#2455 = FACE_OUTER_BOUND ( 'NONE', #46483, .T. ) ;
#2456 = LINE ( 'NONE', #41830, #62734 ) ;
#2457 = VECTOR ( 'NONE', #51480, 1000.000000000000000 ) ;
#2458 = CARTESIAN_POINT ( 'NONE',  ( -75.65499999999998693, -7.632228543268600340, -2.479861379858950166 ) ) ;
#2459 = VERTEX_POINT ( 'NONE', #61629 ) ;
#2460 = FILL_AREA_STYLE_COLOUR ( '', #22760 ) ;
#2461 = DIRECTION ( 'NONE',  ( -1.000000000000000000, 0.000000000000000000, 0.000000000000000000 ) ) ;
#2462 = CARTESIAN_POINT ( 'NONE',  ( -1.502314598737159031E-15, -2.500000000000000000, -9.000000000000000000 ) ) ;
#2463 = ADVANCED_FACE ( 'NONE', ( #66948 ), #50763, .F. ) ;
#2464 = AXIS2_PLACEMENT_3D ( 'NONE', #34955, #56400, #56047 ) ;
#2465 = DIRECTION ( 'NONE',  ( -0.000000000000000000, -0.000000000000000000, 1.000000000000000000 ) ) ;
#2466 = ORIENTED_EDGE ( 'NONE', *, *, #766, .T. ) ;
#2467 = VECTOR ( 'NONE', #35994, 1000.000000000000000 ) ;
#2469 = DIRECTION ( 'NONE',  ( -1.000000000000000000, 0.000000000000000000, 0.000000000000000000 ) ) ;
#2468 = CARTESIAN_POINT ( 'NONE',  ( 41.49999999999997868, 9.999999999999980460, 3.000000000000000000 ) ) ;
#2470 = CARTESIAN_POINT ( 'NONE',  ( 3.094860106618435136, 142.2950000000000159, -9.525000000000000355 ) ) ;
#2471 = CARTESIAN_POINT ( 'NONE',  ( -104.6949999999999790, -8.437984349512085203, 5.166775262442717831E-16 ) ) ;
#2472 =( NAMED_UNIT ( * ) PLANE_ANGLE_UNIT ( ) SI_UNIT ( $, .RADIAN. ) );
#2473 = CIRCLE ( 'NONE', #20515, 0.7499999999999997780 ) ;
#2474 = AXIS2_PLACEMENT_3D ( 'NONE', #30122, #24853, #47059 ) ;
#2475 = CARTESIAN_POINT ( 'NONE',  ( -74.75000000000000000, -4.000000000000000000, 6.000000000000001776 ) ) ;
#2476 = PRODUCT_RELATED_PRODUCT_CATEGORY ( 'part', '', ( #9133 ) ) ;
#2478 = CARTESIAN_POINT ( 'NONE',  ( -19.83697256712734713, 11.93284552246408659, -1.308412769435526091 ) ) ;
#2477 = SURFACE_STYLE_USAGE ( .BOTH. , #50733 ) ;
#2479 = COLOUR_RGB ( '', 0.72549020, 0.75294118, 0.79215686) ;
#2480 = ADVANCED_FACE ( 'NONE', ( #62351, #45849, #55687 ), #8553, .T. ) ;
#2481 = CARTESIAN_POINT ( 'NONE',  ( -139.1929263765337907, -10.01517768586948698, 6.132527647946031529E-16 ) ) ;
#2482 = CARTESIAN_POINT ( 'NONE',  ( -164.8449999999999989, -7.632228543268599452, 2.479861379858951054 ) ) ;
#2483 = COLOUR_RGB ( '', 0.31764706, 0.68627451, 0.89019608) ;
#2484 = EDGE_CURVE ( 'NONE', #6265, #30255, #38713, .T. ) ;
#2485 = ADVANCED_FACE ( 'NONE', ( #41619 ), #63035, .T. ) ;
#2486 = AXIS2_PLACEMENT_3D ( 'NONE', #23252, #55606, #39809 ) ;
#2487 = DIRECTION ( 'NONE',  ( 0.000000000000000000, 0.000000000000000000, 1.000000000000000000 ) ) ;
#2488 = VERTEX_POINT ( 'NONE', #47971 ) ;
#2489 = CARTESIAN_POINT ( 'NONE',  ( -7.632228543268608334, 129.8429263765338249, 2.479861379858952830 ) ) ;
#2490 = ORIENTED_EDGE ( 'NONE', *, *, #24499, .F. ) ;
#2491 = AXIS2_PLACEMENT_3D ( 'NONE', #9952, #52871, #4650 ) ;
#2492 = UNCERTAINTY_MEASURE_WITH_UNIT (LENGTH_MEASURE( 1.000000000000000082E-05 ), #53386, 'distance_accuracy_value', 'NONE');
#2493 = EDGE_CURVE ( 'NONE', #39125, #5467, #47624, .T. ) ;
#2494 = FILL_AREA_STYLE_COLOUR ( '', #60778 ) ;
#2495 = FACE_OUTER_BOUND ( 'NONE', #39996, .T. ) ;
#2496 = CARTESIAN_POINT ( 'NONE',  ( 16.75000000000000711, 25.24999999999998224, -4.000000000000000000 ) ) ;
#2497 = EDGE_CURVE ( 'NONE', #11976, #1198, #57068, .T. ) ;
#2498 = DIRECTION ( 'NONE',  ( 0.000000000000000000, 0.000000000000000000, 1.000000000000000000 ) ) ;
#2499 = PRESENTATION_LAYER_ASSIGNMENT (  '', '', ( #63213 ) ) ;
#2500 = VERTEX_POINT ( 'NONE', #20111 ) ;
#2501 = CARTESIAN_POINT ( 'NONE',  ( -159.9549999999999841, -7.632228543268599452, 2.479861379858951054 ) ) ;
#2502 = VECTOR ( 'NONE', #66181, 1000.000000000000000 ) ;
#2503 = ORIENTED_EDGE ( 'NONE', *, *, #21511, .F. ) ;
#2504 = PRESENTATION_LAYER_ASSIGNMENT (  '', '', ( #43042 ) ) ;
#2505 = CYLINDRICAL_SURFACE ( 'NONE', #61236, 4.999999999999997335 ) ;
#2506 = ORIENTED_EDGE ( 'NONE', *, *, #54300, .F. ) ;
#2507 = EDGE_CURVE ( 'NONE', #56670, #18337, #32738, .T. ) ;
#2508 =( NAMED_UNIT ( * ) SI_UNIT ( $, .STERADIAN. ) SOLID_ANGLE_UNIT ( ) );
#2509 = LINE ( 'NONE', #1465, #48886 ) ;
#2510 = CARTESIAN_POINT ( 'NONE',  ( -1.166476076187854022E-15, 110.9449999999999932, 9.525000000000000355 ) ) ;
#2511 = AXIS2_PLACEMENT_3D ( 'NONE', #35926, #24641, #36995 ) ;
#2512 = EDGE_LOOP ( 'NONE', ( #675, #60942, #31621 ) ) ;
#2513 = LINE ( 'NONE', #39894, #49849 ) ;
#2514 = CARTESIAN_POINT ( 'NONE',  ( 0.000000000000000000, 110.5549999999999926, -9.525000000000000355 ) ) ;
#2515 = CARTESIAN_POINT ( 'NONE',  ( -75.05499999999997840, -9.827790563157499189E-16, -8.024999999999991473 ) ) ;
#2516 = EDGE_CURVE ( 'NONE', #22068, #8806, #51985, .T. ) ;
#2517 = CARTESIAN_POINT ( 'NONE',  ( 10.01517768586949231, 124.8049999999999642, 1.839758294383810543E-15 ) ) ;
#2518 = UNCERTAINTY_MEASURE_WITH_UNIT (LENGTH_MEASURE( 1.000000000000000082E-05 ), #25440, 'distance_accuracy_value', 'NONE');
#2519 = AXIS2_PLACEMENT_3D ( 'NONE', #62965, #6302, #5953 ) ;
#2520 = DIRECTION ( 'NONE',  ( 0.000000000000000000, 0.000000000000000000, 1.000000000000000000 ) ) ;
#2521 = DIRECTION ( 'NONE',  ( -1.000000000000000000, 0.000000000000000000, 0.000000000000000000 ) ) ;
#2522 = FACE_OUTER_BOUND ( 'NONE', #4551, .T. ) ;
#2523 = ORIENTED_EDGE ( 'NONE', *, *, #33273, .T. ) ;
#2524 = CIRCLE ( 'NONE', #20554, 0.5000000000000004441 ) ;
#2525 = CIRCLE ( 'NONE', #9326, 0.5000000000000004441 ) ;
#2526 = FACE_OUTER_BOUND ( 'NONE', #13806, .T. ) ;
#2527 = CARTESIAN_POINT ( 'NONE',  ( -55.19499999999998607, 8.437984349512085203, -1.550032578732815448E-15 ) ) ;
#2528 = EDGE_LOOP ( 'NONE', ( #8203, #68573, #5606, #57331 ) ) ;
#2529 = LINE ( 'NONE', #24036, #44107 ) ;
#2530 = CARTESIAN_POINT ( 'NONE',  ( 6.938426666069061000, 2.291132984336068823, -1.982292489777642164 ) ) ;
#2531 = CARTESIAN_POINT ( 'NONE',  ( -86.99292637653378790, 8.102448949553172852, -5.886773742842744461 ) ) ;
#2532 = CARTESIAN_POINT ( 'NONE',  ( 6.062177826491071286, -3.500000000000002220, 0.000000000000000000 ) ) ;
#2533 = ORIENTED_EDGE ( 'NONE', *, *, #32733, .F. ) ;
#2534 = CARTESIAN_POINT ( 'NONE',  ( -50.85337874892448440, -12.07627951188113080, 3.038067889716521197 ) ) ;
#2535 = CARTESIAN_POINT ( 'NONE',  ( -53.09499999999997755, -2.607480562269071545, -8.024999999999991473 ) ) ;
#2536 = FACE_OUTER_BOUND ( 'NONE', #18430, .T. ) ;
#2537 = ORIENTED_EDGE ( 'NONE', *, *, #9870, .T. ) ;
#2538 = CARTESIAN_POINT ( 'NONE',  ( -75.00000000000000000, 9.675838479951730520, 6.195399861057270030 ) ) ;
#2539 = CARTESIAN_POINT ( 'NONE',  ( -104.7549999999999812, 4.716976649647091513, -6.492361379858946790 ) ) ;
#2540 = EDGE_LOOP ( 'NONE', ( #19733, #39653, #35537, #69008 ) ) ;
#2541 =( NAMED_UNIT ( * ) SI_UNIT ( $, .STERADIAN. ) SOLID_ANGLE_UNIT ( ) );
#2542 = LINE ( 'NONE', #60978, #42670 ) ;
#2543 = DIRECTION ( 'NONE',  ( 1.156482317317873451E-16, 1.000000000000000000, 0.000000000000000000 ) ) ;
#2544 = CARTESIAN_POINT ( 'NONE',  ( -144.0570736234661808, 0.000000000000000000, 9.524999999999991473 ) ) ;
#2545 = COLOUR_RGB ( '', 0.40784314, 0.44705882, 0.49803922) ;
#2546 = DIRECTION ( 'NONE',  ( -0.000000000000000000, -1.000000000000000000, -0.000000000000000000 ) ) ;
#2547 = CARTESIAN_POINT ( 'NONE',  ( 9.058813317711338797, 138.8449999999999989, -2.943386871421372675 ) ) ;
#2548 = CARTESIAN_POINT ( 'NONE',  ( -83.30707362346619504, -10.01517768586948698, 6.132527647946031529E-16 ) ) ;
#2549 =( GEOMETRIC_REPRESENTATION_CONTEXT ( 3 ) GLOBAL_UNCERTAINTY_ASSIGNED_CONTEXT ( ( #54525 ) ) GLOBAL_UNIT_ASSIGNED_CONTEXT ( ( #17244, #60112, #23186 ) ) REPRESENTATION_CONTEXT ( 'NONE', 'WORKASPACE' ) );
#2550 = MECHANICAL_DESIGN_GEOMETRIC_PRESENTATION_REPRESENTATION (  '', ( #29722 ), #45324 ) ;
#2551 = DIRECTION ( 'NONE',  ( 0.000000000000000000, 1.000000000000000000, 0.000000000000000000 ) ) ;
#2552 = CARTESIAN_POINT ( 'NONE',  ( 31.00000000000000711, 50.00000000000000000, -60.00000000000000711 ) ) ;
#2554 = DIRECTION ( 'NONE',  ( 0.000000000000000000, 0.000000000000000000, 1.000000000000000000 ) ) ;
#2553 =( NAMED_UNIT ( * ) SI_UNIT ( $, .STERADIAN. ) SOLID_ANGLE_UNIT ( ) );
#2555 = AXIS2_PLACEMENT_3D ( 'NONE', #35981, #4640, #57426 ) ;
#2556 = AXIS2_PLACEMENT_3D ( 'NONE', #29166, #8451, #51348 ) ;
#2557 = CARTESIAN_POINT ( 'NONE',  ( -125.0049999999999812, 6.826472737025116366, 4.959722759717898555 ) ) ;
#2558 = CARTESIAN_POINT ( 'NONE',  ( -74.99999999999998579, 50.00000000000000000, 6.999999999999988454 ) ) ;
#2559 = DIRECTION ( 'NONE',  ( 1.000000000000000000, 0.000000000000000000, 0.000000000000000000 ) ) ;
#2560 = SURFACE_SIDE_STYLE ('',( #38207 ) ) ;
#2561 = CARTESIAN_POINT ( 'NONE',  ( -131.5449999999999875, -7.632228543268600340, -2.479861379858950166 ) ) ;
#2562 = CARTESIAN_POINT ( 'NONE',  ( -117.2950000000000017, -2.607480562269069768, 8.024999999999991473 ) ) ;
#2563 = CARTESIAN_POINT ( 'NONE',  ( -45.48309787872866394, 9.683080749504640039, -3.000000000000000444 ) ) ;
#2564 = VERTEX_POINT ( 'NONE', #30310 ) ;
#2565 = DIRECTION ( 'NONE',  ( 0.000000000000000000, -1.000000000000000000, 0.000000000000000000 ) ) ;
#2566 = CIRCLE ( 'NONE', #3681, 0.5000000000000004441 ) ;
#2567 =( NAMED_UNIT ( * ) PLANE_ANGLE_UNIT ( ) SI_UNIT ( $, .RADIAN. ) );
#2568 = ADVANCED_FACE ( 'NONE', ( #63726 ), #42673, .F. ) ;
#2569 = CARTESIAN_POINT ( 'NONE',  ( -171.4429263765337907, -1.166476076187852838E-15, -9.524999999999991473 ) ) ;
#2570 = DIRECTION ( 'NONE',  ( 0.000000000000000000, -0.000000000000000000, -1.000000000000000000 ) ) ;
#2571 = EDGE_CURVE ( 'NONE', #9516, #33963, #1551, .T. ) ;
#2572 = EDGE_CURVE ( 'NONE', #7443, #68025, #40966, .T. ) ;
#2573 = SURFACE_SIDE_STYLE ('',( #15220 ) ) ;
#2574 = DIRECTION ( 'NONE',  ( 0.000000000000000000, 1.000000000000000000, 0.000000000000000000 ) ) ;
#2575 = AXIS2_PLACEMENT_3D ( 'NONE', #67750, #9367, #62795 ) ;
#2577 = AXIS2_PLACEMENT_3D ( 'NONE', #17403, #28228, #56996 ) ;
#2576 = CIRCLE ( 'NONE', #42002, 0.2500000000000002220 ) ;
#2578 = DIRECTION ( 'NONE',  ( 1.000000000000000000, 0.000000000000000000, -1.300977106640434891E-16 ) ) ;
#2579 = DIRECTION ( 'NONE',  ( 0.000000000000000000, 0.000000000000000000, 1.000000000000000000 ) ) ;
#2580 = ORIENTED_EDGE ( 'NONE', *, *, #45397, .T. ) ;
#2581 = CARTESIAN_POINT ( 'NONE',  ( -94.19292637653380496, -10.01517768586948698, 6.132527647946031529E-16 ) ) ;
#2582 = APPLICATION_PROTOCOL_DEFINITION ( 'draft international standard', 'automotive_design', 1998, #47872 ) ;
#2583 = CARTESIAN_POINT ( 'NONE',  ( -53.18756747357285519, -10.02680648607945102, -3.500000000000002220 ) ) ;
#2584 = FILL_AREA_STYLE_COLOUR ( '', #29362 ) ;
#2585 = AXIS2_PLACEMENT_3D ( 'NONE', #13472, #8224, #30005 ) ;
#2586 = LINE ( 'NONE', #18480, #2227 ) ;
#2587 = CARTESIAN_POINT ( 'NONE',  ( -12.72792206135785698, 114.9999999999999574, 10.50000000000000000 ) ) ;
#2588 = CARTESIAN_POINT ( 'NONE',  ( -79.10707362346616378, 8.102448949553172852, -5.886773742842744461 ) ) ;
#2589 = EDGE_CURVE ( 'NONE', #61460, #12604, #29681, .T. ) ;
#2590 = SURFACE_STYLE_FILL_AREA ( #9320 ) ;
#2591 = CIRCLE ( 'NONE', #12727, 10.00000000000000000 ) ;
#2592 = ORIENTED_EDGE ( 'NONE', *, *, #12382, .T. ) ;
#2593 = FACE_OUTER_BOUND ( 'NONE', #50511, .T. ) ;
#2594 = ORIENTED_EDGE ( 'NONE', *, *, #35095, .T. ) ;
#2595 = CARTESIAN_POINT ( 'NONE',  ( -7.632228543268608334, 133.9570736234661581, 2.479861379858952830 ) ) ;
#2596 = AXIS2_PLACEMENT_3D ( 'NONE', #8731, #56207, #51300 ) ;
#2597 = CARTESIAN_POINT ( 'NONE',  ( -4.716976649647097730, 133.3570736234661638, -6.492361379858953896 ) ) ;
#2598 = CIRCLE ( 'NONE', #64471, 0.5000000000000004441 ) ;
#2599 = DIRECTION ( 'NONE',  ( 1.000000000000000000, 0.000000000000000000, 0.000000000000000000 ) ) ;
#2601 = CARTESIAN_POINT ( 'NONE',  ( 74.50000000000000000, 19.30628705663858469, -6.500000000000000888 ) ) ;
#2600 = AXIS2_PLACEMENT_3D ( 'NONE', #47237, #8863, #62651 ) ;
#2602 = SPHERICAL_SURFACE ( 'NONE', #46627, 1.000000000000000000 ) ;
#2603 = ORIENTED_EDGE ( 'NONE', *, *, #64246, .F. ) ;
#2604 =( GEOMETRIC_REPRESENTATION_CONTEXT ( 3 ) GLOBAL_UNCERTAINTY_ASSIGNED_CONTEXT ( ( #64455 ) ) GLOBAL_UNIT_ASSIGNED_CONTEXT ( ( #35889, #62268, #14095 ) ) REPRESENTATION_CONTEXT ( 'NONE', 'WORKASPACE' ) );
#2605 = LINE ( 'NONE', #19518, #51190 ) ;
#2606 = AXIS2_PLACEMENT_3D ( 'NONE', #33685, #66745, #28741 ) ;
#2607 = PLANE ( 'NONE',  #20415 ) ;
#2608 = CYLINDRICAL_SURFACE ( 'NONE', #20971, 0.2500000000000002220 ) ;
#2609 = EDGE_CURVE ( 'NONE', #18673, #27373, #69510, .T. ) ;
#2610 = DIRECTION ( 'NONE',  ( -0.000000000000000000, -0.000000000000000000, -1.000000000000000000 ) ) ;
#2611 = AXIS2_PLACEMENT_3D ( 'NONE', #1391, #49302, #32762 ) ;
#2612 = CARTESIAN_POINT ( 'NONE',  ( -71.45707362346617231, -9.058813317711329915, 2.943386871421371787 ) ) ;
#2613 = ADVANCED_FACE ( 'NONE', ( #6368, #59845 ), #64075, .T. ) ;
#2614 = CARTESIAN_POINT ( 'NONE',  ( -77.99499999999997613, -6.826472737025115478, 4.959722759717900331 ) ) ;
#2615 = VERTEX_POINT ( 'NONE', #33459 ) ;
#2616 = AXIS2_PLACEMENT_3D ( 'NONE', #51317, #31219, #67850 ) ;
#2617 = SURFACE_STYLE_FILL_AREA ( #61388 ) ;
#2618 = SURFACE_STYLE_FILL_AREA ( #19527 ) ;
#2619 = CARTESIAN_POINT ( 'NONE',  ( -12.34222745343792127, 115.4999999999999574, -10.18181818181818166 ) ) ;
#2620 = ORIENTED_EDGE ( 'NONE', *, *, #36828, .T. ) ;
#2621 = SURFACE_STYLE_USAGE ( .BOTH. , #61049 ) ;
#2623 = CARTESIAN_POINT ( 'NONE',  ( -7.440601873764707719, -1.112499515747335854, 0.4948905776603325646 ) ) ;
#2622 = VECTOR ( 'NONE', #32591, 1000.000000000000000 ) ;
#2624 = ORIENTED_EDGE ( 'NONE', *, *, #68364, .F. ) ;
#2625 = FILL_AREA_STYLE ('',( #19537 ) ) ;
#2626 = ORIENTED_EDGE ( 'NONE', *, *, #3354, .T. ) ;
#2627 = CARTESIAN_POINT ( 'NONE',  ( -74.99999999999998579, 50.00000000000000000, -12.00000000000000000 ) ) ;
#2628 = DIRECTION ( 'NONE',  ( -1.000000000000000000, 0.000000000000000000, 0.000000000000000000 ) ) ;
#2629 = DIRECTION ( 'NONE',  ( -0.000000000000000000, -1.000000000000000000, -0.000000000000000000 ) ) ;
#2630 =( GEOMETRIC_REPRESENTATION_CONTEXT ( 3 ) GLOBAL_UNCERTAINTY_ASSIGNED_CONTEXT ( ( #43168 ) ) GLOBAL_UNIT_ASSIGNED_CONTEXT ( ( #37204, #58613, #41428 ) ) REPRESENTATION_CONTEXT ( 'NONE', 'WORKASPACE' ) );
#2631 =( GEOMETRIC_REPRESENTATION_CONTEXT ( 3 ) GLOBAL_UNCERTAINTY_ASSIGNED_CONTEXT ( ( #31951 ) ) GLOBAL_UNIT_ASSIGNED_CONTEXT ( ( #5223, #43608, #49546 ) ) REPRESENTATION_CONTEXT ( 'NONE', 'WORKASPACE' ) );
#2632 = CARTESIAN_POINT ( 'NONE',  ( -170.3070736234661524, -10.01517768586948698, 6.132527647946031529E-16 ) ) ;
#2633 = DIRECTION ( 'NONE',  ( 0.000000000000000000, -0.000000000000000000, -1.000000000000000000 ) ) ;
#2634 = CARTESIAN_POINT ( 'NONE',  ( -8.102448949553179958, 116.4949999999999761, 5.886773742842747126 ) ) ;
#2635 = CARTESIAN_POINT ( 'NONE',  ( -111.9570736234661723, 9.058813317711329915, -2.943386871421373119 ) ) ;
#2636 = CARTESIAN_POINT ( 'NONE',  ( -183.2030253043162702, 3.561627562078368392, -8.644815131452912027 ) ) ;
#2637 = DIRECTION ( 'NONE',  ( -0.000000000000000000, -1.000000000000000000, -0.000000000000000000 ) ) ;
#2638 = ORIENTED_EDGE ( 'NONE', *, *, #36605, .F. ) ;
#2639 = CARTESIAN_POINT ( 'NONE',  ( 5.196152422706628471, -1.107695154586738173, -9.000000000000005329 ) ) ;
#2640 = DIRECTION ( 'NONE',  ( 0.000000000000000000, 0.000000000000000000, 1.000000000000000000 ) ) ;
#2641 = FACE_OUTER_BOUND ( 'NONE', #31961, .T. ) ;
#2642 = PRESENTATION_STYLE_ASSIGNMENT (( #40020 ) ) ;
#2643 = COLOUR_RGB ( '', 0.08235294, 0.09019608, 0.10196078) ;
#2644 = CARTESIAN_POINT ( 'NONE',  ( -153.2049999999999272, -2.607480562269071545, -8.024999999999991473 ) ) ;
#2645 = CARTESIAN_POINT ( 'NONE',  ( 0.000000000000000000, -2.500000000000000000, 0.000000000000000000 ) ) ;
#2646 = CARTESIAN_POINT ( 'NONE',  ( -8.425330761298491566, 111.4667181716287132, -1.555325770122464979 ) ) ;
#2647 = EDGE_CURVE ( 'NONE', #65093, #44423, #32397, .T. ) ;
#2648 = CARTESIAN_POINT ( 'NONE',  ( -167.5449999999999875, -7.632228543268600340, -2.479861379858950166 ) ) ;
#2649 = VECTOR ( 'NONE', #36470, 1000.000000000000000 ) ;
#2650 = CARTESIAN_POINT ( 'NONE',  ( -152.6949999999999932, -8.437984349512086979, 5.166775262442717831E-16 ) ) ;
#2651 = B_SPLINE_CURVE_WITH_KNOTS ( 'NONE', 3,
 ( #33285, #22037, #64604, #32943, #43540, #49469, #16778, #65633 ),
 .UNSPECIFIED., .F., .F.,
 ( 4, 2, 2, 4 ),
 ( 2.544316211733585141E-07, 0.002094919859796805575, 0.003142252573884622441, 0.004189585287972440175 ),
 .UNSPECIFIED. ) ;
#2652 = ORIENTED_EDGE ( 'NONE', *, *, #68224, .F. ) ;
#2653 = DIRECTION ( 'NONE',  ( 0.000000000000000000, 0.000000000000000000, -1.000000000000000000 ) ) ;
#2654 = PRESENTATION_STYLE_ASSIGNMENT (( #57556 ) ) ;
#2655 = CARTESIAN_POINT ( 'NONE',  ( -122.2429263765338021, 5.598654528085804216, 7.705886871421366635 ) ) ;
#2656 = CARTESIAN_POINT ( 'NONE',  ( -72.80499999999997840, -8.437984349512085203, 5.166775262442717831E-16 ) ) ;
#2657 = LINE ( 'NONE', #45310, #16914 ) ;
#2658 =( LENGTH_UNIT ( ) NAMED_UNIT ( * ) SI_UNIT ( .MILLI., .METRE. ) );
#2659 = AXIS2_PLACEMENT_3D ( 'NONE', #51438, #18396, #39884 ) ;
#2660 = EDGE_CURVE ( 'NONE', #9513, #6729, #35254, .T. ) ;
#2661 = CARTESIAN_POINT ( 'NONE',  ( -73.04499999999998749, 7.632228543268600340, 2.479861379858949277 ) ) ;
#2662 = CARTESIAN_POINT ( 'NONE',  ( 9.058813317711337021, 142.6549999999999727, 2.943386871421375783 ) ) ;
#2663 = LINE ( 'NONE', #6943, #5056 ) ;
#2664 = LINE ( 'NONE', #29064, #57048 ) ;
#2665 =( GEOMETRIC_REPRESENTATION_CONTEXT ( 3 ) GLOBAL_UNCERTAINTY_ASSIGNED_CONTEXT ( ( #20848 ) ) GLOBAL_UNIT_ASSIGNED_CONTEXT ( ( #64198, #49430, #55014 ) ) REPRESENTATION_CONTEXT ( 'NONE', 'WORKASPACE' ) );
#2666 = FACE_OUTER_BOUND ( 'NONE', #24215, .T. ) ;
#2667 = DIRECTION ( 'NONE',  ( 0.000000000000000000, 0.000000000000000000, 1.000000000000000000 ) ) ;
#2668 = PRESENTATION_LAYER_ASSIGNMENT (  '', '', ( #55485 ) ) ;
#2669 = LINE ( 'NONE', #25209, #37108 ) ;
#2670 = CARTESIAN_POINT ( 'NONE',  ( -195.0000000000000000, 0.000000000000000000, 9.524999999999991473 ) ) ;
#2671 = EDGE_CURVE ( 'NONE', #60077, #44927, #34143, .T. ) ;
#2672 = CIRCLE ( 'NONE', #38727, 0.5000000000000004441 ) ;
#2673 = DIRECTION ( 'NONE',  ( -1.000000000000000000, -1.156482317317870344E-15, 0.000000000000000000 ) ) ;
#2674 = CARTESIAN_POINT ( 'NONE',  ( -70.87837837837835764, 13.70805908423324482, -10.00000000000000000 ) ) ;
#2675 = FILL_AREA_STYLE ('',( #55489 ) ) ;
#2676 = EDGE_LOOP ( 'NONE', ( #9878, #47349, #46477, #2010 ) ) ;
#2677 = VERTEX_POINT ( 'NONE', #54885 ) ;
#2678 = CIRCLE ( 'NONE', #42109, 0.2500000000000002220 ) ;
#2679 = DIRECTION ( 'NONE',  ( 1.156482317317873451E-16, 1.000000000000000000, -0.000000000000000000 ) ) ;
#2680 = CARTESIAN_POINT ( 'NONE',  ( -132.5070736234661410, 8.102448949553176405, 5.886773742842740909 ) ) ;
#2681 = CARTESIAN_POINT ( 'NONE',  ( 1.000000000000000000, 36.99999999999999289, 3.750000000000000000 ) ) ;
#2682 = VERTEX_POINT ( 'NONE', #16283 ) ;
#2683 = ORIENTED_EDGE ( 'NONE', *, *, #22324, .T. ) ;
#2684 = PRESENTATION_STYLE_ASSIGNMENT (( #41435 ) ) ;
#2685 = SURFACE_STYLE_USAGE ( .BOTH. , #24508 ) ;
#2686 = VECTOR ( 'NONE', #230, 1000.000000000000000 ) ;
#2687 = ORIENTED_EDGE ( 'NONE', *, *, #8457, .T. ) ;
#2688 = CARTESIAN_POINT ( 'NONE',  ( 2.999999999999997335, 0.000000000000000000, 72.00402776293822171 ) ) ;
#2689 = VERTEX_POINT ( 'NONE', #21512 ) ;
#2690 = MECHANICAL_DESIGN_GEOMETRIC_PRESENTATION_REPRESENTATION (  '', ( #37647 ), #21893 ) ;
#2691 = CARTESIAN_POINT ( 'NONE',  ( 15.98999599679679839, 146.4999999999999716, 7.500000000000000000 ) ) ;
#2692 =( BOUNDED_CURVE ( )  B_SPLINE_CURVE ( 3, ( #69229, #57268, #4843, #21027 ),
 .UNSPECIFIED., .F., .F. ) 
 B_SPLINE_CURVE_WITH_KNOTS ( ( 4, 4 ),
 ( 4.712388980384689674, 6.283185307179586232 ),
 .UNSPECIFIED. ) 
 CURVE ( )  GEOMETRIC_REPRESENTATION_ITEM ( )  RATIONAL_B_SPLINE_CURVE ( ( 1.000000000000000000, 0.8047378541243649375, 0.8047378541243649375, 1.000000000000000000 ) ) 
 REPRESENTATION_ITEM ( '' )  );
#2693 = CARTESIAN_POINT ( 'NONE',  ( 23.71231517720798010, 117.9999999999999716, -7.500000000000000000 ) ) ;
#2694 = CARTESIAN_POINT ( 'NONE',  ( -112.1949999999999932, 8.437984349512085203, -1.550032578732815448E-15 ) ) ;
#2695 = ORIENTED_EDGE ( 'NONE', *, *, #39851, .T. ) ;
#2696 = COLOUR_RGB ( '', 0.72549020, 0.75294118, 0.79215686) ;
#2697 = CARTESIAN_POINT ( 'NONE',  ( -6.408284378168763062, 110.4999999999999858, -7.060458185319238744 ) ) ;
#2698 = DIRECTION ( 'NONE',  ( -0.000000000000000000, -1.000000000000000000, -0.000000000000000000 ) ) ;
#2699 = CARTESIAN_POINT ( 'NONE',  ( -10.00805068894159788, -11.99663851293724548, -0.3286071531843878235 ) ) ;
#2700 = CARTESIAN_POINT ( 'NONE',  ( -180.0570736234661808, 0.000000000000000000, 9.524999999999991473 ) ) ;
#2701 = CIRCLE ( 'NONE', #20736, 13.99999999999999822 ) ;
#2702 = ORIENTED_EDGE ( 'NONE', *, *, #38026, .F. ) ;
#2703 = CARTESIAN_POINT ( 'NONE',  ( -7.632228543268608334, 141.8429263765338249, 2.479861379858952830 ) ) ;
#2704 = CARTESIAN_POINT ( 'NONE',  ( -28.74999999999999645, -13.99999999999999822, 15.00000000000000178 ) ) ;
#2705 = LINE ( 'NONE', #8392, #4009 ) ;
#2706 = AXIS2_PLACEMENT_3D ( 'NONE', #61530, #13358, #56272 ) ;
#2707 = SURFACE_STYLE_USAGE ( .BOTH. , #45362 ) ;
#2708 = ORIENTED_EDGE ( 'NONE', *, *, #14870, .F. ) ;
#2709 = CARTESIAN_POINT ( 'NONE',  ( -123.0570736234661808, 0.000000000000000000, 9.524999999999991473 ) ) ;
#2710 = EDGE_LOOP ( 'NONE', ( #13803, #11245, #54789, #8873, #61232, #35732 ) ) ;
#2711 =( NAMED_UNIT ( * ) PLANE_ANGLE_UNIT ( ) SI_UNIT ( $, .RADIAN. ) );
#2712 =( LENGTH_UNIT ( ) NAMED_UNIT ( * ) SI_UNIT ( .MILLI., .METRE. ) );
#2713 = CARTESIAN_POINT ( 'NONE',  ( -20.46171737063436424, 114.7896496367841479, 10.31361660310133033 ) ) ;
#2714 = DIRECTION ( 'NONE',  ( -0.000000000000000000, 1.000000000000000000, -0.000000000000000000 ) ) ;
#2715 = CARTESIAN_POINT ( 'NONE',  ( -135.2050000000000125, -2.607480562269071545, -8.024999999999991473 ) ) ;
#2716 = DIRECTION ( 'NONE',  ( -1.000000000000000000, 0.000000000000000000, 0.000000000000000000 ) ) ;
#2717 = EDGE_LOOP ( 'NONE', ( #49165, #24446, #55591, #38167 ) ) ;
#2718 = AXIS2_PLACEMENT_3D ( 'NONE', #10242, #30983, #56065 ) ;
#2719 = CIRCLE ( 'NONE', #65677, 0.5000000000000004441 ) ;
#2720 = LINE ( 'NONE', #7685, #14959 ) ;
#2721 = CARTESIAN_POINT ( 'NONE',  ( 57.74999999999998579, 30.99999999999999289, 3.750000000000000000 ) ) ;
#2722 = DIRECTION ( 'NONE',  ( -1.000000000000000000, 0.000000000000000000, 0.000000000000000000 ) ) ;
#2723 = VERTEX_POINT ( 'NONE', #43030 ) ;
#2724 = ORIENTED_EDGE ( 'NONE', *, *, #40458, .T. ) ;
#2725 = CARTESIAN_POINT ( 'NONE',  ( -20.99028635741426640, 114.7785533247281933, 10.00000000000000000 ) ) ;
#2726 = DIRECTION ( 'NONE',  ( 1.000000000000000000, 0.000000000000000000, 0.000000000000000000 ) ) ;
#2728 = CARTESIAN_POINT ( 'NONE',  ( -48.05499999999998550, -9.827790563157499189E-16, -8.024999999999991473 ) ) ;
#2727 = CIRCLE ( 'NONE', #57874, 0.5000000000000004441 ) ;
#2729 = ORIENTED_EDGE ( 'NONE', *, *, #162, .F. ) ;
#2730 = FACE_OUTER_BOUND ( 'NONE', #20690, .T. ) ;
#2731 = CARTESIAN_POINT ( 'NONE',  ( -180.8050000000000068, -8.437984349512085203, 5.166775262442717831E-16 ) ) ;
#2732 = CARTESIAN_POINT ( 'NONE',  ( -91.49292637653378790, -8.102448949553174629, 5.886773742842742685 ) ) ;
#2733 = ADVANCED_FACE ( 'NONE', ( #65468 ), #49647, .T. ) ;
#2734 = CARTESIAN_POINT ( 'NONE',  ( -54.05707362346618083, 0.000000000000000000, 9.524999999999991473 ) ) ;
#2735 = PRESENTATION_LAYER_ASSIGNMENT (  '', '', ( #24114 ) ) ;
#2736 = CIRCLE ( 'NONE', #54488, 23.00000000000000000 ) ;
#2737 = CARTESIAN_POINT ( 'NONE',  ( -24.21231517720798010, 112.9999999999999858, -7.000000000000000000 ) ) ;
#2739 = EDGE_CURVE ( 'NONE', #32017, #48200, #64779, .T. ) ;
#2738 = EDGE_LOOP ( 'NONE', ( #13558, #7318, #46143, #48998 ) ) ;
#2740 = FILL_AREA_STYLE ('',( #19654 ) ) ;
#2741 = DIRECTION ( 'NONE',  ( 1.000000000000000000, 0.000000000000000000, 0.000000000000000000 ) ) ;
#2742 = CARTESIAN_POINT ( 'NONE',  ( -104.1549999999999869, 7.632228543268600340, 2.479861379858949277 ) ) ;
#2743 = CARTESIAN_POINT ( 'NONE',  ( -27.42382197899661733, -8.499999999999996447, 0.9999999970521835646 ) ) ;
#2744 = FILL_AREA_STYLE ('',( #55199 ) ) ;
#2745 = FACE_OUTER_BOUND ( 'NONE', #54559, .T. ) ;
#2746 = EDGE_CURVE ( 'NONE', #65704, #55073, #10961, .T. ) ;
#2747 = VECTOR ( 'NONE', #17503, 1000.000000000000114 ) ;
#2748 = EDGE_CURVE ( 'NONE', #31048, #55582, #65577, .T. ) ;
#2749 = CARTESIAN_POINT ( 'NONE',  ( -103.7949999999999733, 2.607480562269069324, -8.024999999999993250 ) ) ;
#2750 = CARTESIAN_POINT ( 'NONE',  ( -3.094860106618432471, 119.7049999999999983, -9.525000000000000355 ) ) ;
#2751 = CARTESIAN_POINT ( 'NONE',  ( -66.89499999999996760, 6.826472737025116366, 4.959722759717898555 ) ) ;
#2752 = ADVANCED_FACE ( 'NONE', ( #51031 ), #40152, .T. ) ;
#2753 = FACE_OUTER_BOUND ( 'NONE', #8256, .T. ) ;
#2754 = AXIS2_PLACEMENT_3D ( 'NONE', #7842, #23677, #45537 ) ;
#2755 = EDGE_CURVE ( 'NONE', #48114, #618, #45393, .T. ) ;
#2756 = CARTESIAN_POINT ( 'NONE',  ( 22.75000000000000711, 34.24999999999999289, -3.750000000000000000 ) ) ;
#2757 = PRESENTATION_LAYER_ASSIGNMENT (  '', '', ( #3931 ) ) ;
#2758 = DIRECTION ( 'NONE',  ( 0.000000000000000000, 0.000000000000000000, -1.000000000000000000 ) ) ;
#2759 = EDGE_LOOP ( 'NONE', ( #42495, #46925, #52957, #46942 ) ) ;
#2760 = EDGE_CURVE ( 'NONE', #4579, #2313, #53252, .T. ) ;
#2761 = CARTESIAN_POINT ( 'NONE',  ( -118.6429263765337936, -5.598654528085801552, 7.705886871421367523 ) ) ;
#2762 = TOROIDAL_SURFACE ( 'NONE', #42179, 0.7500000000000000000, 0.2500000000000000000 ) ;
#2763 = CARTESIAN_POINT ( 'NONE',  ( -133.6449999999999818, 4.716976649647091513, -6.492361379858946790 ) ) ;
#2764 =( NAMED_UNIT ( * ) PLANE_ANGLE_UNIT ( ) SI_UNIT ( $, .RADIAN. ) );
#2765 = CARTESIAN_POINT ( 'NONE',  ( -195.0000000000000000, 0.000000000000000000, 0.000000000000000000 ) ) ;
#2767 = CARTESIAN_POINT ( 'NONE',  ( 57.00000000000000000, 5.000000000000000000, -60.00402776293827145 ) ) ;
#2766 = DIRECTION ( 'NONE',  ( 0.000000000000000000, 0.000000000000000000, 1.000000000000000000 ) ) ;
#2768 = DIRECTION ( 'NONE',  ( 1.000000000000000000, 0.000000000000000000, 0.000000000000000000 ) ) ;
#2769 = ORIENTED_EDGE ( 'NONE', *, *, #5693, .F. ) ;
#2770 = VERTEX_POINT ( 'NONE', #66144 ) ;
#2771 = CARTESIAN_POINT ( 'NONE',  ( -63.29292637653380638, 3.094860106618428031, -9.524999999999993250 ) ) ;
#2772 = MECHANICAL_DESIGN_GEOMETRIC_PRESENTATION_REPRESENTATION (  '', ( #5066 ), #19632 ) ;
#2773 = DIRECTION ( 'NONE',  ( 1.000000000000000000, 0.000000000000000000, 0.000000000000000000 ) ) ;
#2774 = CARTESIAN_POINT ( 'NONE',  ( -97.70707362346722391, -3.094860106636044605, -9.524999999987192822 ) ) ;
#2775 = DIRECTION ( 'NONE',  ( 0.000000000000000000, 0.000000000000000000, 1.000000000000000000 ) ) ;
#2776 = VERTEX_POINT ( 'NONE', #28853 ) ;
#2777 = CARTESIAN_POINT ( 'NONE',  ( -128.3050000000000068, 8.437984349512086979, -1.550032578732815448E-15 ) ) ;
#2778 = EDGE_LOOP ( 'NONE', ( #37636, #65071, #57160, #39172 ) ) ;
#2779 = AXIS2_PLACEMENT_3D ( 'NONE', #48093, #16068, #16753 ) ;
#2780 = DIRECTION ( 'NONE',  ( 0.000000000000000000, 0.000000000000000000, -1.000000000000000000 ) ) ;
#2781 = CARTESIAN_POINT ( 'NONE',  ( -121.2570736234661695, 5.598654528085800663, -7.705886871421367523 ) ) ;
#2782 = VERTEX_POINT ( 'NONE', #35190 ) ;
#2783 = CARTESIAN_POINT ( 'NONE',  ( -172.6429263765338078, -5.598654528085801552, 7.705886871421367523 ) ) ;
#2784 = ORIENTED_EDGE ( 'NONE', *, *, #31129, .F. ) ;
#2785 = CIRCLE ( 'NONE', #14085, 1.000000000000000888 ) ;
#2786 = CIRCLE ( 'NONE', #42212, 2.000000000000003553 ) ;
#2787 = DIRECTION ( 'NONE',  ( -0.000000000000000000, -0.000000000000000000, 1.000000000000000000 ) ) ;
#2788 = CARTESIAN_POINT ( 'NONE',  ( -9.058813317711337021, 140.0449999999999875, -2.943386871421374895 ) ) ;
#2789 = FACE_OUTER_BOUND ( 'NONE', #52188, .T. ) ;
#2790 = VERTEX_POINT ( 'NONE', #55246 ) ;
#2791 = FACE_OUTER_BOUND ( 'NONE', #4912, .T. ) ;
#2792 = CARTESIAN_POINT ( 'NONE',  ( -1.166476076187854022E-15, 142.0549999999999784, 9.525000000000000355 ) ) ;
#2793 = CARTESIAN_POINT ( 'NONE',  ( 41.00000000735874295, 108.0041655766031425, -3.104053578549443415 ) ) ;
#2794 = ORIENTED_EDGE ( 'NONE', *, *, #18808, .F. ) ;
#2795 = CARTESIAN_POINT ( 'NONE',  ( 7.632228543268607446, 113.0429263765338135, 2.479861379858954606 ) ) ;
#2796 = FILL_AREA_STYLE_COLOUR ( '', #43601 ) ;
#2797 = PRESENTATION_STYLE_ASSIGNMENT (( #55255 ) ) ;
#2798 = FILL_AREA_STYLE ('',( #46134 ) ) ;
#2799 = AXIS2_PLACEMENT_3D ( 'NONE', #29274, #54960, #56013 ) ;
#2800 = FACE_OUTER_BOUND ( 'NONE', #50340, .T. ) ;
#2801 = ORIENTED_EDGE ( 'NONE', *, *, #54854, .T. ) ;
#2802 = CIRCLE ( 'NONE', #6201, 1.999999999999998224 ) ;
#2803 = FACE_OUTER_BOUND ( 'NONE', #44040, .T. ) ;
#2804 = VERTEX_POINT ( 'NONE', #23586 ) ;
#2805 = CARTESIAN_POINT ( 'NONE',  ( 57.00000000000000000, 14.00000000000000000, 79.00402776293826435 ) ) ;
#2806 = B_SPLINE_CURVE_WITH_KNOTS ( 'NONE', 3,
 ( #38700, #924, #61140, #49919, #60101, #12947 ),
 .UNSPECIFIED., .F., .F.,
 ( 4, 2, 4 ),
 ( 0.005386537104126974673, 0.008060814333094815098, 0.01073509156206265379 ),
 .UNSPECIFIED. ) ;
#2807 = CARTESIAN_POINT ( 'NONE',  ( -31.52128483857211094, -8.189042938456932319, -1.771464601026943919 ) ) ;
#2808 = LINE ( 'NONE', #67563, #45317 ) ;
#2809 = CARTESIAN_POINT ( 'NONE',  ( -162.2049999999999557, -2.607480562269071545, -8.024999999999991473 ) ) ;
#2810 = ORIENTED_EDGE ( 'NONE', *, *, #53401, .T. ) ;
#2811 = VECTOR ( 'NONE', #8473, 1000.000000000000000 ) ;
#2812 =( BOUNDED_CURVE ( )  B_SPLINE_CURVE ( 2, ( #56066, #50808, #39939, #45893, #8251, #8595, #62396, #3249, #29693, #24737, #24399 ),
 .UNSPECIFIED., .F., .F. ) 
 B_SPLINE_CURVE_WITH_KNOTS ( ( 3, 2, 2, 2, 2, 3 ),
 ( 0.1847826086956477487, 0.1869565217391259693, 0.1891304347826041621, 0.1913043478260823549, 0.1934782608695605477, 0.1956521739130387683 ),
 .UNSPECIFIED. ) 
 CURVE ( )  GEOMETRIC_REPRESENTATION_ITEM ( )  RATIONAL_B_SPLINE_CURVE ( ( 1.000000000000099254, 0.9510565162950540552, 1.000000000000000000, 0.9510565162951535312, 1.000000000000000000, 0.9510565162951535312, 1.000000000000000000, 0.9510565162951535312, 1.000000000000000000, 0.9510565162952597795, 0.9999999999998937517 ) ) 
 REPRESENTATION_ITEM ( '' )  );
#2813 =( LENGTH_UNIT ( ) NAMED_UNIT ( * ) SI_UNIT ( .MILLI., .METRE. ) );
#2814 = ORIENTED_EDGE ( 'NONE', *, *, #32988, .T. ) ;
#2815 = ORIENTED_EDGE ( 'NONE', *, *, #6946, .T. ) ;
#2816 = DIRECTION ( 'NONE',  ( 0.000000000000000000, 0.000000000000000000, -1.000000000000000000 ) ) ;
#2817 = CARTESIAN_POINT ( 'NONE',  ( 25.75000000000001066, 21.99999999999998224, 4.000000000000000000 ) ) ;
#2818 = CARTESIAN_POINT ( 'NONE',  ( -72.65499999999998693, -7.632228543268600340, -2.479861379858950166 ) ) ;
#2819 = ORIENTED_EDGE ( 'NONE', *, *, #2572, .F. ) ;
#2820 = ADVANCED_FACE ( 'NONE', ( #18674 ), #17653, .T. ) ;
#2821 = CARTESIAN_POINT ( 'NONE',  ( 32.00000000000000000, 15.00000000000000000, -79.00402776293826435 ) ) ;
#2822 = EDGE_CURVE ( 'NONE', #26425, #26262, #16209, .T. ) ;
#2823 = CARTESIAN_POINT ( 'NONE',  ( 53.24999999999999289, 27.74999999999998579, -3.750000000000000000 ) ) ;
#2824 = EDGE_CURVE ( 'NONE', #8197, #4422, #36457, .T. ) ;
#2825 = STYLED_ITEM ( 'NONE', ( #2642 ), #8523 ) ;
#2826 = CARTESIAN_POINT ( 'NONE',  ( -74.15754429128251957, 9.151528339695955694, -6.292049778185740294 ) ) ;
#2827 = VERTEX_POINT ( 'NONE', #45450 ) ;
#2828 = CARTESIAN_POINT ( 'NONE',  ( -32.56443198605217049, -8.762778093183483108, -2.500000000007921219 ) ) ;
#2830 =( NAMED_UNIT ( * ) PLANE_ANGLE_UNIT ( ) SI_UNIT ( $, .RADIAN. ) );
#2829 = DIRECTION ( 'NONE',  ( -1.000000000000000000, -1.156482317317873451E-16, 0.000000000000000000 ) ) ;
#2831 = AXIS2_PLACEMENT_3D ( 'NONE', #35817, #51649, #8735 ) ;
#2832 = CARTESIAN_POINT ( 'NONE',  ( 5.598654528085805993, 135.2450000000000045, 7.705886871421374629 ) ) ;
#2833 = CARTESIAN_POINT ( 'NONE',  ( -107.8449999999999989, -7.632228543268599452, 2.479861379858951054 ) ) ;
#2834 = EDGE_CURVE ( 'NONE', #55052, #54990, #66869, .T. ) ;
#2835 = VECTOR ( 'NONE', #68851, 1000.000000000000000 ) ;
#2836 = CARTESIAN_POINT ( 'NONE',  ( -0.000000000000000000, 8.270287287112621792E-15, -12.50000000000000000 ) ) ;
#2838 = CARTESIAN_POINT ( 'NONE',  ( 36.00000000000002842, 0.000000000000000000, 32.00402776293825724 ) ) ;
#2837 = CARTESIAN_POINT ( 'NONE',  ( 61.74999999999998579, 31.24999999999999289, 4.000000000000000000 ) ) ;
#2839 = ADVANCED_FACE ( 'NONE', ( #2791 ), #24281, .T. ) ;
#2840 = CARTESIAN_POINT ( 'NONE',  ( -139.6429263765338078, -5.598654528085801552, 7.705886871421367523 ) ) ;
#2841 = FILL_AREA_STYLE ('',( #34893 ) ) ;
#2842 = CARTESIAN_POINT ( 'NONE',  ( -171.1449999999999818, -4.716976649647092401, 6.492361379858946790 ) ) ;
#2843 = AXIS2_PLACEMENT_3D ( 'NONE', #6701, #60503, #7423 ) ;
#2844 = CARTESIAN_POINT ( 'NONE',  ( 0.000000000000000000, 154.4258142642185305, -9.450814264218562855 ) ) ;
#2845 = AXIS2_PLACEMENT_3D ( 'NONE', #31993, #32333, #53784 ) ;
#2846 = VERTEX_POINT ( 'NONE', #41198 ) ;
#2847 = LINE ( 'NONE', #61604, #4711 ) ;
#2848 = VERTEX_POINT ( 'NONE', #47533 ) ;
#2849 = CARTESIAN_POINT ( 'NONE',  ( -15.48999599679679662, 146.4999999999999716, 7.500000000000000000 ) ) ;
#2850 = DIRECTION ( 'NONE',  ( -0.000000000000000000, -0.000000000000000000, -1.000000000000000000 ) ) ;
#2851 = DIRECTION ( 'NONE',  ( 0.000000000000000000, 0.000000000000000000, 1.000000000000000000 ) ) ;
#2852 = EDGE_LOOP ( 'NONE', ( #11947, #41861, #63495, #26806, #53757, #4081, #31832, #17738, #18764, #20242, #34660, #31018, #42870, #39980, #1127, #53447, #37758, #60704 ) ) ;
#2853 = CARTESIAN_POINT ( 'NONE',  ( -156.3549999999999898, -4.716976649647093289, -6.492361379858945902 ) ) ;
#2854 = ORIENTED_EDGE ( 'NONE', *, *, #44010, .T. ) ;
#2855 = DIRECTION ( 'NONE',  ( -0.000000000000000000, 0.000000000000000000, -1.000000000000000000 ) ) ;
#2856 = DIRECTION ( 'NONE',  ( -1.387778780781444413E-14, 1.000000000000000000, 0.000000000000000000 ) ) ;
#2857 = ORIENTED_EDGE ( 'NONE', *, *, #58792, .F. ) ;
#2858 = SURFACE_SIDE_STYLE ('',( #46569 ) ) ;
#2859 = CARTESIAN_POINT ( 'NONE',  ( -57.35707362346617799, 5.598654528085804216, 7.705886871421366635 ) ) ;
#2860 = CARTESIAN_POINT ( 'NONE',  ( -3.094860106618432471, 115.5949999999999704, -9.525000000000000355 ) ) ;
#2861 = EDGE_CURVE ( 'NONE', #64044, #34249, #64483, .T. ) ;
#2862 =( REPRESENTATION_RELATIONSHIP ('NONE','NONE', #5102, #60355 ) REPRESENTATION_RELATIONSHIP_WITH_TRANSFORMATION ( #410 )SHAPE_REPRESENTATION_RELATIONSHIP( ) );
#2863 = MECHANICAL_DESIGN_GEOMETRIC_PRESENTATION_REPRESENTATION (  '', ( #40012 ), #62461 ) ;
#2864 = ORIENTED_EDGE ( 'NONE', *, *, #23515, .F. ) ;
#2865 = DIRECTION ( 'NONE',  ( 0.000000000000000000, 0.000000000000000000, 1.000000000000000000 ) ) ;
#2866 = CYLINDRICAL_SURFACE ( 'NONE', #18162, 0.2500000000000002220 ) ;
#2867 = CARTESIAN_POINT ( 'NONE',  ( -70.40499999999998693, -2.607480562269069768, 8.024999999999991473 ) ) ;
#2868 = CARTESIAN_POINT ( 'NONE',  ( -7.632228543268608334, 121.9570736234661723, 2.479861379858952830 ) ) ;
#2869 = ORIENTED_EDGE ( 'NONE', *, *, #33273, .F. ) ;
#2870 = CARTESIAN_POINT ( 'NONE',  ( -10.01517768586949231, 138.3049999999999500, -6.132527647946036459E-16 ) ) ;
#2871 = FACE_OUTER_BOUND ( 'NONE', #48118, .T. ) ;
#2872 = SURFACE_SIDE_STYLE ('',( #38864 ) ) ;
#2873 = DIRECTION ( 'NONE',  ( -0.000000000000000000, -0.000000000000000000, -1.000000000000000000 ) ) ;
#2874 = DIRECTION ( 'NONE',  ( -1.000000000000000000, 0.000000000000000000, 0.000000000000000000 ) ) ;
#2875 = AXIS2_PLACEMENT_3D ( 'NONE', #27722, #39041, #38705 ) ;
#2876 = ORIENTED_EDGE ( 'NONE', *, *, #7350, .T. ) ;
#2877 = AXIS2_PLACEMENT_3D ( 'NONE', #8329, #2640, #39313 ) ;
#2878 =( NAMED_UNIT ( * ) SI_UNIT ( $, .STERADIAN. ) SOLID_ANGLE_UNIT ( ) );
#2879 = CARTESIAN_POINT ( 'NONE',  ( -51.74499999999998323, 4.716976649647094177, 6.492361379858945902 ) ) ;
#2880 = ORIENTED_EDGE ( 'NONE', *, *, #2609, .F. ) ;
#2881 =( NAMED_UNIT ( * ) SI_UNIT ( $, .STERADIAN. ) SOLID_ANGLE_UNIT ( ) );
#2882 = CARTESIAN_POINT ( 'NONE',  ( -86.39292637653379359, 8.102448949553176405, 5.886773742842740909 ) ) ;
#2883 = FACE_OUTER_BOUND ( 'NONE', #45645, .T. ) ;
#2884 = ORIENTED_EDGE ( 'NONE', *, *, #9795, .T. ) ;
#2885 = CARTESIAN_POINT ( 'NONE',  ( -48.89499999999999602, 6.826472737025115478, 4.959722759717899443 ) ) ;
#2886 =( NAMED_UNIT ( * ) SI_UNIT ( $, .STERADIAN. ) SOLID_ANGLE_UNIT ( ) );
#2887 = ORIENTED_EDGE ( 'NONE', *, *, #37565, .F. ) ;
#2888 = EDGE_CURVE ( 'NONE', #1408, #37840, #67854, .T. ) ;
#2889 = AXIS2_PLACEMENT_3D ( 'NONE', #18890, #29088, #40063 ) ;
#2890 =( NAMED_UNIT ( * ) PLANE_ANGLE_UNIT ( ) SI_UNIT ( $, .RADIAN. ) );
#2891 = CARTESIAN_POINT ( 'NONE',  ( -108.3549999999999898, -4.716976649647093289, -6.492361379858945902 ) ) ;
#2892 = ORIENTED_EDGE ( 'NONE', *, *, #13497, .F. ) ;
#2893 = EDGE_CURVE ( 'NONE', #47886, #63234, #31635, .T. ) ;
#2894 = CARTESIAN_POINT ( 'NONE',  ( 45.00000000000000000, 10.69371294336137801, 4.000000000000000000 ) ) ;
#2895 = DIRECTION ( 'NONE',  ( 0.000000000000000000, 1.000000000000000000, 0.000000000000000000 ) ) ;
#2896 = CIRCLE ( 'NONE', #11931, 0.2500000000000002220 ) ;
#2897 = CARTESIAN_POINT ( 'NONE',  ( -139.1070736234661354, 8.102448949553171076, -5.886773742842744461 ) ) ;
#2898 = PLANE ( 'NONE',  #53034 ) ;
#2899 = CARTESIAN_POINT ( 'NONE',  ( -10.01517768586949408, 140.1949999999999932, -6.132527647946036459E-16 ) ) ;
#2900 = CIRCLE ( 'NONE', #15197, 1.000000000000000000 ) ;
#2901 = CARTESIAN_POINT ( 'NONE',  ( -88.70707362346615810, -3.094860106618431139, -9.524999999999991473 ) ) ;
#2902 = EDGE_CURVE ( 'NONE', #51817, #35442, #52771, .T. ) ;
#2903 = SURFACE_STYLE_USAGE ( .BOTH. , #8247 ) ;
#2904 = EDGE_CURVE ( 'NONE', #31954, #32384, #62599, .T. ) ;
#2906 = LINE ( 'NONE', #68038, #65066 ) ;
#2905 = CARTESIAN_POINT ( 'NONE',  ( 7.632228543268608334, 120.4570736234661723, -2.479861379858951942 ) ) ;
#2907 = CARTESIAN_POINT ( 'NONE',  ( -120.9549999999999983, -7.632228543268599452, 2.479861379858951054 ) ) ;
#2908 = CARTESIAN_POINT ( 'NONE',  ( 0.000000000000000000, 112.4449999999999932, -9.525000000000000355 ) ) ;
#2909 = CARTESIAN_POINT ( 'NONE',  ( -135.4449999999999932, 0.000000000000000000, 8.024999999999991473 ) ) ;
#2910 = ADVANCED_FACE ( 'NONE', ( #57332 ), #48801, .T. ) ;
#2911 = CARTESIAN_POINT ( 'NONE',  ( -119.5449999999999875, -7.632228543268600340, -2.479861379858950166 ) ) ;
#2912 = DIRECTION ( 'NONE',  ( 0.000000000000000000, 1.000000000000000000, 0.000000000000000000 ) ) ;
#2913 = EDGE_LOOP ( 'NONE', ( #66712, #54153, #48643, #45274, #50930, #55390, #8155, #51464 ) ) ;
#2914 = CARTESIAN_POINT ( 'NONE',  ( 60.00000000000000000, 1.797044900979284448E-15, 6.999999999999999112 ) ) ;
#2915 = PRESENTATION_STYLE_ASSIGNMENT (( #12821 ) ) ;
#2916 =( NAMED_UNIT ( * ) PLANE_ANGLE_UNIT ( ) SI_UNIT ( $, .RADIAN. ) );
#2917 = EDGE_CURVE ( 'NONE', #66309, #53684, #21443, .T. ) ;
#2918 = CARTESIAN_POINT ( 'NONE',  ( -170.8429263765337964, 9.058813317711329915, -2.943386871421373119 ) ) ;
#2919 = CARTESIAN_POINT ( 'NONE',  ( -46.79499999999996618, 2.607480562269068880, -8.024999999999993250 ) ) ;
#2920 = AXIS2_PLACEMENT_3D ( 'NONE', #22129, #48557, #21424 ) ;
#2921 =( NAMED_UNIT ( * ) SI_UNIT ( $, .STERADIAN. ) SOLID_ANGLE_UNIT ( ) );
#2922 = COLOUR_RGB ( '', 0.72549020, 0.75294118, 0.79215686) ;
#2923 = CARTESIAN_POINT ( 'NONE',  ( -48.50000000000000000, 14.49137674618942562, 7.500000000000000000 ) ) ;
#2924 = ORIENTED_EDGE ( 'NONE', *, *, #57553, .F. ) ;
#2925 = PRODUCT_DEFINITION_CONTEXT ( 'detailed design', #24878, 'design' ) ;
#2926 = CARTESIAN_POINT ( 'NONE',  ( -89.09292637653379643, 3.094860106618433360, 9.524999999999991473 ) ) ;
#2927 = DIRECTION ( 'NONE',  ( -1.000000000000000000, 0.000000000000000000, 0.000000000000000000 ) ) ;
#2928 = DIRECTION ( 'NONE',  ( 0.000000000000000000, 1.000000000000000000, -0.000000000000000000 ) ) ;
#2929 = CARTESIAN_POINT ( 'NONE',  ( 57.00000000000000000, 16.00000000000000000, 47.50402776293824303 ) ) ;
#2930 = CARTESIAN_POINT ( 'NONE',  ( 9.250000000000003553, 27.74999999999998934, 3.750000000000000000 ) ) ;
#2931 = CARTESIAN_POINT ( 'NONE',  ( -41.05030025768335378, 107.9631293162025116, 3.671816393059857297 ) ) ;
#2932 =( GEOMETRIC_REPRESENTATION_CONTEXT ( 3 ) GLOBAL_UNCERTAINTY_ASSIGNED_CONTEXT ( ( #67918 ) ) GLOBAL_UNIT_ASSIGNED_CONTEXT ( ( #11817, #56828, #56108 ) ) REPRESENTATION_CONTEXT ( 'NONE', 'WORKASPACE' ) );
#2933 = DIRECTION ( 'NONE',  ( 1.000000000000000000, 0.000000000000000000, 0.000000000000000000 ) ) ;
#2934 = VERTEX_POINT ( 'NONE', #35552 ) ;
#2935 = CARTESIAN_POINT ( 'NONE',  ( 82.09357085539578236, 0.000000000000000000, 37.00402776293825724 ) ) ;
#2936 = DIRECTION ( 'NONE',  ( -0.000000000000000000, -1.000000000000000000, -0.000000000000000000 ) ) ;
#2937 = ORIENTED_EDGE ( 'NONE', *, *, #25977, .T. ) ;
#2938 = CARTESIAN_POINT ( 'NONE',  ( -2.607480562268991608, 134.4070736234661467, 8.025000000000060751 ) ) ;
#2939 = CARTESIAN_POINT ( 'NONE',  ( 7.632228543268607446, 138.1570736234661467, 2.479861379858954606 ) ) ;
#2940 = EDGE_CURVE ( 'NONE', #40236, #53491, #32997, .T. ) ;
#2941 = VERTEX_POINT ( 'NONE', #43623 ) ;
#2942 =( LENGTH_UNIT ( ) NAMED_UNIT ( * ) SI_UNIT ( .MILLI., .METRE. ) );
#2943 =( LENGTH_UNIT ( ) NAMED_UNIT ( * ) SI_UNIT ( .MILLI., .METRE. ) );
#2944 = DIRECTION ( 'NONE',  ( -0.000000000000000000, -1.000000000000000000, -0.000000000000000000 ) ) ;
#2945 = VERTEX_POINT ( 'NONE', #48207 ) ;
#2946 = SURFACE_SIDE_STYLE ('',( #57147 ) ) ;
#2947 = DIRECTION ( 'NONE',  ( 0.000000000000000000, 1.000000000000000000, 0.000000000000000000 ) ) ;
#2948 = CARTESIAN_POINT ( 'NONE',  ( -9.827790563157511022E-16, 149.5570736234661524, 8.025000000000000355 ) ) ;
#2949 = FILL_AREA_STYLE ('',( #51205 ) ) ;
#2950 = DIRECTION ( 'NONE',  ( 0.000000000000000000, 1.000000000000000000, 0.000000000000000000 ) ) ;
#2951 = CARTESIAN_POINT ( 'NONE',  ( -79.49499999999999034, 6.826472737025113702, -4.959722759717902107 ) ) ;
#2952 = ORIENTED_EDGE ( 'NONE', *, *, #15800, .F. ) ;
#2953 = EDGE_CURVE ( 'NONE', #57008, #55963, #47675, .T. ) ;
#2954 = DIRECTION ( 'NONE',  ( -0.000000000000000000, 0.000000000000000000, 1.000000000000000000 ) ) ;
#2955 = LINE ( 'NONE', #35726, #35257 ) ;
#2956 = UNCERTAINTY_MEASURE_WITH_UNIT (LENGTH_MEASURE( 1.000000000000000082E-05 ), #69313, 'distance_accuracy_value', 'NONE');
#2957 = ORIENTED_EDGE ( 'NONE', *, *, #45632, .F. ) ;
#2958 = DIRECTION ( 'NONE',  ( 1.000000000000000000, 0.000000000000000000, 0.000000000000000000 ) ) ;
#2959 = CIRCLE ( 'NONE', #11958, 5.500000000000005329 ) ;
#2960 = EDGE_CURVE ( 'NONE', #38702, #26603, #25417, .T. ) ;
#2961 = DIRECTION ( 'NONE',  ( -1.156482317317873451E-16, -1.000000000000000000, 0.000000000000000000 ) ) ;
#2962 = CARTESIAN_POINT ( 'NONE',  ( -48.14292637653380780, 5.598654528085800663, -7.705886871421367523 ) ) ;
#2963 = ORIENTED_EDGE ( 'NONE', *, *, #15183, .T. ) ;
#2964 = ADVANCED_FACE ( 'NONE', ( #58725 ), #37882, .F. ) ;
#2965 = DIRECTION ( 'NONE',  ( -1.000000000000000000, 0.000000000000000000, 0.000000000000000000 ) ) ;
#2966 = EDGE_LOOP ( 'NONE', ( #64750, #1328, #2638, #29923 ) ) ;
#2967 = PRESENTATION_LAYER_ASSIGNMENT (  '', '', ( #51337 ) ) ;
#2968 =( LENGTH_UNIT ( ) NAMED_UNIT ( * ) SI_UNIT ( .MILLI., .METRE. ) );
#2969 = CARTESIAN_POINT ( 'NONE',  ( -170.1570736234661751, -9.058813317711329915, -2.943386871421370898 ) ) ;
#2970 = LINE ( 'NONE', #13217, #67983 ) ;
#2971 = CARTESIAN_POINT ( 'NONE',  ( 3.094860106618431583, 114.0949999999999704, 9.525000000000000355 ) ) ;
#2972 = CARTESIAN_POINT ( 'NONE',  ( -117.9570736234661723, 9.058813317711329915, -2.943386871421373119 ) ) ;
#2973 =( NAMED_UNIT ( * ) PLANE_ANGLE_UNIT ( ) SI_UNIT ( $, .RADIAN. ) );
#2974 = EDGE_CURVE ( 'NONE', #9284, #61460, #32667, .T. ) ;
#2975 = CARTESIAN_POINT ( 'NONE',  ( 22.25000000000000711, 33.99999999999999289, 3.750000000000000000 ) ) ;
#2976 = EDGE_LOOP ( 'NONE', ( #50392, #12873, #60251, #31713 ) ) ;
#2977 = CARTESIAN_POINT ( 'NONE',  ( 2.607480562269107072, 122.7929263765338135, -8.024999999999979039 ) ) ;
#2978 = FILL_AREA_STYLE ('',( #48844 ) ) ;
#2979 = ADVANCED_FACE ( 'NONE', ( #11218 ), #43971, .T. ) ;
#2981 = CARTESIAN_POINT ( 'NONE',  ( -114.3570736234661780, 5.598654528085804216, 7.705886871421366635 ) ) ;
#2980 = CARTESIAN_POINT ( 'NONE',  ( -74.99999999999998579, 50.00000000000000000, -6.999999999999988454 ) ) ;
#2982 = CARTESIAN_POINT ( 'NONE',  ( -145.7050000000000125, 2.607480562269073321, 8.024999999999991473 ) ) ;
#2983 = CARTESIAN_POINT ( 'NONE',  ( -8.458988388480607412, 111.4970379835461642, -1.154793543936462719 ) ) ;
#2984 = CARTESIAN_POINT ( 'NONE',  ( -163.6449999999999818, 4.716976649647091513, -6.492361379858946790 ) ) ;
#2985 = CARTESIAN_POINT ( 'NONE',  ( -144.5949999999999989, 2.607480562269072433, 8.024999999999991473 ) ) ;
#2986 = ORIENTED_EDGE ( 'NONE', *, *, #11354, .F. ) ;
#2987 = CARTESIAN_POINT ( 'NONE',  ( -195.0000000000000000, 0.000000000000000000, 0.000000000000000000 ) ) ;
#2988 = CARTESIAN_POINT ( 'NONE',  ( 2.999999999999990230, 5.000000000000000000, 37.00402776293829277 ) ) ;
#2989 =( NAMED_UNIT ( * ) PLANE_ANGLE_UNIT ( ) SI_UNIT ( $, .RADIAN. ) );
#2990 = CARTESIAN_POINT ( 'NONE',  ( -63.80499999999998550, -8.437984349512085203, 5.166775262442717831E-16 ) ) ;
#2991 = DIRECTION ( 'NONE',  ( 0.000000000000000000, 0.000000000000000000, 1.000000000000000000 ) ) ;
#2992 = CARTESIAN_POINT ( 'NONE',  ( -63.44499999999998607, 0.000000000000000000, 8.024999999999991473 ) ) ;
#2993 = CARTESIAN_POINT ( 'NONE',  ( -1.166476076187854022E-15, 151.0550000000000068, 9.525000000000000355 ) ) ;
#2994 = EDGE_CURVE ( 'NONE', #48545, #1748, #42584, .T. ) ;
#2995 = DIRECTION ( 'NONE',  ( 0.000000000000000000, 0.000000000000000000, 1.000000000000000000 ) ) ;
#2996 = SURFACE_SIDE_STYLE ('',( #19915 ) ) ;
#2997 = EDGE_CURVE ( 'NONE', #6242, #36469, #28621, .T. ) ;
#2998 = UNCERTAINTY_MEASURE_WITH_UNIT (LENGTH_MEASURE( 1.000000000000000082E-05 ), #60919, 'distance_accuracy_value', 'NONE');
#2999 = CARTESIAN_POINT ( 'NONE',  ( -159.0570736234661808, 0.000000000000000000, 9.524999999999991473 ) ) ;
#3000 = CARTESIAN_POINT ( 'NONE',  ( -20.35445791815277161, 114.9981483343694748, -10.00000000000000000 ) ) ;
#3001 =( NAMED_UNIT ( * ) SI_UNIT ( $, .STERADIAN. ) SOLID_ANGLE_UNIT ( ) );
#3002 =( LENGTH_UNIT ( ) NAMED_UNIT ( * ) SI_UNIT ( .MILLI., .METRE. ) );
#3003 = STYLED_ITEM ( 'NONE', ( #56201 ), #58599 ) ;
#3004 = PRESENTATION_LAYER_ASSIGNMENT (  '', '', ( #26591 ) ) ;
#3005 = CARTESIAN_POINT ( 'NONE',  ( 20.71231517720797655, 149.4999999999999716, 10.00000000000000000 ) ) ;
#3006 = CIRCLE ( 'NONE', #7583, 1.000000000000000000 ) ;
#3007 = SURFACE_SIDE_STYLE ('',( #13967 ) ) ;
#3008 = CARTESIAN_POINT ( 'NONE',  ( -3.542344102440325049, -1.863645424029197750, -9.000000000000007105 ) ) ;
#3009 = EDGE_LOOP ( 'NONE', ( #30945, #2323, #43, #57017 ) ) ;
#3010 = ORIENTED_EDGE ( 'NONE', *, *, #4675, .F. ) ;
#3011 = FILL_AREA_STYLE ('',( #57222 ) ) ;
#3012 =( LENGTH_UNIT ( ) NAMED_UNIT ( * ) SI_UNIT ( .MILLI., .METRE. ) );
#3013 = AXIS2_PLACEMENT_3D ( 'NONE', #53654, #48429, #21647 ) ;
#3014 =( NAMED_UNIT ( * ) PLANE_ANGLE_UNIT ( ) SI_UNIT ( $, .RADIAN. ) );
#3015 = ORIENTED_EDGE ( 'NONE', *, *, #20735, .F. ) ;
#3016 = ORIENTED_EDGE ( 'NONE', *, *, #4801, .T. ) ;
#3017 = CARTESIAN_POINT ( 'NONE',  ( -60.00000000000000000, -2.024042244987997205E-14, -10.49999999999999822 ) ) ;
#3018 = AXIS2_PLACEMENT_3D ( 'NONE', #1300, #11569, #22478 ) ;
#3019 = ORIENTED_EDGE ( 'NONE', *, *, #4682, .F. ) ;
#3020 = LINE ( 'NONE', #61796, #33270 ) ;
#3021 = VERTEX_POINT ( 'NONE', #49215 ) ;
#3022 = ADVANCED_FACE ( 'NONE', ( #11915 ), #26353, .F. ) ;
#3023 = DIRECTION ( 'NONE',  ( 0.000000000000000000, 1.000000000000000000, -0.000000000000000000 ) ) ;
#3024 = CARTESIAN_POINT ( 'NONE',  ( -115.1949999999999932, 8.437984349512085203, -1.550032578732815448E-15 ) ) ;
#3025 = EDGE_LOOP ( 'NONE', ( #63297, #33534, #67926 ) ) ;
#3026 = FACE_OUTER_BOUND ( 'NONE', #44690, .T. ) ;
#3027 = CARTESIAN_POINT ( 'NONE',  ( -12.76760319936551724, -11.13076769754811757, 4.486084945087644549 ) ) ;
#3028 = EDGE_CURVE ( 'NONE', #20287, #33218, #57843, .T. ) ;
#3029 = CARTESIAN_POINT ( 'NONE',  ( -74.50000000000000000, 9.708372675170620525, 6.000000000000000888 ) ) ;
#3030 = ORIENTED_EDGE ( 'NONE', *, *, #16573, .T. ) ;
#3031 = CARTESIAN_POINT ( 'NONE',  ( -7.632228543268607446, 147.5429263765338135, -2.479861379858953718 ) ) ;
#3032 = SURFACE_STYLE_USAGE ( .BOTH. , #40756 ) ;
#3033 = PRESENTATION_STYLE_ASSIGNMENT (( #51290 ) ) ;
#3034 = EDGE_CURVE ( 'NONE', #50390, #3561, #49916, .T. ) ;
#3035 = FILL_AREA_STYLE_COLOUR ( '', #17701 ) ;
#3036 = ORIENTED_EDGE ( 'NONE', *, *, #57249, .T. ) ;
#3037 = LINE ( 'NONE', #56559, #58847 ) ;
#3038 = ORIENTED_EDGE ( 'NONE', *, *, #2760, .T. ) ;
#3039 = DIRECTION ( 'NONE',  ( -1.000000000000000000, 0.000000000000000000, 0.000000000000000000 ) ) ;
#3040 = CARTESIAN_POINT ( 'NONE',  ( -8.437984349512095861, 139.8070736234661524, -5.166775262442723748E-16 ) ) ;
#3041 = CARTESIAN_POINT ( 'NONE',  ( 45.50000000000000000, 10.69371294336137801, 10.00000000000000000 ) ) ;
#3042 = CARTESIAN_POINT ( 'NONE',  ( -126.3549999999999898, -4.716976649647093289, -6.492361379858945902 ) ) ;
#3043 = CARTESIAN_POINT ( 'NONE',  ( -60.00000000000000000, -2.024042244987997205E-14, 6.500000000000000000 ) ) ;
#3044 = DIRECTION ( 'NONE',  ( -1.000000000000000000, 0.000000000000000000, -3.469446951953611033E-15 ) ) ;
#3045 = ORIENTED_EDGE ( 'NONE', *, *, #30476, .F. ) ;
#3046 = FACE_OUTER_BOUND ( 'NONE', #3461, .T. ) ;
#3047 = STYLED_ITEM ( 'NONE', ( #13235 ), #67261 ) ;
#3048 = DIRECTION ( 'NONE',  ( -1.000000000000000000, 0.000000000000000000, 0.000000000000000000 ) ) ;
#3049 = DIRECTION ( 'NONE',  ( -0.000000000000000000, -0.000000000000000000, 1.000000000000000000 ) ) ;
#3050 = DIRECTION ( 'NONE',  ( 0.000000000000000000, 0.000000000000000000, -1.000000000000000000 ) ) ;
#3051 = ORIENTED_EDGE ( 'NONE', *, *, #49380, .T. ) ;
#3052 = AXIS2_PLACEMENT_3D ( 'NONE', #32869, #6130, #446 ) ;
#3053 = EDGE_LOOP ( 'NONE', ( #20213, #28789, #746 ) ) ;
#3054 = DIRECTION ( 'NONE',  ( -1.000000000000000000, 0.000000000000000000, 0.000000000000000000 ) ) ;
#3055 = DIRECTION ( 'NONE',  ( -1.000000000000000000, -0.000000000000000000, -0.000000000000000000 ) ) ;
#3056 = EDGE_CURVE ( 'NONE', #4894, #56993, #10784, .T. ) ;
#3057 = CARTESIAN_POINT ( 'NONE',  ( 7.440601873764704166, -2.005109422339667269, 1.112499515747340073 ) ) ;
#3058 =( LENGTH_UNIT ( ) NAMED_UNIT ( * ) SI_UNIT ( .MILLI., .METRE. ) );
#3059 = ORIENTED_EDGE ( 'NONE', *, *, #39998, .T. ) ;
#3060 = FACE_OUTER_BOUND ( 'NONE', #24221, .T. ) ;
#3061 = CARTESIAN_POINT ( 'NONE',  ( -180.9550000000000125, -7.632228543268599452, 2.479861379858951054 ) ) ;
#3062 = DIRECTION ( 'NONE',  ( -1.000000000000000000, 0.000000000000000000, 0.000000000000000000 ) ) ;
#3063 = SURFACE_STYLE_FILL_AREA ( #35831 ) ;
#3064 = CARTESIAN_POINT ( 'NONE',  ( -59.75707362346617657, -5.598654528085801552, 7.705886871421367523 ) ) ;
#3065 = AXIS2_PLACEMENT_3D ( 'NONE', #62820, #58600, #48439 ) ;
#3066 = CARTESIAN_POINT ( 'NONE',  ( -176.8449999999999989, -7.632228543268599452, 2.479861379858951054 ) ) ;
#3067 = DIRECTION ( 'NONE',  ( 0.000000000000000000, 1.000000000000000000, 0.000000000000000000 ) ) ;
#3068 = VERTEX_POINT ( 'NONE', #17890 ) ;
#3069 = CARTESIAN_POINT ( 'NONE',  ( -75.00000000000002842, 35.50862325381058326, -9.555990219820042597 ) ) ;
#3070 = SURFACE_STYLE_USAGE ( .BOTH. , #52034 ) ;
#3071 = LINE ( 'NONE', #8427, #25917 ) ;
#3072 = CARTESIAN_POINT ( 'NONE',  ( -96.05499999999999261, -9.827790563157499189E-16, -8.024999999999991473 ) ) ;
#3073 = DIRECTION ( 'NONE',  ( -1.000000000000000000, 0.000000000000000000, 2.478176394252586564E-16 ) ) ;
#3074 = SURFACE_STYLE_FILL_AREA ( #51328 ) ;
#3075 = FILL_AREA_STYLE ('',( #30539 ) ) ;
#3076 = STYLED_ITEM ( 'NONE', ( #44559 ), #41344 ) ;
#3077 = CARTESIAN_POINT ( 'NONE',  ( -97.19499999999997897, 8.437984349512086979, -1.550032578732815448E-15 ) ) ;
#3078 = CARTESIAN_POINT ( 'NONE',  ( 3.094860106618431583, 115.2049999999999983, 9.525000000000000355 ) ) ;
#3079 = CARTESIAN_POINT ( 'NONE',  ( -67.19499999999999318, 8.437984349512085203, -1.550032578732815448E-15 ) ) ;
#3080 = DIRECTION ( 'NONE',  ( 0.000000000000000000, 0.000000000000000000, 1.000000000000000000 ) ) ;
#3081 = CARTESIAN_POINT ( 'NONE',  ( 3.000000000000000000, 5.000000000000000000, -72.00402776293822171 ) ) ;
#3082 = UNCERTAINTY_MEASURE_WITH_UNIT (LENGTH_MEASURE( 1.000000000000000082E-05 ), #5851, 'distance_accuracy_value', 'NONE');
#3083 = FACE_OUTER_BOUND ( 'NONE', #41325, .T. ) ;
#3084 = FILL_AREA_STYLE ('',( #8444 ) ) ;
#3085 = EDGE_LOOP ( 'NONE', ( #36467, #33112, #55177, #51059 ) ) ;
#3086 = CARTESIAN_POINT ( 'NONE',  ( -114.8929263765337936, -8.102448949553172852, -5.886773742842741797 ) ) ;
#3087 = CARTESIAN_POINT ( 'NONE',  ( -131.6949999999999932, -8.437984349512085203, 5.166775262442717831E-16 ) ) ;
#3088 = DIRECTION ( 'NONE',  ( -0.000000000000000000, 1.000000000000000000, -0.000000000000000000 ) ) ;
#3090 = SURFACE_STYLE_FILL_AREA ( #28202 ) ;
#3089 = FILL_AREA_STYLE ('',( #29885 ) ) ;
#3091 = VERTEX_POINT ( 'NONE', #6610 ) ;
#3092 = ORIENTED_EDGE ( 'NONE', *, *, #23206, .T. ) ;
#3093 =( BOUNDED_SURFACE ( )  B_SPLINE_SURFACE ( 3, 2, ( 
 ( #49399, #1831, #1125 ),
 ( #23340, #59583, #28236 ),
 ( #6810, #16716, #49082 ),
 ( #27895, #768, #33556 ),
 ( #55707, #12426, #34251 ),
 ( #54655, #7176, #43802 ),
 ( #6458, #22660, #44166 ),
 ( #65562, #66247, #11749 ),
 ( #18074, #17413, #54308 ),
 ( #38180, #32870, #48744 ),
 ( #38877, #22306, #33887 ),
 ( #60287, #27207, #65211 ),
 ( #17062, #38541, #59933 ),
 ( #54985, #49746, #1484 ),
 ( #23013, #65913, #55354 ),
 ( #13129, #46594, #57085 ),
 ( #24712, #40239, #13471 ),
 ( #3580, #19087, #8908 ) ),
 .UNSPECIFIED., .F., .F., .F. ) 
 B_SPLINE_SURFACE_WITH_KNOTS ( ( 4, 2, 2, 2, 2, 2, 2, 2, 4 ),
 ( 3, 3 ),
 ( 0.0008275086428995113161, 0.0009765612317269591579, 0.001125613820554406891, 0.001274666409381854625, 0.001423718998209302358, 0.001721824175864198041, 0.002019929353519093508, 0.002616139708828884441, 0.003212350064138675809 ),
 ( 0.000000000000000000, 1.000000000000000000 ),
 .UNSPECIFIED. ) 
 GEOMETRIC_REPRESENTATION_ITEM ( )  RATIONAL_B_SPLINE_SURFACE ( (
 ( 1.000000000000000000, 0.2907356542125085763, 1.000000000000000000),
 ( 1.000000000000000000, 0.2907339171234460951, 1.000000000000000000),
 ( 1.000000000000000000, 0.2933218126491319855, 1.000000000000000000),
 ( 1.000000000000000000, 0.3027174795994745371, 1.000000000000000000),
 ( 1.000000000000000000, 0.3096405143333968435, 1.000000000000000000),
 ( 1.000000000000000000, 0.3258903432231445296, 1.000000000000000000),
 ( 1.000000000000000000, 0.3352112554373404829, 1.000000000000000000),
 ( 1.000000000000000000, 0.3552330613602922571, 1.000000000000000000),
 ( 1.000000000000000000, 0.3657822831406245534, 1.000000000000000000),
 ( 1.000000000000000000, 0.3977110304218586800, 1.000000000000000000),
 ( 1.000000000000000000, 0.4197187326554602249, 1.000000000000000000),
 ( 1.000000000000000000, 0.4623670587026428302, 1.000000000000000000),
 ( 1.000000000000000000, 0.4829316641227516249, 1.000000000000000000),
 ( 1.000000000000000000, 0.5424860661042875121, 1.000000000000000000),
 ( 1.000000000000000000, 0.5795047887219657579, 1.000000000000000000),
 ( 1.000000000000000000, 0.6470713767465448019, 1.000000000000000000),
 ( 1.000000000000000000, 0.6780453138457507301, 1.000000000000000000),
 ( 1.000000000000000000, 0.7071067811865523467, 1.000000000000000000) ) ) 
 REPRESENTATION_ITEM ( '' )  SURFACE ( )  );
#3094 = DIRECTION ( 'NONE',  ( 1.982541115402069054E-16, 0.000000000000000000, -1.000000000000000000 ) ) ;
#3095 = LINE ( 'NONE', #35867, #10249 ) ;
#3096 = CARTESIAN_POINT ( 'NONE',  ( 3.728455551739338514, 1.573594397639262343, 7.000000000000000888 ) ) ;
#3097 = STYLED_ITEM ( 'NONE', ( #14901 ), #50902 ) ;
#3098 = CARTESIAN_POINT ( 'NONE',  ( 75.00000000000000000, 19.30628705663858469, 6.999999999999999112 ) ) ;
#3099 = AXIS2_PLACEMENT_3D ( 'NONE', #13577, #56856, #51933 ) ;
#3100 = ORIENTED_EDGE ( 'NONE', *, *, #46951, .T. ) ;
#3101 = CARTESIAN_POINT ( 'NONE',  ( -128.7549999999999955, 4.716976649647091513, -6.492361379858946790 ) ) ;
#3102 = EDGE_LOOP ( 'NONE', ( #3375, #31173, #49907, #49228 ) ) ;
#3103 = CYLINDRICAL_SURFACE ( 'NONE', #46626, 0.2500000000000002220 ) ;
#3104 = CARTESIAN_POINT ( 'NONE',  ( -126.8070736234661666, 10.01517768586948698, -1.839758294383808571E-15 ) ) ;
#3105 = ORIENTED_EDGE ( 'NONE', *, *, #44467, .T. ) ;
#3106 = DIRECTION ( 'NONE',  ( 0.000000000000000000, -1.000000000000000000, 0.000000000000000000 ) ) ;
#3107 = LINE ( 'NONE', #13366, #44515 ) ;
#3108 = ORIENTED_EDGE ( 'NONE', *, *, #10238, .T. ) ;
#3109 = ADVANCED_FACE ( 'NONE', ( #66057 ), #50590, .F. ) ;
#3110 = VECTOR ( 'NONE', #34985, 1000.000000000000000 ) ;
#3111 =( NAMED_UNIT ( * ) SI_UNIT ( $, .STERADIAN. ) SOLID_ANGLE_UNIT ( ) );
#3112 = CARTESIAN_POINT ( 'NONE',  ( 8.102448949553183510, 138.9949999999999193, -5.886773742842746238 ) ) ;
#3113 = ORIENTED_EDGE ( 'NONE', *, *, #19765, .F. ) ;
#3114 = SURFACE_STYLE_FILL_AREA ( #67196 ) ;
#3115 = CARTESIAN_POINT ( 'NONE',  ( -1.166476076187854022E-15, 136.0549999999999784, 9.525000000000000355 ) ) ;
#3116 = FACE_OUTER_BOUND ( 'NONE', #2717, .T. ) ;
#3117 = VERTEX_POINT ( 'NONE', #40396 ) ;
#3118 = CARTESIAN_POINT ( 'NONE',  ( 4.716976649647096842, 118.7429263765338163, 6.492361379858953896 ) ) ;
#3119 =( LENGTH_UNIT ( ) NAMED_UNIT ( * ) SI_UNIT ( .MILLI., .METRE. ) );
#3120 = UNCERTAINTY_MEASURE_WITH_UNIT (LENGTH_MEASURE( 1.000000000000000082E-05 ), #49416, 'distance_accuracy_value', 'NONE');
#3121 = VECTOR ( 'NONE', #54835, 1000.000000000000000 ) ;
#3122 = CARTESIAN_POINT ( 'NONE',  ( -88.34292637653381064, -9.058813317711329915, 2.943386871421371787 ) ) ;
#3123 = CARTESIAN_POINT ( 'NONE',  ( 4.000000000000030198, 43.00000000000000000, 90.00000000000000000 ) ) ;
#3124 = EDGE_CURVE ( 'NONE', #37946, #66402, #42729, .T. ) ;
#3125 = CARTESIAN_POINT ( 'NONE',  ( -22.75000000000000711, 34.24999999999999289, 4.000000000000000000 ) ) ;
#3126 = ORIENTED_EDGE ( 'NONE', *, *, #66262, .T. ) ;
#3127 = EDGE_CURVE ( 'NONE', #66584, #54496, #46755, .T. ) ;
#3128 = CARTESIAN_POINT ( 'NONE',  ( 41.16129102860539746, 107.5075374186653931, 3.372645969649438413 ) ) ;
#3129 = VERTEX_POINT ( 'NONE', #67448 ) ;
#3130 = CARTESIAN_POINT ( 'NONE',  ( -24.75000000000000355, 36.75000000000000000, 3.000000000000000000 ) ) ;
#3131 = CARTESIAN_POINT ( 'NONE',  ( 57.00000000000000000, 16.00000000000000000, 65.00402776293825013 ) ) ;
#3132 = PLANE ( 'NONE',  #13797 ) ;
#3133 = CARTESIAN_POINT ( 'NONE',  ( -161.9050000000000011, 2.607480562269068880, -8.024999999999993250 ) ) ;
#3135 = ORIENTED_EDGE ( 'NONE', *, *, #14381, .T. ) ;
#3134 = ADVANCED_FACE ( 'NONE', ( #9777 ), #19611, .T. ) ;
#3136 = UNCERTAINTY_MEASURE_WITH_UNIT (LENGTH_MEASURE( 1.000000000000000082E-05 ), #12265, 'distance_accuracy_value', 'NONE');
#3137 = EDGE_CURVE ( 'NONE', #13131, #4028, #25567, .T. ) ;
#3138 = VECTOR ( 'NONE', #57380, 1000.000000000000000 ) ;
#3139 = LINE ( 'NONE', #24631, #21766 ) ;
#3140 = CARTESIAN_POINT ( 'NONE',  ( -25.21060798583054563, 0.000000000000000000, -5.000000000000000000 ) ) ;
#3141 = CARTESIAN_POINT ( 'NONE',  ( 75.00000000000000000, 20.22733879051532568, 6.503618960537718152 ) ) ;
#3142 = DIRECTION ( 'NONE',  ( 0.000000000000000000, -1.000000000000000000, -0.000000000000000000 ) ) ;
#3143 = VERTEX_POINT ( 'NONE', #25236 ) ;
#3144 = ORIENTED_EDGE ( 'NONE', *, *, #32812, .F. ) ;
#3145 = DIRECTION ( 'NONE',  ( -1.000000000000000000, 0.000000000000000000, 0.000000000000000000 ) ) ;
#3146 = MECHANICAL_DESIGN_GEOMETRIC_PRESENTATION_REPRESENTATION (  '', ( #68382 ), #67263 ) ;
#3147 = EDGE_CURVE ( 'NONE', #33883, #8197, #15072, .T. ) ;
#3148 = LINE ( 'NONE', #46875, #56947 ) ;
#3149 = CARTESIAN_POINT ( 'NONE',  ( -71.60499999999997556, 6.826472737025113702, -4.959722759717902107 ) ) ;
#3150 = VERTEX_POINT ( 'NONE', #30492 ) ;
#3151 = DIRECTION ( 'NONE',  ( 0.000000000000000000, 0.000000000000000000, -1.000000000000000000 ) ) ;
#3152 = PRESENTATION_LAYER_ASSIGNMENT (  '', '', ( #41401 ) ) ;
#3153 = CARTESIAN_POINT ( 'NONE',  ( -91.55707362346616662, -1.166476076187852838E-15, -9.524999999999991473 ) ) ;
#3154 = LINE ( 'NONE', #61260, #60005 ) ;
#3155 = CIRCLE ( 'NONE', #64955, 0.5000000000000004441 ) ;
#3156 = CARTESIAN_POINT ( 'NONE',  ( -74.10600381765247846, 9.348666914230193470, -6.164661031308983574 ) ) ;
#3157 = ORIENTED_EDGE ( 'NONE', *, *, #17080, .T. ) ;
#3158 = DIRECTION ( 'NONE',  ( 1.000000000000000000, 0.000000000000000000, 0.000000000000000000 ) ) ;
#3159 = PRESENTATION_LAYER_ASSIGNMENT (  '', '', ( #13345 ) ) ;
#3160 = CARTESIAN_POINT ( 'NONE',  ( -53.00707362346619078, -8.102448949553174629, -5.886773742842741797 ) ) ;
#3161 = CARTESIAN_POINT ( 'NONE',  ( 8.102448949553183510, 138.9949999999999193, -5.886773742842746238 ) ) ;
#3162 = CARTESIAN_POINT ( 'NONE',  ( -97.49499999999999034, 6.826472737025113702, -4.959722759717902107 ) ) ;
#3163 = DIRECTION ( 'NONE',  ( 0.000000000000000000, 0.000000000000000000, 1.000000000000000000 ) ) ;
#3164 = STYLED_ITEM ( 'NONE', ( #69479 ), #14808 ) ;
#3165 =( NAMED_UNIT ( * ) SI_UNIT ( $, .STERADIAN. ) SOLID_ANGLE_UNIT ( ) );
#3166 = UNCERTAINTY_MEASURE_WITH_UNIT (LENGTH_MEASURE( 1.000000000000000082E-05 ), #64161, 'distance_accuracy_value', 'NONE');
#3168 = CARTESIAN_POINT ( 'NONE',  ( -71.24292637653380211, 5.598654528085804216, 7.705886871421366635 ) ) ;
#3167 = CARTESIAN_POINT ( 'NONE',  ( -97.40707362346722675, 3.094860106600815453, -9.525000000012790125 ) ) ;
#3169 = CARTESIAN_POINT ( 'NONE',  ( -146.8429263765338249, 9.058813317711329915, -2.943386871421373119 ) ) ;
#3170 =( LENGTH_UNIT ( ) NAMED_UNIT ( * ) SI_UNIT ( .MILLI., .METRE. ) );
#3171 = SURFACE_SIDE_STYLE ('',( #29963 ) ) ;
#3172 = CARTESIAN_POINT ( 'NONE',  ( -155.9949999999999761, -6.826472737025115478, 4.959722759717900331 ) ) ;
#3173 = CARTESIAN_POINT ( 'NONE',  ( 0.000000000000000000, 27.74999999999998934, 4.000000000000000000 ) ) ;
#3174 = CARTESIAN_POINT ( 'NONE',  ( -44.99999999999977263, 147.4999999999999716, -10.00000000000000000 ) ) ;
#3175 = ORIENTED_EDGE ( 'NONE', *, *, #15745, .F. ) ;
#3176 = DIRECTION ( 'NONE',  ( -0.000000000000000000, -0.000000000000000000, 1.000000000000000000 ) ) ;
#3177 = ORIENTED_EDGE ( 'NONE', *, *, #65268, .F. ) ;
#3178 = UNCERTAINTY_MEASURE_WITH_UNIT (LENGTH_MEASURE( 1.000000000000000082E-05 ), #48494, 'distance_accuracy_value', 'NONE');
#3179 = AXIS2_PLACEMENT_3D ( 'NONE', #19117, #12459, #50465 ) ;
#3180 = LINE ( 'NONE', #8540, #68655 ) ;
#3181 = CARTESIAN_POINT ( 'NONE',  ( -45.00000000000000000, 8.164117261306884643, 6.987107442241105915 ) ) ;
#3182 = CARTESIAN_POINT ( 'NONE',  ( -12.72792206135785165, 1.797044900979284448E-15, -10.00000000000000000 ) ) ;
#3183 = CARTESIAN_POINT ( 'NONE',  ( -57.11974195711956526, -8.499999999999992895, 0.06931351858043294234 ) ) ;
#3184 = CIRCLE ( 'NONE', #52726, 30.00000000000000000 ) ;
#3185 = ORIENTED_EDGE ( 'NONE', *, *, #32707, .T. ) ;
#3186 = CARTESIAN_POINT ( 'NONE',  ( -161.4549999999999841, 7.632228543268599452, -2.479861379858951942 ) ) ;
#3187 = ORIENTED_EDGE ( 'NONE', *, *, #43099, .F. ) ;
#3188 =( NAMED_UNIT ( * ) PLANE_ANGLE_UNIT ( ) SI_UNIT ( $, .RADIAN. ) );
#3189 = CARTESIAN_POINT ( 'NONE',  ( 44.99999999999977973, 146.4999999999999716, -7.500000000000000000 ) ) ;
#3190 = ORIENTED_EDGE ( 'NONE', *, *, #22261, .F. ) ;
#3191 = EDGE_CURVE ( 'NONE', #35189, #66039, #65888, .T. ) ;
#3192 = AXIS2_PLACEMENT_3D ( 'NONE', #59699, #5883, #49178 ) ;
#3193 = VECTOR ( 'NONE', #52078, 1000.000000000000000 ) ;
#3194 = PRESENTATION_STYLE_ASSIGNMENT (( #35628 ) ) ;
#3195 = CARTESIAN_POINT ( 'NONE',  ( -57.20707362346615810, 3.094860106618433360, 9.524999999999991473 ) ) ;
#3196 = CARTESIAN_POINT ( 'NONE',  ( -8.102448949553181734, 113.4949999999999619, 5.886773742842747126 ) ) ;
#3197 = ADVANCED_FACE ( 'NONE', ( #24879 ), #47442, .T. ) ;
#3198 =( BOUNDED_CURVE ( )  B_SPLINE_CURVE ( 3, ( #64947, #61730, #34664, #3312 ),
 .UNSPECIFIED., .F., .F. ) 
 B_SPLINE_CURVE_WITH_KNOTS ( ( 4, 4 ),
 ( 5.683226373146454513, 6.380992534147263306 ),
 .UNSPECIFIED. ) 
 CURVE ( )  GEOMETRIC_REPRESENTATION_ITEM ( )  RATIONAL_B_SPLINE_CURVE ( ( 1.000000000000000000, 0.9598367440515259696, 0.9598367440515259696, 1.000000000000000000 ) ) 
 REPRESENTATION_ITEM ( '' )  );
#3199 = VERTEX_POINT ( 'NONE', #36172 ) ;
#3200 = CARTESIAN_POINT ( 'NONE',  ( 0.000000000000000000, 0.000000000000000000, -4.000000000000000000 ) ) ;
#3201 = DIRECTION ( 'NONE',  ( 0.000000000000000000, 0.000000000000000000, -1.000000000000000000 ) ) ;
#3202 = CARTESIAN_POINT ( 'NONE',  ( -71.90499999999997272, 2.607480562269069324, -8.024999999999993250 ) ) ;
#3203 = SURFACE_STYLE_USAGE ( .BOTH. , #35281 ) ;
#3204 = ORIENTED_EDGE ( 'NONE', *, *, #43657, .T. ) ;
#3205 = CARTESIAN_POINT ( 'NONE',  ( 9.058813317711337021, 133.6550000000000011, 2.943386871421375783 ) ) ;
#3206 = UNCERTAINTY_MEASURE_WITH_UNIT (LENGTH_MEASURE( 1.000000000000000082E-05 ), #54167, 'distance_accuracy_value', 'NONE');
#3207 = DIRECTION ( 'NONE',  ( 0.000000000000000000, 1.000000000000000000, 0.000000000000000000 ) ) ;
#3208 = MECHANICAL_DESIGN_GEOMETRIC_PRESENTATION_REPRESENTATION (  '', ( #6660 ), #51569 ) ;
#3209 = EDGE_CURVE ( 'NONE', #53612, #18297, #46390, .T. ) ;
#3210 = CIRCLE ( 'NONE', #50420, 1.000000000000000000 ) ;
#3211 = CARTESIAN_POINT ( 'NONE',  ( 57.00000000000000000, 0.000000000000000000, -60.00402776293825724 ) ) ;
#3212 = FILL_AREA_STYLE_COLOUR ( '', #8585 ) ;
#3213 = EDGE_CURVE ( 'NONE', #3825, #17887, #14332, .T. ) ;
#3214 = DIRECTION ( 'NONE',  ( 0.000000000000000000, 0.000000000000000000, -1.000000000000000000 ) ) ;
#3215 = EDGE_LOOP ( 'NONE', ( #4979, #59371, #9381, #40862 ) ) ;
#3216 = AXIS2_PLACEMENT_3D ( 'NONE', #25, #32439, #15972 ) ;
#3217 = CYLINDRICAL_SURFACE ( 'NONE', #37402, 8.025000000000000355 ) ;
#3218 =( NAMED_UNIT ( * ) PLANE_ANGLE_UNIT ( ) SI_UNIT ( $, .RADIAN. ) );
#3219 = CARTESIAN_POINT ( 'NONE',  ( -56.39499999999997470, -6.826472737025115478, -4.959722759717899443 ) ) ;
#3220 = ORIENTED_EDGE ( 'NONE', *, *, #5520, .T. ) ;
#3221 = CARTESIAN_POINT ( 'NONE',  ( 6.598003871452727154, 111.1717662273375709, 5.909302594220223526 ) ) ;
#3222 = VECTOR ( 'NONE', #65771, 1000.000000000000227 ) ;
#3223 = CYLINDRICAL_SURFACE ( 'NONE', #18903, 5.000000000000000888 ) ;
#3224 = LINE ( 'NONE', #66967, #11706 ) ;
#3225 = ADVANCED_FACE ( 'NONE', ( #3026 ), #57241, .F. ) ;
#3226 = ORIENTED_EDGE ( 'NONE', *, *, #64346, .T. ) ;
#3227 = CYLINDRICAL_SURFACE ( 'NONE', #24188, 10.00000000000000000 ) ;
#3228 =( NAMED_UNIT ( * ) SI_UNIT ( $, .STERADIAN. ) SOLID_ANGLE_UNIT ( ) );
#3229 = ORIENTED_EDGE ( 'NONE', *, *, #40628, .F. ) ;
#3230 = AXIS2_PLACEMENT_3D ( 'NONE', #36907, #63930, #48154 ) ;
#3231 = DIRECTION ( 'NONE',  ( 0.000000000000000000, 1.000000000000000000, 0.000000000000000000 ) ) ;
#3232 = CARTESIAN_POINT ( 'NONE',  ( -105.2049999999999841, -2.607480562269071545, -8.024999999999991473 ) ) ;
#3233 = ORIENTED_EDGE ( 'NONE', *, *, #19785, .T. ) ;
#3234 = PLANE ( 'NONE',  #2464 ) ;
#3235 = MANIFOLD_SOLID_BREP ( 'Chamfer1', #16079 ) ;
#3236 = SURFACE_STYLE_FILL_AREA ( #29679 ) ;
#3237 = CARTESIAN_POINT ( 'NONE',  ( -142.5570736234661808, -1.166476076187852838E-15, -9.524999999999991473 ) ) ;
#3238 = DIRECTION ( 'NONE',  ( -0.000000000000000000, 1.000000000000000000, 0.000000000000000000 ) ) ;
#3239 = CARTESIAN_POINT ( 'NONE',  ( 9.058813317711337021, 144.5449999999999875, 2.943386871421375783 ) ) ;
#3240 = CARTESIAN_POINT ( 'NONE',  ( -76.10707362346617799, 8.102448949553171076, -5.886773742842744461 ) ) ;
#3241 = COLOUR_RGB ( '', 0.40784314, 0.44705882, 0.49803922) ;
#3242 = CARTESIAN_POINT ( 'NONE',  ( 1.000000000000000000, 42.00000000000000000, -79.00402776293826435 ) ) ;
#3243 = DIRECTION ( 'NONE',  ( 0.000000000000000000, -0.000000000000000000, 1.000000000000000000 ) ) ;
#3244 = DIRECTION ( 'NONE',  ( -0.000000000000000000, -1.000000000000000000, -0.000000000000000000 ) ) ;
#3246 =( NAMED_UNIT ( * ) SI_UNIT ( $, .STERADIAN. ) SOLID_ANGLE_UNIT ( ) );
#3245 = FACE_OUTER_BOUND ( 'NONE', #9534, .T. ) ;
#3247 = AXIS2_PLACEMENT_3D ( 'NONE', #58499, #48003, #43423 ) ;
#3248 = CARTESIAN_POINT ( 'NONE',  ( -119.3049999999999926, 8.437984349512085203, -1.550032578732815448E-15 ) ) ;
#3249 = CARTESIAN_POINT ( 'NONE',  ( -158.3929263765338078, 8.102448949553176405, 5.886773742842740909 ) ) ;
#3250 = CARTESIAN_POINT ( 'NONE',  ( 8.102448949553181734, 111.3949999999999818, 5.886773742842750679 ) ) ;
#3251 = CARTESIAN_POINT ( 'NONE',  ( -124.9450000000000074, -9.827790563157499189E-16, -8.024999999999991473 ) ) ;
#3252 = AXIS2_PLACEMENT_3D ( 'NONE', #46347, #2653, #61418 ) ;
#3253 = COLOUR_RGB ( '', 0.09019608, 0.27058824, 0.51372549) ;
#3254 = CARTESIAN_POINT ( 'NONE',  ( -117.4449999999999932, 0.000000000000000000, 8.024999999999991473 ) ) ;
#3255 = SURFACE_SIDE_STYLE ('',( #13864 ) ) ;
#3256 = VERTEX_POINT ( 'NONE', #15747 ) ;
#3257 = EDGE_CURVE ( 'NONE', #1660, #4324, #63627, .T. ) ;
#3258 = AXIS2_PLACEMENT_3D ( 'NONE', #54631, #6441, #44485 ) ;
#3259 = DIRECTION ( 'NONE',  ( 1.000000000000000000, 0.000000000000000000, 0.000000000000000000 ) ) ;
#3260 = SURFACE_STYLE_USAGE ( .BOTH. , #45902 ) ;
#3261 = CARTESIAN_POINT ( 'NONE',  ( -169.6429263765338078, -5.598654528085801552, 7.705886871421367523 ) ) ;
#3262 = CARTESIAN_POINT ( 'NONE',  ( -53.24499999999999034, -4.716976649647093289, -6.492361379858945902 ) ) ;
#3263 = CIRCLE ( 'NONE', #38149, 2.500000000000002220 ) ;
#3264 = DIRECTION ( 'NONE',  ( -0.000000000000000000, 1.000000000000000000, -0.000000000000000000 ) ) ;
#3265 = CARTESIAN_POINT ( 'NONE',  ( 15.00000000000000000, 8.000000000000000000, 4.000000000000000000 ) ) ;
#3266 = DIRECTION ( 'NONE',  ( -0.000000000000000000, 1.000000000000000000, -0.000000000000000000 ) ) ;
#3267 = ORIENTED_EDGE ( 'NONE', *, *, #52310, .T. ) ;
#3268 = CARTESIAN_POINT ( 'NONE',  ( -84.89292637653377938, -8.102448949553172852, -5.886773742842741797 ) ) ;
#3269 = CONTEXT_DEPENDENT_SHAPE_REPRESENTATION ( #43355, #19347 ) ;
#3270 = CIRCLE ( 'NONE', #41569, 1.000000000000000000 ) ;
#3271 = DIRECTION ( 'NONE',  ( 0.000000000000000000, 0.000000000000000000, 1.000000000000000000 ) ) ;
#3272 = CARTESIAN_POINT ( 'NONE',  ( 15.98999599679679839, 117.9999999999999716, 7.500000000000000000 ) ) ;
#3273 = DIRECTION ( 'NONE',  ( 0.000000000000000000, 0.000000000000000000, 1.000000000000000000 ) ) ;
#3274 = CARTESIAN_POINT ( 'NONE',  ( 4.716976649647099507, 123.7570736234661695, -6.492361379858953008 ) ) ;
#3275 =( NAMED_UNIT ( * ) SI_UNIT ( $, .STERADIAN. ) SOLID_ANGLE_UNIT ( ) );
#3276 = AXIS2_PLACEMENT_3D ( 'NONE', #38567, #1858, #55016 ) ;
#3277 = ADVANCED_FACE ( 'NONE', ( #63895 ), #26270, .T. ) ;
#3278 = ADVANCED_FACE ( 'NONE', ( #21696 ), #164, .T. ) ;
#3279 = ORIENTED_EDGE ( 'NONE', *, *, #62754, .F. ) ;
#3280 = LINE ( 'NONE', #13892, #24124 ) ;
#3281 = DIRECTION ( 'NONE',  ( 1.000000000000000000, 0.000000000000000000, 0.000000000000000000 ) ) ;
#3282 = ORIENTED_EDGE ( 'NONE', *, *, #43269, .F. ) ;
#3283 = DIRECTION ( 'NONE',  ( 0.000000000000000000, -0.000000000000000000, -1.000000000000000000 ) ) ;
#3284 = AXIS2_PLACEMENT_3D ( 'NONE', #58560, #62779, #47015 ) ;
#3285 =( GEOMETRIC_REPRESENTATION_CONTEXT ( 3 ) GLOBAL_UNCERTAINTY_ASSIGNED_CONTEXT ( ( #45416 ) ) GLOBAL_UNIT_ASSIGNED_CONTEXT ( ( #19173, #51551, #18835 ) ) REPRESENTATION_CONTEXT ( 'NONE', 'WORKASPACE' ) );
#3286 =( NAMED_UNIT ( * ) SI_UNIT ( $, .STERADIAN. ) SOLID_ANGLE_UNIT ( ) );
#3287 = CARTESIAN_POINT ( 'NONE',  ( -8.437984349512095861, 133.8070736234661808, -5.166775262442723748E-16 ) ) ;
#3288 = EDGE_CURVE ( 'NONE', #36954, #6981, #29941, .T. ) ;
#3289 = ORIENTED_EDGE ( 'NONE', *, *, #10953, .F. ) ;
#3290 = AXIS2_PLACEMENT_3D ( 'NONE', #13784, #57037, #8854 ) ;
#3291 = CARTESIAN_POINT ( 'NONE',  ( -105.6549999999999869, -7.632228543268600340, -2.479861379858950166 ) ) ;
#3292 = CARTESIAN_POINT ( 'NONE',  ( 75.00000000000000000, 19.38064346792907244, -6.520279032830151422 ) ) ;
#3293 = CYLINDRICAL_SURFACE ( 'NONE', #37630, 7.500000000000000000 ) ;
#3295 = EDGE_LOOP ( 'NONE', ( #34911, #12190, #19331, #41704 ) ) ;
#3294 = VECTOR ( 'NONE', #12988, 1000.000000000000000 ) ;
#3296 = DIRECTION ( 'NONE',  ( 1.000000000000000000, 0.000000000000000000, 0.000000000000000000 ) ) ;
#3297 = CARTESIAN_POINT ( 'NONE',  ( -105.0570736234661666, 0.000000000000000000, 9.524999999999991473 ) ) ;
#3298 = CARTESIAN_POINT ( 'NONE',  ( -28.74999999999999645, -4.000000000000000000, 11.89999999999999680 ) ) ;
#3299 = AXIS2_PLACEMENT_3D ( 'NONE', #57004, #39476, #8134 ) ;
#3300 = EDGE_CURVE ( 'NONE', #9629, #32941, #51908, .T. ) ;
#3301 = PRESENTATION_LAYER_ASSIGNMENT (  '', '', ( #13430 ) ) ;
#3302 = DIRECTION ( 'NONE',  ( -0.000000000000000000, -0.000000000000000000, -1.000000000000000000 ) ) ;
#3303 = CARTESIAN_POINT ( 'NONE',  ( -83.54499999999998749, -7.632228543268600340, -2.479861379858950166 ) ) ;
#3304 = ORIENTED_EDGE ( 'NONE', *, *, #15309, .T. ) ;
#3305 = SURFACE_STYLE_USAGE ( .BOTH. , #30407 ) ;
#3307 = EDGE_CURVE ( 'NONE', #50928, #62177, #7939, .T. ) ;
#3306 = PRESENTATION_LAYER_ASSIGNMENT (  '', '', ( #49422 ) ) ;
#3308 = ORIENTED_EDGE ( 'NONE', *, *, #16322, .F. ) ;
#3309 = PRESENTATION_STYLE_ASSIGNMENT (( #2621 ) ) ;
#3310 = FACE_BOUND ( 'NONE', #59746, .T. ) ;
#3311 = STYLED_ITEM ( 'NONE', ( #12915 ), #51621 ) ;
#3312 = CARTESIAN_POINT ( 'NONE',  ( 1.804495846578303864, 51.08602766979955589, -7.112547338523483198 ) ) ;
#3313 = DIRECTION ( 'NONE',  ( -1.000000000000000000, 1.445602896647339656E-16, 0.000000000000000000 ) ) ;
#3314 = VERTEX_POINT ( 'NONE', #33972 ) ;
#3315 = ORIENTED_EDGE ( 'NONE', *, *, #18960, .F. ) ;
#3316 = LINE ( 'NONE', #14627, #7720 ) ;
#3317 = CARTESIAN_POINT ( 'NONE',  ( -149.3929263765338078, 8.102448949553176405, 5.886773742842740909 ) ) ;
#3318 = PRESENTATION_LAYER_ASSIGNMENT (  '', '', ( #33688 ) ) ;
#3319 = CARTESIAN_POINT ( 'NONE',  ( -169.5570736234661808, -1.166476076187852838E-15, -9.524999999999991473 ) ) ;
#3320 = FILL_AREA_STYLE_COLOUR ( '', #14044 ) ;
#3321 =( GEOMETRIC_REPRESENTATION_CONTEXT ( 3 ) GLOBAL_UNCERTAINTY_ASSIGNED_CONTEXT ( ( #14394 ) ) GLOBAL_UNIT_ASSIGNED_CONTEXT ( ( #25620, #67165, #8774 ) ) REPRESENTATION_CONTEXT ( 'NONE', 'WORKASPACE' ) );
#3322 = CARTESIAN_POINT ( 'NONE',  ( 8.102448949553179958, 111.3949999999999818, 5.886773742842750679 ) ) ;
#3323 = CARTESIAN_POINT ( 'NONE',  ( -100.7070736234661581, -3.094860106618431139, -9.524999999999991473 ) ) ;
#3324 = LINE ( 'NONE', #2260, #56540 ) ;
#3325 = CARTESIAN_POINT ( 'NONE',  ( -65.75707362346616947, -5.598654528085801552, 7.705886871421367523 ) ) ;
#3326 = ORIENTED_EDGE ( 'NONE', *, *, #31759, .T. ) ;
#3327 = CIRCLE ( 'NONE', #31427, 1.000000000000000000 ) ;
#3328 =( LENGTH_UNIT ( ) NAMED_UNIT ( * ) SI_UNIT ( .MILLI., .METRE. ) );
#3329 = DIRECTION ( 'NONE',  ( -1.000000000000000000, 0.000000000000000000, 0.000000000000000000 ) ) ;
#3331 = FILL_AREA_STYLE_COLOUR ( '', #43740 ) ;
#3330 = DIRECTION ( 'NONE',  ( -0.000000000000000000, 0.000000000000000000, -1.000000000000000000 ) ) ;
#3332 = CARTESIAN_POINT ( 'NONE',  ( -148.2549999999999955, -4.716976649647092401, 6.492361379858946790 ) ) ;
#3333 = FILL_AREA_STYLE ('',( #63175 ) ) ;
#3334 = CARTESIAN_POINT ( 'NONE',  ( -166.3449999999999989, 7.632228543268599452, -2.479861379858951942 ) ) ;
#3335 = CARTESIAN_POINT ( 'NONE',  ( -145.3449999999999989, 7.632228543268599452, -2.479861379858951942 ) ) ;
#3336 = ORIENTED_EDGE ( 'NONE', *, *, #56202, .T. ) ;
#3337 = EDGE_CURVE ( 'NONE', #197, #35623, #15050, .T. ) ;
#3338 = DIRECTION ( 'NONE',  ( -0.000000000000000000, -0.000000000000000000, 1.000000000000000000 ) ) ;
#3339 = CARTESIAN_POINT ( 'NONE',  ( 24.00000000000000000, 1.000000000000000888, -3.000000000000000000 ) ) ;
#3340 = VECTOR ( 'NONE', #19065, 1000.000000000000000 ) ;
#3341 = FILL_AREA_STYLE ('',( #51584 ) ) ;
#3342 = CARTESIAN_POINT ( 'NONE',  ( -64.70499999999998408, 2.607480562269073321, 8.024999999999991473 ) ) ;
#3343 = CARTESIAN_POINT ( 'NONE',  ( 5.196152422706629359, 9.000000000000008882, 7.500000000000000000 ) ) ;
#3344 = CARTESIAN_POINT ( 'NONE',  ( -22.75000000000000711, 0.000000000000000000, 3.750000000000000000 ) ) ;
#3345 = CARTESIAN_POINT ( 'NONE',  ( -61.49499999999998323, 6.826472737025113702, -4.959722759717902107 ) ) ;
#3346 = CARTESIAN_POINT ( 'NONE',  ( 3.094860106618435136, 155.4050000000000011, -9.525000000000000355 ) ) ;
#3347 = DIRECTION ( 'NONE',  ( 0.000000000000000000, 0.000000000000000000, -1.000000000000000000 ) ) ;
#3348 = MANIFOLD_SOLID_BREP ( 'Fillet1', #25039 ) ;
#3349 = VECTOR ( 'NONE', #43656, 1000.000000000000000 ) ;
#3350 = DIRECTION ( 'NONE',  ( -1.000000000000000000, 0.000000000000000000, 0.000000000000000000 ) ) ;
#3351 = CARTESIAN_POINT ( 'NONE',  ( -23.21231517720797655, 117.4999999999999716, 9.500000000000000000 ) ) ;
#3352 = EDGE_CURVE ( 'NONE', #65582, #22419, #35622, .T. ) ;
#3353 = PRESENTATION_LAYER_ASSIGNMENT (  '', '', ( #5598 ) ) ;
#3354 = EDGE_CURVE ( 'NONE', #44052, #8864, #62559, .T. ) ;
#3355 = CARTESIAN_POINT ( 'NONE',  ( 27.99999999999999645, 5.000000000000000000, 24.00402776293821816 ) ) ;
#3356 = SURFACE_STYLE_USAGE ( .BOTH. , #63870 ) ;
#3357 = EDGE_CURVE ( 'NONE', #7095, #44000, #35835, .T. ) ;
#3358 = CARTESIAN_POINT ( 'NONE',  ( -195.0000000000000000, 0.000000000000000000, 9.524999999999991473 ) ) ;
#3359 = ADVANCED_FACE ( 'NONE', ( #38616 ), #66690, .F. ) ;
#3360 = CARTESIAN_POINT ( 'NONE',  ( -0.2278693232858696738, -2.499999999999995115, -9.000000000000007105 ) ) ;
#3361 = EDGE_LOOP ( 'NONE', ( #20498, #19017, #55925, #27193, #17474, #37527 ) ) ;
#3362 = AXIS2_PLACEMENT_3D ( 'NONE', #39768, #65429, #33750 ) ;
#3363 = EDGE_LOOP ( 'NONE', ( #20386, #63079, #68936, #44805 ) ) ;
#3364 = CARTESIAN_POINT ( 'NONE',  ( -60.35707362346616378, 5.598654528085804216, 7.705886871421366635 ) ) ;
#3365 = TOROIDAL_SURFACE ( 'NONE', #62967, 8.500000000000012434, 0.5000000000000000000 ) ;
#3366 = DIRECTION ( 'NONE',  ( 0.000000000000000000, 0.000000000000000000, 1.000000000000000000 ) ) ;
#3367 = AXIS2_PLACEMENT_3D ( 'NONE', #67779, #20268, #9750 ) ;
#3368 = EDGE_CURVE ( 'NONE', #5288, #29168, #37425, .T. ) ;
#3369 = DIRECTION ( 'NONE',  ( 1.000000000000000000, 0.000000000000000000, 0.000000000000000000 ) ) ;
#3370 = DIRECTION ( 'NONE',  ( 0.000000000000000000, -0.000000000000000000, -1.000000000000000000 ) ) ;
#3371 = EDGE_CURVE ( 'NONE', #12255, #24951, #5001, .T. ) ;
#3372 = ORIENTED_EDGE ( 'NONE', *, *, #19056, .T. ) ;
#3373 = ORIENTED_EDGE ( 'NONE', *, *, #267, .F. ) ;
#3374 = DIRECTION ( 'NONE',  ( 0.000000000000000000, -1.000000000000000000, -0.000000000000000000 ) ) ;
#3375 = ORIENTED_EDGE ( 'NONE', *, *, #21255, .T. ) ;
#3376 = CARTESIAN_POINT ( 'NONE',  ( -5.598654528085808657, 111.7549999999999955, 7.705886871421373741 ) ) ;
#3377 = DIRECTION ( 'NONE',  ( 1.000000000000000000, 0.000000000000000000, 0.000000000000000000 ) ) ;
#3378 = VERTEX_POINT ( 'NONE', #25758 ) ;
#3379 = AXIS2_PLACEMENT_3D ( 'NONE', #37250, #68886, #15431 ) ;
#3380 = B_SPLINE_CURVE_WITH_KNOTS ( 'NONE', 3,
 ( #32732, #22533, #54183, #5996, #63705, #53174, #15549, #65074 ),
 .UNSPECIFIED., .F., .F.,
 ( 4, 2, 2, 4 ),
 ( 0.007148677244982143929, 0.009235234034391179292, 0.01027851242909569654, 0.01132179082380021552 ),
 .UNSPECIFIED. ) ;
#3381 = CARTESIAN_POINT ( 'NONE',  ( -107.6949999999999932, -8.437984349512085203, 5.166775262442717831E-16 ) ) ;
#3382 = VERTEX_POINT ( 'NONE', #63739 ) ;
#3383 = CARTESIAN_POINT ( 'NONE',  ( -9.489074601111886054, 110.4999999999999574, -0.9355076952660921208 ) ) ;
#3384 = PRESENTATION_STYLE_ASSIGNMENT (( #51629 ) ) ;
#3385 = COLOUR_RGB ( '', 0.66274510, 0.83137255, 0.94901961) ;
#3386 =( NAMED_UNIT ( * ) SI_UNIT ( $, .STERADIAN. ) SOLID_ANGLE_UNIT ( ) );
#3387 = ORIENTED_EDGE ( 'NONE', *, *, #23575, .T. ) ;
#3388 = CARTESIAN_POINT ( 'NONE',  ( 6.826472737025121695, 146.4929263765338305, -4.959722759717905660 ) ) ;
#3389 = CARTESIAN_POINT ( 'NONE',  ( -53.56549681293840592, -9.954220776862749531, -2.519071624164535450 ) ) ;
#3390 =( NAMED_UNIT ( * ) PLANE_ANGLE_UNIT ( ) SI_UNIT ( $, .RADIAN. ) );
#3391 = PLANE ( 'NONE',  #63243 ) ;
#3392 = LINE ( 'NONE', #56912, #19921 ) ;
#3393 = VERTEX_POINT ( 'NONE', #18830 ) ;
#3394 = CIRCLE ( 'NONE', #18120, 0.2500000000000002220 ) ;
#3395 = DIRECTION ( 'NONE',  ( 0.000000000000000000, 1.000000000000000000, 0.000000000000000000 ) ) ;
#3396 = ORIENTED_EDGE ( 'NONE', *, *, #27909, .F. ) ;
#3397 = DIRECTION ( 'NONE',  ( 0.000000000000000000, 0.000000000000000000, -1.000000000000000000 ) ) ;
#3398 = CARTESIAN_POINT ( 'NONE',  ( 0.000000000000000000, 0.000000000000000000, 0.000000000000000000 ) ) ;
#3399 = LINE ( 'NONE', #41124, #38648 ) ;
#3400 = CARTESIAN_POINT ( 'NONE',  ( 41.16151714082911184, 107.5071857241661348, -3.372843186988511377 ) ) ;
#3401 = CARTESIAN_POINT ( 'NONE',  ( -123.0549999999999926, -9.827790563157499189E-16, -8.024999999999991473 ) ) ;
#3402 = EDGE_CURVE ( 'NONE', #46838, #22827, #41632, .T. ) ;
#3403 = CARTESIAN_POINT ( 'NONE',  ( 44.28021770739998431, 9.999999999999980460, 3.500000000000000000 ) ) ;
#3404 = CIRCLE ( 'NONE', #46176, 0.4999999999999994449 ) ;
#3405 = CARTESIAN_POINT ( 'NONE',  ( 33.00000000000000000, 13.00000000000000178, -79.00402776293826435 ) ) ;
#3406 = CARTESIAN_POINT ( 'NONE',  ( 1.000000000000000000, 14.00000000000000000, 80.00402776293826435 ) ) ;
#3407 = FACE_OUTER_BOUND ( 'NONE', #39060, .T. ) ;
#3408 = ORIENTED_EDGE ( 'NONE', *, *, #41772, .T. ) ;
#3409 = MECHANICAL_DESIGN_GEOMETRIC_PRESENTATION_REPRESENTATION (  '', ( #41664 ), #14669 ) ;
#3410 = ORIENTED_EDGE ( 'NONE', *, *, #27860, .T. ) ;
#3411 = SURFACE_STYLE_USAGE ( .BOTH. , #67479 ) ;
#3412 =( NAMED_UNIT ( * ) PLANE_ANGLE_UNIT ( ) SI_UNIT ( $, .RADIAN. ) );
#3413 = CARTESIAN_POINT ( 'NONE',  ( 57.74999999999999289, 28.24999999999998934, 4.000000000000000000 ) ) ;
#3414 =( NAMED_UNIT ( * ) SI_UNIT ( $, .STERADIAN. ) SOLID_ANGLE_UNIT ( ) );
#3415 = ORIENTED_EDGE ( 'NONE', *, *, #68452, .F. ) ;
#3416 = CARTESIAN_POINT ( 'NONE',  ( -123.6570736234661751, 9.058813317711329915, 2.943386871421369566 ) ) ;
#3417 = CARTESIAN_POINT ( 'NONE',  ( -178.7050000000000125, 2.607480562269073321, 8.024999999999991473 ) ) ;
#3418 = PRESENTATION_LAYER_ASSIGNMENT (  '', '', ( #56229 ) ) ;
#3419 = CARTESIAN_POINT ( 'NONE',  ( -54.20707362346615810, 3.094860106618433360, 9.524999999999991473 ) ) ;
#3420 = CARTESIAN_POINT ( 'NONE',  ( -172.3449999999999989, 7.632228543268599452, -2.479861379858951942 ) ) ;
#3421 = SURFACE_STYLE_FILL_AREA ( #32524 ) ;
#3422 = ORIENTED_EDGE ( 'NONE', *, *, #42909, .F. ) ;
#3423 = ORIENTED_EDGE ( 'NONE', *, *, #43191, .T. ) ;
#3424 = CARTESIAN_POINT ( 'NONE',  ( -74.50000000000000000, 36.50926243676796190, -10.00000000000000000 ) ) ;
#3425 = DIRECTION ( 'NONE',  ( -0.000000000000000000, -1.000000000000000000, -0.000000000000000000 ) ) ;
#3426 = CARTESIAN_POINT ( 'NONE',  ( -90.05499999999997840, -9.827790563157499189E-16, -8.024999999999991473 ) ) ;
#3427 = CARTESIAN_POINT ( 'NONE',  ( -88.64499999999998181, 4.716976649647091513, -6.492361379858946790 ) ) ;
#3428 = CARTESIAN_POINT ( 'NONE',  ( 0.000000000000000000, 125.5550000000000068, -9.525000000000000355 ) ) ;
#3429 = CARTESIAN_POINT ( 'NONE',  ( -69.89499999999999602, 6.826472737025116366, 4.959722759717898555 ) ) ;
#3430 = CARTESIAN_POINT ( 'NONE',  ( -48.50000000000000000, 99.99999999999992895, -7.500000000000000000 ) ) ;
#3431 =( NAMED_UNIT ( * ) PLANE_ANGLE_UNIT ( ) SI_UNIT ( $, .RADIAN. ) );
#3432 = COLOUR_RGB ( '', 0.08235294, 0.09019608, 0.10196078) ;
#3433 = SURFACE_STYLE_FILL_AREA ( #46448 ) ;
#3434 = SURFACE_STYLE_FILL_AREA ( #18642 ) ;
#3435 = FILL_AREA_STYLE ('',( #14383 ) ) ;
#3437 = VERTEX_POINT ( 'NONE', #40312 ) ;
#3436 = CONICAL_SURFACE ( 'NONE', #41741, 9.000000000000007105, 0.7853981633974500554 ) ;
#3438 = EDGE_CURVE ( 'NONE', #6055, #26070, #13551, .T. ) ;
#3439 = CARTESIAN_POINT ( 'NONE',  ( -109.9429263765338050, 0.000000000000000000, 9.524999999999991473 ) ) ;
#3440 = AXIS2_PLACEMENT_3D ( 'NONE', #26046, #42302, #31677 ) ;
#3441 = CARTESIAN_POINT ( 'NONE',  ( -125.6950000000000074, -8.437984349512085203, 5.166775262442717831E-16 ) ) ;
#3442 = SURFACE_SIDE_STYLE ('',( #30202 ) ) ;
#3443 = COLOUR_RGB ( '', 0.66274510, 0.83137255, 0.94901961) ;
#3444 = ADVANCED_FACE ( 'NONE', ( #15587 ), #35018, .F. ) ;
#3445 = PRESENTATION_STYLE_ASSIGNMENT (( #23558 ) ) ;
#3446 =( GEOMETRIC_REPRESENTATION_CONTEXT ( 3 ) GLOBAL_UNCERTAINTY_ASSIGNED_CONTEXT ( ( #58200 ) ) GLOBAL_UNIT_ASSIGNED_CONTEXT ( ( #13019, #34475, #67177 ) ) REPRESENTATION_CONTEXT ( 'NONE', 'WORKASPACE' ) );
#3448 = FACE_OUTER_BOUND ( 'NONE', #28034, .T. ) ;
#3447 = CARTESIAN_POINT ( 'NONE',  ( 2.607480562269155921, 134.7070736234661581, 8.024999999999941735 ) ) ;
#3449 = FILL_AREA_STYLE ('',( #51700 ) ) ;
#3450 = ORIENTED_EDGE ( 'NONE', *, *, #12218, .F. ) ;
#3451 = ORIENTED_EDGE ( 'NONE', *, *, #11238, .T. ) ;
#3452 = STYLED_ITEM ( 'NONE', ( #39977 ), #35029 ) ;
#3453 = DIRECTION ( 'NONE',  ( 7.709882115452441682E-16, -1.000000000000000000, 0.000000000000000000 ) ) ;
#3454 = TOROIDAL_SURFACE ( 'NONE', #40641, 2.000000000000000000, 1.000000000000000000 ) ;
#3455 = LINE ( 'NONE', #29542, #15883 ) ;
#3456 = DIRECTION ( 'NONE',  ( -2.578301549612644668E-15, -0.6691306063588581265, 0.7431448254773944662 ) ) ;
#3457 = COLOUR_RGB ( '', 0.72549020, 0.75294118, 0.79215686) ;
#3458 = CARTESIAN_POINT ( 'NONE',  ( -40.78947368421051323, 108.1536491499103505, -3.000000000000000444 ) ) ;
#3459 = CARTESIAN_POINT ( 'NONE',  ( 44.99999999999977973, 147.4999999999999716, -10.00000000000000000 ) ) ;
#3460 = EDGE_CURVE ( 'NONE', #60522, #59058, #20124, .T. ) ;
#3461 = EDGE_LOOP ( 'NONE', ( #40962, #53372, #21110, #67620 ) ) ;
#3462 = CARTESIAN_POINT ( 'NONE',  ( -134.6050000000000182, 6.826472737025113702, -4.959722759717902107 ) ) ;
#3463 = ORIENTED_EDGE ( 'NONE', *, *, #12220, .T. ) ;
#3464 = DIRECTION ( 'NONE',  ( 0.000000000000000000, 0.000000000000000000, -1.000000000000000000 ) ) ;
#3465 = CARTESIAN_POINT ( 'NONE',  ( -122.4570736234661723, -9.058813317711329915, 2.943386871421371787 ) ) ;
#3466 = ORIENTED_EDGE ( 'NONE', *, *, #46283, .T. ) ;
#3467 = CARTESIAN_POINT ( 'NONE',  ( 3.249999999999998668, 36.74999999999999289, 4.000000000000000000 ) ) ;
#3468 = ORIENTED_EDGE ( 'NONE', *, *, #24450, .F. ) ;
#3469 = CARTESIAN_POINT ( 'NONE',  ( -69.44292637653380496, -1.166476076187852838E-15, -9.524999999999991473 ) ) ;
#3470 = CARTESIAN_POINT ( 'NONE',  ( -3.094860106618432471, 136.5949999999999989, -9.525000000000000355 ) ) ;
#3471 = CYLINDRICAL_SURFACE ( 'NONE', #35134, 5.000000000000000888 ) ;
#3472 = CIRCLE ( 'NONE', #67544, 5.000000000000000000 ) ;
#3473 = EDGE_LOOP ( 'NONE', ( #49929, #11652, #43315, #4349 ) ) ;
#3474 = CARTESIAN_POINT ( 'NONE',  ( -9.058813317711337021, 147.1549999999999727, -2.943386871421374895 ) ) ;
#3475 = PRESENTATION_STYLE_ASSIGNMENT (( #62601 ) ) ;
#3476 = DIRECTION ( 'NONE',  ( 0.000000000000000000, 0.000000000000000000, 1.000000000000000000 ) ) ;
#3477 = ORIENTED_EDGE ( 'NONE', *, *, #1217, .F. ) ;
#3478 = CARTESIAN_POINT ( 'NONE',  ( -7.632228543268607446, 120.5429263765338135, -2.479861379858953718 ) ) ;
#3479 = SURFACE_SIDE_STYLE ('',( #8483 ) ) ;
#3480 = PRESENTATION_LAYER_ASSIGNMENT (  '', '', ( #46249 ) ) ;
#3481 = AXIS2_PLACEMENT_3D ( 'NONE', #9883, #62972, #14815 ) ;
#3482 = LINE ( 'NONE', #9865, #44640 ) ;
#3483 = SURFACE_SIDE_STYLE ('',( #39823 ) ) ;
#3484 = CARTESIAN_POINT ( 'NONE',  ( 16.75000000000000711, 27.74999999999998224, 3.750000000000000000 ) ) ;
#3485 = EDGE_CURVE ( 'NONE', #51168, #66608, #5270, .T. ) ;
#3486 = EDGE_LOOP ( 'NONE', ( #17034, #32502, #990, #4722 ) ) ;
#3487 = LINE ( 'NONE', #51043, #43080 ) ;
#3488 = VERTEX_POINT ( 'NONE', #57791 ) ;
#3489 = CARTESIAN_POINT ( 'NONE',  ( -56.99292637653380211, 8.102448949553171076, -5.886773742842744461 ) ) ;
#3490 = FACE_OUTER_BOUND ( 'NONE', #40124, .T. ) ;
#3492 = CARTESIAN_POINT ( 'NONE',  ( -157.4050000000000011, -2.607480562269069768, 8.024999999999991473 ) ) ;
#3491 = AXIS2_PLACEMENT_3D ( 'NONE', #49357, #65873, #28195 ) ;
#3493 = ORIENTED_EDGE ( 'NONE', *, *, #19749, .T. ) ;
#3494 = ADVANCED_FACE ( 'NONE', ( #24443 ), #36375, .F. ) ;
#3495 = CARTESIAN_POINT ( 'NONE',  ( -60.00000000000000000, -2.024042244987997205E-14, -6.000000000000000000 ) ) ;
#3496 = CARTESIAN_POINT ( 'NONE',  ( -2.607480562269116842, 152.4070736234661751, 8.024999999999970157 ) ) ;
#3497 = CARTESIAN_POINT ( 'NONE',  ( 74.99999999999998579, 19.70845863561292433, 6.466567654930966746 ) ) ;
#3498 = FILL_AREA_STYLE_COLOUR ( '', #46794 ) ;
#3499 = EDGE_LOOP ( 'NONE', ( #68926, #51810, #23620, #4841 ) ) ;
#3500 = FILL_AREA_STYLE ('',( #28615 ) ) ;
#3501 = EDGE_LOOP ( 'NONE', ( #25914, #64832, #14198, #5261 ) ) ;
#3502 =( NAMED_UNIT ( * ) PLANE_ANGLE_UNIT ( ) SI_UNIT ( $, .RADIAN. ) );
#3503 = MECHANICAL_DESIGN_GEOMETRIC_PRESENTATION_REPRESENTATION (  '', ( #107 ), #25976 ) ;
#3504 = SURFACE_STYLE_USAGE ( .BOTH. , #62979 ) ;
#3505 = CARTESIAN_POINT ( 'NONE',  ( -69.05499999999999261, -9.827790563157499189E-16, -8.024999999999991473 ) ) ;
#3506 = ORIENTED_EDGE ( 'NONE', *, *, #62830, .F. ) ;
#3507 = CARTESIAN_POINT ( 'NONE',  ( -74.99999999999998579, 50.00000000000000000, -11.50000000000000000 ) ) ;
#3508 = TOROIDAL_SURFACE ( 'NONE', #11429, 0.5000000000000000000, 0.2500000000000000000 ) ;
#3509 = MECHANICAL_DESIGN_GEOMETRIC_PRESENTATION_REPRESENTATION (  '', ( #64204 ), #53021 ) ;
#3510 = CARTESIAN_POINT ( 'NONE',  ( 0.000000000000000000, 2.500000000000000000, 0.000000000000000000 ) ) ;
#3511 = EDGE_LOOP ( 'NONE', ( #54066, #9067, #54459, #54187 ) ) ;
#3512 = VECTOR ( 'NONE', #42944, 1000.000000000000000 ) ;
#3513 = CARTESIAN_POINT ( 'NONE',  ( -75.00000000000001421, 8.253551290271408547, -5.607507417892254153 ) ) ;
#3514 =( NAMED_UNIT ( * ) PLANE_ANGLE_UNIT ( ) SI_UNIT ( $, .RADIAN. ) );
#3516 = CARTESIAN_POINT ( 'NONE',  ( -74.50000000000000000, -2.220952357103124294E-14, 10.00000000000000000 ) ) ;
#3515 = DIRECTION ( 'NONE',  ( 0.000000000000000000, -0.000000000000000000, 1.000000000000000000 ) ) ;
#3517 = AXIS2_PLACEMENT_3D ( 'NONE', #62193, #63245, #45718 ) ;
#3518 = CARTESIAN_POINT ( 'NONE',  ( 3.094860106618431583, 135.0949999999999420, 9.525000000000000355 ) ) ;
#3519 = CARTESIAN_POINT ( 'NONE',  ( -98.99499999999997613, -6.826472737025115478, 4.959722759717900331 ) ) ;
#3520 = AXIS2_PLACEMENT_3D ( 'NONE', #18700, #29229, #55972 ) ;
#3521 = EDGE_CURVE ( 'NONE', #51980, #58400, #24345, .T. ) ;
#3522 = SURFACE_STYLE_FILL_AREA ( #62315 ) ;
#3523 = DIRECTION ( 'NONE',  ( -1.000000000000000000, 0.000000000000000000, 0.000000000000000000 ) ) ;
#3524 =( BOUNDED_CURVE ( )  B_SPLINE_CURVE ( 3, ( #52022, #36575, #9455, #64282 ),
 .UNSPECIFIED., .F., .F. ) 
 B_SPLINE_CURVE_WITH_KNOTS ( ( 4, 4 ),
 ( 1.570796326794896558, 3.141592653589792228 ),
 .UNSPECIFIED. ) 
 CURVE ( )  GEOMETRIC_REPRESENTATION_ITEM ( )  RATIONAL_B_SPLINE_CURVE ( ( 1.000000000000000000, 0.8047378541243652705, 0.8047378541243652705, 1.000000000000000000 ) ) 
 REPRESENTATION_ITEM ( '' )  );
#3525 = CIRCLE ( 'NONE', #32804, 0.5000000000000004441 ) ;
#3526 = CARTESIAN_POINT ( 'NONE',  ( -41.16129102860537614, 107.5075374186653505, -3.372645969649438857 ) ) ;
#3527 = VERTEX_POINT ( 'NONE', #10639 ) ;
#3528 = CARTESIAN_POINT ( 'NONE',  ( -139.4929263765338021, -8.102448949553172852, 5.886773742842742685 ) ) ;
#3529 =( LENGTH_UNIT ( ) NAMED_UNIT ( * ) SI_UNIT ( .MILLI., .METRE. ) );
#3530 = CARTESIAN_POINT ( 'NONE',  ( -152.3950000000000102, -6.826472737025115478, -4.959722759717899443 ) ) ;
#3531 = EDGE_CURVE ( 'NONE', #65093, #64724, #48018, .T. ) ;
#3532 = PRESENTATION_STYLE_ASSIGNMENT (( #40197 ) ) ;
#3533 = DIRECTION ( 'NONE',  ( 0.000000000000000000, 0.000000000000000000, 1.000000000000000000 ) ) ;
#3534 = CARTESIAN_POINT ( 'NONE',  ( 9.827790563157511022E-16, 152.9999999999999716, -8.025000000000000355 ) ) ;
#3535 = ORIENTED_EDGE ( 'NONE', *, *, #15302, .T. ) ;
#3536 = CARTESIAN_POINT ( 'NONE',  ( -6.826472737025120807, 129.9929263765338021, 4.959722759717906548 ) ) ;
#3537 = ORIENTED_EDGE ( 'NONE', *, *, #16397, .F. ) ;
#3538 = VECTOR ( 'NONE', #10938, 1000.000000000000227 ) ;
#3539 = EDGE_CURVE ( 'NONE', #21703, #45027, #67049, .T. ) ;
#3540 = DIRECTION ( 'NONE',  ( 0.000000000000000000, 1.000000000000000000, 0.000000000000000000 ) ) ;
#3541 = EDGE_CURVE ( 'NONE', #61482, #20333, #6045, .T. ) ;
#3542 = AXIS2_PLACEMENT_3D ( 'NONE', #43351, #59111, #25457 ) ;
#3543 = SURFACE_STYLE_USAGE ( .BOTH. , #24673 ) ;
#3544 = DIRECTION ( 'NONE',  ( 0.000000000000000000, 0.000000000000000000, 1.000000000000000000 ) ) ;
#3545 = CARTESIAN_POINT ( 'NONE',  ( 0.000000000000000000, -2.500000000000000000, 0.000000000000000000 ) ) ;
#3546 = AXIS2_PLACEMENT_3D ( 'NONE', #31891, #31541, #53022 ) ;
#3547 = CARTESIAN_POINT ( 'NONE',  ( -44.99999999999977973, 147.4999999999999716, -10.00000000000000000 ) ) ;
#3548 = ADVANCED_FACE ( 'NONE', ( #64451 ), #38794, .T. ) ;
#3549 = ORIENTED_EDGE ( 'NONE', *, *, #57663, .T. ) ;
#3550 = CARTESIAN_POINT ( 'NONE',  ( -162.8050000000000068, -8.437984349512086979, 5.166775262442717831E-16 ) ) ;
#3551 = EDGE_LOOP ( 'NONE', ( #49293, #8502, #48210, #3336, #16414 ) ) ;
#3552 =( NAMED_UNIT ( * ) SI_UNIT ( $, .STERADIAN. ) SOLID_ANGLE_UNIT ( ) );
#3553 = DIRECTION ( 'NONE',  ( -0.000000000000000000, -1.000000000000000000, -0.000000000000000000 ) ) ;
#3554 = COLOUR_RGB ( '', 0.66274510, 0.83137255, 0.94901961) ;
#3555 = ORIENTED_EDGE ( 'NONE', *, *, #62642, .F. ) ;
#3556 = CARTESIAN_POINT ( 'NONE',  ( -195.0000000000000000, 0.000000000000000000, 0.000000000000000000 ) ) ;
#3557 =( GEOMETRIC_REPRESENTATION_CONTEXT ( 3 ) GLOBAL_UNCERTAINTY_ASSIGNED_CONTEXT ( ( #39128 ) ) GLOBAL_UNIT_ASSIGNED_CONTEXT ( ( #54976, #34246, #15748 ) ) REPRESENTATION_CONTEXT ( 'NONE', 'WORKASPACE' ) );
#3558 = DIRECTION ( 'NONE',  ( -0.000000000000000000, 0.9984713486292863260, 0.05527174654752588928 ) ) ;
#3559 = CARTESIAN_POINT ( 'NONE',  ( -5.598654528085806881, 109.7449999999999761, -7.705886871421374629 ) ) ;
#3560 =( GEOMETRIC_REPRESENTATION_CONTEXT ( 3 ) GLOBAL_UNCERTAINTY_ASSIGNED_CONTEXT ( ( #24246 ) ) GLOBAL_UNIT_ASSIGNED_CONTEXT ( ( #17404, #6451, #12418 ) ) REPRESENTATION_CONTEXT ( 'NONE', 'WORKASPACE' ) );
#3561 = VERTEX_POINT ( 'NONE', #27481 ) ;
#3562 = CARTESIAN_POINT ( 'NONE',  ( -57.89292637653377938, -8.102448949553174629, -5.886773742842741797 ) ) ;
#3563 = CARTESIAN_POINT ( 'NONE',  ( -5.598654528085808657, 114.7549999999999812, 7.705886871421373741 ) ) ;
#3564 = CARTESIAN_POINT ( 'NONE',  ( -71.45499999999998408, 7.632228543268599452, -2.479861379858951942 ) ) ;
#3565 = CARTESIAN_POINT ( 'NONE',  ( -80.75707362346616947, -5.598654528085801552, 7.705886871421367523 ) ) ;
#3566 = ORIENTED_EDGE ( 'NONE', *, *, #41616, .T. ) ;
#3567 = CARTESIAN_POINT ( 'NONE',  ( 8.102448949553181734, 139.5049999999999955, 5.886773742842750679 ) ) ;
#3568 = MECHANICAL_DESIGN_GEOMETRIC_PRESENTATION_REPRESENTATION (  '', ( #13702 ), #12573 ) ;
#3569 = VECTOR ( 'NONE', #13486, 1000.000000000000000 ) ;
#3570 = CARTESIAN_POINT ( 'NONE',  ( 19.89974874213239886, 114.9999999999999574, 10.00000000000001421 ) ) ;
#3571 = CARTESIAN_POINT ( 'NONE',  ( -13.25000000000000355, 28.24999999999998934, 4.000000000000000000 ) ) ;
#3572 = VERTEX_POINT ( 'NONE', #59496 ) ;
#3573 = CARTESIAN_POINT ( 'NONE',  ( -60.00000000000000000, -2.024042244987997205E-14, 12.00000000000000000 ) ) ;
#3574 = CARTESIAN_POINT ( 'NONE',  ( 29.00000000000002842, 42.00000000000000000, 89.00000000000000000 ) ) ;
#3575 = CARTESIAN_POINT ( 'NONE',  ( -179.6049999999999898, 6.826472737025113702, -4.959722759717902107 ) ) ;
#3576 = ORIENTED_EDGE ( 'NONE', *, *, #42630, .T. ) ;
#3577 = CARTESIAN_POINT ( 'NONE',  ( 6.050614363280118368, 111.1366428633864558, 6.516612769276372674 ) ) ;
#3578 = AXIS2_PLACEMENT_3D ( 'NONE', #18084, #29678, #34592 ) ;
#3579 = DIRECTION ( 'NONE',  ( -1.000000000000000000, 0.000000000000000000, 0.000000000000000000 ) ) ;
#3580 = CARTESIAN_POINT ( 'NONE',  ( -45.50000000000000000, 7.768687147774684831, -6.500000000000004441 ) ) ;
#3581 = DIRECTION ( 'NONE',  ( 0.000000000000000000, 0.000000000000000000, 1.000000000000000000 ) ) ;
#3582 = ORIENTED_EDGE ( 'NONE', *, *, #14094, .F. ) ;
#3583 = PRESENTATION_STYLE_ASSIGNMENT (( #46943 ) ) ;
#3584 = CARTESIAN_POINT ( 'NONE',  ( 8.000000000000035527, 5.000000000000000000, 77.00402776293825013 ) ) ;
#3585 = ORIENTED_EDGE ( 'NONE', *, *, #28305, .T. ) ;
#3586 = DIRECTION ( 'NONE',  ( 0.000000000000000000, 0.000000000000000000, 1.000000000000000000 ) ) ;
#3587 = CARTESIAN_POINT ( 'NONE',  ( -100.4050000000000011, -2.607480562269069768, 8.024999999999991473 ) ) ;
#3588 = EDGE_LOOP ( 'NONE', ( #421, #68397 ) ) ;
#3589 =( NAMED_UNIT ( * ) PLANE_ANGLE_UNIT ( ) SI_UNIT ( $, .RADIAN. ) );
#3590 = MANIFOLD_SOLID_BREP ( 'Fillet1', #8176 ) ;
#3591 = FACE_BOUND ( 'NONE', #53019, .T. ) ;
#3592 = CARTESIAN_POINT ( 'NONE',  ( -137.1570736234661751, -9.058813317711329915, -2.943386871421370898 ) ) ;
#3593 = AXIS2_PLACEMENT_3D ( 'NONE', #52061, #14064, #56968 ) ;
#3594 = CARTESIAN_POINT ( 'NONE',  ( 8.102448949553181734, 153.9950000000000045, -5.886773742842746238 ) ) ;
#3595 = CARTESIAN_POINT ( 'NONE',  ( -76.55707362346616662, -1.166476076187852838E-15, -9.524999999999991473 ) ) ;
#3596 = AXIS2_PLACEMENT_3D ( 'NONE', #44335, #65733, #17577 ) ;
#3597 = DIRECTION ( 'NONE',  ( 0.000000000000000000, 0.000000000000000000, -1.000000000000000000 ) ) ;
#3598 = ORIENTED_EDGE ( 'NONE', *, *, #48098, .F. ) ;
#3599 = PLANE ( 'NONE',  #2375 ) ;
#3600 = COLOUR_RGB ( '', 0.31764706, 0.68627451, 0.89019608) ;
#3602 = CARTESIAN_POINT ( 'NONE',  ( -6.062177826491069510, 2.500000000000000000, 3.499999999999999556 ) ) ;
#3601 = DIRECTION ( 'NONE',  ( -0.000000000000000000, -1.000000000000000000, -0.000000000000000000 ) ) ;
#3603 = CARTESIAN_POINT ( 'NONE',  ( -122.6049999999999898, 6.826472737025113702, -4.959722759717902107 ) ) ;
#3604 = CARTESIAN_POINT ( 'NONE',  ( -8.102448949553181734, 110.4949999999999903, 5.886773742842747126 ) ) ;
#3605 = COLOUR_RGB ( '', 0.72549020, 0.75294118, 0.79215686) ;
#3606 = CARTESIAN_POINT ( 'NONE',  ( -128.2450000000000045, -4.716976649647093289, -6.492361379858945902 ) ) ;
#3607 = ADVANCED_FACE ( 'NONE', ( #64792 ), #3969, .F. ) ;
#3608 =( GEOMETRIC_REPRESENTATION_CONTEXT ( 3 ) GLOBAL_UNCERTAINTY_ASSIGNED_CONTEXT ( ( #12330 ) ) GLOBAL_UNIT_ASSIGNED_CONTEXT ( ( #27814, #39478, #32416 ) ) REPRESENTATION_CONTEXT ( 'NONE', 'WORKASPACE' ) );
#3609 = ORIENTED_EDGE ( 'NONE', *, *, #51785, .F. ) ;
#3610 = EDGE_CURVE ( 'NONE', #58089, #67711, #1031, .T. ) ;
#3611 = MECHANICAL_DESIGN_GEOMETRIC_PRESENTATION_REPRESENTATION (  '', ( #55375 ), #35188 ) ;
#3612 =( LENGTH_UNIT ( ) NAMED_UNIT ( * ) SI_UNIT ( .MILLI., .METRE. ) );
#3614 = EDGE_CURVE ( 'NONE', #62964, #48775, #59183, .T. ) ;
#3613 = CARTESIAN_POINT ( 'NONE',  ( 0.000000000000000000, 0.000000000000000000, 7.500000000000000000 ) ) ;
#3615 = CARTESIAN_POINT ( 'NONE',  ( -75.50000000000000000, 64.49137674618943095, -6.499999999999999112 ) ) ;
#3616 = CARTESIAN_POINT ( 'NONE',  ( -173.6929263765338192, 10.01517768586948698, -1.839758294383808571E-15 ) ) ;
#3617 = FILL_AREA_STYLE ('',( #46971 ) ) ;
#3618 = CARTESIAN_POINT ( 'NONE',  ( 8.701243704650558186, -2.929003814506409675, 0.1702817813269560110 ) ) ;
#3619 = EDGE_CURVE ( 'NONE', #8149, #11591, #43045, .T. ) ;
#3620 = AXIS2_PLACEMENT_3D ( 'NONE', #44009, #15872, #65052 ) ;
#3621 = EDGE_CURVE ( 'NONE', #55506, #27751, #11165, .T. ) ;
#3622 = AXIS2_PLACEMENT_3D ( 'NONE', #41390, #30793, #19552 ) ;
#3623 = EDGE_CURVE ( 'NONE', #21703, #38944, #41935, .T. ) ;
#3624 = DIRECTION ( 'NONE',  ( 0.000000000000000000, 0.000000000000000000, 1.000000000000000000 ) ) ;
#3625 = CARTESIAN_POINT ( 'NONE',  ( 107.0858988931383777, 5.000000000000000000, -16.89933289725613363 ) ) ;
#3626 = EDGE_LOOP ( 'NONE', ( #45453, #66203, #21867, #19728, #39538, #25276 ) ) ;
#3627 = ADVANCED_FACE ( 'NONE', ( #61922 ), #29577, .F. ) ;
#3628 = CARTESIAN_POINT ( 'NONE',  ( -88.64292637653380780, -5.598654528085801552, 7.705886871421367523 ) ) ;
#3629 =( NAMED_UNIT ( * ) SI_UNIT ( $, .STERADIAN. ) SOLID_ANGLE_UNIT ( ) );
#3630 =( BOUNDED_CURVE ( )  B_SPLINE_CURVE ( 2, ( #39130, #13047, #12687, #17660, #3122, #2434, #45457, #34500, #34160, #44427, #66876 ),
 .UNSPECIFIED., .F., .F. ) 
 B_SPLINE_CURVE_WITH_KNOTS ( ( 3, 2, 2, 2, 2, 3 ),
 ( 0.6956521739130434590, 0.6978260869565217073, 0.6999999999999999556, 0.7021739130434783149, 0.7043478260869565633, 0.7065217391304348116 ),
 .UNSPECIFIED. ) 
 CURVE ( )  GEOMETRIC_REPRESENTATION_ITEM ( )  RATIONAL_B_SPLINE_CURVE ( ( 1.000000000000000000, 0.9510565162951535312, 1.000000000000000000, 0.9510565162951535312, 1.000000000000000000, 0.9510565162951535312, 1.000000000000000000, 0.9510565162951535312, 1.000000000000000000, 0.9510565162951535312, 1.000000000000000000 ) ) 
 REPRESENTATION_ITEM ( '' )  );
#3631 = CARTESIAN_POINT ( 'NONE',  ( 71.50000000000000000, 99.99999999999998579, 7.500000000000000000 ) ) ;
#3632 = COLOUR_RGB ( '', 0.66274510, 0.83137255, 0.94901961) ;
#3633 = EDGE_CURVE ( 'NONE', #27227, #18512, #29976, .T. ) ;
#3634 = COLOUR_RGB ( '', 0.72549020, 0.75294118, 0.79215686) ;
#3635 = CARTESIAN_POINT ( 'NONE',  ( -179.3929263765337794, 8.102448949553176405, 5.886773742842740909 ) ) ;
#3636 = SURFACE_SIDE_STYLE ('',( #47696 ) ) ;
#3637 = AXIS2_PLACEMENT_3D ( 'NONE', #24629, #67567, #19364 ) ;
#3638 = CARTESIAN_POINT ( 'NONE',  ( -24.21231517720798010, 117.4999999999999716, 7.500000000000000000 ) ) ;
#3639 = EDGE_LOOP ( 'NONE', ( #67182, #7617, #33295, #46023 ) ) ;
#3640 = DIRECTION ( 'NONE',  ( -1.000000000000000000, -0.000000000000000000, -0.000000000000000000 ) ) ;
#3641 = SURFACE_STYLE_FILL_AREA ( #67709 ) ;
#3642 = ORIENTED_EDGE ( 'NONE', *, *, #13104, .F. ) ;
#3643 = CARTESIAN_POINT ( 'NONE',  ( 7.566679973970428463, -2.499999999999998224, 4.894125840469273570 ) ) ;
#3644 = STYLED_ITEM ( 'NONE', ( #62191 ), #47581 ) ;
#3645 = PRESENTATION_LAYER_ASSIGNMENT (  '', '', ( #55346 ) ) ;
#3646 = CARTESIAN_POINT ( 'NONE',  ( 7.632228543268607446, 129.1570736234661467, 2.479861379858954606 ) ) ;
#3647 = FACE_OUTER_BOUND ( 'NONE', #25622, .T. ) ;
#3648 = PRESENTATION_LAYER_ASSIGNMENT (  '', '', ( #54245 ) ) ;
#3649 = ORIENTED_EDGE ( 'NONE', *, *, #32183, .F. ) ;
#3650 =( NAMED_UNIT ( * ) PLANE_ANGLE_UNIT ( ) SI_UNIT ( $, .RADIAN. ) );
#3651 = CARTESIAN_POINT ( 'NONE',  ( -102.0549999999999926, -9.827790563157499189E-16, -8.024999999999991473 ) ) ;
#3652 = COLOUR_RGB ( '', 0.31764706, 0.68627451, 0.89019608) ;
#3653 = ORIENTED_EDGE ( 'NONE', *, *, #17011, .T. ) ;
#3654 = CARTESIAN_POINT ( 'NONE',  ( -1.502314598737159031E-15, -2.500000000000000000, -9.000000000000000000 ) ) ;
#3655 = CLOSED_SHELL ( 'NONE', ( #48585, #66169, #58525, #44594, #38181, #11191 ) ) ;
#3656 = CARTESIAN_POINT ( 'NONE',  ( 1.105243736230485067E-15, 152.9999999999999716, -8.025000000000000355 ) ) ;
#3657 = CARTESIAN_POINT ( 'NONE',  ( 29.00000000000000000, 35.42594141563417054, -80.00402776293826435 ) ) ;
#3658 = ORIENTED_EDGE ( 'NONE', *, *, #60547, .T. ) ;
#3659 = AXIS2_PLACEMENT_3D ( 'NONE', #14109, #8136, #18350 ) ;
#3660 = PRESENTATION_STYLE_ASSIGNMENT (( #14607 ) ) ;
#3661 = CARTESIAN_POINT ( 'NONE',  ( -82.94499999999999318, -9.827790563157499189E-16, -8.024999999999991473 ) ) ;
#3662 = ORIENTED_EDGE ( 'NONE', *, *, #67500, .F. ) ;
#3663 = DIRECTION ( 'NONE',  ( 0.000000000000000000, 1.000000000000000000, -0.000000000000000000 ) ) ;
#3664 = EDGE_CURVE ( 'NONE', #13056, #33368, #4869, .T. ) ;
#3665 = SURFACE_STYLE_USAGE ( .BOTH. , #24444 ) ;
#3666 = DIRECTION ( 'NONE',  ( 0.000000000000000000, 0.000000000000000000, 1.000000000000000000 ) ) ;
#3667 = UNCERTAINTY_MEASURE_WITH_UNIT (LENGTH_MEASURE( 1.000000000000000082E-05 ), #15354, 'distance_accuracy_value', 'NONE');
#3668 = EDGE_LOOP ( 'NONE', ( #24495, #47254, #31737, #47537, #43305, #42607, #27015, #27738, #63125, #26671, #32245, #50776, #66537, #64016 ) ) ;
#3669 = CARTESIAN_POINT ( 'NONE',  ( 45.00000000000000000, 10.69371294336137801, 10.00000000000000000 ) ) ;
#3670 =( NAMED_UNIT ( * ) PLANE_ANGLE_UNIT ( ) SI_UNIT ( $, .RADIAN. ) );
#3671 = AXIS2_PLACEMENT_3D ( 'NONE', #44926, #845, #22387 ) ;
#3672 = AXIS2_PLACEMENT_3D ( 'NONE', #56621, #65793, #13348 ) ;
#3673 = CARTESIAN_POINT ( 'NONE',  ( 66.49999999999998579, 33.99999999999999289, 3.750000000000000000 ) ) ;
#3674 = VERTEX_POINT ( 'NONE', #3131 ) ;
#3675 = ORIENTED_EDGE ( 'NONE', *, *, #39032, .F. ) ;
#3676 = DIRECTION ( 'NONE',  ( -1.000000000000000000, 0.000000000000000000, 0.000000000000000000 ) ) ;
#3677 = CARTESIAN_POINT ( 'NONE',  ( 10.00000000000002309, 43.00000000000000000, 90.00000000000000000 ) ) ;
#3678 = CARTESIAN_POINT ( 'NONE',  ( -168.5070736234661979, 8.102448949553176405, 5.886773742842740909 ) ) ;
#3679 = DIRECTION ( 'NONE',  ( 0.7071067811865549002, 8.659560562355024070E-17, -0.7071067811865401342 ) ) ;
#3680 = CARTESIAN_POINT ( 'NONE',  ( -103.2570736234661695, 5.598654528085800663, -7.705886871421367523 ) ) ;
#3681 = AXIS2_PLACEMENT_3D ( 'NONE', #36306, #46521, #10233 ) ;
#3682 = CARTESIAN_POINT ( 'NONE',  ( 8.437984349512095861, 113.1929263765338050, 1.550032578732816828E-15 ) ) ;
#3683 = CARTESIAN_POINT ( 'NONE',  ( -195.0000000000000000, 0.000000000000000000, 9.524999999999991473 ) ) ;
#3684 = VERTEX_POINT ( 'NONE', #67562 ) ;
#3685 =( NAMED_UNIT ( * ) PLANE_ANGLE_UNIT ( ) SI_UNIT ( $, .RADIAN. ) );
#3686 = DIRECTION ( 'NONE',  ( 0.000000000000000000, 0.000000000000000000, -1.000000000000000000 ) ) ;
#3688 = CARTESIAN_POINT ( 'NONE',  ( -60.74292637653380922, -5.598654528085803328, -7.705886871421366635 ) ) ;
#3687 = CARTESIAN_POINT ( 'NONE',  ( 43.75000000000000000, 19.24999999999998224, -3.750000000000000000 ) ) ;
#3689 = DIRECTION ( 'NONE',  ( 1.000000000000000000, 0.000000000000000000, 0.000000000000000000 ) ) ;
#3690 = CARTESIAN_POINT ( 'NONE',  ( -151.5550000000000068, 0.000000000000000000, 8.024999999999991473 ) ) ;
#3691 = EDGE_CURVE ( 'NONE', #20333, #57903, #8135, .T. ) ;
#3692 = CARTESIAN_POINT ( 'NONE',  ( -75.00000000000000000, 9.585819622309035282, 6.373651444779978803 ) ) ;
#3693 = CARTESIAN_POINT ( 'NONE',  ( 0.000000000000000000, 110.5741857357814553, -9.450814264218539762 ) ) ;
#3694 = CARTESIAN_POINT ( 'NONE',  ( -151.0449999999999875, 7.632228543268600340, 2.479861379858949277 ) ) ;
#3695 = PRESENTATION_LAYER_ASSIGNMENT (  '', '', ( #27303 ) ) ;
#3696 = CARTESIAN_POINT ( 'NONE',  ( -145.1949999999999648, 8.437984349512086979, -1.550032578732815448E-15 ) ) ;
#3697 = ORIENTED_EDGE ( 'NONE', *, *, #30630, .F. ) ;
#3698 = ADVANCED_FACE ( 'NONE', ( #18349, #34508 ), #19360, .T. ) ;
#3699 = CARTESIAN_POINT ( 'NONE',  ( -180.6570736234661751, 9.058813317711329915, 2.943386871421369566 ) ) ;
#3700 = CIRCLE ( 'NONE', #8273, 0.2500000000000002220 ) ;
#3701 = CARTESIAN_POINT ( 'NONE',  ( -45.50000000000000000, 99.99999999999992895, -9.500000000000000000 ) ) ;
#3702 = DIRECTION ( 'NONE',  ( -1.000000000000000000, -0.000000000000000000, -0.000000000000000000 ) ) ;
#3703 = UNCERTAINTY_MEASURE_WITH_UNIT (LENGTH_MEASURE( 1.000000000000000082E-05 ), #703, 'distance_accuracy_value', 'NONE');
#3704 = CARTESIAN_POINT ( 'NONE',  ( -64.40499999999998693, -2.607480562269069768, 8.024999999999991473 ) ) ;
#3705 = PRESENTATION_STYLE_ASSIGNMENT (( #62478 ) ) ;
#3706 = DIRECTION ( 'NONE',  ( 0.000000000000000000, 1.000000000000000000, 0.000000000000000000 ) ) ;
#3707 = CARTESIAN_POINT ( 'NONE',  ( -62.69499999999998607, -8.437984349512086979, 5.166775262442717831E-16 ) ) ;
#3708 = AXIS2_PLACEMENT_3D ( 'NONE', #37478, #68752, #42056 ) ;
#3709 = CARTESIAN_POINT ( 'NONE',  ( -3.094860106618432471, 155.7049999999999841, -9.525000000000000355 ) ) ;
#3710 = DIRECTION ( 'NONE',  ( 0.000000000000000000, 0.000000000000000000, 1.000000000000000000 ) ) ;
#3711 = EDGE_CURVE ( 'NONE', #26409, #21935, #24295, .T. ) ;
#3712 = AXIS2_PLACEMENT_3D ( 'NONE', #28784, #39732, #34750 ) ;
#3713 = CARTESIAN_POINT ( 'NONE',  ( 10.00000000000001954, 50.00000000000000000, 46.00000000000000000 ) ) ;
#3714 = UNCERTAINTY_MEASURE_WITH_UNIT (LENGTH_MEASURE( 1.000000000000000082E-05 ), #68652, 'distance_accuracy_value', 'NONE');
#3715 = DIRECTION ( 'NONE',  ( 0.7218214822630870664, 2.132585202559554694E-16, 0.6920792929596433218 ) ) ;
#3716 = VECTOR ( 'NONE', #7673, 1000.000000000000000 ) ;
#3717 = CARTESIAN_POINT ( 'NONE',  ( -4.156108327861140431E-16, 42.24279663153610187, -45.14569480374296973 ) ) ;
#3718 = EDGE_CURVE ( 'NONE', #66384, #68588, #3006, .T. ) ;
#3719 = CARTESIAN_POINT ( 'NONE',  ( -2.451748578458123784E-13, 110.8535625161535592, 9.171437483846442973 ) ) ;
#3720 = SURFACE_STYLE_FILL_AREA ( #4075 ) ;
#3721 = DIRECTION ( 'NONE',  ( -1.000000000000000000, 0.000000000000000000, 0.000000000000000000 ) ) ;
#3722 = DIRECTION ( 'NONE',  ( -0.000000000000000000, -0.000000000000000000, -1.000000000000000000 ) ) ;
#3723 = CARTESIAN_POINT ( 'NONE',  ( -1.502314598737159031E-15, -2.500000000000000000, -9.000000000000000000 ) ) ;
#3724 = ORIENTED_EDGE ( 'NONE', *, *, #61532, .T. ) ;
#3725 = ORIENTED_EDGE ( 'NONE', *, *, #64414, .T. ) ;
#3726 = FACE_OUTER_BOUND ( 'NONE', #44249, .T. ) ;
#3727 = CIRCLE ( 'NONE', #25112, 3.100000000000005418 ) ;
#3728 = AXIS2_PLACEMENT_3D ( 'NONE', #34311, #7570, #17794 ) ;
#3729 = DIRECTION ( 'NONE',  ( -0.000000000000000000, -0.000000000000000000, -1.000000000000000000 ) ) ;
#3730 = FILL_AREA_STYLE_COLOUR ( '', #404 ) ;
#3731 = ORIENTED_EDGE ( 'NONE', *, *, #35594, .T. ) ;
#3732 = ORIENTED_EDGE ( 'NONE', *, *, #23555, .F. ) ;
#3733 = LINE ( 'NONE', #19234, #23072 ) ;
#3734 = AXIS2_PLACEMENT_3D ( 'NONE', #51456, #40229, #68337 ) ;
#3735 = ORIENTED_EDGE ( 'NONE', *, *, #9108, .F. ) ;
#3736 = CARTESIAN_POINT ( 'NONE',  ( -8.102448949553181734, 120.0049999999999955, -5.886773742842749790 ) ) ;
#3737 = CARTESIAN_POINT ( 'NONE',  ( 34.99999999999992895, 113.4999999999999858, 7.000000000000000000 ) ) ;
#3738 = SURFACE_SIDE_STYLE ('',( #32243 ) ) ;
#3739 = DIRECTION ( 'NONE',  ( -1.000000000000000000, 0.000000000000000000, 0.000000000000000000 ) ) ;
#3740 = CARTESIAN_POINT ( 'NONE',  ( -106.3449999999999989, 7.632228543268599452, -2.479861379858951942 ) ) ;
#3741 = ORIENTED_EDGE ( 'NONE', *, *, #67515, .F. ) ;
#3742 = SURFACE_SIDE_STYLE ('',( #64165 ) ) ;
#3743 = ADVANCED_FACE ( 'NONE', ( #51385, #24624 ), #46140, .F. ) ;
#3744 = DIRECTION ( 'NONE',  ( 1.000000000000000000, -0.000000000000000000, -0.000000000000000000 ) ) ;
#3745 = CYLINDRICAL_SURFACE ( 'NONE', #26085, 0.5000000000000004441 ) ;
#3746 =( GEOMETRIC_REPRESENTATION_CONTEXT ( 3 ) GLOBAL_UNCERTAINTY_ASSIGNED_CONTEXT ( ( #56473 ) ) GLOBAL_UNIT_ASSIGNED_CONTEXT ( ( #17388, #22637, #38520 ) ) REPRESENTATION_CONTEXT ( 'NONE', 'WORKASPACE' ) );
#3747 = LINE ( 'NONE', #35799, #65566 ) ;
#3748 = VERTEX_POINT ( 'NONE', #28522 ) ;
#3749 = CARTESIAN_POINT ( 'NONE',  ( 6.826472737025121695, 149.4929263765338021, -4.959722759717905660 ) ) ;
#3750 = FILL_AREA_STYLE_COLOUR ( '', #52362 ) ;
#3751 = ADVANCED_FACE ( 'NONE', ( #50021 ), #54716, .F. ) ;
#3752 = CARTESIAN_POINT ( 'NONE',  ( 52.49999999999998579, 2.746146170318484607E-15, 12.00000000000000000 ) ) ;
#3753 = COLOUR_RGB ( '', 0.72549020, 0.75294118, 0.79215686) ;
#3754 = ORIENTED_EDGE ( 'NONE', *, *, #51669, .F. ) ;
#3755 =( LENGTH_UNIT ( ) NAMED_UNIT ( * ) SI_UNIT ( .MILLI., .METRE. ) );
#3756 = EDGE_LOOP ( 'NONE', ( #64534, #50996, #14334, #58273 ) ) ;
#3757 = LINE ( 'NONE', #49494, #4611 ) ;
#3758 = SURFACE_STYLE_USAGE ( .BOTH. , #62865 ) ;
#3759 = CARTESIAN_POINT ( 'NONE',  ( -140.5429263765338135, 9.058813317711329915, 2.943386871421369566 ) ) ;
#3760 = CARTESIAN_POINT ( 'NONE',  ( 41.40613950039011826, 107.1008216811760718, -3.493724300021677553 ) ) ;
#3761 = CARTESIAN_POINT ( 'NONE',  ( -121.5549999999999926, 0.000000000000000000, 8.024999999999991473 ) ) ;
#3762 = CARTESIAN_POINT ( 'NONE',  ( -183.9999999999999432, -1.549738613431724588, 7.912546321907711899 ) ) ;
#3763 = FACE_OUTER_BOUND ( 'NONE', #925, .T. ) ;
#3764 = CARTESIAN_POINT ( 'NONE',  ( 21.02379604162863913, 154.9999999999999716, 10.50000000000000000 ) ) ;
#3765 = CYLINDRICAL_SURFACE ( 'NONE', #65496, 3.100000000000000533 ) ;
#3767 = DIRECTION ( 'NONE',  ( -0.9486832980505138790, -0.3162277660168378857, 0.000000000000000000 ) ) ;
#3766 = COLOUR_RGB ( '', 0.09019608, 0.27058824, 0.51372549) ;
#3768 = FACE_OUTER_BOUND ( 'NONE', #35734, .T. ) ;
#3769 = EDGE_LOOP ( 'NONE', ( #45352, #61690, #34935, #20153 ) ) ;
#3770 = VERTEX_POINT ( 'NONE', #1758 ) ;
#3771 =( NAMED_UNIT ( * ) PLANE_ANGLE_UNIT ( ) SI_UNIT ( $, .RADIAN. ) );
#3772 = AXIS2_PLACEMENT_3D ( 'NONE', #15498, #20759, #36964 ) ;
#3773 = DIRECTION ( 'NONE',  ( -1.000000000000000000, 0.000000000000000000, 0.000000000000000000 ) ) ;
#3774 = EDGE_CURVE ( 'NONE', #40384, #12618, #42438, .T. ) ;
#3775 = CIRCLE ( 'NONE', #30709, 0.2500000000000002220 ) ;
#3776 = DIRECTION ( 'NONE',  ( 0.000000000000000000, 0.000000000000000000, -1.000000000000000000 ) ) ;
#3777 = ORIENTED_EDGE ( 'NONE', *, *, #46272, .F. ) ;
#3778 = CARTESIAN_POINT ( 'NONE',  ( -154.1929263765338192, -10.01517768586948698, 6.132527647946031529E-16 ) ) ;
#3779 = CARTESIAN_POINT ( 'NONE',  ( -177.9550000000000125, -7.632228543268599452, 2.479861379858951054 ) ) ;
#3780 = EDGE_CURVE ( 'NONE', #34648, #65503, #31291, .T. ) ;
#3781 =( NAMED_UNIT ( * ) SI_UNIT ( $, .STERADIAN. ) SOLID_ANGLE_UNIT ( ) );
#3782 = LINE ( 'NONE', #36208, #38065 ) ;
#3783 = CARTESIAN_POINT ( 'NONE',  ( -181.4950000000000045, 6.826472737025113702, -4.959722759717902107 ) ) ;
#3784 = AXIS2_PLACEMENT_3D ( 'NONE', #17975, #50681, #61229 ) ;
#3785 = CARTESIAN_POINT ( 'NONE',  ( -176.9949999999999761, -6.826472737025113702, 4.959722759717902107 ) ) ;
#3786 = DIRECTION ( 'NONE',  ( 0.000000000000000000, -0.000000000000000000, 1.000000000000000000 ) ) ;
#3787 = VERTEX_POINT ( 'NONE', #3858 ) ;
#3788 = TOROIDAL_SURFACE ( 'NONE', #52158, 0.5000000000000000000, 0.2500000000000000000 ) ;
#3789 = EDGE_CURVE ( 'NONE', #30484, #46307, #42598, .T. ) ;
#3790 = FILL_AREA_STYLE_COLOUR ( '', #21470 ) ;
#3791 = CARTESIAN_POINT ( 'NONE',  ( -93.20499999999998408, -2.607480562269071545, -8.024999999999991473 ) ) ;
#3792 = FACE_OUTER_BOUND ( 'NONE', #58558, .T. ) ;
#3793 = DIRECTION ( 'NONE',  ( -1.239088197126290817E-16, 0.000000000000000000, -1.000000000000000000 ) ) ;
#3794 = CARTESIAN_POINT ( 'NONE',  ( 45.00000000000000000, -1.469576158976824618E-14, -4.000000000000000000 ) ) ;
#3795 = ADVANCED_FACE ( 'NONE', ( #41545 ), #58389, .F. ) ;
#3796 =( GEOMETRIC_REPRESENTATION_CONTEXT ( 3 ) GLOBAL_UNCERTAINTY_ASSIGNED_CONTEXT ( ( #36229 ) ) GLOBAL_UNIT_ASSIGNED_CONTEXT ( ( #22598, #43742, #64807 ) ) REPRESENTATION_CONTEXT ( 'NONE', 'WORKASPACE' ) );
#3797 = CARTESIAN_POINT ( 'NONE',  ( -91.19499999999997897, 8.437984349512086979, -1.550032578732815448E-15 ) ) ;
#3798 = CARTESIAN_POINT ( 'NONE',  ( -3.094860106618432471, 131.7049999999999557, -9.525000000000000355 ) ) ;
#3799 = CARTESIAN_POINT ( 'NONE',  ( -64.64499999999998181, 4.716976649647091513, -6.492361379858946790 ) ) ;
#3800 = CARTESIAN_POINT ( 'NONE',  ( 71.50000000000000000, 14.49137674618942562, 7.000000000000000000 ) ) ;
#3801 = ADVANCED_FACE ( 'NONE', ( #31651 ), #15459, .T. ) ;
#3802 = AXIS2_PLACEMENT_3D ( 'NONE', #55411, #44902, #66310 ) ;
#3803 = STYLED_ITEM ( 'NONE', ( #63555 ), #61877 ) ;
#3804 = DIRECTION ( 'NONE',  ( -1.000000000000000000, -0.000000000000000000, -0.000000000000000000 ) ) ;
#3805 = UNCERTAINTY_MEASURE_WITH_UNIT (LENGTH_MEASURE( 1.000000000000000082E-05 ), #63707, 'distance_accuracy_value', 'NONE');
#3806 = DIRECTION ( 'NONE',  ( 0.000000000000000000, 0.000000000000000000, -1.000000000000000000 ) ) ;
#3807 = ORIENTED_EDGE ( 'NONE', *, *, #15018, .T. ) ;
#3808 = CARTESIAN_POINT ( 'NONE',  ( -100.6429263765337936, -5.598654528085801552, 7.705886871421367523 ) ) ;
#3809 = EDGE_CURVE ( 'NONE', #38442, #68484, #41316, .T. ) ;
#3810 = CARTESIAN_POINT ( 'NONE',  ( -132.2949999999999875, -2.607480562269069768, 8.024999999999991473 ) ) ;
#3811 =( LENGTH_UNIT ( ) NAMED_UNIT ( * ) SI_UNIT ( .MILLI., .METRE. ) );
#3812 = AXIS2_PLACEMENT_3D ( 'NONE', #54191, #27442, #38424 ) ;
#3813 = FILL_AREA_STYLE ('',( #42915 ) ) ;
#3815 = DIRECTION ( 'NONE',  ( 0.000000000000000000, 0.000000000000000000, 1.000000000000000000 ) ) ;
#3814 = CYLINDRICAL_SURFACE ( 'NONE', #4865, 0.2500000000000002220 ) ;
#3816 = ORIENTED_EDGE ( 'NONE', *, *, #10582, .F. ) ;
#3817 = VERTEX_POINT ( 'NONE', #51745 ) ;
#3818 = CARTESIAN_POINT ( 'NONE',  ( 6.826472737025121695, 131.4929263765337737, -4.959722759717905660 ) ) ;
#3819 = CIRCLE ( 'NONE', #59984, 0.5000000000000004441 ) ;
#3820 = STYLED_ITEM ( 'NONE', ( #14603 ), #324 ) ;
#3821 =( GEOMETRIC_REPRESENTATION_CONTEXT ( 3 ) GLOBAL_UNCERTAINTY_ASSIGNED_CONTEXT ( ( #30674 ) ) GLOBAL_UNIT_ASSIGNED_CONTEXT ( ( #49968, #24571, #7389 ) ) REPRESENTATION_CONTEXT ( 'NONE', 'WORKASPACE' ) );
#3822 = DIRECTION ( 'NONE',  ( -1.000000000000000000, 0.000000000000000000, 0.000000000000000000 ) ) ;
#3823 = CARTESIAN_POINT ( 'NONE',  ( -23.71231517720798010, 113.4999999999999858, 7.500000000000000000 ) ) ;
#3824 = CARTESIAN_POINT ( 'NONE',  ( -19.89974874213240597, 115.4999999999999574, 10.50000000000000000 ) ) ;
#3825 = VERTEX_POINT ( 'NONE', #41912 ) ;
#3826 = CARTESIAN_POINT ( 'NONE',  ( -122.6049999999999898, 6.826472737025113702, -4.959722759717902107 ) ) ;
#3827 = ORIENTED_EDGE ( 'NONE', *, *, #54329, .F. ) ;
#3828 = AXIS2_PLACEMENT_3D ( 'NONE', #43776, #38513, #59906 ) ;
#3829 = SURFACE_SIDE_STYLE ('',( #62252 ) ) ;
#3830 = CARTESIAN_POINT ( 'NONE',  ( -127.5570736234661950, -1.166476076187852838E-15, -9.524999999999991473 ) ) ;
#3831 = EDGE_LOOP ( 'NONE', ( #59555, #27502, #52542, #51282, #28508, #11196 ) ) ;
#3832 = DIRECTION ( 'NONE',  ( 0.000000000000000000, 1.000000000000000000, 0.000000000000000000 ) ) ;
#3833 = CARTESIAN_POINT ( 'NONE',  ( 44.00000000000000000, 19.24999999999998224, 4.000000000000000000 ) ) ;
#3834 = ORIENTED_EDGE ( 'NONE', *, *, #60975, .F. ) ;
#3835 = DIRECTION ( 'NONE',  ( -1.000000000000000000, -0.000000000000000000, -0.000000000000000000 ) ) ;
#3836 = CARTESIAN_POINT ( 'NONE',  ( 0.000000000000000000, 148.4449999999999932, -9.525000000000000355 ) ) ;
#3837 = FILL_AREA_STYLE_COLOUR ( '', #47601 ) ;
#3838 = EDGE_CURVE ( 'NONE', #60366, #23764, #24991, .T. ) ;
#3839 = ORIENTED_EDGE ( 'NONE', *, *, #57162, .T. ) ;
#3840 = AXIS2_PLACEMENT_3D ( 'NONE', #54819, #18609, #17587 ) ;
#3841 = CARTESIAN_POINT ( 'NONE',  ( 10.01517768586949408, 151.8049999999999784, 1.839758294383810543E-15 ) ) ;
#3842 = CARTESIAN_POINT ( 'NONE',  ( -48.05499999999998550, -9.827790563157499189E-16, -8.024999999999991473 ) ) ;
#3843 = ORIENTED_EDGE ( 'NONE', *, *, #38614, .T. ) ;
#3844 = CARTESIAN_POINT ( 'NONE',  ( 7.632228543268608334, 113.3429263765338106, -2.479861379858951942 ) ) ;
#3845 = DIRECTION ( 'NONE',  ( -1.000000000000000000, 0.000000000000000000, 0.000000000000000000 ) ) ;
#3846 = UNCERTAINTY_MEASURE_WITH_UNIT (LENGTH_MEASURE( 1.000000000000000082E-05 ), #56279, 'distance_accuracy_value', 'NONE');
#3847 =( LENGTH_UNIT ( ) NAMED_UNIT ( * ) SI_UNIT ( .MILLI., .METRE. ) );
#3848 = DIRECTION ( 'NONE',  ( -0.000000000000000000, -0.000000000000000000, -1.000000000000000000 ) ) ;
#3849 = VECTOR ( 'NONE', #55287, 1000.000000000000000 ) ;
#3850 = CARTESIAN_POINT ( 'NONE',  ( 0.000000000000000000, 0.9999999999999991118, -80.00402776293826435 ) ) ;
#3851 = DIRECTION ( 'NONE',  ( 0.000000000000000000, 1.000000000000000000, 0.000000000000000000 ) ) ;
#3852 = ORIENTED_EDGE ( 'NONE', *, *, #18178, .T. ) ;
#3853 = CARTESIAN_POINT ( 'NONE',  ( -7.441974819423180065, 1.110121504110840762, 0.4967607073414712637 ) ) ;
#3854 = ORIENTED_EDGE ( 'NONE', *, *, #6986, .T. ) ;
#3855 = CARTESIAN_POINT ( 'NONE',  ( -57.89292637653377938, -8.102448949553172852, -5.886773742842741797 ) ) ;
#3856 = COLOUR_RGB ( '', 0.31764706, 0.68627451, 0.89019608) ;
#3857 = AXIS2_PLACEMENT_3D ( 'NONE', #51199, #63482, #20206 ) ;
#3858 = CARTESIAN_POINT ( 'NONE',  ( -165.4429263765337907, -1.166476076187852838E-15, -9.524999999999991473 ) ) ;
#3859 = CARTESIAN_POINT ( 'NONE',  ( -5.356721384544678166, -4.721886399977921478, 0.1324414877861183337 ) ) ;
#3860 = CARTESIAN_POINT ( 'NONE',  ( -150.6549999999999727, -7.632228543268600340, -2.479861379858950166 ) ) ;
#3861 = EDGE_LOOP ( 'NONE', ( #1199, #33181, #50194, #9344, #40824, #24708 ) ) ;
#3862 = UNCERTAINTY_MEASURE_WITH_UNIT (LENGTH_MEASURE( 1.000000000000000082E-05 ), #13227, 'distance_accuracy_value', 'NONE');
#3863 = EDGE_CURVE ( 'NONE', #737, #56578, #49579, .T. ) ;
#3864 = CARTESIAN_POINT ( 'NONE',  ( -61.49999999999998579, 50.00000000000000000, -9.500000000000000000 ) ) ;
#3865 = CARTESIAN_POINT ( 'NONE',  ( -53.22588732449509763, -10.24482008810577582, 4.106145367375290789 ) ) ;
#3866 = CARTESIAN_POINT ( 'NONE',  ( -70.04292637653379927, -9.058813317711329915, -2.943386871421370898 ) ) ;
#3867 = CARTESIAN_POINT ( 'NONE',  ( 45.50000000000000000, 10.69371294336137979, -6.000000000000000000 ) ) ;
#3868 = EDGE_LOOP ( 'NONE', ( #63158, #13657, #52185, #674 ) ) ;
#3869 = AXIS2_PLACEMENT_3D ( 'NONE', #25001, #41557, #46510 ) ;
#3870 = ADVANCED_FACE ( 'NONE', ( #69628 ), #33387, .T. ) ;
#3871 = ORIENTED_EDGE ( 'NONE', *, *, #47980, .F. ) ;
#3872 = CARTESIAN_POINT ( 'NONE',  ( 22.91412244410874166, 24.72131563869667303, 27.25834036759371770 ) ) ;
#3873 = FILL_AREA_STYLE_COLOUR ( '', #20993 ) ;
#3874 = EDGE_CURVE ( 'NONE', #583, #49555, #43545, .T. ) ;
#3875 = CARTESIAN_POINT ( 'NONE',  ( -62.45499999999998408, 7.632228543268599452, -2.479861379858951942 ) ) ;
#3877 = ORIENTED_EDGE ( 'NONE', *, *, #31596, .T. ) ;
#3876 = COLOUR_RGB ( '', 0.08235294, 0.09019608, 0.10196078) ;
#3878 = EDGE_CURVE ( 'NONE', #50390, #47709, #49141, .T. ) ;
#3879 = CARTESIAN_POINT ( 'NONE',  ( -74.99999999999998579, 50.00000000000000000, 6.499999999999999112 ) ) ;
#3880 = STYLED_ITEM ( 'NONE', ( #53849 ), #37537 ) ;
#3881 = CARTESIAN_POINT ( 'NONE',  ( -123.5929263765345638, -3.094860106631271091, -9.524999999990667376 ) ) ;
#3882 = CYLINDRICAL_SURFACE ( 'NONE', #24065, 0.2500000000000002220 ) ;
#3883 = STYLED_ITEM ( 'NONE', ( #47705 ), #56231 ) ;
#3884 = EDGE_LOOP ( 'NONE', ( #893, #39481, #3871 ) ) ;
#3885 = FILL_AREA_STYLE ('',( #56689 ) ) ;
#3886 = VECTOR ( 'NONE', #58677, 1000.000000000000227 ) ;
#3887 = DIRECTION ( 'NONE',  ( -0.000000000000000000, -0.000000000000000000, -1.000000000000000000 ) ) ;
#3889 = FACE_BOUND ( 'NONE', #22831, .T. ) ;
#3888 = DIRECTION ( 'NONE',  ( 0.000000000000000000, -0.000000000000000000, 1.000000000000000000 ) ) ;
#3890 = EDGE_CURVE ( 'NONE', #3437, #13821, #34503, .T. ) ;
#3891 = CARTESIAN_POINT ( 'NONE',  ( 9.058813317711338797, 150.8449999999999989, -2.943386871421372675 ) ) ;
#3892 = CARTESIAN_POINT ( 'NONE',  ( -94.34499999999998465, 7.632228543268599452, -2.479861379858951942 ) ) ;
#3893 = FACE_OUTER_BOUND ( 'NONE', #25998, .T. ) ;
#3894 = CARTESIAN_POINT ( 'NONE',  ( -67.99999999999998579, -2.024042244987997205E-14, 10.50000000000000000 ) ) ;
#3895 = UNCERTAINTY_MEASURE_WITH_UNIT (LENGTH_MEASURE( 1.000000000000000082E-05 ), #29993, 'distance_accuracy_value', 'NONE');
#3896 = CIRCLE ( 'NONE', #26350, 0.5000000000000004441 ) ;
#3897 = CARTESIAN_POINT ( 'NONE',  ( -71.39292637653377938, 8.102448949553176405, 5.886773742842740909 ) ) ;
#3898 = CONICAL_SURFACE ( 'NONE', #57867, 6.999999999999997335, 0.7853981633974500554 ) ;
#3899 = ORIENTED_EDGE ( 'NONE', *, *, #9744, .T. ) ;
#3900 = CARTESIAN_POINT ( 'NONE',  ( -147.4429263765338192, -1.166476076187852838E-15, -9.524999999999991473 ) ) ;
#3901 = DIRECTION ( 'NONE',  ( -0.000000000000000000, -0.000000000000000000, -1.000000000000000000 ) ) ;
#3902 = CARTESIAN_POINT ( 'NONE',  ( -155.0949999999999989, -2.607480562269071545, -8.024999999999991473 ) ) ;
#3903 = CARTESIAN_POINT ( 'NONE',  ( -46.55707362346617373, -1.166476076187852838E-15, -9.524999999999991473 ) ) ;
#3904 = CIRCLE ( 'NONE', #58962, 1.000000000000000888 ) ;
#3905 = ADVANCED_FACE ( 'NONE', ( #22141 ), #1310, .F. ) ;
#3906 = DIRECTION ( 'NONE',  ( 1.000000000000000000, 0.000000000000000000, -0.000000000000000000 ) ) ;
#3907 = PLANE ( 'NONE',  #4905 ) ;
#3908 = MECHANICAL_DESIGN_GEOMETRIC_PRESENTATION_REPRESENTATION (  '', ( #24159 ), #36580 ) ;
#3910 = DIRECTION ( 'NONE',  ( 0.000000000000000000, 1.000000000000000000, 0.000000000000000000 ) ) ;
#3909 = VECTOR ( 'NONE', #55916, 1000.000000000000000 ) ;
#3911 = ORIENTED_EDGE ( 'NONE', *, *, #52057, .T. ) ;
#3912 = VERTEX_POINT ( 'NONE', #28067 ) ;
#3913 = AXIS2_PLACEMENT_3D ( 'NONE', #15060, #48459, #21682 ) ;
#3914 = EDGE_CURVE ( 'NONE', #42263, #17125, #12043, .T. ) ;
#3915 = SURFACE_STYLE_USAGE ( .BOTH. , #57051 ) ;
#3916 = CARTESIAN_POINT ( 'NONE',  ( -143.8429263765338249, 9.058813317711329915, -2.943386871421373119 ) ) ;
#3917 = CARTESIAN_POINT ( 'NONE',  ( 7.632228543268607446, 119.0429263765338135, 2.479861379858954606 ) ) ;
#3918 = CARTESIAN_POINT ( 'NONE',  ( -44.99999999999998579, 119.9999999999999716, 7.500000000000000000 ) ) ;
#3919 = SURFACE_STYLE_USAGE ( .BOTH. , #10272 ) ;
#3920 = ORIENTED_EDGE ( 'NONE', *, *, #26448, .T. ) ;
#3921 = CARTESIAN_POINT ( 'NONE',  ( -155.7549999999999955, 4.716976649647091513, -6.492361379858946790 ) ) ;
#3922 = VECTOR ( 'NONE', #3925, 1000.000000000000000 ) ;
#3923 = ORIENTED_EDGE ( 'NONE', *, *, #14706, .T. ) ;
#3924 = DIRECTION ( 'NONE',  ( 0.000000000000000000, 1.000000000000000000, 0.000000000000000000 ) ) ;
#3925 = DIRECTION ( 'NONE',  ( 1.000000000000000000, -0.000000000000000000, -0.000000000000000000 ) ) ;
#3926 = VERTEX_POINT ( 'NONE', #21440 ) ;
#3927 = CIRCLE ( 'NONE', #27518, 0.5000000000000004441 ) ;
#3928 = DIRECTION ( 'NONE',  ( 0.000000000000000000, 0.000000000000000000, 1.000000000000000000 ) ) ;
#3929 = SURFACE_STYLE_FILL_AREA ( #15240 ) ;
#3930 = CARTESIAN_POINT ( 'NONE',  ( 2.607480562269076430, 159.9070736234661183, -8.025000000000000355 ) ) ;
#3931 = STYLED_ITEM ( 'NONE', ( #53860 ), #56708 ) ;
#3932 = VERTEX_POINT ( 'NONE', #42956 ) ;
#3933 = CARTESIAN_POINT ( 'NONE',  ( 92.41620014002536720, 0.000000000000000000, -24.00402776293825369 ) ) ;
#3934 = CARTESIAN_POINT ( 'NONE',  ( 3.094860106618435136, 116.4049999999999869, -9.525000000000000355 ) ) ;
#3935 = CARTESIAN_POINT ( 'NONE',  ( -70.10499999999998977, -6.826472737025113702, 4.959722759717902107 ) ) ;
#3936 = STYLED_ITEM ( 'NONE', ( #51869 ), #32479 ) ;
#3937 = DIRECTION ( 'NONE',  ( 0.000000000000000000, 0.000000000000000000, 1.000000000000000000 ) ) ;
#3938 =( BOUNDED_CURVE ( )  B_SPLINE_CURVE ( 2, ( #17337, #43048, #27484, #26461, #6388, #11672, #22230, #32095, #53219, #5339, #27817 ),
 .UNSPECIFIED., .F., .F. ) 
 B_SPLINE_CURVE_WITH_KNOTS ( ( 3, 2, 2, 2, 2, 3 ),
 ( 0.6847826086956522174, 0.6869565217391304657, 0.6891304347826087140, 0.6913043478260869623, 0.6934782608695652106, 0.6956521739130434590 ),
 .UNSPECIFIED. ) 
 CURVE ( )  GEOMETRIC_REPRESENTATION_ITEM ( )  RATIONAL_B_SPLINE_CURVE ( ( 1.000000000000000000, 0.9510565162951535312, 1.000000000000000000, 0.9510565162951535312, 1.000000000000000000, 0.9510565162951535312, 1.000000000000000000, 0.9510565162951535312, 1.000000000000000000, 0.9510565162951535312, 1.000000000000000000 ) ) 
 REPRESENTATION_ITEM ( '' )  );
#3939 = EDGE_LOOP ( 'NONE', ( #14966, #12743, #26301, #13717 ) ) ;
#3940 = CARTESIAN_POINT ( 'NONE',  ( -1.166476076187854022E-15, 139.0549999999999784, 9.525000000000000355 ) ) ;
#3941 = UNCERTAINTY_MEASURE_WITH_UNIT (LENGTH_MEASURE( 1.000000000000000082E-05 ), #17192, 'distance_accuracy_value', 'NONE');
#3942 =( LENGTH_UNIT ( ) NAMED_UNIT ( * ) SI_UNIT ( .MILLI., .METRE. ) );
#3943 =( NAMED_UNIT ( * ) PLANE_ANGLE_UNIT ( ) SI_UNIT ( $, .RADIAN. ) );
#3944 = SURFACE_SIDE_STYLE ('',( #41287 ) ) ;
#3945 = ADVANCED_FACE ( 'NONE', ( #27038 ), #55832, .T. ) ;
#3946 =( NAMED_UNIT ( * ) PLANE_ANGLE_UNIT ( ) SI_UNIT ( $, .RADIAN. ) );
#3947 = ORIENTED_EDGE ( 'NONE', *, *, #33286, .T. ) ;
#3948 = DIRECTION ( 'NONE',  ( -0.000000000000000000, -1.000000000000000000, -0.000000000000000000 ) ) ;
#3949 = CARTESIAN_POINT ( 'NONE',  ( -177.9550000000000125, -7.632228543268599452, 2.479861379858951054 ) ) ;
#3950 = ORIENTED_EDGE ( 'NONE', *, *, #55677, .T. ) ;
#3951 = CARTESIAN_POINT ( 'NONE',  ( -74.75000000000000000, -3.000000000000000000, 7.000000000000001776 ) ) ;
#3952 = EDGE_CURVE ( 'NONE', #30747, #67303, #10949, .T. ) ;
#3953 = SURFACE_SIDE_STYLE ('',( #46597 ) ) ;
#3954 = ORIENTED_EDGE ( 'NONE', *, *, #17731, .F. ) ;
#3955 = DIRECTION ( 'NONE',  ( 0.5000000000000001110, -0.8660254037844384856, 0.000000000000000000 ) ) ;
#3956 = DIRECTION ( 'NONE',  ( -2.312964634635740689E-15, 1.000000000000000000, -0.000000000000000000 ) ) ;
#3957 = VERTEX_POINT ( 'NONE', #43985 ) ;
#3958 = LINE ( 'NONE', #25432, #64214 ) ;
#3960 = ADVANCED_FACE ( 'NONE', ( #65399 ), #10559, .F. ) ;
#3959 = CARTESIAN_POINT ( 'NONE',  ( 13.75000000000000533, 30.74999999999999289, 3.750000000000000000 ) ) ;
#3961 = CARTESIAN_POINT ( 'NONE',  ( -92.00499999999998124, 6.826472737025116366, 4.959722759717898555 ) ) ;
#3962 = ORIENTED_EDGE ( 'NONE', *, *, #29145, .F. ) ;
#3963 = FILL_AREA_STYLE ('',( #53232 ) ) ;
#3964 = MANIFOLD_SOLID_BREP ( 'Cut-Sweep4', #67724 ) ;
#3965 = DIRECTION ( 'NONE',  ( 1.000000000000000000, 2.312964634635707951E-15, 0.000000000000000000 ) ) ;
#3966 = AXIS2_PLACEMENT_3D ( 'NONE', #21681, #9418, #63214 ) ;
#3967 = CARTESIAN_POINT ( 'NONE',  ( -144.8070736234661808, 10.01517768586948698, -1.839758294383808571E-15 ) ) ;
#3968 = COLOUR_RGB ( '', 0.31764706, 0.68627451, 0.89019608) ;
#3969 =( BOUNDED_SURFACE ( )  B_SPLINE_SURFACE ( 3, 2, ( 
 ( #27813, #32780, #38099 ),
 ( #48662, #49664, #59859 ),
 ( #12340, #43723, #16632 ),
 ( #21892, #11320, #28151 ),
 ( #10268, #26777, #44435 ),
 ( #697, #49317, #33475 ) ),
 .UNSPECIFIED., .F., .F., .F. ) 
 B_SPLINE_SURFACE_WITH_KNOTS ( ( 4, 2, 4 ),
 ( 3, 3 ),
 ( 0.03640205491000769039, 0.03794596731985265536, 0.03948987972969762034 ),
 ( 0.6341638506276230380, 1.000000000000000000 ),
 .UNSPECIFIED. ) 
 GEOMETRIC_REPRESENTATION_ITEM ( )  RATIONAL_B_SPLINE_SURFACE ( (
 ( 0.9651092272895998025, 0.9724907272183133111, 1.000000000000000000),
 ( 0.9651083974483595229, 0.9724900729384773346, 1.000000000000000000),
 ( 0.9649374241050432399, 0.9723552707551401664, 1.000000000000000000),
 ( 0.9642640192915807873, 0.9718243316194610237, 1.000000000000000000),
 ( 0.9637558210279215665, 0.9714236478977728018, 1.000000000000000000),
 ( 0.9630880506049159795, 0.9708971511396047305, 1.000000000000000000) ) ) 
 REPRESENTATION_ITEM ( '' )  SURFACE ( )  );
#3970 = FILL_AREA_STYLE_COLOUR ( '', #20653 ) ;
#3971 = CARTESIAN_POINT ( 'NONE',  ( -73.55707362346616662, -1.166476076187852838E-15, -9.524999999999991473 ) ) ;
#3972 = CARTESIAN_POINT ( 'NONE',  ( -92.09292637653497593, 3.094860106637794317, 9.524999999985924504 ) ) ;
#3973 = ORIENTED_EDGE ( 'NONE', *, *, #33153, .T. ) ;
#3974 = CARTESIAN_POINT ( 'NONE',  ( -16.61951246926111381, -11.02716856853298033, 4.733319217996198702 ) ) ;
#3975 = DIRECTION ( 'NONE',  ( 1.000000000000000000, 0.000000000000000000, 0.000000000000000000 ) ) ;
#3976 = EDGE_CURVE ( 'NONE', #65417, #61564, #61491, .T. ) ;
#3977 = CARTESIAN_POINT ( 'NONE',  ( -107.9050000000000011, 2.607480562269068880, -8.024999999999993250 ) ) ;
#3978 = DIRECTION ( 'NONE',  ( 0.000000000000000000, 0.000000000000000000, 1.000000000000000000 ) ) ;
#3979 = CARTESIAN_POINT ( 'NONE',  ( 10.01517768586949231, 117.6949999999999790, 1.839758294383810543E-15 ) ) ;
#3980 = CARTESIAN_POINT ( 'NONE',  ( -129.8949999999999818, 6.826472737025116366, 4.959722759717898555 ) ) ;
#3981 = MECHANICAL_DESIGN_GEOMETRIC_PRESENTATION_REPRESENTATION (  '', ( #6252 ), #60183 ) ;
#3982 = CYLINDRICAL_SURFACE ( 'NONE', #54934, 0.5000000000000004441 ) ;
#3983 = ORIENTED_EDGE ( 'NONE', *, *, #577, .T. ) ;
#3984 = SURFACE_SIDE_STYLE ('',( #52224 ) ) ;
#3985 = CARTESIAN_POINT ( 'NONE',  ( 26.00000000000001066, 18.99999999999997868, 4.000000000000000000 ) ) ;
#3986 = ORIENTED_EDGE ( 'NONE', *, *, #51406, .T. ) ;
#3987 = CARTESIAN_POINT ( 'NONE',  ( -166.7070736234663570, -3.094860106621724949, -9.524999999997598721 ) ) ;
#3988 = CIRCLE ( 'NONE', #60194, 10.02500000000000568 ) ;
#3989 = CARTESIAN_POINT ( 'NONE',  ( -173.9929263765338021, 8.102448949553171076, -5.886773742842744461 ) ) ;
#3990 = CARTESIAN_POINT ( 'NONE',  ( -182.2450000000000045, -4.716976649647093289, -6.492361379858945902 ) ) ;
#3991 = CARTESIAN_POINT ( 'NONE',  ( -44.99282180236183848, 9.603602307716927911, -3.208073701553950219 ) ) ;
#3992 = LINE ( 'NONE', #52576, #60447 ) ;
#3993 = DIRECTION ( 'NONE',  ( 1.000000000000000000, 7.709882115452468306E-16, 0.000000000000000000 ) ) ;
#3994 = ORIENTED_EDGE ( 'NONE', *, *, #49735, .F. ) ;
#3995 = CARTESIAN_POINT ( 'NONE',  ( -81.74292637653380211, -5.598654528085803328, -7.705886871421366635 ) ) ;
#3996 = CONTEXT_DEPENDENT_SHAPE_REPRESENTATION ( #26226, #17083 ) ;
#3997 = VECTOR ( 'NONE', #62801, 1000.000000000000000 ) ;
#3998 = CYLINDRICAL_SURFACE ( 'NONE', #33778, 1.000000000000000000 ) ;
#3999 = SURFACE_SIDE_STYLE ('',( #8619 ) ) ;
#4000 = SURFACE_STYLE_USAGE ( .BOTH. , #3636 ) ;
#4001 =( GEOMETRIC_REPRESENTATION_CONTEXT ( 3 ) GLOBAL_UNCERTAINTY_ASSIGNED_CONTEXT ( ( #42550 ) ) GLOBAL_UNIT_ASSIGNED_CONTEXT ( ( #56571, #14717, #66796 ) ) REPRESENTATION_CONTEXT ( 'NONE', 'WORKASPACE' ) );
#4002 = CARTESIAN_POINT ( 'NONE',  ( -75.75000000000000000, -4.000000000000000000, 19.00000000000000000 ) ) ;
#4003 = ORIENTED_EDGE ( 'NONE', *, *, #6431, .T. ) ;
#4004 = DIRECTION ( 'NONE',  ( -0.000000000000000000, -1.000000000000000000, -0.000000000000000000 ) ) ;
#4005 = FACE_OUTER_BOUND ( 'NONE', #59870, .T. ) ;
#4006 = SURFACE_STYLE_USAGE ( .BOTH. , #52250 ) ;
#4008 = ORIENTED_EDGE ( 'NONE', *, *, #51896, .T. ) ;
#4007 = AXIS2_PLACEMENT_3D ( 'NONE', #13824, #35285, #44831 ) ;
#4009 = VECTOR ( 'NONE', #13286, 1000.000000000000000 ) ;
#4010 = CARTESIAN_POINT ( 'NONE',  ( 71.49999999999998579, 64.07124727947029896, -7.500000000000000000 ) ) ;
#4011 = CARTESIAN_POINT ( 'NONE',  ( -7.632228543268608334, 130.9570736234661581, 2.479861379858952830 ) ) ;
#4012 = LINE ( 'NONE', #45339, #21419 ) ;
#4013 = ORIENTED_EDGE ( 'NONE', *, *, #34615, .F. ) ;
#4014 = CARTESIAN_POINT ( 'NONE',  ( -100.5570736234661808, -1.166476076187852838E-15, -9.524999999999991473 ) ) ;
#4015 = CARTESIAN_POINT ( 'NONE',  ( -100.2549999999999812, -4.716976649647092401, 6.492361379858946790 ) ) ;
#4016 = UNCERTAINTY_MEASURE_WITH_UNIT (LENGTH_MEASURE( 1.000000000000000082E-05 ), #42839, 'distance_accuracy_value', 'NONE');
#4017 = CARTESIAN_POINT ( 'NONE',  ( 75.15811388300841145, 19.52565835097472302, 6.500000000000000000 ) ) ;
#4018 = VERTEX_POINT ( 'NONE', #23188 ) ;
#4019 = SURFACE_SIDE_STYLE ('',( #41359 ) ) ;
#4020 = VECTOR ( 'NONE', #8010, 1000.000000000000000 ) ;
#4021 = CARTESIAN_POINT ( 'NONE',  ( -104.3070736234661666, -10.01517768586948698, 6.132527647946031529E-16 ) ) ;
#4022 = DIRECTION ( 'NONE',  ( 1.000000000000000000, 0.000000000000000000, 0.000000000000000000 ) ) ;
#4023 = EDGE_CURVE ( 'NONE', #21246, #47500, #57404, .T. ) ;
#4024 = CIRCLE ( 'NONE', #59080, 5.499999999999985789 ) ;
#4025 = ORIENTED_EDGE ( 'NONE', *, *, #2940, .T. ) ;
#4026 = CARTESIAN_POINT ( 'NONE',  ( 6.759171781091401598, 2.292771058063876932, 0.1074872947962648290 ) ) ;
#4027 = CARTESIAN_POINT ( 'NONE',  ( -67.64499999999998181, 4.716976649647091513, -6.492361379858946790 ) ) ;
#4028 = VERTEX_POINT ( 'NONE', #34749 ) ;
#4029 = STYLED_ITEM ( 'NONE', ( #56903 ), #57326 ) ;
#4030 = CARTESIAN_POINT ( 'NONE',  ( -72.00000000000000000, 35.92875272052971525, 10.00000000000000000 ) ) ;
#4031 = SURFACE_STYLE_FILL_AREA ( #35020 ) ;
#4032 = ORIENTED_EDGE ( 'NONE', *, *, #33524, .T. ) ;
#4033 = CARTESIAN_POINT ( 'NONE',  ( 3.851859888774471706E-31, -8.500000000000000000, 24.00000000000000000 ) ) ;
#4034 = DIRECTION ( 'NONE',  ( 0.000000000000000000, 1.000000000000000000, 0.000000000000000000 ) ) ;
#4035 = DIRECTION ( 'NONE',  ( 1.000000000000000000, 0.000000000000000000, 0.000000000000000000 ) ) ;
#4036 = ADVANCED_FACE ( 'NONE', ( #24533 ), #12960, .F. ) ;
#4037 = ORIENTED_EDGE ( 'NONE', *, *, #35524, .T. ) ;
#4038 = DIRECTION ( 'NONE',  ( 0.000000000000000000, 0.000000000000000000, 1.000000000000000000 ) ) ;
#4039 = ADVANCED_FACE ( 'NONE', ( #7355 ), #1987, .T. ) ;
#4040 = VERTEX_POINT ( 'NONE', #28418 ) ;
#4041 = SURFACE_STYLE_USAGE ( .BOTH. , #36808 ) ;
#4042 = CARTESIAN_POINT ( 'NONE',  ( -133.9429263765338192, 0.000000000000000000, 9.524999999999991473 ) ) ;
#4043 = CARTESIAN_POINT ( 'NONE',  ( 10.99999999999999645, 11.99999999999999289, 4.000000000000000000 ) ) ;
#4044 = CARTESIAN_POINT ( 'NONE',  ( -167.0070736234661695, -8.102448949553172852, -5.886773742842741797 ) ) ;
#4045 = ADVANCED_FACE ( 'NONE', ( #56562 ), #46048, .T. ) ;
#4046 = CARTESIAN_POINT ( 'NONE',  ( 0.000000000000000000, 121.4449999999999790, -9.525000000000000355 ) ) ;
#4047 = CARTESIAN_POINT ( 'NONE',  ( -100.4070736234661894, 3.094860106618428031, -9.524999999999993250 ) ) ;
#4048 = EDGE_CURVE ( 'NONE', #22068, #24120, #59316, .T. ) ;
#4049 = CARTESIAN_POINT ( 'NONE',  ( -65.90707362346617515, -3.094860106618429807, 9.524999999999991473 ) ) ;
#4050 = PRODUCT ( '6. Lower Jaw', '6. Lower Jaw', '', ( #11796 ) ) ;
#4051 = ORIENTED_EDGE ( 'NONE', *, *, #8132, .F. ) ;
#4052 = CARTESIAN_POINT ( 'NONE',  ( -107.3929263765338078, 8.102448949553176405, 5.886773742842740909 ) ) ;
#4054 = CARTESIAN_POINT ( 'NONE',  ( 72.00000000000000000, 35.92875272052971525, 7.500000000000000000 ) ) ;
#4053 = CARTESIAN_POINT ( 'NONE',  ( 34.99999999999992895, 113.4999999999999858, -7.500000000000000000 ) ) ;
#4056 = DIRECTION ( 'NONE',  ( 0.000000000000000000, 0.000000000000000000, -1.000000000000000000 ) ) ;
#4055 = AXIS2_PLACEMENT_3D ( 'NONE', #27393, #66075, #59770 ) ;
#4057 = CARTESIAN_POINT ( 'NONE',  ( -153.5049999999999670, -6.826472737025115478, -4.959722759717899443 ) ) ;
#4058 = FILL_AREA_STYLE ('',( #67759 ) ) ;
#4059 = CARTESIAN_POINT ( 'NONE',  ( -155.6949999999999932, -8.437984349512085203, 5.166775262442717831E-16 ) ) ;
#4060 = CARTESIAN_POINT ( 'NONE',  ( -152.5449999999999875, -7.632228543268600340, -2.479861379858950166 ) ) ;
#4061 = ORIENTED_EDGE ( 'NONE', *, *, #15514, .F. ) ;
#4062 =( BOUNDED_CURVE ( )  B_SPLINE_CURVE ( 2, ( #6305, #54822, #277, #44687, #65408, #21810, #17592, #33059, #27734, #60126, #5957 ),
 .UNSPECIFIED., .F., .F. ) 
 B_SPLINE_CURVE_WITH_KNOTS ( ( 3, 2, 2, 2, 2, 3 ),
 ( 0.5652173913043344600, 0.5673913043478127083, 0.5695652173912908456, 0.5717391304347690939, 0.5739130434782472312, 0.5760869565217253685 ),
 .UNSPECIFIED. ) 
 CURVE ( )  GEOMETRIC_REPRESENTATION_ITEM ( )  RATIONAL_B_SPLINE_CURVE ( ( 1.000000000000299982, 0.9510565162948535489, 1.000000000000000000, 0.9510565162951535312, 1.000000000000000000, 0.9510565162951535312, 1.000000000000000000, 0.9510565162951535312, 1.000000000000000000, 0.9510565162954635055, 0.9999999999996900257 ) ) 
 REPRESENTATION_ITEM ( '' )  );
#4063 = DIRECTION ( 'NONE',  ( 0.000000000000000000, 0.000000000000000000, 1.000000000000000000 ) ) ;
#4064 = CARTESIAN_POINT ( 'NONE',  ( -75.00000000000000000, 67.00000000000000000, -6.500000000000000000 ) ) ;
#4065 = CARTESIAN_POINT ( 'NONE',  ( -59.30499999999999972, 8.437984349512085203, -1.550032578732815448E-15 ) ) ;
#4066 = SURFACE_STYLE_FILL_AREA ( #14656 ) ;
#4067 = STYLED_ITEM ( 'NONE', ( #20999 ), #40143 ) ;
#4068 = CARTESIAN_POINT ( 'NONE',  ( -64.34499999999998465, 7.632228543268599452, -2.479861379858951942 ) ) ;
#4069 = CARTESIAN_POINT ( 'NONE',  ( -3.094860106618434248, 153.9049999999999443, 9.525000000000000355 ) ) ;
#4070 = CARTESIAN_POINT ( 'NONE',  ( -51.74292637653380211, -5.598654528085803328, -7.705886871421366635 ) ) ;
#4071 = MANIFOLD_SOLID_BREP ( 'Fillet7', #55362 ) ;
#4072 = DIRECTION ( 'NONE',  ( 1.000000000000000000, 1.091455702833322304E-16, 1.786087863151538256E-17 ) ) ;
#4073 = SURFACE_STYLE_USAGE ( .BOTH. , #63537 ) ;
#4074 = LINE ( 'NONE', #68475, #67379 ) ;
#4075 = FILL_AREA_STYLE ('',( #4789 ) ) ;
#4076 = DIRECTION ( 'NONE',  ( -1.000000000000000000, 0.000000000000000000, 0.000000000000000000 ) ) ;
#4077 = CARTESIAN_POINT ( 'NONE',  ( -23.71231517720798010, 118.4999999999999716, -7.000000000000000000 ) ) ;
#4078 = CARTESIAN_POINT ( 'NONE',  ( 8.000000000000000000, 5.000000000000000000, -72.00402776293825013 ) ) ;
#4079 =( LENGTH_UNIT ( ) NAMED_UNIT ( * ) SI_UNIT ( .MILLI., .METRE. ) );
#4080 = ORIENTED_EDGE ( 'NONE', *, *, #13990, .T. ) ;
#4081 = ORIENTED_EDGE ( 'NONE', *, *, #29447, .F. ) ;
#4082 = SURFACE_STYLE_FILL_AREA ( #52330 ) ;
#4083 = FACE_OUTER_BOUND ( 'NONE', #35255, .T. ) ;
#4084 = CARTESIAN_POINT ( 'NONE',  ( 9.250000000000003553, 25.24999999999998934, -3.750000000000000000 ) ) ;
#4085 = ORIENTED_EDGE ( 'NONE', *, *, #44036, .T. ) ;
#4086 = VERTEX_POINT ( 'NONE', #41822 ) ;
#4087 =( GEOMETRIC_REPRESENTATION_CONTEXT ( 3 ) GLOBAL_UNCERTAINTY_ASSIGNED_CONTEXT ( ( #59349 ) ) GLOBAL_UNIT_ASSIGNED_CONTEXT ( ( #22062, #50872, #19179 ) ) REPRESENTATION_CONTEXT ( 'NONE', 'WORKASPACE' ) );
#4088 = CARTESIAN_POINT ( 'NONE',  ( -109.5570736234661666, -1.166476076187852838E-15, -9.524999999999991473 ) ) ;
#4089 =( NAMED_UNIT ( * ) PLANE_ANGLE_UNIT ( ) SI_UNIT ( $, .RADIAN. ) );
#4090 = ORIENTED_EDGE ( 'NONE', *, *, #35258, .F. ) ;
#4091 = CARTESIAN_POINT ( 'NONE',  ( -3.094860106618432471, 116.7049999999999983, -9.525000000000000355 ) ) ;
#4092 = CARTESIAN_POINT ( 'NONE',  ( -84.74292637653380211, -5.598654528085803328, -7.705886871421366635 ) ) ;
#4093 = ORIENTED_EDGE ( 'NONE', *, *, #62014, .F. ) ;
#4094 = EDGE_CURVE ( 'NONE', #51729, #67943, #55979, .T. ) ;
#4095 = LINE ( 'NONE', #14694, #2373 ) ;
#4096 = CARTESIAN_POINT ( 'NONE',  ( -98.09499999999997044, -2.607480562269071545, -8.024999999999991473 ) ) ;
#4097 = ORIENTED_EDGE ( 'NONE', *, *, #11882, .F. ) ;
#4098 = ADVANCED_FACE ( 'NONE', ( #58301 ), #56917, .T. ) ;
#4099 = FILL_AREA_STYLE ('',( #41108 ) ) ;
#4100 = DIRECTION ( 'NONE',  ( 0.000000000000000000, 0.000000000000000000, 1.000000000000000000 ) ) ;
#4101 = DIRECTION ( 'NONE',  ( 7.080503983578803083E-17, -1.000000000000000000, 0.000000000000000000 ) ) ;
#4102 = VERTEX_POINT ( 'NONE', #15084 ) ;
#4103 = CARTESIAN_POINT ( 'NONE',  ( 4.716976649647099507, 158.6429263765338078, -6.492361379858953008 ) ) ;
#4104 = DIRECTION ( 'NONE',  ( 0.000000000000000000, -1.000000000000000000, 0.000000000000000000 ) ) ;
#4105 = VECTOR ( 'NONE', #39127, 1000.000000000000000 ) ;
#4106 = LINE ( 'NONE', #8393, #14309 ) ;
#4107 = ORIENTED_EDGE ( 'NONE', *, *, #69561, .T. ) ;
#4108 = CARTESIAN_POINT ( 'NONE',  ( 19.98431065987488608, 114.9999999999999574, -10.47133983857574613 ) ) ;
#4109 = EDGE_CURVE ( 'NONE', #68484, #454, #28991, .T. ) ;
#4110 = ORIENTED_EDGE ( 'NONE', *, *, #22794, .F. ) ;
#4111 = CARTESIAN_POINT ( 'NONE',  ( 0.000000000000000000, 0.000000000000000000, 0.2499999999999941436 ) ) ;
#4112 = PRESENTATION_STYLE_ASSIGNMENT (( #3758 ) ) ;
#4113 = CARTESIAN_POINT ( 'NONE',  ( -140.0929263765343649, 3.094860106627776997, 9.524999999993202238 ) ) ;
#4114 = CARTESIAN_POINT ( 'NONE',  ( -128.6049999999999898, 6.826472737025113702, -4.959722759717902107 ) ) ;
#4115 = CARTESIAN_POINT ( 'NONE',  ( 36.00000000000002842, 5.000000000000000000, -29.00402776293825724 ) ) ;
#4116 = DIRECTION ( 'NONE',  ( -1.224646799147353207E-16, 1.000000000000000000, 0.000000000000000000 ) ) ;
#4117 = VECTOR ( 'NONE', #43882, 1000.000000000000000 ) ;
#4118 = CARTESIAN_POINT ( 'NONE',  ( -126.4429263765338192, -1.166476076187852838E-15, -9.524999999999991473 ) ) ;
#4119 = EDGE_CURVE ( 'NONE', #58118, #2414, #69489, .T. ) ;
#4120 = SPHERICAL_SURFACE ( 'NONE', #61997, 0.2500000000000000000 ) ;
#4121 = PRESENTATION_STYLE_ASSIGNMENT (( #24901 ) ) ;
#4122 = LINE ( 'NONE', #2817, #51501 ) ;
#4123 = EDGE_LOOP ( 'NONE', ( #21502, #31337, #42919 ) ) ;
#4124 = EDGE_LOOP ( 'NONE', ( #19322, #63004, #28694, #64597 ) ) ;
#4125 = CARTESIAN_POINT ( 'NONE',  ( -9.827790563157511022E-16, 151.4429263765338192, 8.025000000000000355 ) ) ;
#4126 =( LENGTH_UNIT ( ) NAMED_UNIT ( * ) SI_UNIT ( .MILLI., .METRE. ) );
#4127 = DIRECTION ( 'NONE',  ( -0.000000000000000000, -0.000000000000000000, 1.000000000000000000 ) ) ;
#4128 = DIRECTION ( 'NONE',  ( 0.5000000000000002220, 0.000000000000000000, 0.8660254037844384856 ) ) ;
#4129 = EDGE_LOOP ( 'NONE', ( #6995, #20071, #13810, #26628 ) ) ;
#4130 = FILL_AREA_STYLE_COLOUR ( '', #19150 ) ;
#4131 = CARTESIAN_POINT ( 'NONE',  ( -174.2050000000000125, -2.607480562269071545, -8.024999999999991473 ) ) ;
#4132 = DIRECTION ( 'NONE',  ( 1.000000000000000000, 0.000000000000000000, 0.000000000000000000 ) ) ;
#4133 = DIRECTION ( 'NONE',  ( 0.000000000000000000, 0.000000000000000000, 1.000000000000000000 ) ) ;
#4134 = CARTESIAN_POINT ( 'NONE',  ( -47.00707362346617657, -8.102448949553172852, -5.886773742842741797 ) ) ;
#4135 = CARTESIAN_POINT ( 'NONE',  ( -179.9949999999999761, -6.826472737025113702, 4.959722759717902107 ) ) ;
#4136 = VERTEX_POINT ( 'NONE', #25929 ) ;
#4137 = LINE ( 'NONE', #53063, #63890 ) ;
#4138 = CARTESIAN_POINT ( 'NONE',  ( 3.673940397442060361E-16, 0.000000000000000000, 3.000000000000000444 ) ) ;
#4139 = CARTESIAN_POINT ( 'NONE',  ( -12.48350263443806618, 11.19219915118087982, 4.332593345627109294 ) ) ;
#4140 = CARTESIAN_POINT ( 'NONE',  ( -93.80499999999999261, -8.437984349512085203, 5.166775262442717831E-16 ) ) ;
#4141 = CARTESIAN_POINT ( 'NONE',  ( -74.55554437418339830, 36.39399965470389731, -10.00000000000000000 ) ) ;
#4142 = AXIS2_PLACEMENT_3D ( 'NONE', #11061, #22674, #43817 ) ;
#4143 = CARTESIAN_POINT ( 'NONE',  ( -94.19499999999999318, 8.437984349512086979, -1.550032578732815448E-15 ) ) ;
#4144 = CARTESIAN_POINT ( 'NONE',  ( -1.166476076187854022E-15, 127.0549999999999784, 9.525000000000000355 ) ) ;
#4145 =( GEOMETRIC_REPRESENTATION_CONTEXT ( 3 ) GLOBAL_UNCERTAINTY_ASSIGNED_CONTEXT ( ( #62776 ) ) GLOBAL_UNIT_ASSIGNED_CONTEXT ( ( #936, #10897, #59768 ) ) REPRESENTATION_CONTEXT ( 'NONE', 'WORKASPACE' ) );
#4146 = CARTESIAN_POINT ( 'NONE',  ( -70.79499999999998749, 2.607480562269068880, -8.024999999999993250 ) ) ;
#4147 = CARTESIAN_POINT ( 'NONE',  ( -75.00000000000000000, 8.163938725409359165, -6.987118804072281364 ) ) ;
#4148 = SURFACE_STYLE_USAGE ( .BOTH. , #40452 ) ;
#4149 = EDGE_CURVE ( 'NONE', #2048, #48570, #51113, .T. ) ;
#4150 = SURFACE_STYLE_USAGE ( .BOTH. , #9485 ) ;
#4151 = FACE_OUTER_BOUND ( 'NONE', #28866, .T. ) ;
#4152 = ORIENTED_EDGE ( 'NONE', *, *, #25563, .F. ) ;
#4153 = CARTESIAN_POINT ( 'NONE',  ( -100.7929263765338135, -3.094860106618429807, 9.524999999999991473 ) ) ;
#4154 = CARTESIAN_POINT ( 'NONE',  ( -126.2950000000000017, -2.607480562269069768, 8.024999999999991473 ) ) ;
#4155 = CARTESIAN_POINT ( 'NONE',  ( -6.826472737025120807, 146.1070736234661354, 4.959722759717906548 ) ) ;
#4156 = AXIS2_PLACEMENT_3D ( 'NONE', #55951, #17982, #66517 ) ;
#4157 = CARTESIAN_POINT ( 'NONE',  ( 34.99999999999999289, 99.99999999999997158, -9.500000000000000000 ) ) ;
#4158 = CARTESIAN_POINT ( 'NONE',  ( 0.000000000000000000, 136.0570736234661808, -8.025000000000000355 ) ) ;
#4159 = SURFACE_SIDE_STYLE ('',( #9496 ) ) ;
#4160 = ORIENTED_EDGE ( 'NONE', *, *, #23412, .F. ) ;
#4161 = ORIENTED_EDGE ( 'NONE', *, *, #23903, .F. ) ;
#4162 =( LENGTH_UNIT ( ) NAMED_UNIT ( * ) SI_UNIT ( .MILLI., .METRE. ) );
#4163 = CARTESIAN_POINT ( 'NONE',  ( -133.9429263765338192, 0.000000000000000000, 9.524999999999991473 ) ) ;
#4164 = CARTESIAN_POINT ( 'NONE',  ( 57.00000000000000000, 16.00000000000000000, 60.00402776293825724 ) ) ;
#4165 = CYLINDRICAL_SURFACE ( 'NONE', #23633, 9.524999999999991473 ) ;
#4166 = DIRECTION ( 'NONE',  ( 1.000000000000000000, 0.000000000000000000, 0.000000000000000000 ) ) ;
#4167 = DIRECTION ( 'NONE',  ( 0.000000000000000000, 1.000000000000000000, 0.000000000000000000 ) ) ;
#4168 = ORIENTED_EDGE ( 'NONE', *, *, #36815, .T. ) ;
#4169 = CARTESIAN_POINT ( 'NONE',  ( -121.8549999999999898, 4.716976649647094177, 6.492361379858945902 ) ) ;
#4171 = EDGE_CURVE ( 'NONE', #25674, #67533, #23431, .T. ) ;
#4170 = EDGE_LOOP ( 'NONE', ( #24539, #10384, #12025, #61731 ) ) ;
#4172 = FACE_OUTER_BOUND ( 'NONE', #55774, .T. ) ;
#4173 = CARTESIAN_POINT ( 'NONE',  ( -120.5070736234661695, 8.102448949553176405, 5.886773742842740909 ) ) ;
#4174 = EDGE_CURVE ( 'NONE', #27816, #36075, #3155, .T. ) ;
#4175 = VERTEX_POINT ( 'NONE', #62182 ) ;
#4176 = LINE ( 'NONE', #58044, #53811 ) ;
#4177 = DIRECTION ( 'NONE',  ( 1.000000000000000000, 0.000000000000000000, 0.000000000000000000 ) ) ;
#4178 = ORIENTED_EDGE ( 'NONE', *, *, #31616, .T. ) ;
#4179 = CARTESIAN_POINT ( 'NONE',  ( 10.01517768586949231, 153.6949999999999932, 1.839758294383810543E-15 ) ) ;
#4180 = VERTEX_POINT ( 'NONE', #35472 ) ;
#4181 =( LENGTH_UNIT ( ) NAMED_UNIT ( * ) SI_UNIT ( .MILLI., .METRE. ) );
#4183 = EDGE_CURVE ( 'NONE', #45247, #63225, #25249, .T. ) ;
#4182 = CARTESIAN_POINT ( 'NONE',  ( -9.058813317711337021, 150.1549999999999727, -2.943386871421374895 ) ) ;
#4184 = CARTESIAN_POINT ( 'NONE',  ( -74.99999999999998579, 50.00000000000000000, 10.50000000000000000 ) ) ;
#4185 = CARTESIAN_POINT ( 'NONE',  ( 24.21231517720798010, 112.9999999999999858, -7.500000000000000000 ) ) ;
#4186 = ORIENTED_EDGE ( 'NONE', *, *, #52517, .T. ) ;
#4187 = CARTESIAN_POINT ( 'NONE',  ( -6.826472737025120807, 126.3929263765338220, -4.959722759717907437 ) ) ;
#4188 = DIRECTION ( 'NONE',  ( -1.000000000000000000, 0.000000000000000000, 0.000000000000000000 ) ) ;
#4190 = CARTESIAN_POINT ( 'NONE',  ( 45.00000000000000000, 10.69371294329215516, 6.262534692517949253 ) ) ;
#4189 = CIRCLE ( 'NONE', #35669, 7.000000000000001776 ) ;
#4191 = AXIS2_PLACEMENT_3D ( 'NONE', #38985, #22767, #7283 ) ;
#4192 = CARTESIAN_POINT ( 'NONE',  ( 24.00000000000000355, 37.00000000000000000, -3.000000000000000000 ) ) ;
#4193 = STYLED_ITEM ( 'NONE', ( #29483 ), #4039 ) ;
#4194 = ORIENTED_EDGE ( 'NONE', *, *, #35521, .T. ) ;
#4195 = CARTESIAN_POINT ( 'NONE',  ( 30.50000000000001066, 16.24999999999997513, -4.000000000000000000 ) ) ;
#4196 = ADVANCED_FACE ( 'NONE', ( #57255 ), #30504, .F. ) ;
#4197 = VERTEX_POINT ( 'NONE', #27300 ) ;
#4198 = CARTESIAN_POINT ( 'NONE',  ( -61.79292637653379217, -3.094860106618429807, 9.524999999999991473 ) ) ;
#4199 = FILL_AREA_STYLE_COLOUR ( '', #24398 ) ;
#4200 = CARTESIAN_POINT ( 'NONE',  ( 31.00000000000002132, 50.00000000000000000, 59.99999999999999289 ) ) ;
#4201 = CARTESIAN_POINT ( 'NONE',  ( -151.7049999999999841, 2.607480562269073321, 8.024999999999991473 ) ) ;
#4202 = EDGE_LOOP ( 'NONE', ( #51029, #434, #506, #41564 ) ) ;
#4203 = PRESENTATION_STYLE_ASSIGNMENT (( #31658 ) ) ;
#4204 = EDGE_CURVE ( 'NONE', #61310, #19333, #54052, .T. ) ;
#4205 = LINE ( 'NONE', #19726, #63082 ) ;
#4206 = SPHERICAL_SURFACE ( 'NONE', #59513, 0.5000000000000000000 ) ;
#4207 = CARTESIAN_POINT ( 'NONE',  ( 34.99999999999999289, 99.99999999999997158, 10.00000000000000000 ) ) ;
#4208 = EDGE_LOOP ( 'NONE', ( #12232, #49943, #26696, #16542 ) ) ;
#4209 = COLOUR_RGB ( '', 0.72549020, 0.75294118, 0.79215686) ;
#4210 = ORIENTED_EDGE ( 'NONE', *, *, #17806, .T. ) ;
#4211 = CARTESIAN_POINT ( 'NONE',  ( 22.42372113159793656, 26.68536559262205543, 27.43315461247279430 ) ) ;
#4212 = AXIS2_PLACEMENT_3D ( 'NONE', #54806, #6990, #18237 ) ;
#4213 = CARTESIAN_POINT ( 'NONE',  ( -68.60499999999996135, 6.826472737025113702, -4.959722759717902107 ) ) ;
#4214 = ORIENTED_EDGE ( 'NONE', *, *, #46004, .T. ) ;
#4215 = SURFACE_STYLE_FILL_AREA ( #69321 ) ;
#4216 = DIRECTION ( 'NONE',  ( 0.000000000000000000, 0.000000000000000000, 1.000000000000000000 ) ) ;
#4217 = LINE ( 'NONE', #41567, #38564 ) ;
#4218 = CARTESIAN_POINT ( 'NONE',  ( 48.50000000000000000, 21.74999999999998579, -3.750000000000000000 ) ) ;
#4219 = ORIENTED_EDGE ( 'NONE', *, *, #13410, .T. ) ;
#4220 = CARTESIAN_POINT ( 'NONE',  ( -75.00000000000000000, 8.380821545698800890, -5.549835146672132957 ) ) ;
#4221 = LINE ( 'NONE', #63690, #60754 ) ;
#4223 = CARTESIAN_POINT ( 'NONE',  ( 107.0858988931383493, 5.000000000000000000, 16.89933289725615850 ) ) ;
#4222 = DIRECTION ( 'NONE',  ( -0.000000000000000000, -0.000000000000000000, -1.000000000000000000 ) ) ;
#4224 = CARTESIAN_POINT ( 'NONE',  ( 10.01517768586949231, 144.6949999999999932, 1.839758294383810543E-15 ) ) ;
#4225 = CARTESIAN_POINT ( 'NONE',  ( -101.9949999999999903, -6.826472737025115478, 4.959722759717900331 ) ) ;
#4226 = LINE ( 'NONE', #68997, #27380 ) ;
#4227 = CARTESIAN_POINT ( 'NONE',  ( 20.71231517720797655, 149.4999999999999716, -10.00000000000000000 ) ) ;
#4228 = EDGE_CURVE ( 'NONE', #44728, #11138, #62742, .T. ) ;
#4229 = CARTESIAN_POINT ( 'NONE',  ( 57.00000000000000000, 5.000000000000000000, 60.00402776293827145 ) ) ;
#4230 = VERTEX_POINT ( 'NONE', #32258 ) ;
#4231 = CIRCLE ( 'NONE', #8736, 5.500000000000005329 ) ;
#4232 = CARTESIAN_POINT ( 'NONE',  ( -129.7429263765338021, -5.598654528085803328, -7.705886871421366635 ) ) ;
#4233 = DIRECTION ( 'NONE',  ( 1.000000000000000000, 0.000000000000000000, 0.000000000000000000 ) ) ;
#4234 = CARTESIAN_POINT ( 'NONE',  ( -159.8950000000000102, 6.826472737025116366, 4.959722759717898555 ) ) ;
#4235 = AXIS2_PLACEMENT_3D ( 'NONE', #30003, #57084, #7514 ) ;
#4236 = STYLED_ITEM ( 'NONE', ( #55459 ), #65992 ) ;
#4237 = CYLINDRICAL_SURFACE ( 'NONE', #28074, 0.2500000000000002220 ) ;
#4238 = CARTESIAN_POINT ( 'NONE',  ( 57.00000000000000000, 0.000000000000000000, -60.00402776293827145 ) ) ;
#4239 = ORIENTED_EDGE ( 'NONE', *, *, #14930, .F. ) ;
#4240 = AXIS2_PLACEMENT_3D ( 'NONE', #17111, #16430, #32541 ) ;
#4241 = PRESENTATION_STYLE_ASSIGNMENT (( #25386 ) ) ;
#4242 = VERTEX_POINT ( 'NONE', #37242 ) ;
#4243 = CARTESIAN_POINT ( 'NONE',  ( 23.71231517720798010, 117.4999999999999716, 7.500000000000000000 ) ) ;
#4244 = ADVANCED_FACE ( 'NONE', ( #38279 ), #16474, .T. ) ;
#4245 = DIRECTION ( 'NONE',  ( 0.000000000000000000, 0.000000000000000000, -1.000000000000000000 ) ) ;
#4246 = CARTESIAN_POINT ( 'NONE',  ( -45.89399618234750733, 9.348666914230159719, 6.164661031308989791 ) ) ;
#4247 = CARTESIAN_POINT ( 'NONE',  ( -173.1570736234662036, -9.058813317711329915, -2.943386871421370898 ) ) ;
#4248 = MECHANICAL_DESIGN_GEOMETRIC_PRESENTATION_REPRESENTATION (  '', ( #9927 ), #42487 ) ;
#4249 = COLOUR_RGB ( '', 0.72549020, 0.75294118, 0.79215686) ;
#4250 = VERTEX_POINT ( 'NONE', #31905 ) ;
#4251 = CARTESIAN_POINT ( 'NONE',  ( -148.4050000000000011, -2.607480562269069768, 8.024999999999991473 ) ) ;
#4252 = EDGE_CURVE ( 'NONE', #60522, #19333, #31250, .T. ) ;
#4253 = EDGE_CURVE ( 'NONE', #6972, #9166, #11496, .T. ) ;
#4254 = VERTEX_POINT ( 'NONE', #32965 ) ;
#4255 = CARTESIAN_POINT ( 'NONE',  ( 57.00000000000000000, 5.000000000000000000, -77.00402776293825013 ) ) ;
#4256 = CARTESIAN_POINT ( 'NONE',  ( 0.000000000000000000, 149.9999999999999716, 0.000000000000000000 ) ) ;
#4257 = VERTEX_POINT ( 'NONE', #54400 ) ;
#4258 = CARTESIAN_POINT ( 'NONE',  ( 0.000000000000000000, -2.500000000000000000, 0.000000000000000000 ) ) ;
#4259 = CARTESIAN_POINT ( 'NONE',  ( -57.65707362346616804, 9.058813317711329915, 2.943386871421369566 ) ) ;
#4260 = CARTESIAN_POINT ( 'NONE',  ( -8.102448949553181734, 125.4949999999999903, 5.886773742842747126 ) ) ;
#4261 = VERTEX_POINT ( 'NONE', #6221 ) ;
#4262 = DIRECTION ( 'NONE',  ( 0.000000000000000000, 0.000000000000000000, -1.000000000000000000 ) ) ;
#4264 = EDGE_CURVE ( 'NONE', #33970, #3527, #42567, .T. ) ;
#4263 = CARTESIAN_POINT ( 'NONE',  ( 8.102448949553179958, 118.5049999999999955, 5.886773742842750679 ) ) ;
#4265 = CARTESIAN_POINT ( 'NONE',  ( -68.15499999999997272, 7.632228543268600340, 2.479861379858949277 ) ) ;
#4266 = DIRECTION ( 'NONE',  ( -0.000000000000000000, -1.000000000000000000, -0.000000000000000000 ) ) ;
#4267 = ORIENTED_EDGE ( 'NONE', *, *, #55376, .F. ) ;
#4268 = CARTESIAN_POINT ( 'NONE',  ( -1.166476076187854022E-15, 136.0549999999999784, 9.525000000000000355 ) ) ;
#4269 = CARTESIAN_POINT ( 'NONE',  ( 57.00000000000000000, 13.00000000000000178, -80.00402776293826435 ) ) ;
#4270 = EDGE_CURVE ( 'NONE', #34116, #41524, #33311, .T. ) ;
#4271 = CARTESIAN_POINT ( 'NONE',  ( 8.256904162901426147, 56.03086067945960735, 6.591072975109653953 ) ) ;
#4272 = PRESENTATION_STYLE_ASSIGNMENT (( #47270 ) ) ;
#4273 =( NAMED_UNIT ( * ) PLANE_ANGLE_UNIT ( ) SI_UNIT ( $, .RADIAN. ) );
#4274 = EDGE_LOOP ( 'NONE', ( #14342, #55492, #61794, #62503 ) ) ;
#4275 = VECTOR ( 'NONE', #12672, 1000.000000000000000 ) ;
#4276 = CARTESIAN_POINT ( 'NONE',  ( 2.000000000000008438, 26.00000000000000355, -27.50000000000000355 ) ) ;
#4277 = CARTESIAN_POINT ( 'NONE',  ( -26.79538245034556709, -8.499999999999996447, 1.000000000000000000 ) ) ;
#4278 = CARTESIAN_POINT ( 'NONE',  ( -60.99999999999998579, 50.00000000000000000, 7.000000000000000000 ) ) ;
#4279 = CARTESIAN_POINT ( 'NONE',  ( -180.8050000000000068, -8.437984349512085203, 5.166775262442717831E-16 ) ) ;
#4280 = EDGE_LOOP ( 'NONE', ( #14354, #20010, #7496, #18611 ) ) ;
#4281 = CARTESIAN_POINT ( 'NONE',  ( 2.139872436712063397, 110.9430683727271685, 8.842724602598599049 ) ) ;
#4282 = PRESENTATION_LAYER_ASSIGNMENT (  '', '', ( #9958 ) ) ;
#4283 = SURFACE_SIDE_STYLE ('',( #25764 ) ) ;
#4284 = CARTESIAN_POINT ( 'NONE',  ( -74.50000000000000000, -2.220952357103124925E-14, 6.999999999999999112 ) ) ;
#4285 = ORIENTED_EDGE ( 'NONE', *, *, #60742, .F. ) ;
#4286 = ORIENTED_EDGE ( 'NONE', *, *, #30059, .F. ) ;
#4287 = COLOUR_RGB ( '', 0.08235294, 0.09019608, 0.10196078) ;
#4288 = FILL_AREA_STYLE_COLOUR ( '', #47402 ) ;
#4289 = SURFACE_STYLE_FILL_AREA ( #52198 ) ;
#4290 = CARTESIAN_POINT ( 'NONE',  ( -95.15499999999998693, 7.632228543268600340, 2.479861379858949277 ) ) ;
#4291 = EDGE_LOOP ( 'NONE', ( #39789, #264, #3038, #66591, #50857, #1984, #5177, #32336, #1865, #66498, #24742, #5439, #46378, #37136, #47519, #45097, #28688, #25996, #60039, #19614, #58211, #31462 ) ) ;
#4292 = DIRECTION ( 'NONE',  ( 0.000000000000000000, 0.000000000000000000, 1.000000000000000000 ) ) ;
#4293 = FACE_OUTER_BOUND ( 'NONE', #37995, .T. ) ;
#4294 = CARTESIAN_POINT ( 'NONE',  ( -128.9070736234661751, -3.094860106618429807, 9.524999999999991473 ) ) ;
#4295 = ADVANCED_FACE ( 'NONE', ( #42510 ), #53387, .F. ) ;
#4296 = SURFACE_SIDE_STYLE ('',( #63073 ) ) ;
#4297 = CARTESIAN_POINT ( 'NONE',  ( 3.094860106618431583, 150.0949999999999420, 9.525000000000000355 ) ) ;
#4298 = CARTESIAN_POINT ( 'NONE',  ( -75.35707362346617799, 5.598654528085804216, 7.705886871421366635 ) ) ;
#4299 = CARTESIAN_POINT ( 'NONE',  ( 24.00000000000000000, 1.000000000000000000, -4.000000000000000000 ) ) ;
#4300 = ORIENTED_EDGE ( 'NONE', *, *, #67795, .F. ) ;
#4301 = SURFACE_STYLE_FILL_AREA ( #62026 ) ;
#4302 = DIRECTION ( 'NONE',  ( 0.000000000000000000, 0.000000000000000000, 1.000000000000000000 ) ) ;
#4303 = MECHANICAL_DESIGN_GEOMETRIC_PRESENTATION_REPRESENTATION (  '', ( #30121 ), #45937 ) ;
#4305 = CARTESIAN_POINT ( 'NONE',  ( -83.99999999999997158, 50.00000000000000000, -11.50000000000000000 ) ) ;
#4304 = FILL_AREA_STYLE ('',( #46618 ) ) ;
#4306 = CARTESIAN_POINT ( 'NONE',  ( -110.0049999999999955, 6.826472737025116366, 4.959722759717898555 ) ) ;
#4307 = DIRECTION ( 'NONE',  ( 0.000000000000000000, 0.000000000000000000, -1.000000000000000000 ) ) ;
#4308 = CARTESIAN_POINT ( 'NONE',  ( -9.058813317711337021, 122.0449999999999875, -2.943386871421374895 ) ) ;
#4309 = CARTESIAN_POINT ( 'NONE',  ( -123.1449999999999960, -4.716976649647092401, 6.492361379858946790 ) ) ;
#4310 = DIRECTION ( 'NONE',  ( -0.000000000000000000, -0.000000000000000000, 1.000000000000000000 ) ) ;
#4311 = CARTESIAN_POINT ( 'NONE',  ( -117.5929263765346633, -3.094860106632549179, -9.524999999989734789 ) ) ;
#4312 = ORIENTED_EDGE ( 'NONE', *, *, #59090, .T. ) ;
#4313 = VECTOR ( 'NONE', #296, 1000.000000000000000 ) ;
#4314 = CARTESIAN_POINT ( 'NONE',  ( -166.4929263765338021, -8.102448949553172852, 5.886773742842742685 ) ) ;
#4315 = FILL_AREA_STYLE_COLOUR ( '', #58561 ) ;
#4316 = CARTESIAN_POINT ( 'NONE',  ( -21.02379604162864268, 110.4999999999999858, -10.00000000000000000 ) ) ;
#4317 = CIRCLE ( 'NONE', #2016, 0.2500000000000002220 ) ;
#4318 = CARTESIAN_POINT ( 'NONE',  ( 74.89452121010485541, 1.000000000000000000, 66.39042820928573008 ) ) ;
#4319 = ADVANCED_FACE ( 'NONE', ( #16116 ), #180, .F. ) ;
#4320 =( GEOMETRIC_REPRESENTATION_CONTEXT ( 3 ) GLOBAL_UNCERTAINTY_ASSIGNED_CONTEXT ( ( #55336 ) ) GLOBAL_UNIT_ASSIGNED_CONTEXT ( ( #51582, #8338, #39325 ) ) REPRESENTATION_CONTEXT ( 'NONE', 'WORKASPACE' ) );
#4321 = CARTESIAN_POINT ( 'NONE',  ( 44.25000000000000000, 21.74999999999998579, 3.750000000000000000 ) ) ;
#4322 = DIRECTION ( 'NONE',  ( 0.000000000000000000, 0.000000000000000000, 1.000000000000000000 ) ) ;
#4323 = FILL_AREA_STYLE_COLOUR ( '', #4663 ) ;
#4324 = VERTEX_POINT ( 'NONE', #63909 ) ;
#4325 = CARTESIAN_POINT ( 'NONE',  ( -84.74292637653380211, -5.598654528085803328, -7.705886871421366635 ) ) ;
#4326 = ITEM_DEFINED_TRANSFORMATION ( 'NONE', 'NONE', #23648,  #42840 ) ;
#4327 = PRESENTATION_LAYER_ASSIGNMENT (  '', '', ( #67277 ) ) ;
#4328 = CARTESIAN_POINT ( 'NONE',  ( 1.000000000000000888, 43.00000000000000000, -45.61250543006183733 ) ) ;
#4329 = SURFACE_STYLE_USAGE ( .BOTH. , #10689 ) ;
#4330 = EDGE_CURVE ( 'NONE', #42106, #41694, #15761, .T. ) ;
#4332 = DIRECTION ( 'NONE',  ( 0.000000000000000000, 0.000000000000000000, 1.000000000000000000 ) ) ;
#4331 =( BOUNDED_SURFACE ( )  B_SPLINE_SURFACE ( 3, 2, ( 
 ( #3183, #24676, #53520 ),
 ( #36343, #37392, #26078 ),
 ( #21149, #68669, #20467 ),
 ( #57409, #46561, #35964 ),
 ( #67984, #9234, #31012 ),
 ( #63021, #5302, #52162 ) ),
 .UNSPECIFIED., .F., .F., .F. ) 
 B_SPLINE_SURFACE_WITH_KNOTS ( ( 4, 2, 4 ),
 ( 3, 3 ),
 ( 1.549108064047288735E-15, 0.001858363558057203775, 0.003716727116112858442 ),
 ( 0.000000000000000000, 1.000000000000000000 ),
 .UNSPECIFIED. ) 
 GEOMETRIC_REPRESENTATION_ITEM ( )  RATIONAL_B_SPLINE_SURFACE ( (
 ( 1.000000000000000000, 0.7942671885213775651, 1.000000000000000000),
 ( 1.000000000000000000, 0.7793712970752797453, 1.000000000000000000),
 ( 1.000000000000000000, 0.7645460165485118420, 1.000000000000000000),
 ( 1.000000000000000000, 0.7352674701534978041, 1.000000000000000000),
 ( 1.000000000000000000, 0.7207339695077151775, 1.000000000000000000),
 ( 1.000000000000000000, 0.7071067811865475727, 1.000000000000000000) ) ) 
 REPRESENTATION_ITEM ( '' )  SURFACE ( )  );
#4333 = SURFACE_STYLE_FILL_AREA ( #35699 ) ;
#4334 = CARTESIAN_POINT ( 'NONE',  ( -175.7049999999999841, 2.607480562269072433, 8.024999999999991473 ) ) ;
#4335 = EDGE_CURVE ( 'NONE', #31338, #57372, #69542, .T. ) ;
#4336 = ORIENTED_EDGE ( 'NONE', *, *, #68201, .F. ) ;
#4337 = CARTESIAN_POINT ( 'NONE',  ( 68.99999999999998579, 1.000000000000008438, 3.000000000000000000 ) ) ;
#4338 = FACE_OUTER_BOUND ( 'NONE', #61733, .T. ) ;
#4339 = ORIENTED_EDGE ( 'NONE', *, *, #19213, .F. ) ;
#4340 = AXIS2_PLACEMENT_3D ( 'NONE', #10749, #11422, #37878 ) ;
#4341 = CARTESIAN_POINT ( 'NONE',  ( -2.607480562269073765, 145.2070736234661581, -8.025000000000000355 ) ) ;
#4342 = CARTESIAN_POINT ( 'NONE',  ( 11.00000000000001776, 42.00000000000000000, -29.68999999999999417 ) ) ;
#4343 = VECTOR ( 'NONE', #13492, 1000.000000000000000 ) ;
#4344 = VERTEX_POINT ( 'NONE', #10811 ) ;
#4345 = CARTESIAN_POINT ( 'NONE',  ( 25.00000000000000000, 1.000000000000000888, 3.000000000000000000 ) ) ;
#4346 = CARTESIAN_POINT ( 'NONE',  ( -100.5549999999999926, 0.000000000000000000, 8.024999999999991473 ) ) ;
#4347 = AXIS2_PLACEMENT_3D ( 'NONE', #57276, #56588, #31220 ) ;
#4348 = SURFACE_SIDE_STYLE ('',( #35714 ) ) ;
#4349 = ORIENTED_EDGE ( 'NONE', *, *, #38509, .T. ) ;
#4350 = DIRECTION ( 'NONE',  ( -0.9704308468600219006, -0.2413793103448194366, -0.000000000000000000 ) ) ;
#4351 = EDGE_CURVE ( 'NONE', #11138, #46046, #65655, .T. ) ;
#4352 = CARTESIAN_POINT ( 'NONE',  ( 14.98999599679679662, 146.4999999999999716, -9.500000000000000000 ) ) ;
#4353 = DIRECTION ( 'NONE',  ( -0.000000000000000000, -0.000000000000000000, -1.000000000000000000 ) ) ;
#4354 = CARTESIAN_POINT ( 'NONE',  ( 10.50000000000002309, 8.000000000000000000, -4.000000000000000000 ) ) ;
#4355 = EDGE_LOOP ( 'NONE', ( #20650, #24455, #17466, #45196 ) ) ;
#4356 = CARTESIAN_POINT ( 'NONE',  ( -10.11618306975752368, 54.14354156754873060, 6.790106699912857202 ) ) ;
#4357 = CARTESIAN_POINT ( 'NONE',  ( -71.39499999999998181, -6.826472737025115478, -4.959722759717899443 ) ) ;
#4358 = ORIENTED_EDGE ( 'NONE', *, *, #23428, .T. ) ;
#4359 =( BOUNDED_CURVE ( )  B_SPLINE_CURVE ( 2, ( #22041, #49142, #39283, #33290, #48816, #6522, #43546, #60686, #32947, #54377, #6199 ),
 .UNSPECIFIED., .F., .F. ) 
 B_SPLINE_CURVE_WITH_KNOTS ( ( 3, 2, 2, 2, 2, 3 ),
 ( 0.4565217391304240424, 0.4586956521739022907, 0.4608695652173804835, 0.4630434782608586763, 0.4652173913043368692, 0.4673913043478151175 ),
 .UNSPECIFIED. ) 
 CURVE ( )  GEOMETRIC_REPRESENTATION_ITEM ( )  RATIONAL_B_SPLINE_CURVE ( ( 1.000000000000241140, 0.9510565162949122797, 1.000000000000000000, 0.9510565162951535312, 1.000000000000000000, 0.9510565162951535312, 1.000000000000000000, 0.9510565162951535312, 1.000000000000000000, 0.9510565162954009999, 0.9999999999997525313 ) ) 
 REPRESENTATION_ITEM ( '' )  );
#4360 = DIRECTION ( 'NONE',  ( -0.000000000000000000, -0.000000000000000000, 1.000000000000000000 ) ) ;
#4361 = DIRECTION ( 'NONE',  ( 0.000000000000000000, 1.000000000000000000, 0.000000000000000000 ) ) ;
#4362 = CARTESIAN_POINT ( 'NONE',  ( 0.000000000000000000, 15.74999999999997513, 4.000000000000000000 ) ) ;
#4363 = MECHANICAL_DESIGN_GEOMETRIC_PRESENTATION_REPRESENTATION (  '', ( #62775 ), #24561 ) ;
#4364 = VERTEX_POINT ( 'NONE', #6909 ) ;
#4365 = DIRECTION ( 'NONE',  ( 1.000000000000000000, 7.703719777548942317E-32, 0.000000000000000000 ) ) ;
#4366 = DIRECTION ( 'NONE',  ( 0.000000000000000000, 0.000000000000000000, 1.000000000000000000 ) ) ;
#4367 = VECTOR ( 'NONE', #47374, 1000.000000000000000 ) ;
#4368 = B_SPLINE_CURVE_WITH_KNOTS ( 'NONE', 3,
 ( #32388, #26756, #63385, #27102, #52510, #37748, #9600, #5310 ),
 .UNSPECIFIED., .F., .F.,
 ( 4, 2, 2, 4 ),
 ( 2.544316211733585141E-07, 0.002094919859796809478, 0.003142252573884625911, 0.004189585287972442777 ),
 .UNSPECIFIED. ) ;
#4369 = DIRECTION ( 'NONE',  ( 1.000000000000000000, 0.000000000000000000, 0.000000000000000000 ) ) ;
#4370 = PRESENTATION_STYLE_ASSIGNMENT (( #32746 ) ) ;
#4371 = ORIENTED_EDGE ( 'NONE', *, *, #19305, .F. ) ;
#4372 = DIRECTION ( 'NONE',  ( -1.000000000000000000, 0.000000000000000000, 0.000000000000000000 ) ) ;
#4373 = ORIENTED_EDGE ( 'NONE', *, *, #41261, .F. ) ;
#4374 = MECHANICAL_DESIGN_GEOMETRIC_PRESENTATION_REPRESENTATION (  '', ( #47131 ), #6647 ) ;
#4375 = DIRECTION ( 'NONE',  ( -1.000000000000000000, 1.224646799147349509E-16, 0.000000000000000000 ) ) ;
#4376 = FILL_AREA_STYLE ('',( #52624 ) ) ;
#4377 = CARTESIAN_POINT ( 'NONE',  ( 15.00000000000000000, 8.000000000000000000, 4.000000000000000000 ) ) ;
#4378 = CARTESIAN_POINT ( 'NONE',  ( -157.8570736234661922, -5.598654528085803328, -7.705886871421366635 ) ) ;
#4379 = EDGE_CURVE ( 'NONE', #17287, #55122, #66109, .T. ) ;
#4380 = STYLED_ITEM ( 'NONE', ( #68834 ), #33355 ) ;
#4381 = CARTESIAN_POINT ( 'NONE',  ( 5.598654528085809545, 127.1449999999999818, -7.705886871421373741 ) ) ;
#4382 = STYLED_ITEM ( 'NONE', ( #40964 ), #4768 ) ;
#4383 = CARTESIAN_POINT ( 'NONE',  ( -100.1070736234661780, 8.102448949553171076, -5.886773742842744461 ) ) ;
#4384 = TOROIDAL_SURFACE ( 'NONE', #35793, 22.50000000000000000, 0.5000000000000000000 ) ;
#4385 = LINE ( 'NONE', #53320, #49353 ) ;
#4386 = ORIENTED_EDGE ( 'NONE', *, *, #54151, .F. ) ;
#4387 = STYLED_ITEM ( 'NONE', ( #65443 ), #51434 ) ;
#4388 = CARTESIAN_POINT ( 'NONE',  ( -107.0929263765347628, 3.094860106634567565, 9.524999999988271071 ) ) ;
#4390 = SURFACE_STYLE_USAGE ( .BOTH. , #47380 ) ;
#4389 = LINE ( 'NONE', #25864, #11037 ) ;
#4391 = PRESENTATION_STYLE_ASSIGNMENT (( #57907 ) ) ;
#4392 = CARTESIAN_POINT ( 'NONE',  ( -140.4549999999999841, 7.632228543268599452, -2.479861379858951942 ) ) ;
#4393 =( NAMED_UNIT ( * ) SI_UNIT ( $, .STERADIAN. ) SOLID_ANGLE_UNIT ( ) );
#4394 = CARTESIAN_POINT ( 'NONE',  ( -24.21231517720798010, 113.4999999999999858, -7.000000000000000000 ) ) ;
#4395 = CARTESIAN_POINT ( 'NONE',  ( -151.3449999999999989, 7.632228543268599452, -2.479861379858951942 ) ) ;
#4396 = STYLED_ITEM ( 'NONE', ( #18781 ), #14878 ) ;
#4397 = CARTESIAN_POINT ( 'NONE',  ( -139.9449999999999932, -9.827790563157499189E-16, -8.024999999999991473 ) ) ;
#4398 = VERTEX_POINT ( 'NONE', #12169 ) ;
#4399 = PRESENTATION_LAYER_ASSIGNMENT (  '', '', ( #56091 ) ) ;
#4400 = CYLINDRICAL_SURFACE ( 'NONE', #14552, 0.2500000000000002220 ) ;
#4401 =( NAMED_UNIT ( * ) SI_UNIT ( $, .STERADIAN. ) SOLID_ANGLE_UNIT ( ) );
#4402 = FILL_AREA_STYLE_COLOUR ( '', #22626 ) ;
#4403 = UNCERTAINTY_MEASURE_WITH_UNIT (LENGTH_MEASURE( 1.000000000000000082E-05 ), #53576, 'distance_accuracy_value', 'NONE');
#4404 = CARTESIAN_POINT ( 'NONE',  ( -66.20499999999996987, -2.607480562269071545, -8.024999999999991473 ) ) ;
#4405 = DIRECTION ( 'NONE',  ( -5.782411586589351722E-16, 1.000000000000000000, 0.000000000000000000 ) ) ;
#4406 = CARTESIAN_POINT ( 'NONE',  ( 3.094860106618431583, 160.2050000000000125, 9.525000000000000355 ) ) ;
#4407 = DIRECTION ( 'NONE',  ( 0.000000000000000000, 1.000000000000000000, 0.000000000000000000 ) ) ;
#4408 = ADVANCED_FACE ( 'NONE', ( #65998 ), #1911, .T. ) ;
#4409 = AXIS2_PLACEMENT_3D ( 'NONE', #41376, #68429, #10395 ) ;
#4410 = UNCERTAINTY_MEASURE_WITH_UNIT (LENGTH_MEASURE( 1.000000000000000082E-05 ), #44545, 'distance_accuracy_value', 'NONE');
#4411 =( LENGTH_UNIT ( ) NAMED_UNIT ( * ) SI_UNIT ( .MILLI., .METRE. ) );
#4412 = FILL_AREA_STYLE ('',( #133 ) ) ;
#4413 = CIRCLE ( 'NONE', #60558, 1.000000000000000000 ) ;
#4414 = CARTESIAN_POINT ( 'NONE',  ( -81.95707362346617231, 9.058813317711329915, -2.943386871421373119 ) ) ;
#4415 = CARTESIAN_POINT ( 'NONE',  ( -40.99999999999998579, 107.7459666924148394, 3.500000000000000444 ) ) ;
#4416 = SURFACE_STYLE_USAGE ( .BOTH. , #63198 ) ;
#4417 = EDGE_CURVE ( 'NONE', #33237, #51630, #31314, .T. ) ;
#4418 = FACE_OUTER_BOUND ( 'NONE', #44325, .T. ) ;
#4419 = AXIS2_PLACEMENT_3D ( 'NONE', #19359, #1757, #17987 ) ;
#4420 = DIRECTION ( 'NONE',  ( -1.000000000000000000, 0.000000000000000000, 0.000000000000000000 ) ) ;
#4421 = CARTESIAN_POINT ( 'NONE',  ( -74.75000000000000000, -4.000000000000000000, 18.00000000000000000 ) ) ;
#4422 = VERTEX_POINT ( 'NONE', #55081 ) ;
#4423 = AXIS2_PLACEMENT_3D ( 'NONE', #12087, #65915, #27565 ) ;
#4424 = ORIENTED_EDGE ( 'NONE', *, *, #21022, .T. ) ;
#4425 = EDGE_CURVE ( 'NONE', #28436, #58801, #26822, .T. ) ;
#4426 = AXIS2_PLACEMENT_3D ( 'NONE', #42749, #43455, #64142 ) ;
#4427 = CARTESIAN_POINT ( 'NONE',  ( 2.755156416453792279, -1.983268963954967434, -7.000000000000002665 ) ) ;
#4428 = EDGE_CURVE ( 'NONE', #52813, #19239, #29029, .T. ) ;
#4430 = CARTESIAN_POINT ( 'NONE',  ( 2.418535808707046542, -7.000000000000002665, 0.3989014552058374741 ) ) ;
#4429 = VECTOR ( 'NONE', #32500, 1000.000000000000000 ) ;
#4431 = DIRECTION ( 'NONE',  ( 0.000000000000000000, 1.000000000000000000, 0.000000000000000000 ) ) ;
#4432 = ORIENTED_EDGE ( 'NONE', *, *, #18194, .F. ) ;
#4433 = EDGE_LOOP ( 'NONE', ( #63202, #19737, #38622, #55162 ) ) ;
#4434 = CARTESIAN_POINT ( 'NONE',  ( -108.3570736234661780, 5.598654528085804216, 7.705886871421366635 ) ) ;
#4435 = ADVANCED_FACE ( 'NONE', ( #55791 ), #33586, .T. ) ;
#4436 =( NAMED_UNIT ( * ) PLANE_ANGLE_UNIT ( ) SI_UNIT ( $, .RADIAN. ) );
#4437 = CARTESIAN_POINT ( 'NONE',  ( -7.794228634059948035, 2.500000000000000000, 4.499999999999999112 ) ) ;
#4438 = VERTEX_POINT ( 'NONE', #61734 ) ;
#4439 = CARTESIAN_POINT ( 'NONE',  ( 10.01517768586949231, 118.8049999999999926, 1.839758294383810543E-15 ) ) ;
#4440 = CARTESIAN_POINT ( 'NONE',  ( -85.79292637653378506, -3.094860106618429807, 9.524999999999991473 ) ) ;
#4441 = CARTESIAN_POINT ( 'NONE',  ( 45.00000000000000000, 10.25709351175097694, 7.000000000000000000 ) ) ;
#4442 = VECTOR ( 'NONE', #19026, 1000.000000000000000 ) ;
#4443 = DIRECTION ( 'NONE',  ( -0.000000000000000000, -1.000000000000000000, -0.000000000000000000 ) ) ;
#4444 = CARTESIAN_POINT ( 'NONE',  ( -101.9949999999999903, -6.826472737025115478, 4.959722759717900331 ) ) ;
#4445 = ORIENTED_EDGE ( 'NONE', *, *, #26740, .F. ) ;
#4446 = CIRCLE ( 'NONE', #40454, 0.5000000000000004441 ) ;
#4447 = CARTESIAN_POINT ( 'NONE',  ( -20.57648123223228254, 114.4999999999999574, -10.27659574468085069 ) ) ;
#4448 = CARTESIAN_POINT ( 'NONE',  ( 44.99999999999977973, 149.4999999999999716, -9.500000000000000000 ) ) ;
#4449 = UNCERTAINTY_MEASURE_WITH_UNIT (LENGTH_MEASURE( 1.000000000000000082E-05 ), #34662, 'distance_accuracy_value', 'NONE');
#4450 = EDGE_LOOP ( 'NONE', ( #60189, #48257, #8666, #6151 ) ) ;
#4451 = CARTESIAN_POINT ( 'NONE',  ( -6.826472737025120807, 153.9929263765338021, 4.959722759717906548 ) ) ;
#4452 = DIRECTION ( 'NONE',  ( 1.300977106640434891E-16, 0.000000000000000000, 1.000000000000000000 ) ) ;
#4453 = COLOUR_RGB ( '', 0.72549020, 0.75294118, 0.79215686) ;
#4454 = PLANE ( 'NONE',  #67086 ) ;
#4455 = ORIENTED_EDGE ( 'NONE', *, *, #570, .F. ) ;
#4456 = CARTESIAN_POINT ( 'NONE',  ( 20.35573775503900151, 114.9974703310426634, -9.999999999999998224 ) ) ;
#4457 = VERTEX_POINT ( 'NONE', #68106 ) ;
#4458 = CARTESIAN_POINT ( 'NONE',  ( 19.89974874213240597, 115.4999999999999574, 10.00000000000000000 ) ) ;
#4459 = FILL_AREA_STYLE ('',( #67828 ) ) ;
#4460 = SURFACE_STYLE_USAGE ( .BOTH. , #52695 ) ;
#4461 = CARTESIAN_POINT ( 'NONE',  ( -35.65778776279520912, -9.947368421052630083, 4.481646853389227303 ) ) ;
#4462 = CARTESIAN_POINT ( 'NONE',  ( -184.0000000000000568, -3.034060806962692425, 7.439417636962661007 ) ) ;
#4463 = PRESENTATION_LAYER_ASSIGNMENT (  '', '', ( #46103 ) ) ;
#4464 = CYLINDRICAL_SURFACE ( 'NONE', #25165, 5.000000000000000888 ) ;
#4465 =( BOUNDED_CURVE ( )  B_SPLINE_CURVE ( 2, ( #15910, #38426, #669, #5645, #6010, #64417, #5300, #58447, #26423, #37741, #27446 ),
 .UNSPECIFIED., .F., .F. ) 
 B_SPLINE_CURVE_WITH_KNOTS ( ( 3, 2, 2, 2, 2, 3 ),
 ( 0.9021739130434782705, 0.9043478260869565188, 0.9065217391304347672, 0.9086956521739130155, 0.9108695652173912638, 0.9130434782608695121 ),
 .UNSPECIFIED. ) 
 CURVE ( )  GEOMETRIC_REPRESENTATION_ITEM ( )  RATIONAL_B_SPLINE_CURVE ( ( 1.000000000000000000, 0.9510565162951535312, 1.000000000000000000, 0.9510565162951535312, 1.000000000000000000, 0.9510565162951535312, 1.000000000000000000, 0.9510565162951535312, 1.000000000000000000, 0.9510565162951535312, 1.000000000000000000 ) ) 
 REPRESENTATION_ITEM ( '' )  );
#4466 = AXIS2_PLACEMENT_3D ( 'NONE', #25371, #57389, #30632 ) ;
#4467 = FACE_OUTER_BOUND ( 'NONE', #47565, .T. ) ;
#4468 = CARTESIAN_POINT ( 'NONE',  ( 75.83633811589984930, 0.9999999999999991118, -66.72655454856717938 ) ) ;
#4469 = CARTESIAN_POINT ( 'NONE',  ( -2.607480562269020918, 120.0929263765338249, -8.025000000000037659 ) ) ;
#4470 = CARTESIAN_POINT ( 'NONE',  ( -45.96823954197535045, -12.05717624383679087, 3.207817295096130561 ) ) ;
#4471 = ORIENTED_EDGE ( 'NONE', *, *, #21273, .F. ) ;
#4472 = VERTEX_POINT ( 'NONE', #19882 ) ;
#4473 = DIRECTION ( 'NONE',  ( 0.000000000000000000, 0.000000000000000000, -1.000000000000000000 ) ) ;
#4474 = CARTESIAN_POINT ( 'NONE',  ( -24.21231517720798010, 113.4999999999999858, 7.000000000000000000 ) ) ;
#4475 = DIRECTION ( 'NONE',  ( 1.000000000000000000, 0.000000000000000000, 0.000000000000000000 ) ) ;
#4476 = CARTESIAN_POINT ( 'NONE',  ( 74.59262096826685706, 19.64589727361706650, 6.500000000000000000 ) ) ;
#4477 = ORIENTED_EDGE ( 'NONE', *, *, #15533, .T. ) ;
#4478 = CARTESIAN_POINT ( 'NONE',  ( -154.4929263765338021, -8.102448949553174629, 5.886773742842742685 ) ) ;
#4479 = CARTESIAN_POINT ( 'NONE',  ( -173.1550000000000011, 7.632228543268600340, 2.479861379858949277 ) ) ;
#4480 = CARTESIAN_POINT ( 'NONE',  ( 23.50000000000001776, 42.00000000000000000, -27.18999999999999417 ) ) ;
#4481 = SURFACE_SIDE_STYLE ('',( #25269 ) ) ;
#4482 = AXIS2_PLACEMENT_3D ( 'NONE', #44211, #17463, #51513 ) ;
#4483 = CARTESIAN_POINT ( 'NONE',  ( -49.55707362346617373, -1.166476076187852838E-15, -9.524999999999991473 ) ) ;
#4484 = COLOUR_RGB ( '', 0.72549020, 0.75294118, 0.79215686) ;
#4485 = CARTESIAN_POINT ( 'NONE',  ( -176.2449999999999761, -4.716976649647093289, -6.492361379858945902 ) ) ;
#4486 = VECTOR ( 'NONE', #1371, 1000.000000000000000 ) ;
#4487 = EDGE_LOOP ( 'NONE', ( #10166, #6476, #41292, #11420 ) ) ;
#4488 = PRESENTATION_STYLE_ASSIGNMENT (( #63935 ) ) ;
#4489 = FILL_AREA_STYLE_COLOUR ( '', #61609 ) ;
#4490 = CARTESIAN_POINT ( 'NONE',  ( -14.66572272744468641, 10.90871211463571377, 5.000000000000001776 ) ) ;
#4491 = CARTESIAN_POINT ( 'NONE',  ( -93.65499999999998693, -7.632228543268600340, -2.479861379858950166 ) ) ;
#4492 = SURFACE_STYLE_FILL_AREA ( #40801 ) ;
#4493 = AXIS2_PLACEMENT_3D ( 'NONE', #39264, #12481, #60664 ) ;
#4494 =( NAMED_UNIT ( * ) SI_UNIT ( $, .STERADIAN. ) SOLID_ANGLE_UNIT ( ) );
#4495 = CARTESIAN_POINT ( 'NONE',  ( -88.04499999999998749, 7.632228543268600340, 2.479861379858949277 ) ) ;
#4496 = CARTESIAN_POINT ( 'NONE',  ( 9.058813317711338797, 124.9549999999999841, -2.943386871421372675 ) ) ;
#4497 = CARTESIAN_POINT ( 'NONE',  ( -58.49499999999998323, 6.826472737025113702, -4.959722759717902107 ) ) ;
#4498 = DIRECTION ( 'NONE',  ( 0.000000000000000000, 0.000000000000000000, 1.000000000000000000 ) ) ;
#4499 = PRESENTATION_LAYER_ASSIGNMENT (  '', '', ( #49474 ) ) ;
#4500 = ADVANCED_FACE ( 'NONE', ( #46688 ), #29758, .T. ) ;
#4501 = CIRCLE ( 'NONE', #42737, 4.999999999999997335 ) ;
#4502 = CARTESIAN_POINT ( 'NONE',  ( 43.75000000000000000, 19.24999999999998224, 3.750000000000000000 ) ) ;
#4503 = CYLINDRICAL_SURFACE ( 'NONE', #40582, 9.524999999999991473 ) ;
#4504 = UNCERTAINTY_MEASURE_WITH_UNIT (LENGTH_MEASURE( 1.000000000000000082E-05 ), #53360, 'distance_accuracy_value', 'NONE');
#4505 = PRESENTATION_LAYER_ASSIGNMENT (  '', '', ( #43887 ) ) ;
#4506 = EDGE_CURVE ( 'NONE', #3957, #7058, #3316, .T. ) ;
#4507 = CARTESIAN_POINT ( 'NONE',  ( -1.233556390963996163, -2.406758536253310155, -7.000000000000001776 ) ) ;
#4508 = SURFACE_STYLE_FILL_AREA ( #8775 ) ;
#4509 = ADVANCED_FACE ( 'NONE', ( #35735 ), #57893, .F. ) ;
#4510 = ORIENTED_EDGE ( 'NONE', *, *, #43270, .T. ) ;
#4511 = FACE_OUTER_BOUND ( 'NONE', #28390, .T. ) ;
#4512 = AXIS2_PLACEMENT_3D ( 'NONE', #51247, #68463, #52646 ) ;
#4513 = EDGE_CURVE ( 'NONE', #44423, #631, #64997, .T. ) ;
#4514 = ADVANCED_FACE ( 'NONE', ( #40683, #25855 ), #62097, .F. ) ;
#4515 = SURFACE_STYLE_USAGE ( .BOTH. , #47503 ) ;
#4516 = EDGE_CURVE ( 'NONE', #64993, #46369, #51557, .T. ) ;
#4518 = CARTESIAN_POINT ( 'NONE',  ( -34.99999999999999289, 99.99999999999998579, -7.500000000000000000 ) ) ;
#4517 = DIRECTION ( 'NONE',  ( 1.000000000000000000, 0.000000000000000000, -0.000000000000000000 ) ) ;
#4519 = DIRECTION ( 'NONE',  ( 3.469446951953611033E-15, -1.000000000000000000, 0.000000000000000000 ) ) ;
#4520 = ORIENTED_EDGE ( 'NONE', *, *, #28307, .F. ) ;
#4521 = ORIENTED_EDGE ( 'NONE', *, *, #16322, .T. ) ;
#4522 = DIRECTION ( 'NONE',  ( 1.000000000000000000, -0.000000000000000000, 0.000000000000000000 ) ) ;
#4523 = MECHANICAL_DESIGN_GEOMETRIC_PRESENTATION_REPRESENTATION (  '', ( #34872 ), #67443 ) ;
#4524 = UNCERTAINTY_MEASURE_WITH_UNIT (LENGTH_MEASURE( 1.000000000000000082E-05 ), #59042, 'distance_accuracy_value', 'NONE');
#4525 = AXIS2_PLACEMENT_3D ( 'NONE', #17621, #60155, #55913 ) ;
#4526 = ADVANCED_FACE ( 'NONE', ( #26546 ), #17073, .T. ) ;
#4527 = AXIS2_PLACEMENT_3D ( 'NONE', #38819, #44106, #1779 ) ;
#4528 = CARTESIAN_POINT ( 'NONE',  ( -9.827790563157511022E-16, 148.4429263765338476, 8.025000000000000355 ) ) ;
#4529 = DIRECTION ( 'NONE',  ( -1.000000000000000000, 0.000000000000000000, 0.000000000000000000 ) ) ;
#4530 = DIRECTION ( 'NONE',  ( 0.000000000000000000, 0.000000000000000000, 1.000000000000000000 ) ) ;
#4531 = ORIENTED_EDGE ( 'NONE', *, *, #10269, .F. ) ;
#4532 = CARTESIAN_POINT ( 'NONE',  ( -117.8049999999999926, -8.437984349512086979, 5.166775262442717831E-16 ) ) ;
#4533 = ORIENTED_EDGE ( 'NONE', *, *, #35808, .T. ) ;
#4534 = DIRECTION ( 'NONE',  ( -1.734723475976805714E-15, -5.782411586589310307E-16, -1.000000000000000000 ) ) ;
#4535 = CARTESIAN_POINT ( 'NONE',  ( 6.826472737025119919, 129.0070736234661695, 4.959722759717908325 ) ) ;
#4536 = ORIENTED_EDGE ( 'NONE', *, *, #8589, .F. ) ;
#4537 = FILL_AREA_STYLE ('',( #10874 ) ) ;
#4538 = DIRECTION ( 'NONE',  ( -0.000000000000000000, -0.000000000000000000, -1.000000000000000000 ) ) ;
#4539 = ORIENTED_EDGE ( 'NONE', *, *, #51635, .T. ) ;
#4540 =( GEOMETRIC_REPRESENTATION_CONTEXT ( 3 ) GLOBAL_UNCERTAINTY_ASSIGNED_CONTEXT ( ( #1106 ) ) GLOBAL_UNIT_ASSIGNED_CONTEXT ( ( #415, #15315, #31425 ) ) REPRESENTATION_CONTEXT ( 'NONE', 'WORKASPACE' ) );
#4541 = STYLED_ITEM ( 'NONE', ( #68895 ), #11453 ) ;
#4542 = CARTESIAN_POINT ( 'NONE',  ( 8.246138225238281549, 2.499999999999997780, 3.717269627651450303 ) ) ;
#4543 = CARTESIAN_POINT ( 'NONE',  ( 3.094860106618435136, 148.2949999999999307, -9.525000000000000355 ) ) ;
#4544 = DIRECTION ( 'NONE',  ( 0.000000000000000000, 0.000000000000000000, -1.000000000000000000 ) ) ;
#4545 = ORIENTED_EDGE ( 'NONE', *, *, #69589, .T. ) ;
#4546 = CARTESIAN_POINT ( 'NONE',  ( -55.40707362346616094, 3.094860106618428031, -9.524999999999993250 ) ) ;
#4547 = CARTESIAN_POINT ( 'NONE',  ( -8.102448949553179958, 153.0049999999999955, -5.886773742842749790 ) ) ;
#4548 = CARTESIAN_POINT ( 'NONE',  ( -135.2070736234667550, 3.094860106628449792, 9.524999999992715516 ) ) ;
#4549 = VECTOR ( 'NONE', #68476, 1000.000000000000000 ) ;
#4550 = FACE_OUTER_BOUND ( 'NONE', #6117, .T. ) ;
#4551 = EDGE_LOOP ( 'NONE', ( #49049, #66038, #717, #65347, #64530, #68335 ) ) ;
#4552 = CARTESIAN_POINT ( 'NONE',  ( 0.000000000000000000, 128.9429263765338192, -8.025000000000000355 ) ) ;
#4553 = LINE ( 'NONE', #15166, #65991 ) ;
#4554 = UNCERTAINTY_MEASURE_WITH_UNIT (LENGTH_MEASURE( 1.000000000000000082E-05 ), #42301, 'distance_accuracy_value', 'NONE');
#4555 = CARTESIAN_POINT ( 'NONE',  ( -75.37259712596974737, 36.06274621594484842, -9.736487711843981430 ) ) ;
#4556 = AXIS2_PLACEMENT_3D ( 'NONE', #1087, #17380, #43773 ) ;
#4557 = CARTESIAN_POINT ( 'NONE',  ( -44.50000000000000000, 99.99999999999998579, 3.500000000000000000 ) ) ;
#4558 = DIRECTION ( 'NONE',  ( 0.7292845505553197105, 0.6842105263157864936, -0.000000000000000000 ) ) ;
#4559 = EDGE_LOOP ( 'NONE', ( #7169, #67659 ) ) ;
#4560 = COLOUR_RGB ( '', 0.08235294, 0.09019608, 0.10196078) ;
#4561 = CARTESIAN_POINT ( 'NONE',  ( 0.000000000000000000, 87.30187232391182306, 0.000000000000000000 ) ) ;
#4562 = ORIENTED_EDGE ( 'NONE', *, *, #29613, .T. ) ;
#4563 = CARTESIAN_POINT ( 'NONE',  ( -54.44292637653380496, -1.166476076187852838E-15, -9.524999999999991473 ) ) ;
#4564 = DIRECTION ( 'NONE',  ( 0.000000000000000000, 0.000000000000000000, 1.000000000000000000 ) ) ;
#4565 = CARTESIAN_POINT ( 'NONE',  ( -155.1550000000000011, 7.632228543268600340, 2.479861379858949277 ) ) ;
#4566 = ORIENTED_EDGE ( 'NONE', *, *, #32640, .T. ) ;
#4567 = UNCERTAINTY_MEASURE_WITH_UNIT (LENGTH_MEASURE( 1.000000000000000082E-05 ), #18889, 'distance_accuracy_value', 'NONE');
#4568 = EDGE_CURVE ( 'NONE', #49089, #40754, #35853, .T. ) ;
#4569 = FILL_AREA_STYLE ('',( #9546 ) ) ;
#4570 = CARTESIAN_POINT ( 'NONE',  ( -53.38227578680366037, -9.152876382972605640, 5.508355886455341022 ) ) ;
#4571 = CARTESIAN_POINT ( 'NONE',  ( -69.59292637653379643, -3.094860106618431139, -9.524999999999991473 ) ) ;
#4572 = DIRECTION ( 'NONE',  ( -1.000000000000000000, 0.000000000000000000, 0.000000000000000000 ) ) ;
#4573 = ORIENTED_EDGE ( 'NONE', *, *, #67515, .T. ) ;
#4574 = PRESENTATION_LAYER_ASSIGNMENT (  '', '', ( #11315 ) ) ;
#4575 = VERTEX_POINT ( 'NONE', #5770 ) ;
#4576 = CARTESIAN_POINT ( 'NONE',  ( 22.65098652982589300, 24.94475854255456326, 27.33790873936361621 ) ) ;
#4577 = LINE ( 'NONE', #58756, #67087 ) ;
#4578 = CARTESIAN_POINT ( 'NONE',  ( -64.70499999999998408, 2.607480562269073321, 8.024999999999991473 ) ) ;
#4579 = VERTEX_POINT ( 'NONE', #27216 ) ;
#4580 = CARTESIAN_POINT ( 'NONE',  ( 55.89999999999999147, 11.99999999999999822, 4.000000000000000000 ) ) ;
#4581 = CARTESIAN_POINT ( 'NONE',  ( 0.000000000000000000, 0.000000000000000000, 0.000000000000000000 ) ) ;
#4582 = AXIS2_PLACEMENT_3D ( 'NONE', #31953, #27681, #43596 ) ;
#4583 = DIRECTION ( 'NONE',  ( 0.000000000000000000, -1.000000000000000000, 0.000000000000000000 ) ) ;
#4584 = PLANE ( 'NONE',  #61168 ) ;
#4585 = EDGE_LOOP ( 'NONE', ( #55170, #13122, #24697, #17376 ) ) ;
#4586 = STYLED_ITEM ( 'NONE', ( #34916 ), #45142 ) ;
#4587 = DIRECTION ( 'NONE',  ( 0.000000000000000000, 1.000000000000000000, 0.000000000000000000 ) ) ;
#4588 = DIRECTION ( 'NONE',  ( 1.000000000000000000, 0.000000000000000000, 0.000000000000000000 ) ) ;
#4589 = FILL_AREA_STYLE ('',( #47929 ) ) ;
#4591 = FACE_OUTER_BOUND ( 'NONE', #13665, .T. ) ;
#4590 = LINE ( 'NONE', #62311, #16654 ) ;
#4592 = PRESENTATION_LAYER_ASSIGNMENT (  '', '', ( #30433 ) ) ;
#4593 = EDGE_CURVE ( 'NONE', #60087, #27592, #20945, .T. ) ;
#4594 = CARTESIAN_POINT ( 'NONE',  ( -118.6449999999999818, 4.716976649647091513, -6.492361379858946790 ) ) ;
#4595 = CARTESIAN_POINT ( 'NONE',  ( -5.598654528085806881, 148.7449999999999761, -7.705886871421374629 ) ) ;
#4596 = CARTESIAN_POINT ( 'NONE',  ( -101.6949999999999790, -8.437984349512085203, 5.166775262442717831E-16 ) ) ;
#4597 = CIRCLE ( 'NONE', #42867, 0.4999999999999994449 ) ;
#4598 = DIRECTION ( 'NONE',  ( 1.000000000000000000, 0.000000000000000000, 0.000000000000000000 ) ) ;
#4599 = DIRECTION ( 'NONE',  ( -1.000000000000000000, 0.000000000000000000, 0.000000000000000000 ) ) ;
#4600 = STYLED_ITEM ( 'NONE', ( #18140 ), #34863 ) ;
#4601 = UNCERTAINTY_MEASURE_WITH_UNIT (LENGTH_MEASURE( 1.000000000000000082E-05 ), #7400, 'distance_accuracy_value', 'NONE');
#4602 = EDGE_CURVE ( 'NONE', #4230, #4175, #58287, .T. ) ;
#4603 = VECTOR ( 'NONE', #28377, 1000.000000000000000 ) ;
#4604 =( NAMED_UNIT ( * ) PLANE_ANGLE_UNIT ( ) SI_UNIT ( $, .RADIAN. ) );
#4605 = ORIENTED_EDGE ( 'NONE', *, *, #8626, .T. ) ;
#4606 = CARTESIAN_POINT ( 'NONE',  ( -134.6929263765337907, 10.01517768586948698, -1.839758294383808571E-15 ) ) ;
#4607 = LINE ( 'NONE', #20085, #23120 ) ;
#4608 = CARTESIAN_POINT ( 'NONE',  ( -158.3949999999999818, -6.826472737025115478, -4.959722759717899443 ) ) ;
#4610 = DIRECTION ( 'NONE',  ( -1.000000000000000000, 0.000000000000000000, 0.000000000000000000 ) ) ;
#4609 = CIRCLE ( 'NONE', #13592, 26.99999999999999645 ) ;
#4611 = VECTOR ( 'NONE', #21345, 1000.000000000000000 ) ;
#4612 = EDGE_CURVE ( 'NONE', #29580, #6296, #16391, .T. ) ;
#4613 = CARTESIAN_POINT ( 'NONE',  ( -133.1929263765337623, -10.01517768586948698, 6.132527647946031529E-16 ) ) ;
#4614 = ORIENTED_EDGE ( 'NONE', *, *, #31995, .F. ) ;
#4615 = ORIENTED_EDGE ( 'NONE', *, *, #39985, .T. ) ;
#4616 = STYLED_ITEM ( 'NONE', ( #42405 ), #17272 ) ;
#4617 = LINE ( 'NONE', #10267, #52135 ) ;
#4618 = EDGE_CURVE ( 'NONE', #42104, #23846, #64599, .T. ) ;
#4619 = CARTESIAN_POINT ( 'NONE',  ( -143.3929263765338078, 8.102448949553176405, 5.886773742842740909 ) ) ;
#4620 = CARTESIAN_POINT ( 'NONE',  ( -45.00000000000000000, 9.027119726910822095, 6.778758691516320489 ) ) ;
#4621 =( GEOMETRIC_REPRESENTATION_CONTEXT ( 3 ) GLOBAL_UNCERTAINTY_ASSIGNED_CONTEXT ( ( #40360 ) ) GLOBAL_UNIT_ASSIGNED_CONTEXT ( ( #37, #69421, #64824 ) ) REPRESENTATION_CONTEXT ( 'NONE', 'WORKASPACE' ) );
#4622 = AXIS2_PLACEMENT_3D ( 'NONE', #21106, #11588, #32007 ) ;
#4623 = SURFACE_STYLE_FILL_AREA ( #36700 ) ;
#4624 = ORIENTED_EDGE ( 'NONE', *, *, #16570, .T. ) ;
#4625 = CARTESIAN_POINT ( 'NONE',  ( -150.8050000000000068, -8.437984349512086979, 5.166775262442717831E-16 ) ) ;
#4626 = ORIENTED_EDGE ( 'NONE', *, *, #24067, .F. ) ;
#4627 = DIRECTION ( 'NONE',  ( -0.000000000000000000, -1.000000000000000000, -0.000000000000000000 ) ) ;
#4628 = ORIENTED_EDGE ( 'NONE', *, *, #20178, .F. ) ;
#4629 = CIRCLE ( 'NONE', #24857, 7.000000000000001776 ) ;
#4630 = FILL_AREA_STYLE ('',( #20475 ) ) ;
#4631 = DIRECTION ( 'NONE',  ( -0.000000000000000000, -0.000000000000000000, -1.000000000000000000 ) ) ;
#4632 = CARTESIAN_POINT ( 'NONE',  ( -5.598654528085806881, 118.7449999999999903, -7.705886871421374629 ) ) ;
#4633 =( NAMED_UNIT ( * ) PLANE_ANGLE_UNIT ( ) SI_UNIT ( $, .RADIAN. ) );
#4634 = ORIENTED_EDGE ( 'NONE', *, *, #25431, .T. ) ;
#4635 = AXIS2_PLACEMENT_3D ( 'NONE', #6887, #28313, #49819 ) ;
#4636 = CARTESIAN_POINT ( 'NONE',  ( 45.00000000000000000, -1.469576158976824618E-14, 10.00000000000000000 ) ) ;
#4637 = CARTESIAN_POINT ( 'NONE',  ( 5.598654528085809545, 119.2549999999999812, -7.705886871421373741 ) ) ;
#4638 = MECHANICAL_DESIGN_GEOMETRIC_PRESENTATION_REPRESENTATION (  '', ( #58576 ), #45116 ) ;
#4639 = CARTESIAN_POINT ( 'NONE',  ( -59.75499999999998835, 4.716976649647091513, -6.492361379858946790 ) ) ;
#4640 = DIRECTION ( 'NONE',  ( 0.000000000000000000, 0.000000000000000000, 1.000000000000000000 ) ) ;
#4641 = ORIENTED_EDGE ( 'NONE', *, *, #24134, .F. ) ;
#4642 = CARTESIAN_POINT ( 'NONE',  ( -9.058813317711338797, 147.4550000000000125, 2.943386871421373563 ) ) ;
#4643 = UNCERTAINTY_MEASURE_WITH_UNIT (LENGTH_MEASURE( 1.000000000000000082E-05 ), #54692, 'distance_accuracy_value', 'NONE');
#4644 = CARTESIAN_POINT ( 'NONE',  ( -183.0259559770162809, -0.7697107438453818506, 9.475620892396962702 ) ) ;
#4645 = CIRCLE ( 'NONE', #42913, 0.5000000000000004441 ) ;
#4646 = CARTESIAN_POINT ( 'NONE',  ( 21.02379604162874926, 114.4999999999999574, 10.00000000000000000 ) ) ;
#4647 = DIRECTION ( 'NONE',  ( 0.000000000000000000, 0.000000000000000000, -1.000000000000000000 ) ) ;
#4648 = AXIS2_PLACEMENT_3D ( 'NONE', #64682, #59735, #11542 ) ;
#4649 = ORIENTED_EDGE ( 'NONE', *, *, #68979, .T. ) ;
#4650 = DIRECTION ( 'NONE',  ( -1.000000000000000000, 0.000000000000000000, 0.000000000000000000 ) ) ;
#4651 = CARTESIAN_POINT ( 'NONE',  ( 0.000000000000000000, 33.74999999999998579, 3.750000000000000000 ) ) ;
#4652 = CARTESIAN_POINT ( 'NONE',  ( -179.3049999999999784, 8.437984349512085203, -1.550032578732815448E-15 ) ) ;
#4654 = VERTEX_POINT ( 'NONE', #10735 ) ;
#4653 = AXIS2_PLACEMENT_3D ( 'NONE', #51197, #50844, #2599 ) ;
#4655 = CARTESIAN_POINT ( 'NONE',  ( -47.50000000000000000, 99.99999999999992895, -10.00000000000000000 ) ) ;
#4656 = ADVANCED_FACE ( 'NONE', ( #53969, #49092 ), #31472, .T. ) ;
#4657 = MECHANICAL_DESIGN_GEOMETRIC_PRESENTATION_REPRESENTATION (  '', ( #21483 ), #37297 ) ;
#4658 = FACE_OUTER_BOUND ( 'NONE', #11839, .T. ) ;
#4659 = DIRECTION ( 'NONE',  ( -0.000000000000000000, -0.000000000000000000, 1.000000000000000000 ) ) ;
#4660 = ORIENTED_EDGE ( 'NONE', *, *, #59155, .F. ) ;
#4661 = DIRECTION ( 'NONE',  ( -1.000000000000000000, 0.000000000000000000, 0.000000000000000000 ) ) ;
#4662 = DIRECTION ( 'NONE',  ( 0.000000000000000000, 0.000000000000000000, 1.000000000000000000 ) ) ;
#4663 = COLOUR_RGB ( '', 0.09019608, 0.27058824, 0.51372549) ;
#4664 = ORIENTED_EDGE ( 'NONE', *, *, #35447, .T. ) ;
#4665 = CARTESIAN_POINT ( 'NONE',  ( -92.75499999999999545, 4.716976649647091513, -6.492361379858946790 ) ) ;
#4666 = EDGE_LOOP ( 'NONE', ( #60747, #58132, #63138 ) ) ;
#4667 = FACE_OUTER_BOUND ( 'NONE', #57367, .T. ) ;
#4668 = VECTOR ( 'NONE', #50869, 1000.000000000000000 ) ;
#4669 = LINE ( 'NONE', #379, #14557 ) ;
#4670 = CARTESIAN_POINT ( 'NONE',  ( -132.3570736234661922, 5.598654528085804216, 7.705886871421366635 ) ) ;
#4671 = PRESENTATION_STYLE_ASSIGNMENT (( #52550 ) ) ;
#4672 = CARTESIAN_POINT ( 'NONE',  ( 0.000000000000000000, 154.4449999999999932, -9.525000000000000355 ) ) ;
#4673 = CARTESIAN_POINT ( 'NONE',  ( -77.75707362346618368, -5.598654528085801552, 7.705886871421367523 ) ) ;
#4674 = PRODUCT_RELATED_PRODUCT_CATEGORY ( 'part', '', ( #25974 ) ) ;
#4675 = EDGE_CURVE ( 'NONE', #46607, #16845, #27927, .T. ) ;
#4676 = DIRECTION ( 'NONE',  ( -0.000000000000000000, -0.000000000000000000, -1.000000000000000000 ) ) ;
#4677 = ORIENTED_EDGE ( 'NONE', *, *, #22574, .T. ) ;
#4678 = VECTOR ( 'NONE', #1348, 1000.000000000000000 ) ;
#4679 = CARTESIAN_POINT ( 'NONE',  ( -8.082903768654761123, 2.500000000000000000, -1.781658826789683271E-15 ) ) ;
#4680 = ADVANCED_FACE ( 'NONE', ( #47743 ), #69139, .F. ) ;
#4681 = CARTESIAN_POINT ( 'NONE',  ( -111.6549999999999869, -7.632228543268600340, -2.479861379858950166 ) ) ;
#4682 = EDGE_CURVE ( 'NONE', #67303, #37663, #2170, .T. ) ;
#4683 = CARTESIAN_POINT ( 'NONE',  ( -8.102448949553181734, 116.4949999999999761, 5.886773742842747126 ) ) ;
#4684 = CARTESIAN_POINT ( 'NONE',  ( -130.0449999999999875, 7.632228543268600340, 2.479861379858949277 ) ) ;
#4685 = CARTESIAN_POINT ( 'NONE',  ( -112.4070736234670989, 3.094860106603908090, -9.525000000010546586 ) ) ;
#4686 =( BOUNDED_SURFACE ( )  B_SPLINE_SURFACE ( 3, 2, ( 
 ( #15085, #15427, #4461 ),
 ( #58302, #31559, #36885 ),
 ( #57975, #5170, #63911 ),
 ( #53039, #46771, #48137 ),
 ( #68519, #68182, #20317 ),
 ( #26616, #31201, #69544 ),
 ( #21348, #19960, #60030 ),
 ( #32967, #54734, #39303 ) ),
 .UNSPECIFIED., .F., .F., .F. ) 
 B_SPLINE_SURFACE_WITH_KNOTS ( ( 4, 2, 2, 4 ),
 ( 3, 3 ),
 ( 3.931838538365183044, 4.126976148870059369, 4.322113759374936137, 4.712388980384689674 ),
 ( 0.000000000000000000, 1.000000000000000000 ),
 .UNSPECIFIED. ) 
 GEOMETRIC_REPRESENTATION_ITEM ( )  RATIONAL_B_SPLINE_SURFACE ( (
 ( 1.000000000000000000, 0.8674236696762900323, 1.000000000000000000),
 ( 1.000000000000000000, 0.8861805033181661129, 1.000000000000000000),
 ( 1.000000000000000000, 0.9042436661780808294, 1.000000000000000000),
 ( 1.000000000000000000, 0.9367862960115365123, 1.000000000000000000),
 ( 1.000000000000000000, 0.9512556414920706471, 1.000000000000000000),
 ( 1.000000000000000000, 0.9868976895440315644, 1.000000000000000000),
 ( 1.000000000000000000, 1.000154660590196087, 1.000000000000000000),
 ( 1.000000000000000000, 1.000000000000000000, 1.000000000000000000) ) ) 
 REPRESENTATION_ITEM ( '' )  SURFACE ( )  );
#4687 = CARTESIAN_POINT ( 'NONE',  ( -118.7929263765346377, -3.094860106604648831, 9.525000000010006573 ) ) ;
#4688 = AXIS2_PLACEMENT_3D ( 'NONE', #68085, #36068, #30068 ) ;
#4689 = EDGE_CURVE ( 'NONE', #62990, #56887, #2542, .T. ) ;
#4690 = ORIENTED_EDGE ( 'NONE', *, *, #60406, .T. ) ;
#4691 = VECTOR ( 'NONE', #42992, 1000.000000000000000 ) ;
#4692 = CARTESIAN_POINT ( 'NONE',  ( -160.9429263765338192, 0.000000000000000000, 9.524999999999991473 ) ) ;
#4693 =( GEOMETRIC_REPRESENTATION_CONTEXT ( 3 ) GLOBAL_UNCERTAINTY_ASSIGNED_CONTEXT ( ( #6796 ) ) GLOBAL_UNIT_ASSIGNED_CONTEXT ( ( #39712, #51986, #25232 ) ) REPRESENTATION_CONTEXT ( 'NONE', 'WORKASPACE' ) );
#4694 = EDGE_CURVE ( 'NONE', #66883, #50598, #68441, .T. ) ;
#4695 = VECTOR ( 'NONE', #52480, 1000.000000000000000 ) ;
#4696 = SURFACE_SIDE_STYLE ('',( #403 ) ) ;
#4697 = TOROIDAL_SURFACE ( 'NONE', #35028, 0.5000000000000000000, 0.2500000000000000000 ) ;
#4698 = ADVANCED_FACE ( 'NONE', ( #54997 ), #55367, .T. ) ;
#4699 = CARTESIAN_POINT ( 'NONE',  ( 53.24999999999999289, 27.74999999999998579, -4.000000000000000000 ) ) ;
#4700 = CARTESIAN_POINT ( 'NONE',  ( 18.25000000000000711, 31.24999999999999289, -3.750000000000000000 ) ) ;
#4701 = CARTESIAN_POINT ( 'NONE',  ( 75.00000000000000000, -2.215169945516535778E-14, -9.500000000000000000 ) ) ;
#4702 = ORIENTED_EDGE ( 'NONE', *, *, #42406, .T. ) ;
#4703 = STYLED_ITEM ( 'NONE', ( #50253 ), #35510 ) ;
#4704 = CARTESIAN_POINT ( 'NONE',  ( -72.29292637653379927, 3.094860106618428031, -9.524999999999993250 ) ) ;
#4705 = CONTEXT_DEPENDENT_SHAPE_REPRESENTATION ( #56321, #6472 ) ;
#4706 = CARTESIAN_POINT ( 'NONE',  ( 6.999798566743346662, 9.396926207859090496, 12.50000000000000000 ) ) ;
#4707 = DIRECTION ( 'NONE',  ( -0.000000000000000000, -0.000000000000000000, 1.000000000000000000 ) ) ;
#4708 = EDGE_CURVE ( 'NONE', #25004, #599, #20167, .T. ) ;
#4709 = FACE_OUTER_BOUND ( 'NONE', #39849, .T. ) ;
#4710 = CARTESIAN_POINT ( 'NONE',  ( -9.827790563157511022E-16, 149.5570736234661524, 8.025000000000000355 ) ) ;
#4711 = VECTOR ( 'NONE', #29260, 1000.000000000000000 ) ;
#4712 = CARTESIAN_POINT ( 'NONE',  ( -177.0549999999999784, -9.827790563157499189E-16, -8.024999999999991473 ) ) ;
#4713 = AXIS2_PLACEMENT_3D ( 'NONE', #29838, #67131, #3767 ) ;
#4714 = ORIENTED_EDGE ( 'NONE', *, *, #13741, .T. ) ;
#4715 = AXIS2_PLACEMENT_3D ( 'NONE', #5962, #16564, #1681 ) ;
#4716 = DIRECTION ( 'NONE',  ( -1.000000000000000000, -2.168404344971006896E-16, 0.000000000000000000 ) ) ;
#4717 = DIRECTION ( 'NONE',  ( 0.000000000000000000, 8.673617379884035472E-16, -1.000000000000000000 ) ) ;
#4718 = ORIENTED_EDGE ( 'NONE', *, *, #40463, .T. ) ;
#4719 = FACE_OUTER_BOUND ( 'NONE', #65087, .T. ) ;
#4720 = CARTESIAN_POINT ( 'NONE',  ( -2.607480562269075097, 146.4070736234661183, 8.025000000000000355 ) ) ;
#4721 = MECHANICAL_DESIGN_GEOMETRIC_PRESENTATION_REPRESENTATION (  '', ( #45237 ), #63181 ) ;
#4722 = ORIENTED_EDGE ( 'NONE', *, *, #36084, .T. ) ;
#4723 = CARTESIAN_POINT ( 'NONE',  ( 45.00000000000000000, 10.69371294336137979, -4.000000000000000000 ) ) ;
#4724 = CARTESIAN_POINT ( 'NONE',  ( -96.20499999999996987, -2.607480562269071545, -8.024999999999991473 ) ) ;
#4725 = UNCERTAINTY_MEASURE_WITH_UNIT (LENGTH_MEASURE( 1.000000000000000082E-05 ), #40644, 'distance_accuracy_value', 'NONE');
#4726 = AXIS2_PLACEMENT_3D ( 'NONE', #23546, #28458, #55569 ) ;
#4727 = ORIENTED_EDGE ( 'NONE', *, *, #69644, .T. ) ;
#4728 = SURFACE_STYLE_FILL_AREA ( #57150 ) ;
#4729 = ORIENTED_EDGE ( 'NONE', *, *, #17795, .T. ) ;
#4730 = CIRCLE ( 'NONE', #62020, 17.00000000000000000 ) ;
#4731 = CARTESIAN_POINT ( 'NONE',  ( -13.23915246117191025, 52.65078610323165265, 6.947530358905294356 ) ) ;
#4732 = CARTESIAN_POINT ( 'NONE',  ( -74.84499999999998465, -7.632228543268599452, 2.479861379858951054 ) ) ;
#4733 = VERTEX_POINT ( 'NONE', #7191 ) ;
#4734 =( NAMED_UNIT ( * ) PLANE_ANGLE_UNIT ( ) SI_UNIT ( $, .RADIAN. ) );
#4735 = CARTESIAN_POINT ( 'NONE',  ( 44.25000000000000000, 21.74999999999998579, -3.750000000000000000 ) ) ;
#4736 = AXIS2_PLACEMENT_3D ( 'NONE', #44717, #66108, #6335 ) ;
#4737 = VERTEX_POINT ( 'NONE', #1496 ) ;
#4738 = FACE_OUTER_BOUND ( 'NONE', #14478, .T. ) ;
#4739 = LINE ( 'NONE', #57887, #69609 ) ;
#4740 = AXIS2_PLACEMENT_3D ( 'NONE', #27280, #60011, #11477 ) ;
#4741 =( LENGTH_UNIT ( ) NAMED_UNIT ( * ) SI_UNIT ( .MILLI., .METRE. ) );
#4742 = DIRECTION ( 'NONE',  ( 0.000000000000000000, 0.000000000000000000, 1.000000000000000000 ) ) ;
#4743 = ORIENTED_EDGE ( 'NONE', *, *, #25562, .T. ) ;
#4744 = COLOUR_RGB ( '', 0.08235294, 0.09019608, 0.10196078) ;
#4745 = DIRECTION ( 'NONE',  ( 0.000000000000000000, 0.000000000000000000, 1.000000000000000000 ) ) ;
#4746 = VERTEX_POINT ( 'NONE', #18086 ) ;
#4747 = CARTESIAN_POINT ( 'NONE',  ( 17.75000000000000711, 31.24999999999999289, 4.000000000000000000 ) ) ;
#4748 = DIRECTION ( 'NONE',  ( -1.000000000000000000, 0.000000000000000000, 1.300977106640434891E-16 ) ) ;
#4749 = CARTESIAN_POINT ( 'NONE',  ( -41.84210526315788314, 107.2928455055531600, 4.000000000000000000 ) ) ;
#4750 = CARTESIAN_POINT ( 'NONE',  ( -156.8070736234661524, 10.01517768586948698, -1.839758294383808571E-15 ) ) ;
#4751 = CARTESIAN_POINT ( 'NONE',  ( 3.094860106618431583, 123.0949999999999704, 9.525000000000000355 ) ) ;
#4752 = CARTESIAN_POINT ( 'NONE',  ( -99.35707362346617799, 5.598654528085804216, 7.705886871421366635 ) ) ;
#4753 = AXIS2_PLACEMENT_3D ( 'NONE', #38353, #28408, #607 ) ;
#4754 = ADVANCED_FACE ( 'NONE', ( #34593 ), #56049, .F. ) ;
#4755 = FILL_AREA_STYLE ('',( #46332 ) ) ;
#4756 = ORIENTED_EDGE ( 'NONE', *, *, #60335, .F. ) ;
#4757 = CARTESIAN_POINT ( 'NONE',  ( 9.000000000000003553, 24.74999999999998579, -3.750000000000000000 ) ) ;
#4758 = EDGE_CURVE ( 'NONE', #11331, #69112, #59476, .T. ) ;
#4760 =( LENGTH_UNIT ( ) NAMED_UNIT ( * ) SI_UNIT ( .MILLI., .METRE. ) );
#4759 = DIRECTION ( 'NONE',  ( 0.000000000000000000, 0.000000000000000000, -1.000000000000000000 ) ) ;
#4761 = DIRECTION ( 'NONE',  ( 0.000000000000000000, 0.000000000000000000, -1.000000000000000000 ) ) ;
#4762 = ADVANCED_FACE ( 'NONE', ( #67310, #3591, #41652 ), #24723, .F. ) ;
#4763 = COLOUR_RGB ( '', 0.09019608, 0.27058824, 0.51372549) ;
#4764 = CARTESIAN_POINT ( 'NONE',  ( -141.3550000000000182, -4.716976649647093289, -6.492361379858945902 ) ) ;
#4765 = CARTESIAN_POINT ( 'NONE',  ( -87.05707362346618083, 0.000000000000000000, 9.524999999999991473 ) ) ;
#4766 = CARTESIAN_POINT ( 'NONE',  ( 0.000000000000000000, 87.30187232391182306, 0.000000000000000000 ) ) ;
#4767 = AXIS2_PLACEMENT_3D ( 'NONE', #29770, #6921, #40696 ) ;
#4768 = ADVANCED_FACE ( 'NONE', ( #68027 ), #30015, .T. ) ;
#4769 = CARTESIAN_POINT ( 'NONE',  ( -151.7949999999999591, 2.607480562269068880, -8.024999999999993250 ) ) ;
#4770 = CARTESIAN_POINT ( 'NONE',  ( -134.3949999999999250, -6.826472737025113702, -4.959722759717900331 ) ) ;
#4771 = VERTEX_POINT ( 'NONE', #57096 ) ;
#4772 = CARTESIAN_POINT ( 'NONE',  ( -181.1070736234661354, 8.102448949553172852, -5.886773742842744461 ) ) ;
#4773 = AXIS2_PLACEMENT_3D ( 'NONE', #42708, #43737, #32430 ) ;
#4774 = DIRECTION ( 'NONE',  ( 1.000000000000000000, 0.000000000000000000, 0.000000000000000000 ) ) ;
#4775 = CARTESIAN_POINT ( 'NONE',  ( -83.49999999999997158, 50.00000000000000000, 11.50000000000000000 ) ) ;
#4776 = CARTESIAN_POINT ( 'NONE',  ( -51.65499999999997982, -7.632228543268600340, -2.479861379858950166 ) ) ;
#4777 = CIRCLE ( 'NONE', #13776, 0.2500000000000002220 ) ;
#4778 = EDGE_CURVE ( 'NONE', #3748, #39091, #61674, .T. ) ;
#4779 = CARTESIAN_POINT ( 'NONE',  ( -5.598654528085808657, 153.7549999999999670, 7.705886871421373741 ) ) ;
#4780 = SURFACE_SIDE_STYLE ('',( #52987 ) ) ;
#4781 = DIRECTION ( 'NONE',  ( 4.336808689941999001E-16, 1.000000000000000000, -0.000000000000000000 ) ) ;
#4782 = MECHANICAL_DESIGN_GEOMETRIC_PRESENTATION_REPRESENTATION (  '', ( #42058 ), #17174 ) ;
#4783 = CIRCLE ( 'NONE', #62065, 4.000000000000003553 ) ;
#4784 = LINE ( 'NONE', #36130, #8753 ) ;
#4785 = CARTESIAN_POINT ( 'NONE',  ( 4.999999999999993783, 115.6078173946806942, 14.99999999999997513 ) ) ;
#4786 = CARTESIAN_POINT ( 'NONE',  ( -10.50000000000002309, 8.000000000000000000, -4.000000000000000000 ) ) ;
#4787 = PRESENTATION_LAYER_ASSIGNMENT (  '', '', ( #8172 ) ) ;
#4788 = CARTESIAN_POINT ( 'NONE',  ( 3.999798566743339556, 8.867945265733707672, 2.000000000000000000 ) ) ;
#4789 = FILL_AREA_STYLE_COLOUR ( '', #38302 ) ;
#4790 = AXIS2_PLACEMENT_3D ( 'NONE', #19082, #39553, #40588 ) ;
#4791 = PRESENTATION_STYLE_ASSIGNMENT (( #42477 ) ) ;
#4792 = UNCERTAINTY_MEASURE_WITH_UNIT (LENGTH_MEASURE( 1.000000000000000082E-05 ), #53570, 'distance_accuracy_value', 'NONE');
#4793 = EDGE_CURVE ( 'NONE', #23836, #26070, #31357, .T. ) ;
#4794 = AXIS2_PLACEMENT_3D ( 'NONE', #65015, #17229, #38694 ) ;
#4795 = SURFACE_STYLE_USAGE ( .BOTH. , #52998 ) ;
#4796 = FACE_OUTER_BOUND ( 'NONE', #47006, .T. ) ;
#4797 = CARTESIAN_POINT ( 'NONE',  ( 30.25000000000000711, 18.74999999999997868, 3.750000000000000000 ) ) ;
#4798 = VERTEX_POINT ( 'NONE', #52548 ) ;
#4799 = ORIENTED_EDGE ( 'NONE', *, *, #20500, .F. ) ;
#4800 = FILL_AREA_STYLE_COLOUR ( '', #67807 ) ;
#4801 = EDGE_CURVE ( 'NONE', #25904, #5648, #66206, .T. ) ;
#4802 = CARTESIAN_POINT ( 'NONE',  ( 0.000000000000000000, 115.0570736234661666, -8.025000000000000355 ) ) ;
#4803 = DIRECTION ( 'NONE',  ( 1.084202172485504434E-16, 0.000000000000000000, 1.000000000000000000 ) ) ;
#4804 = ORIENTED_EDGE ( 'NONE', *, *, #59726, .T. ) ;
#4805 = ORIENTED_EDGE ( 'NONE', *, *, #50791, .T. ) ;
#4806 = CARTESIAN_POINT ( 'NONE',  ( 74.99999999999998579, 50.00000000000000000, -10.00000000000000000 ) ) ;
#4807 = CARTESIAN_POINT ( 'NONE',  ( 1.000000000000000000, 36.74999999999999289, -4.000000000000000000 ) ) ;
#4808 = STYLED_ITEM ( 'NONE', ( #42621 ), #29206 ) ;
#4809 = FILL_AREA_STYLE_COLOUR ( '', #49 ) ;
#4810 = ORIENTED_EDGE ( 'NONE', *, *, #570, .T. ) ;
#4811 = CARTESIAN_POINT ( 'NONE',  ( 8.102448949553183510, 116.1049999999999756, -5.886773742842746238 ) ) ;
#4812 =( NAMED_UNIT ( * ) PLANE_ANGLE_UNIT ( ) SI_UNIT ( $, .RADIAN. ) );
#4813 = CARTESIAN_POINT ( 'NONE',  ( -71.50000000000000000, 35.92875272052971525, -7.500000000000000000 ) ) ;
#4814 = DIRECTION ( 'NONE',  ( -1.000000000000000000, 0.000000000000000000, 0.000000000000000000 ) ) ;
#4815 = CARTESIAN_POINT ( 'NONE',  ( -99.44499999999999318, 0.000000000000000000, 8.024999999999991473 ) ) ;
#4816 = EDGE_LOOP ( 'NONE', ( #31934, #47957, #32477, #51983 ) ) ;
#4817 = AXIS2_PLACEMENT_3D ( 'NONE', #52808, #26037, #47575 ) ;
#4818 = CARTESIAN_POINT ( 'NONE',  ( -163.8570736234661922, -5.598654528085803328, -7.705886871421366635 ) ) ;
#4819 = EDGE_LOOP ( 'NONE', ( #4743, #52373, #64686, #65728 ) ) ;
#4820 = CARTESIAN_POINT ( 'NONE',  ( -4.716976649647097730, 153.2429263765338021, -6.492361379858953896 ) ) ;
#4821 = CARTESIAN_POINT ( 'NONE',  ( -13.75000000000000533, 30.74999999999999289, -4.000000000000000000 ) ) ;
#4822 = CARTESIAN_POINT ( 'NONE',  ( 5.196152422706631135, 1.107695154586740394, 9.000000000000001776 ) ) ;
#4823 = DIRECTION ( 'NONE',  ( -1.239088197126290324E-16, 0.000000000000000000, -1.000000000000000000 ) ) ;
#4824 = ADVANCED_FACE ( 'NONE', ( #13482 ), #40377, .T. ) ;
#4825 = CARTESIAN_POINT ( 'NONE',  ( -62.75707362346616236, -5.598654528085801552, 7.705886871421367523 ) ) ;
#4826 = ORIENTED_EDGE ( 'NONE', *, *, #50651, .T. ) ;
#4827 = CARTESIAN_POINT ( 'NONE',  ( 20.17679519342876304, 115.4776649671489963, 10.00000000000000000 ) ) ;
#4828 = DIRECTION ( 'NONE',  ( 0.000000000000000000, -1.000000000000000000, 0.000000000000000000 ) ) ;
#4829 = DIRECTION ( 'NONE',  ( -1.000000000000000000, 0.000000000000000000, 0.000000000000000000 ) ) ;
#4830 =( NAMED_UNIT ( * ) PLANE_ANGLE_UNIT ( ) SI_UNIT ( $, .RADIAN. ) );
#4831 = CIRCLE ( 'NONE', #40771, 0.2500000000000002220 ) ;
#4832 = PRESENTATION_LAYER_ASSIGNMENT (  '', '', ( #11557 ) ) ;
#4833 =( NAMED_UNIT ( * ) SI_UNIT ( $, .STERADIAN. ) SOLID_ANGLE_UNIT ( ) );
#4834 = B_SPLINE_CURVE_WITH_KNOTS ( 'NONE', 3,
 ( #37268, #53415, #69569, #5195, #15112, #26637, #21372, #34281, #45577, #12818 ),
 .UNSPECIFIED., .F., .F.,
 ( 4, 2, 2, 2, 4 ),
 ( 0.000000000000000000, 0.001409835084339927094, 0.002819670168679854188, 0.004229505253019781065, 0.005639340337359708376 ),
 .UNSPECIFIED. ) ;
#4835 = FACE_OUTER_BOUND ( 'NONE', #44840, .T. ) ;
#4836 = CIRCLE ( 'NONE', #43068, 2.000000000000001776 ) ;
#4837 = CARTESIAN_POINT ( 'NONE',  ( -195.0000000000000000, 0.000000000000000000, 9.524999999999991473 ) ) ;
#4838 = DIRECTION ( 'NONE',  ( 0.000000000000000000, 0.000000000000000000, 1.000000000000000000 ) ) ;
#4839 = DIRECTION ( 'NONE',  ( -1.000000000000000000, -0.000000000000000000, -0.000000000000000000 ) ) ;
#4840 = CARTESIAN_POINT ( 'NONE',  ( -71.99999999999998579, 119.9999999999997868, 9.500000000000000000 ) ) ;
#4841 = ORIENTED_EDGE ( 'NONE', *, *, #23434, .F. ) ;
#4842 = ORIENTED_EDGE ( 'NONE', *, *, #18285, .F. ) ;
#4843 = CARTESIAN_POINT ( 'NONE',  ( -11.74999999999999467, -0.4142135623730948124, 19.00000000000000000 ) ) ;
#4844 = FILL_AREA_STYLE_COLOUR ( '', #3968 ) ;
#4845 = CARTESIAN_POINT ( 'NONE',  ( -169.8570736234661922, -5.598654528085803328, -7.705886871421366635 ) ) ;
#4846 = DIRECTION ( 'NONE',  ( 1.000000000000000000, 0.000000000000000000, 0.000000000000000000 ) ) ;
#4847 = VERTEX_POINT ( 'NONE', #56767 ) ;
#4848 = PRESENTATION_STYLE_ASSIGNMENT (( #53054 ) ) ;
#4849 = ADVANCED_FACE ( 'NONE', ( #4293 ), #14200, .T. ) ;
#4850 = CARTESIAN_POINT ( 'NONE',  ( -168.8049999999999500, -8.437984349512085203, 5.166775262442717831E-16 ) ) ;
#4851 = CARTESIAN_POINT ( 'NONE',  ( 0.000000000000000000, -2.500000000000000000, 0.000000000000000000 ) ) ;
#4852 = CARTESIAN_POINT ( 'NONE',  ( -181.9449999999999932, -9.827790563157499189E-16, -8.024999999999991473 ) ) ;
#4853 = AXIS2_PLACEMENT_3D ( 'NONE', #64360, #12252, #6626 ) ;
#4854 = CARTESIAN_POINT ( 'NONE',  ( -168.4449999999999932, 0.000000000000000000, 8.024999999999991473 ) ) ;
#4855 = VERTEX_POINT ( 'NONE', #25438 ) ;
#4856 = VECTOR ( 'NONE', #67210, 1000.000000000000000 ) ;
#4857 = CARTESIAN_POINT ( 'NONE',  ( 10.39230484541327115, -3.482307324624967703E-15, 1.392304845413258718 ) ) ;
#4858 = CARTESIAN_POINT ( 'NONE',  ( -12.92299149854152063, 11.10368424694205203, -4.551139136257919660 ) ) ;
#4859 = AXIS2_PLACEMENT_3D ( 'NONE', #9505, #30925, #4166 ) ;
#4860 = CARTESIAN_POINT ( 'NONE',  ( -81.65499999999998693, -7.632228543268600340, -2.479861379858950166 ) ) ;
#4861 = CARTESIAN_POINT ( 'NONE',  ( 9.489509921829204941, 154.5000000000000568, -0.9314843046822294248 ) ) ;
#4862 = CARTESIAN_POINT ( 'NONE',  ( -168.2070736234663570, 3.094860106621407869, 9.524999999997831424 ) ) ;
#4863 = CARTESIAN_POINT ( 'NONE',  ( -74.58429712092500097, 36.42179758710307169, -9.999999998919950173 ) ) ;
#4864 = EDGE_CURVE ( 'NONE', #4197, #24855, #45879, .T. ) ;
#4865 = AXIS2_PLACEMENT_3D ( 'NONE', #20725, #68226, #36611 ) ;
#4866 = CARTESIAN_POINT ( 'NONE',  ( -85.04499999999998749, 7.632228543268600340, 2.479861379858949277 ) ) ;
#4867 = CARTESIAN_POINT ( 'NONE',  ( 10.01517768586949231, 127.8050000000000068, 1.839758294383810543E-15 ) ) ;
#4868 = DIRECTION ( 'NONE',  ( 1.000000000000000000, 0.000000000000000000, 0.000000000000000000 ) ) ;
#4869 = B_SPLINE_CURVE_WITH_KNOTS ( 'NONE', 3,
 ( #66526, #62284, #45793, #2807, #67213, #40510, #50696, #12697 ),
 .UNSPECIFIED., .F., .F.,
 ( 4, 2, 2, 4 ),
 ( 0.000000000000000000, 0.001659144101464961850, 0.002488716152197438004, 0.003318288202929914159 ),
 .UNSPECIFIED. ) ;
#4870 = CARTESIAN_POINT ( 'NONE',  ( -172.1070736234661069, 8.102448949553172852, -5.886773742842744461 ) ) ;
#4871 = CARTESIAN_POINT ( 'NONE',  ( 0.2500000000000000000, 36.99999999999999289, -3.000000000000000000 ) ) ;
#4872 = CIRCLE ( 'NONE', #24004, 3.000000000000000444 ) ;
#4873 = FILL_AREA_STYLE ('',( #20355 ) ) ;
#4874 = VECTOR ( 'NONE', #43861, 1000.000000000000227 ) ;
#4875 = ORIENTED_EDGE ( 'NONE', *, *, #40850, .T. ) ;
#4876 = CARTESIAN_POINT ( 'NONE',  ( 65.50000000000000000, 1.797044900979284448E-15, -6.500000000000000000 ) ) ;
#4877 = DIRECTION ( 'NONE',  ( -1.000000000000000000, 0.000000000000000000, 0.000000000000000000 ) ) ;
#4879 = DIRECTION ( 'NONE',  ( -0.000000000000000000, -0.000000000000000000, 1.000000000000000000 ) ) ;
#4878 = CARTESIAN_POINT ( 'NONE',  ( 65.00000000000000000, 1.797044900979284448E-15, -12.00000000000000000 ) ) ;
#4880 = ORIENTED_EDGE ( 'NONE', *, *, #65751, .T. ) ;
#4882 = ORIENTED_EDGE ( 'NONE', *, *, #65607, .F. ) ;
#4881 = AXIS2_PLACEMENT_3D ( 'NONE', #62106, #66004, #23433 ) ;
#4883 = CARTESIAN_POINT ( 'NONE',  ( -45.89269293898073698, 9.343722028457033701, -6.169771923672656477 ) ) ;
#4884 = CARTESIAN_POINT ( 'NONE',  ( -174.6570736234662036, 9.058813317711329915, 2.943386871421369566 ) ) ;
#4885 = COLOUR_RGB ( '', 0.31764706, 0.68627451, 0.89019608) ;
#4886 = CARTESIAN_POINT ( 'NONE',  ( 4.750000000000002665, 22.24999999999998579, -3.750000000000000000 ) ) ;
#4887 = PRESENTATION_STYLE_ASSIGNMENT (( #69272 ) ) ;
#4888 = CARTESIAN_POINT ( 'NONE',  ( 9.000000000000003553, 24.99999999999998579, 4.000000000000000000 ) ) ;
#4889 = EDGE_LOOP ( 'NONE', ( #5242, #27167, #20305, #64424 ) ) ;
#4890 = CARTESIAN_POINT ( 'NONE',  ( -120.9549999999999983, -7.632228543268599452, 2.479861379858951054 ) ) ;
#4891 = ORIENTED_EDGE ( 'NONE', *, *, #33979, .F. ) ;
#4892 = CARTESIAN_POINT ( 'NONE',  ( -136.5570736234661808, -1.166476076187852838E-15, -9.524999999999991473 ) ) ;
#4893 = CARTESIAN_POINT ( 'NONE',  ( 20.17806131642189271, 115.4772719928210876, -10.00000000000000178 ) ) ;
#4894 = VERTEX_POINT ( 'NONE', #20143 ) ;
#4895 =( NAMED_UNIT ( * ) SI_UNIT ( $, .STERADIAN. ) SOLID_ANGLE_UNIT ( ) );
#4896 =( NAMED_UNIT ( * ) PLANE_ANGLE_UNIT ( ) SI_UNIT ( $, .RADIAN. ) );
#4897 = ORIENTED_EDGE ( 'NONE', *, *, #16324, .T. ) ;
#4898 = DIRECTION ( 'NONE',  ( 0.000000000000000000, 1.000000000000000000, 0.000000000000000000 ) ) ;
#4899 = CARTESIAN_POINT ( 'NONE',  ( 3.094860106618435136, 154.2949999999999875, -9.525000000000000355 ) ) ;
#4900 = VECTOR ( 'NONE', #63575, 1000.000000000000000 ) ;
#4901 = ORIENTED_EDGE ( 'NONE', *, *, #7483, .F. ) ;
#4902 = CARTESIAN_POINT ( 'NONE',  ( -118.5570736234661808, -1.166476076187852838E-15, -9.524999999999991473 ) ) ;
#4903 = CARTESIAN_POINT ( 'NONE',  ( 3.094860106618435136, 149.4049999999999443, -9.525000000000000355 ) ) ;
#4904 = CARTESIAN_POINT ( 'NONE',  ( -34.99999999999992895, 112.4999999999999858, 9.500000000000000000 ) ) ;
#4905 = AXIS2_PLACEMENT_3D ( 'NONE', #47949, #63369, #41592 ) ;
#4906 = ORIENTED_EDGE ( 'NONE', *, *, #55980, .T. ) ;
#4907 = CARTESIAN_POINT ( 'NONE',  ( 7.632228543268608334, 128.3429263765338249, -2.479861379858951942 ) ) ;
#4908 = CARTESIAN_POINT ( 'NONE',  ( -23.21231517720798010, 113.4999999999999858, -10.00000000000000000 ) ) ;
#4909 = SURFACE_STYLE_USAGE ( .BOTH. , #37674 ) ;
#4910 = DIRECTION ( 'NONE',  ( 0.000000000000000000, 0.000000000000000000, 1.000000000000000000 ) ) ;
#4911 =( GEOMETRIC_REPRESENTATION_CONTEXT ( 3 ) GLOBAL_UNCERTAINTY_ASSIGNED_CONTEXT ( ( #5327 ) ) GLOBAL_UNIT_ASSIGNED_CONTEXT ( ( #7640, #34034, #29072 ) ) REPRESENTATION_CONTEXT ( 'NONE', 'WORKASPACE' ) );
#4912 = EDGE_LOOP ( 'NONE', ( #56644, #49211, #64768, #33306 ) ) ;
#4913 = EDGE_CURVE ( 'NONE', #49132, #2827, #33629, .T. ) ;
#4914 = CARTESIAN_POINT ( 'NONE',  ( -0.000000000000000000, 8.270287287112621792E-15, -12.50000000000000000 ) ) ;
#4915 = ORIENTED_EDGE ( 'NONE', *, *, #39621, .F. ) ;
#4916 = CARTESIAN_POINT ( 'NONE',  ( -61.19292637653379074, -10.01517768586948698, 6.132527647946031529E-16 ) ) ;
#4917 = DIRECTION ( 'NONE',  ( 0.000000000000000000, 0.000000000000000000, 1.000000000000000000 ) ) ;
#4918 = DIRECTION ( 'NONE',  ( -0.000000000000000000, -1.000000000000000000, -0.000000000000000000 ) ) ;
#4919 = STYLED_ITEM ( 'NONE', ( #34151 ), #2839 ) ;
#4920 = CARTESIAN_POINT ( 'NONE',  ( -149.4550000000000125, 7.632228543268599452, -2.479861379858951942 ) ) ;
#4921 = DIRECTION ( 'NONE',  ( -0.000000000000000000, -0.000000000000000000, -1.000000000000000000 ) ) ;
#4922 = EDGE_CURVE ( 'NONE', #21587, #28936, #49364, .T. ) ;
#4923 = AXIS2_PLACEMENT_3D ( 'NONE', #20250, #68118, #19899 ) ;
#4924 = EDGE_CURVE ( 'NONE', #60894, #15891, #4669, .T. ) ;
#4925 = CIRCLE ( 'NONE', #18448, 5.000000000000004441 ) ;
#4926 = SURFACE_STYLE_FILL_AREA ( #4569 ) ;
#4927 = LINE ( 'NONE', #38377, #25958 ) ;
#4928 = CARTESIAN_POINT ( 'NONE',  ( 41.39060477125153170, 107.1334711628775693, 3.500000000000000888 ) ) ;
#4929 = DIRECTION ( 'NONE',  ( 0.000000000000000000, 0.000000000000000000, -1.000000000000000000 ) ) ;
#4930 = ORIENTED_EDGE ( 'NONE', *, *, #57660, .T. ) ;
#4931 = ADVANCED_FACE ( 'NONE', ( #20868 ), #26121, .T. ) ;
#4932 = ORIENTED_EDGE ( 'NONE', *, *, #12796, .F. ) ;
#4933 = CARTESIAN_POINT ( 'NONE',  ( 23.31805810294994075, 27.43935250242352453, 27.19033932930832620 ) ) ;
#4934 =( NAMED_UNIT ( * ) PLANE_ANGLE_UNIT ( ) SI_UNIT ( $, .RADIAN. ) );
#4935 = CARTESIAN_POINT ( 'NONE',  ( -65.60499999999997556, 6.826472737025113702, -4.959722759717902107 ) ) ;
#4936 = ORIENTED_EDGE ( 'NONE', *, *, #16019, .T. ) ;
#4937 =( NAMED_UNIT ( * ) SI_UNIT ( $, .STERADIAN. ) SOLID_ANGLE_UNIT ( ) );
#4938 = ADVANCED_FACE ( 'NONE', ( #27146 ), #16, .F. ) ;
#4939 = DIRECTION ( 'NONE',  ( -0.000000000000000000, -0.000000000000000000, 1.000000000000000000 ) ) ;
#4940 = CARTESIAN_POINT ( 'NONE',  ( -30.38025804287905629, -8.499999999999996447, 0.06931351858032895608 ) ) ;
#4941 = LINE ( 'NONE', #32352, #66086 ) ;
#4942 = EDGE_CURVE ( 'NONE', #37991, #15417, #2055, .T. ) ;
#4943 = CIRCLE ( 'NONE', #53263, 1.000000000000000000 ) ;
#4944 = EDGE_CURVE ( 'NONE', #23886, #64569, #56077, .T. ) ;
#4945 = DIRECTION ( 'NONE',  ( 1.000000000000000000, 0.000000000000000000, 0.000000000000000000 ) ) ;
#4946 = FACE_OUTER_BOUND ( 'NONE', #34124, .T. ) ;
#4947 = ORIENTED_EDGE ( 'NONE', *, *, #47798, .T. ) ;
#4948 = ADVANCED_FACE ( 'NONE', ( #69063 ), #32800, .T. ) ;
#4949 = SURFACE_SIDE_STYLE ('',( #36667 ) ) ;
#4950 = SURFACE_SIDE_STYLE ('',( #53155 ) ) ;
#4952 =( NAMED_UNIT ( * ) PLANE_ANGLE_UNIT ( ) SI_UNIT ( $, .RADIAN. ) );
#4951 = DIRECTION ( 'NONE',  ( 1.000000000000000000, 0.000000000000000000, 0.000000000000000000 ) ) ;
#4953 = CARTESIAN_POINT ( 'NONE',  ( -122.9949999999999903, -6.826472737025113702, 4.959722759717902107 ) ) ;
#4954 = CARTESIAN_POINT ( 'NONE',  ( 0.000000000000000000, 151.4449999999999932, -9.525000000000000355 ) ) ;
#4955 = CARTESIAN_POINT ( 'NONE',  ( -83.99499999999999034, -6.826472737025115478, 4.959722759717900331 ) ) ;
#4956 = CARTESIAN_POINT ( 'NONE',  ( -44.50000000000000000, 10.49999999999998224, -3.000000000000000444 ) ) ;
#4957 = CIRCLE ( 'NONE', #47704, 0.2500000000000002220 ) ;
#4958 = SURFACE_STYLE_USAGE ( .BOTH. , #64040 ) ;
#4959 = DIRECTION ( 'NONE',  ( 0.000000000000000000, 0.000000000000000000, -1.000000000000000000 ) ) ;
#4960 = ORIENTED_EDGE ( 'NONE', *, *, #64085, .T. ) ;
#4961 = CARTESIAN_POINT ( 'NONE',  ( -132.7429263765338021, -5.598654528085803328, -7.705886871421366635 ) ) ;
#4962 = VECTOR ( 'NONE', #15210, 1000.000000000000000 ) ;
#4963 = DIRECTION ( 'NONE',  ( -1.000000000000000000, 0.000000000000000000, 0.000000000000000000 ) ) ;
#4964 = CARTESIAN_POINT ( 'NONE',  ( -149.2449999999999761, -4.716976649647093289, -6.492361379858945902 ) ) ;
#4965 = DIRECTION ( 'NONE',  ( 1.000000000000000000, 0.000000000000000000, 0.000000000000000000 ) ) ;
#4966 = MECHANICAL_DESIGN_GEOMETRIC_PRESENTATION_REPRESENTATION (  '', ( #35305 ), #52197 ) ;
#4967 =( NAMED_UNIT ( * ) PLANE_ANGLE_UNIT ( ) SI_UNIT ( $, .RADIAN. ) );
#4968 = EDGE_LOOP ( 'NONE', ( #33773, #61380, #28120, #16946, #13028, #49468 ) ) ;
#4970 = ORIENTED_EDGE ( 'NONE', *, *, #61100, .T. ) ;
#4969 =( GEOMETRIC_REPRESENTATION_CONTEXT ( 3 ) GLOBAL_UNCERTAINTY_ASSIGNED_CONTEXT ( ( #35383 ) ) GLOBAL_UNIT_ASSIGNED_CONTEXT ( ( #51450, #50412, #23326 ) ) REPRESENTATION_CONTEXT ( 'NONE', 'WORKASPACE' ) );
#4971 = FACE_OUTER_BOUND ( 'NONE', #45631, .T. ) ;
#4972 = AXIS2_PLACEMENT_3D ( 'NONE', #23369, #44868, #65938 ) ;
#4973 = CIRCLE ( 'NONE', #399, 0.9999999999999978906 ) ;
#4974 = DIRECTION ( 'NONE',  ( -0.000000000000000000, -1.000000000000000000, 0.000000000000000000 ) ) ;
#4975 = CARTESIAN_POINT ( 'NONE',  ( 17.25000000000000711, 24.74999999999997868, -3.750000000000000000 ) ) ;
#4976 = ORIENTED_EDGE ( 'NONE', *, *, #30117, .F. ) ;
#4977 = CARTESIAN_POINT ( 'NONE',  ( -154.4049999999999727, -2.607480562269069768, 8.024999999999991473 ) ) ;
#4978 = CIRCLE ( 'NONE', #62324, 1.000000000000000000 ) ;
#4979 = ORIENTED_EDGE ( 'NONE', *, *, #2144, .F. ) ;
#4980 = CARTESIAN_POINT ( 'NONE',  ( 0.000000000000000000, 33.74999999999999289, 4.000000000000000000 ) ) ;
#4981 = EDGE_LOOP ( 'NONE', ( #42214, #2453, #69608, #54827 ) ) ;
#4982 = STYLED_ITEM ( 'NONE', ( #60675 ), #48567 ) ;
#4983 = DIRECTION ( 'NONE',  ( 0.000000000000000000, 0.000000000000000000, -1.000000000000000000 ) ) ;
#4984 = DIRECTION ( 'NONE',  ( -0.000000000000000000, -0.000000000000000000, 1.000000000000000000 ) ) ;
#4985 = CARTESIAN_POINT ( 'NONE',  ( -9.058813317711338797, 116.3449999999999847, 2.943386871421373563 ) ) ;
#4986 = CARTESIAN_POINT ( 'NONE',  ( 0.000000000000000000, -7.000000000000000888, 0.000000000000000000 ) ) ;
#4987 = ORIENTED_EDGE ( 'NONE', *, *, #12057, .T. ) ;
#4988 = CARTESIAN_POINT ( 'NONE',  ( -4.357963766315036125, 6.451785339198147007, 0.7663918866669852115 ) ) ;
#4989 = CARTESIAN_POINT ( 'NONE',  ( 8.102448949553179958, 124.5049999999999812, 5.886773742842750679 ) ) ;
#4990 = CARTESIAN_POINT ( 'NONE',  ( -63.35499999999998266, -4.716976649647093289, -6.492361379858945902 ) ) ;
#4991 = CARTESIAN_POINT ( 'NONE',  ( -41.39060477124900927, 107.1334711628759493, -3.500000000000001776 ) ) ;
#4992 = ORIENTED_EDGE ( 'NONE', *, *, #29873, .F. ) ;
#4993 = CARTESIAN_POINT ( 'NONE',  ( 0.000000000000000000, 146.5549999999999784, -9.525000000000000355 ) ) ;
#4994 = SURFACE_STYLE_USAGE ( .BOTH. , #36719 ) ;
#4995 = DIRECTION ( 'NONE',  ( 0.000000000000000000, 1.000000000000000000, 0.000000000000000000 ) ) ;
#4996 = PRESENTATION_LAYER_ASSIGNMENT (  '', '', ( #42119 ) ) ;
#4997 = PLANE ( 'NONE',  #46732 ) ;
#4998 = EDGE_CURVE ( 'NONE', #58318, #15154, #54321, .T. ) ;
#4999 = CARTESIAN_POINT ( 'NONE',  ( -195.0000000000000000, 0.000000000000000000, 0.000000000000000000 ) ) ;
#5000 = ORIENTED_EDGE ( 'NONE', *, *, #32218, .T. ) ;
#5001 = LINE ( 'NONE', #56469, #7491 ) ;
#5003 =( LENGTH_UNIT ( ) NAMED_UNIT ( * ) SI_UNIT ( .MILLI., .METRE. ) );
#5002 = AXIS2_PLACEMENT_3D ( 'NONE', #60979, #7526, #34594 ) ;
#5004 = CARTESIAN_POINT ( 'NONE',  ( -178.8549999999999898, 4.716976649647094177, 6.492361379858945902 ) ) ;
#5005 = ORIENTED_EDGE ( 'NONE', *, *, #61776, .F. ) ;
#5006 = DIRECTION ( 'NONE',  ( 0.000000000000000000, -1.000000000000000000, 0.000000000000000000 ) ) ;
#5007 = EDGE_CURVE ( 'NONE', #62297, #47726, #47196, .T. ) ;
#5008 = DIRECTION ( 'NONE',  ( -0.000000000000000000, 0.000000000000000000, -1.000000000000000000 ) ) ;
#5009 = VECTOR ( 'NONE', #22877, 1000.000000000000000 ) ;
#5010 =( NAMED_UNIT ( * ) PLANE_ANGLE_UNIT ( ) SI_UNIT ( $, .RADIAN. ) );
#5011 = ORIENTED_EDGE ( 'NONE', *, *, #157, .T. ) ;
#5012 = SURFACE_STYLE_FILL_AREA ( #43052 ) ;
#5013 = DIRECTION ( 'NONE',  ( 1.300977106640434891E-16, -0.000000000000000000, 1.000000000000000000 ) ) ;
#5014 = ORIENTED_EDGE ( 'NONE', *, *, #54583, .T. ) ;
#5015 = CARTESIAN_POINT ( 'NONE',  ( -71.50000000000000000, 35.92875272052971525, -7.000000000000000000 ) ) ;
#5016 = CARTESIAN_POINT ( 'NONE',  ( -91.10500000000000398, -6.826472737025115478, 4.959722759717900331 ) ) ;
#5017 = ORIENTED_EDGE ( 'NONE', *, *, #65668, .T. ) ;
#5018 =( LENGTH_UNIT ( ) NAMED_UNIT ( * ) SI_UNIT ( .MILLI., .METRE. ) );
#5019 = EDGE_CURVE ( 'NONE', #8109, #53103, #27557, .T. ) ;
#5020 = FILL_AREA_STYLE ('',( #15607 ) ) ;
#5021 = CARTESIAN_POINT ( 'NONE',  ( -133.2570736234661695, 5.598654528085800663, -7.705886871421367523 ) ) ;
#5022 = DIRECTION ( 'NONE',  ( 0.000000000000000000, 0.000000000000000000, -1.000000000000000000 ) ) ;
#5023 = CARTESIAN_POINT ( 'NONE',  ( -3.094860106618434248, 149.7949999999999875, 9.525000000000000355 ) ) ;
#5024 = CARTESIAN_POINT ( 'NONE',  ( -62.60707362346617089, -8.102448949553172852, 5.886773742842742685 ) ) ;
#5025 = CIRCLE ( 'NONE', #16263, 0.5000000000000004441 ) ;
#5026 = ADVANCED_FACE ( 'NONE', ( #67480 ), #45320, .T. ) ;
#5027 = CARTESIAN_POINT ( 'NONE',  ( -80.24292637653380211, 5.598654528085804216, 7.705886871421366635 ) ) ;
#5028 = VERTEX_POINT ( 'NONE', #50617 ) ;
#5029 = CARTESIAN_POINT ( 'NONE',  ( 39.24999999999999289, 16.24999999999997513, 3.750000000000000000 ) ) ;
#5030 = DIRECTION ( 'NONE',  ( 0.000000000000000000, 1.000000000000000000, 3.469446951953611033E-15 ) ) ;
#5032 = DIRECTION ( 'NONE',  ( 0.000000000000000000, 0.000000000000000000, -1.000000000000000000 ) ) ;
#5031 = CARTESIAN_POINT ( 'NONE',  ( 60.00000000000000000, 1.797044900979284448E-15, -12.00000000000000000 ) ) ;
#5033 = AXIS2_PLACEMENT_3D ( 'NONE', #17269, #54161, #6318 ) ;
#5034 = CARTESIAN_POINT ( 'NONE',  ( -111.9549999999999841, -7.632228543268599452, 2.479861379858951054 ) ) ;
#5035 = CARTESIAN_POINT ( 'NONE',  ( -3.094860106618432471, 121.5949999999999847, -9.525000000000000355 ) ) ;
#5036 = CARTESIAN_POINT ( 'NONE',  ( -112.3449999999999847, 7.632228543268599452, -2.479861379858951942 ) ) ;
#5037 = AXIS2_PLACEMENT_3D ( 'NONE', #25994, #31624, #15484 ) ;
#5038 = AXIS2_PLACEMENT_3D ( 'NONE', #18060, #66234, #1817 ) ;
#5039 = AXIS2_PLACEMENT_3D ( 'NONE', #20995, #59288, #42493 ) ;
#5040 =( LENGTH_UNIT ( ) NAMED_UNIT ( * ) SI_UNIT ( .MILLI., .METRE. ) );
#5041 = CARTESIAN_POINT ( 'NONE',  ( 18.00000000000000711, 33.99999999999999289, 4.000000000000000000 ) ) ;
#5042 = VERTEX_POINT ( 'NONE', #39747 ) ;
#5043 = CARTESIAN_POINT ( 'NONE',  ( -163.6429263765338078, -5.598654528085801552, 7.705886871421367523 ) ) ;
#5044 = SURFACE_STYLE_USAGE ( .BOTH. , #58176 ) ;
#5045 = CARTESIAN_POINT ( 'NONE',  ( -183.2949999999999307, -2.607480562269069768, 8.024999999999991473 ) ) ;
#5046 = AXIS2_PLACEMENT_3D ( 'NONE', #47564, #67939, #53139 ) ;
#5047 = DIRECTION ( 'NONE',  ( 1.000000000000000000, 0.000000000000000000, 0.000000000000000000 ) ) ;
#5048 = AXIS2_PLACEMENT_3D ( 'NONE', #13992, #58206, #10029 ) ;
#5049 = DIRECTION ( 'NONE',  ( -1.000000000000000000, -0.000000000000000000, -0.000000000000000000 ) ) ;
#5050 = SURFACE_STYLE_FILL_AREA ( #10348 ) ;
#5051 = VERTEX_POINT ( 'NONE', #29500 ) ;
#5052 = CARTESIAN_POINT ( 'NONE',  ( -78.59292637653381064, -3.094860106618431139, -9.524999999999991473 ) ) ;
#5053 = AXIS2_PLACEMENT_3D ( 'NONE', #44819, #23663, #39535 ) ;
#5054 = FACE_BOUND ( 'NONE', #65714, .T. ) ;
#5055 = EDGE_CURVE ( 'NONE', #53177, #60077, #55187, .T. ) ;
#5056 = VECTOR ( 'NONE', #61101, 1000.000000000000000 ) ;
#5057 = FILL_AREA_STYLE_COLOUR ( '', #15844 ) ;
#5058 = DIRECTION ( 'NONE',  ( 0.6402681315062906942, 0.000000000000000000, 0.7681514953298230752 ) ) ;
#5059 = CARTESIAN_POINT ( 'NONE',  ( -24.00000000000000000, 1.000000000000000000, -4.000000000000000000 ) ) ;
#5060 = CARTESIAN_POINT ( 'NONE',  ( -179.9049999999999727, 2.607480562269069324, -8.024999999999993250 ) ) ;
#5061 = EDGE_LOOP ( 'NONE', ( #58878, #33808, #753, #48582, #62588 ) ) ;
#5062 = PLANE ( 'NONE',  #17437 ) ;
#5063 = DIRECTION ( 'NONE',  ( 0.000000000000000000, 1.000000000000000000, -0.000000000000000000 ) ) ;
#5064 = CARTESIAN_POINT ( 'NONE',  ( 6.826472737025121695, 141.6070736234661354, -4.959722759717905660 ) ) ;
#5065 = STYLED_ITEM ( 'NONE', ( #64457 ), #27772 ) ;
#5066 = STYLED_ITEM ( 'NONE', ( #48138 ), #7960 ) ;
#5067 = ORIENTED_EDGE ( 'NONE', *, *, #52466, .T. ) ;
#5068 = CARTESIAN_POINT ( 'NONE',  ( -101.6070736234661780, -8.102448949553174629, 5.886773742842742685 ) ) ;
#5069 = CARTESIAN_POINT ( 'NONE',  ( -98.00499999999999545, 6.826472737025115478, 4.959722759717899443 ) ) ;
#5070 = CARTESIAN_POINT ( 'NONE',  ( -52.50000000000000000, -2.024042244987997205E-14, -12.00000000000000000 ) ) ;
#5071 = ORIENTED_EDGE ( 'NONE', *, *, #108, .T. ) ;
#5072 = ADVANCED_FACE ( 'NONE', ( #29843 ), #7358, .T. ) ;
#5073 =( GEOMETRIC_REPRESENTATION_CONTEXT ( 3 ) GLOBAL_UNCERTAINTY_ASSIGNED_CONTEXT ( ( #64985 ) ) GLOBAL_UNIT_ASSIGNED_CONTEXT ( ( #6481, #12117, #27920 ) ) REPRESENTATION_CONTEXT ( 'NONE', 'WORKASPACE' ) );
#5074 = DIRECTION ( 'NONE',  ( -1.000000000000000000, 0.000000000000000000, 0.000000000000000000 ) ) ;
#5075 = EDGE_CURVE ( 'NONE', #24108, #33812, #46062, .T. ) ;
#5076 = CARTESIAN_POINT ( 'NONE',  ( -74.75000000000000000, -3.000000000000000000, 7.000000000000001776 ) ) ;
#5077 = PRESENTATION_STYLE_ASSIGNMENT (( #10383 ) ) ;
#5078 = SURFACE_STYLE_FILL_AREA ( #43118 ) ;
#5079 = STYLED_ITEM ( 'NONE', ( #33697 ), #49078 ) ;
#5080 = EDGE_LOOP ( 'NONE', ( #7769, #3777, #33373, #22096 ) ) ;
#5081 = AXIS2_PLACEMENT_3D ( 'NONE', #4474, #42201, #68191 ) ;
#5082 =( NAMED_UNIT ( * ) SI_UNIT ( $, .STERADIAN. ) SOLID_ANGLE_UNIT ( ) );
#5083 = CARTESIAN_POINT ( 'NONE',  ( -75.74499999999999034, 4.716976649647094177, 6.492361379858945902 ) ) ;
#5084 = VERTEX_POINT ( 'NONE', #55544 ) ;
#5085 = CARTESIAN_POINT ( 'NONE',  ( 66.74999999999998579, 36.75000000000000000, 3.750000000000000000 ) ) ;
#5086 = EDGE_CURVE ( 'NONE', #42518, #26425, #60659, .T. ) ;
#5087 = SURFACE_STYLE_FILL_AREA ( #11049 ) ;
#5088 = VERTEX_POINT ( 'NONE', #28796 ) ;
#5089 = CARTESIAN_POINT ( 'NONE',  ( -43.75000000000000000, 0.000000000000000000, -5.000000000000000000 ) ) ;
#5090 =( LENGTH_UNIT ( ) NAMED_UNIT ( * ) SI_UNIT ( .MILLI., .METRE. ) );
#5091 = MECHANICAL_DESIGN_GEOMETRIC_PRESENTATION_REPRESENTATION (  '', ( #26388 ), #54501 ) ;
#5092 = DIRECTION ( 'NONE',  ( 0.000000000000000000, 0.000000000000000000, 1.000000000000000000 ) ) ;
#5093 = ORIENTED_EDGE ( 'NONE', *, *, #15996, .F. ) ;
#5094 = CIRCLE ( 'NONE', #54507, 5.000000000000004441 ) ;
#5095 = ORIENTED_EDGE ( 'NONE', *, *, #48628, .F. ) ;
#5096 = EDGE_CURVE ( 'NONE', #65582, #51799, #552, .T. ) ;
#5097 = CARTESIAN_POINT ( 'NONE',  ( -160.4929263765338021, -8.102448949553174629, 5.886773742842742685 ) ) ;
#5098 =( NAMED_UNIT ( * ) SI_UNIT ( $, .STERADIAN. ) SOLID_ANGLE_UNIT ( ) );
#5099 = CARTESIAN_POINT ( 'NONE',  ( 0.000000000000000000, 0.000000000000000000, -3.000000000000000444 ) ) ;
#5100 = CARTESIAN_POINT ( 'NONE',  ( -158.3070736234662093, -10.01517768586948698, 6.132527647946031529E-16 ) ) ;
#5101 = CARTESIAN_POINT ( 'NONE',  ( 10.01517768586949408, 123.6949999999999790, 1.839758294383810543E-15 ) ) ;
#5102 = SHAPE_REPRESENTATION ( 'MAS-684', ( #46147, #23648, #60693, #53976, #3367, #62969, #29264, #51752, #21390, #42802, #61853, #16955, #30360, #47312, #49587, #38312, #12391, #2239, #55070, #49534, #37207, #68618, #22560, #5662, #39413, #56236, #46194, #9052, #65231, #48410 ), #34903 ) ;
#5103 = CARTESIAN_POINT ( 'NONE',  ( -90.35707362346617799, 5.598654528085804216, 7.705886871421366635 ) ) ;
#5104 = EDGE_CURVE ( 'NONE', #1652, #46628, #35429, .T. ) ;
#5105 = VERTEX_POINT ( 'NONE', #58656 ) ;
#5106 = SURFACE_STYLE_USAGE ( .BOTH. , #26875 ) ;
#5108 = SURFACE_STYLE_FILL_AREA ( #31836 ) ;
#5107 = CYLINDRICAL_SURFACE ( 'NONE', #35717, 0.2500000000000002220 ) ;
#5109 = CARTESIAN_POINT ( 'NONE',  ( -8.437984349512095861, 130.8070736234661524, -5.166775262442723748E-16 ) ) ;
#5110 = CARTESIAN_POINT ( 'NONE',  ( -137.4549999999999841, 7.632228543268599452, -2.479861379858951942 ) ) ;
#5111 = SURFACE_STYLE_USAGE ( .BOTH. , #38206 ) ;
#5112 = CARTESIAN_POINT ( 'NONE',  ( -157.1950000000000216, 8.437984349512085203, -1.550032578732815448E-15 ) ) ;
#5113 = CARTESIAN_POINT ( 'NONE',  ( -142.4949999999999761, 6.826472737025113702, -4.959722759717902107 ) ) ;
#5114 = ORIENTED_EDGE ( 'NONE', *, *, #9314, .T. ) ;
#5115 = CARTESIAN_POINT ( 'NONE',  ( 179.4098300562505415, -5.000000000000010658, -6.123233995736778115E-16 ) ) ;
#5116 = DIRECTION ( 'NONE',  ( -1.000000000000000000, 0.000000000000000000, 0.000000000000000000 ) ) ;
#5117 = CARTESIAN_POINT ( 'NONE',  ( -63.44292637653379785, -1.166476076187852838E-15, -9.524999999999991473 ) ) ;
#5118 = UNCERTAINTY_MEASURE_WITH_UNIT (LENGTH_MEASURE( 1.000000000000000082E-05 ), #52629, 'distance_accuracy_value', 'NONE');
#5119 = CARTESIAN_POINT ( 'NONE',  ( -52.40499999999998693, -2.607480562269069768, 8.024999999999991473 ) ) ;
#5120 = STYLED_ITEM ( 'NONE', ( #56923 ), #64489 ) ;
#5121 = CARTESIAN_POINT ( 'NONE',  ( -52.94292637653380496, 0.000000000000000000, 9.524999999999991473 ) ) ;
#5122 = CARTESIAN_POINT ( 'NONE',  ( 60.00000000000000000, 1.797044900979284448E-15, 12.00000000000000000 ) ) ;
#5123 = CIRCLE ( 'NONE', #14139, 13.99999999999999822 ) ;
#5124 = UNCERTAINTY_MEASURE_WITH_UNIT (LENGTH_MEASURE( 1.000000000000000082E-05 ), #49961, 'distance_accuracy_value', 'NONE');
#5125 = CARTESIAN_POINT ( 'NONE',  ( -0.7999999999999327649, 50.00000000000002132, 60.00000000000001421 ) ) ;
#5126 = CARTESIAN_POINT ( 'NONE',  ( -153.4429263765338192, -1.166476076187852838E-15, -9.524999999999991473 ) ) ;
#5127 = ADVANCED_FACE ( 'NONE', ( #36202, #14727 ), #51657, .F. ) ;
#5128 = LINE ( 'NONE', #43181, #51734 ) ;
#5129 = DIRECTION ( 'NONE',  ( 0.000000000000000000, 0.000000000000000000, 1.000000000000000000 ) ) ;
#5130 = AXIS2_PLACEMENT_3D ( 'NONE', #30224, #35545, #61538 ) ;
#5131 = DIRECTION ( 'NONE',  ( 1.000000000000000000, -3.469446951953611033E-15, 0.000000000000000000 ) ) ;
#5132 = DIRECTION ( 'NONE',  ( 0.000000000000000000, -1.000000000000000000, 0.000000000000000000 ) ) ;
#5133 = AXIS2_PLACEMENT_3D ( 'NONE', #9533, #58060, #40505 ) ;
#5134 = PRESENTATION_STYLE_ASSIGNMENT (( #32224 ) ) ;
#5135 = AXIS2_PLACEMENT_3D ( 'NONE', #32791, #6391, #27137 ) ;
#5136 = ORIENTED_EDGE ( 'NONE', *, *, #63624, .T. ) ;
#5138 = CARTESIAN_POINT ( 'NONE',  ( -4.716976649647097730, 118.3570736234661638, -6.492361379858953896 ) ) ;
#5137 = AXIS2_PLACEMENT_3D ( 'NONE', #17563, #60426, #12585 ) ;
#5139 = ADVANCED_FACE ( 'NONE', ( #57629 ), #36570, .T. ) ;
#5140 = STYLED_ITEM ( 'NONE', ( #47684 ), #32592 ) ;
#5141 = CARTESIAN_POINT ( 'NONE',  ( 3.728548500389071485, -7.000000000000003553, 0.9264520766856032541 ) ) ;
#5142 = CARTESIAN_POINT ( 'NONE',  ( -74.99999999999998579, 50.00000000000000000, 9.500000000000001776 ) ) ;
#5143 = DIRECTION ( 'NONE',  ( 0.000000000000000000, -1.000000000000000000, 0.000000000000000000 ) ) ;
#5144 = ORIENTED_EDGE ( 'NONE', *, *, #42385, .F. ) ;
#5145 = ORIENTED_EDGE ( 'NONE', *, *, #63847, .T. ) ;
#5146 = CARTESIAN_POINT ( 'NONE',  ( -108.9570736234661723, 9.058813317711329915, -2.943386871421373119 ) ) ;
#5147 = EDGE_CURVE ( 'NONE', #20549, #29123, #21971, .T. ) ;
#5148 = CARTESIAN_POINT ( 'NONE',  ( -101.9929263765338021, 8.102448949553172852, -5.886773742842744461 ) ) ;
#5149 = ORIENTED_EDGE ( 'NONE', *, *, #13907, .T. ) ;
#5150 = ADVANCED_FACE ( 'NONE', ( #52707 ), #25263, .F. ) ;
#5151 = CARTESIAN_POINT ( 'NONE',  ( -10.01517768586949231, 117.3049999999999784, -6.132527647946036459E-16 ) ) ;
#5152 = CARTESIAN_POINT ( 'NONE',  ( -74.99999999999998579, 119.9999999999997726, 10.00000000000000000 ) ) ;
#5153 = DIRECTION ( 'NONE',  ( 1.000000000000000000, 0.000000000000000000, 0.000000000000000000 ) ) ;
#5154 = CARTESIAN_POINT ( 'NONE',  ( -104.2449999999999903, -4.716976649647093289, -6.492361379858945902 ) ) ;
#5155 = ORIENTED_EDGE ( 'NONE', *, *, #5961, .F. ) ;
#5156 =( GEOMETRIC_REPRESENTATION_CONTEXT ( 3 ) GLOBAL_UNCERTAINTY_ASSIGNED_CONTEXT ( ( #62289 ) ) GLOBAL_UNIT_ASSIGNED_CONTEXT ( ( #44266, #12183, #34000 ) ) REPRESENTATION_CONTEXT ( 'NONE', 'WORKASPACE' ) );
#5157 = CARTESIAN_POINT ( 'NONE',  ( 0.000000000000000000, 0.000000000000000000, 1.000000000000000000 ) ) ;
#5158 = LINE ( 'NONE', #59927, #8138 ) ;
#5159 = EDGE_CURVE ( 'NONE', #27999, #6972, #26419, .T. ) ;
#5160 = FILL_AREA_STYLE ('',( #69533 ) ) ;
#5161 = EDGE_LOOP ( 'NONE', ( #59188, #43424, #36157, #18899, #34260, #67235 ) ) ;
#5162 = CARTESIAN_POINT ( 'NONE',  ( -2.607480562269073765, 159.0929263765338533, -8.025000000000000355 ) ) ;
#5163 = EDGE_CURVE ( 'NONE', #42076, #29454, #44462, .T. ) ;
#5164 = CARTESIAN_POINT ( 'NONE',  ( 0.000000000000000000, 0.000000000000000000, 0.000000000000000000 ) ) ;
#5165 = ORIENTED_EDGE ( 'NONE', *, *, #38417, .F. ) ;
#5166 = STYLED_ITEM ( 'NONE', ( #29290 ), #49897 ) ;
#5167 = VECTOR ( 'NONE', #6991, 1000.000000000000000 ) ;
#5168 = CARTESIAN_POINT ( 'NONE',  ( -71.99999999999998579, 63.67479433117734544, 9.500000000000000000 ) ) ;
#5169 = DIRECTION ( 'NONE',  ( 0.000000000000000000, 0.000000000000000000, -1.000000000000000000 ) ) ;
#5170 = CARTESIAN_POINT ( 'NONE',  ( -34.01240315408732329, -9.962924773521290689, 4.367854888791723234 ) ) ;
#5171 = CARTESIAN_POINT ( 'NONE',  ( 23.50000000000001776, 14.00000000000000000, 29.68999999999999417 ) ) ;
#5172 = CARTESIAN_POINT ( 'NONE',  ( -125.6929263765338192, 10.01517768586948698, -1.839758294383808966E-15 ) ) ;
#5173 = DIRECTION ( 'NONE',  ( -1.000000000000000000, -1.445602896647336698E-16, 0.000000000000000000 ) ) ;
#5174 = CARTESIAN_POINT ( 'NONE',  ( 7.632228543268607446, 116.0429263765338277, 2.479861379858954606 ) ) ;
#5175 = DIRECTION ( 'NONE',  ( 0.000000000000000000, 0.000000000000000000, -1.000000000000000000 ) ) ;
#5176 = EDGE_LOOP ( 'NONE', ( #22307, #19176 ) ) ;
#5177 = ORIENTED_EDGE ( 'NONE', *, *, #1622, .T. ) ;
#5178 = CARTESIAN_POINT ( 'NONE',  ( -45.89905495956738690, 9.405628579031729330, -6.500000000000000000 ) ) ;
#5179 = DIRECTION ( 'NONE',  ( 0.000000000000000000, 1.000000000000000000, -0.000000000000000000 ) ) ;
#5180 = DIRECTION ( 'NONE',  ( 0.000000000000000000, 0.000000000000000000, 1.000000000000000000 ) ) ;
#5181 = CARTESIAN_POINT ( 'NONE',  ( 49.12162162162162105, 13.70805908423323594, -9.500000000000000000 ) ) ;
#5183 = ORIENTED_EDGE ( 'NONE', *, *, #9856, .T. ) ;
#5182 = CIRCLE ( 'NONE', #13026, 0.5000000000000004441 ) ;
#5184 = SURFACE_SIDE_STYLE ('',( #36904 ) ) ;
#5185 = CARTESIAN_POINT ( 'NONE',  ( -167.0049999999999670, 6.826472737025116366, 4.959722759717898555 ) ) ;
#5186 = SURFACE_STYLE_FILL_AREA ( #21032 ) ;
#5187 = EDGE_CURVE ( 'NONE', #11384, #21950, #32267, .T. ) ;
#5188 = DIRECTION ( 'NONE',  ( 0.000000000000000000, 0.000000000000000000, -1.000000000000000000 ) ) ;
#5189 = CARTESIAN_POINT ( 'NONE',  ( -49.40707362346615383, 3.094860106618428031, -9.524999999999993250 ) ) ;
#5190 = AXIS2_PLACEMENT_3D ( 'NONE', #68706, #36001, #52880 ) ;
#5191 = CARTESIAN_POINT ( 'NONE',  ( -166.9450000000000216, -9.827790563157499189E-16, -8.024999999999991473 ) ) ;
#5192 = EDGE_CURVE ( 'NONE', #2770, #25430, #14086, .T. ) ;
#5193 = ORIENTED_EDGE ( 'NONE', *, *, #19621, .T. ) ;
#5194 = CARTESIAN_POINT ( 'NONE',  ( 9.566487832665400148, 1.430357023834056385, 0.6362876910938520814 ) ) ;
#5195 = CARTESIAN_POINT ( 'NONE',  ( -38.88671403932455206, -11.45492897060496240, 3.435370330900509916 ) ) ;
#5196 = CARTESIAN_POINT ( 'NONE',  ( -12.48648248363261004, 11.19366133502252048, -4.325373782235834241 ) ) ;
#5197 = CARTESIAN_POINT ( 'NONE',  ( -84.95499999999998408, -7.632228543268599452, 2.479861379858951054 ) ) ;
#5198 = CARTESIAN_POINT ( 'NONE',  ( -15.00000000000000000, 8.000000000000000000, 3.500000000000003997 ) ) ;
#5199 = CARTESIAN_POINT ( 'NONE',  ( 16.00000000000001776, 14.00000000000000000, -33.68999999999999773 ) ) ;
#5200 = CARTESIAN_POINT ( 'NONE',  ( -78.29499999999994486, -2.607480562269069768, 8.024999999999991473 ) ) ;
#5201 = CARTESIAN_POINT ( 'NONE',  ( 5.598654528085805993, 136.3550000000000182, 7.705886871421374629 ) ) ;
#5202 = FACE_OUTER_BOUND ( 'NONE', #27007, .T. ) ;
#5203 = PLANE ( 'NONE',  #50593 ) ;
#5204 = FILL_AREA_STYLE_COLOUR ( '', #42865 ) ;
#5205 = UNCERTAINTY_MEASURE_WITH_UNIT (LENGTH_MEASURE( 1.000000000000000082E-05 ), #10100, 'distance_accuracy_value', 'NONE');
#5206 = CARTESIAN_POINT ( 'NONE',  ( -108.0570736234661666, 0.000000000000000000, 9.524999999999991473 ) ) ;
#5207 = EDGE_LOOP ( 'NONE', ( #56502, #67294, #36694, #3662 ) ) ;
#5208 = CIRCLE ( 'NONE', #44589, 3.599999999999992095 ) ;
#5209 =( LENGTH_UNIT ( ) NAMED_UNIT ( * ) SI_UNIT ( .MILLI., .METRE. ) );
#5210 = AXIS2_PLACEMENT_3D ( 'NONE', #20300, #9073, #20666 ) ;
#5211 = EDGE_CURVE ( 'NONE', #42181, #69289, #11154, .T. ) ;
#5213 =( NAMED_UNIT ( * ) PLANE_ANGLE_UNIT ( ) SI_UNIT ( $, .RADIAN. ) );
#5212 = CARTESIAN_POINT ( 'NONE',  ( 23.50000000000001776, -3.148064030671221758, -27.18999999999999417 ) ) ;
#5214 = AXIS2_PLACEMENT_3D ( 'NONE', #35638, #25413, #36369 ) ;
#5215 = ORIENTED_EDGE ( 'NONE', *, *, #55313, .F. ) ;
#5216 = EDGE_LOOP ( 'NONE', ( #33426, #59584, #42951, #9873 ) ) ;
#5217 = CARTESIAN_POINT ( 'NONE',  ( -45.91547277936962246, 9.430195807687216103, -6.039972492249777503 ) ) ;
#5218 = CARTESIAN_POINT ( 'NONE',  ( -135.1429263765338078, 5.598654528085800663, -7.705886871421367523 ) ) ;
#5219 = EDGE_CURVE ( 'NONE', #53591, #3129, #6239, .T. ) ;
#5220 =( NAMED_UNIT ( * ) SI_UNIT ( $, .STERADIAN. ) SOLID_ANGLE_UNIT ( ) );
#5221 = SURFACE_SIDE_STYLE ('',( #26333 ) ) ;
#5222 = DIRECTION ( 'NONE',  ( 0.000000000000000000, 0.000000000000000000, -1.000000000000000000 ) ) ;
#5223 =( LENGTH_UNIT ( ) NAMED_UNIT ( * ) SI_UNIT ( .MILLI., .METRE. ) );
#5224 = EDGE_LOOP ( 'NONE', ( #24717, #5900, #9626, #63987 ) ) ;
#5225 = CARTESIAN_POINT ( 'NONE',  ( -119.9049999999999869, 2.607480562269069324, -8.024999999999993250 ) ) ;
#5226 = ORIENTED_EDGE ( 'NONE', *, *, #66932, .F. ) ;
#5227 = LINE ( 'NONE', #37992, #8471 ) ;
#5228 = AXIS2_PLACEMENT_3D ( 'NONE', #40664, #62075, #24438 ) ;
#5229 = CARTESIAN_POINT ( 'NONE',  ( 0.000000000000000000, 130.0570736234661524, -8.025000000000000355 ) ) ;
#5230 = EDGE_CURVE ( 'NONE', #40317, #57439, #63533, .T. ) ;
#5231 = ORIENTED_EDGE ( 'NONE', *, *, #60605, .F. ) ;
#5232 = LINE ( 'NONE', #26675, #52675 ) ;
#5233 = ORIENTED_EDGE ( 'NONE', *, *, #37871, .T. ) ;
#5234 = PRESENTATION_STYLE_ASSIGNMENT (( #26678 ) ) ;
#5235 = CARTESIAN_POINT ( 'NONE',  ( -10.01517768586949231, 152.1949999999999932, -6.132527647946036459E-16 ) ) ;
#5236 =( NAMED_UNIT ( * ) SI_UNIT ( $, .STERADIAN. ) SOLID_ANGLE_UNIT ( ) );
#5237 = ORIENTED_EDGE ( 'NONE', *, *, #20348, .T. ) ;
#5238 = STYLED_ITEM ( 'NONE', ( #36868 ), #46 ) ;
#5239 = CARTESIAN_POINT ( 'NONE',  ( -2.243484957755116582, 2.233878551459170136, 9.000000000000005329 ) ) ;
#5240 = DIRECTION ( 'NONE',  ( 0.000000000000000000, 0.000000000000000000, -1.000000000000000000 ) ) ;
#5241 = DIRECTION ( 'NONE',  ( 1.000000000000000000, -0.000000000000000000, -0.000000000000000000 ) ) ;
#5242 = ORIENTED_EDGE ( 'NONE', *, *, #30097, .T. ) ;
#5243 = CARTESIAN_POINT ( 'NONE',  ( -6.826472737025120807, 129.9929263765338021, 4.959722759717906548 ) ) ;
#5244 = UNCERTAINTY_MEASURE_WITH_UNIT (LENGTH_MEASURE( 1.000000000000000082E-05 ), #56322, 'distance_accuracy_value', 'NONE');
#5245 = DIRECTION ( 'NONE',  ( -1.000000000000000000, 0.000000000000000000, 0.000000000000000000 ) ) ;
#5246 =( GEOMETRIC_REPRESENTATION_CONTEXT ( 3 ) GLOBAL_UNCERTAINTY_ASSIGNED_CONTEXT ( ( #33976 ) ) GLOBAL_UNIT_ASSIGNED_CONTEXT ( ( #54648, #761, #59573 ) ) REPRESENTATION_CONTEXT ( 'NONE', 'WORKASPACE' ) );
#5247 = EDGE_CURVE ( 'NONE', #48466, #40049, #62384, .T. ) ;
#5248 = LINE ( 'NONE', #4557, #45252 ) ;
#5249 = ORIENTED_EDGE ( 'NONE', *, *, #38652, .F. ) ;
#5250 = DIRECTION ( 'NONE',  ( -0.000000000000000000, 0.000000000000000000, -1.000000000000000000 ) ) ;
#5251 = ORIENTED_EDGE ( 'NONE', *, *, #8824, .T. ) ;
#5252 = DIRECTION ( 'NONE',  ( -0.000000000000000000, 0.000000000000000000, 1.000000000000000000 ) ) ;
#5253 =( NAMED_UNIT ( * ) PLANE_ANGLE_UNIT ( ) SI_UNIT ( $, .RADIAN. ) );
#5254 = CARTESIAN_POINT ( 'NONE',  ( -145.4050000000000296, -2.607480562269069768, 8.024999999999991473 ) ) ;
#5255 = LINE ( 'NONE', #64008, #20755 ) ;
#5256 =( LENGTH_UNIT ( ) NAMED_UNIT ( * ) SI_UNIT ( .MILLI., .METRE. ) );
#5257 = UNCERTAINTY_MEASURE_WITH_UNIT (LENGTH_MEASURE( 1.000000000000000082E-05 ), #33574, 'distance_accuracy_value', 'NONE');
#5258 = DIRECTION ( 'NONE',  ( 0.000000000000000000, 0.000000000000000000, -1.000000000000000000 ) ) ;
#5259 =( NAMED_UNIT ( * ) PLANE_ANGLE_UNIT ( ) SI_UNIT ( $, .RADIAN. ) );
#5260 = CARTESIAN_POINT ( 'NONE',  ( 22.99999999999999645, 5.000000000000000000, -72.00402776293825013 ) ) ;
#5261 = ORIENTED_EDGE ( 'NONE', *, *, #62101, .F. ) ;
#5262 = ORIENTED_EDGE ( 'NONE', *, *, #60547, .F. ) ;
#5263 = DIRECTION ( 'NONE',  ( 0.000000000000000000, 0.000000000000000000, -1.000000000000000000 ) ) ;
#5264 = TOROIDAL_SURFACE ( 'NONE', #48017, 14.49999999999999822, 0.5000000000000000000 ) ;
#5265 = CARTESIAN_POINT ( 'NONE',  ( -60.80499999999998550, -8.437984349512085203, 5.166775262442717831E-16 ) ) ;
#5266 = EDGE_LOOP ( 'NONE', ( #16790, #8004, #9779, #12242, #66524, #59127 ) ) ;
#5267 = DIRECTION ( 'NONE',  ( -1.000000000000000000, 0.000000000000000000, 0.000000000000000000 ) ) ;
#5268 = CARTESIAN_POINT ( 'NONE',  ( 27.99999999999998224, 5.000000000000000000, 72.00402776293822171 ) ) ;
#5270 = CIRCLE ( 'NONE', #31077, 0.2500000000000002220 ) ;
#5269 = DIRECTION ( 'NONE',  ( -1.000000000000000000, 0.000000000000000000, -0.000000000000000000 ) ) ;
#5271 = LINE ( 'NONE', #16906, #44801 ) ;
#5272 = STYLED_ITEM ( 'NONE', ( #41370 ), #50424 ) ;
#5273 = EDGE_CURVE ( 'NONE', #69646, #64044, #32599, .T. ) ;
#5274 = DIRECTION ( 'NONE',  ( 0.000000000000000000, 1.000000000000000000, 0.000000000000000000 ) ) ;
#5275 = ORIENTED_EDGE ( 'NONE', *, *, #15467, .F. ) ;
#5276 = CARTESIAN_POINT ( 'NONE',  ( -60.00000000000000000, -2.024042244987997205E-14, 10.00000000000000000 ) ) ;
#5277 = CARTESIAN_POINT ( 'NONE',  ( 15.98999599679679839, 117.9999999999999716, -7.000000000000000000 ) ) ;
#5278 =( NAMED_UNIT ( * ) PLANE_ANGLE_UNIT ( ) SI_UNIT ( $, .RADIAN. ) );
#5279 = CIRCLE ( 'NONE', #4156, 4.999999999999997335 ) ;
#5280 = CARTESIAN_POINT ( 'NONE',  ( -112.6449999999999960, 4.716976649647091513, -6.492361379858946790 ) ) ;
#5281 = CARTESIAN_POINT ( 'NONE',  ( -5.598654528085806881, 157.7450000000000045, -7.705886871421374629 ) ) ;
#5282 = CARTESIAN_POINT ( 'NONE',  ( -88.49500000000000455, 6.826472737025113702, -4.959722759717902107 ) ) ;
#5283 = CARTESIAN_POINT ( 'NONE',  ( -2.607480562269094637, 112.2070736234661439, -8.024999999999986144 ) ) ;
#5284 = FACE_OUTER_BOUND ( 'NONE', #30715, .T. ) ;
#5285 = LINE ( 'NONE', #35684, #4691 ) ;
#5286 = UNCERTAINTY_MEASURE_WITH_UNIT (LENGTH_MEASURE( 1.000000000000000082E-05 ), #37377, 'distance_accuracy_value', 'NONE');
#5287 = FACE_OUTER_BOUND ( 'NONE', #51265, .T. ) ;
#5288 = VERTEX_POINT ( 'NONE', #16816 ) ;
#5289 = CARTESIAN_POINT ( 'NONE',  ( -129.1429263765338078, 5.598654528085800663, -7.705886871421367523 ) ) ;
#5290 = CARTESIAN_POINT ( 'NONE',  ( -150.2949999999999875, -2.607480562269069768, 8.024999999999991473 ) ) ;
#5291 = CARTESIAN_POINT ( 'NONE',  ( -8.082903768654761123, 1.417096231345241097, -1.759977097422839922E-15 ) ) ;
#5292 = EDGE_CURVE ( 'NONE', #34410, #12869, #11853, .T. ) ;
#5293 = CYLINDRICAL_SURFACE ( 'NONE', #45329, 9.524999999999991473 ) ;
#5294 =( NAMED_UNIT ( * ) SI_UNIT ( $, .STERADIAN. ) SOLID_ANGLE_UNIT ( ) );
#5295 = ORIENTED_EDGE ( 'NONE', *, *, #26733, .F. ) ;
#5296 = ORIENTED_EDGE ( 'NONE', *, *, #13243, .F. ) ;
#5297 = CYLINDRICAL_SURFACE ( 'NONE', #57738, 10.00000000000000000 ) ;
#5298 = UNCERTAINTY_MEASURE_WITH_UNIT (LENGTH_MEASURE( 1.000000000000000082E-05 ), #1309, 'distance_accuracy_value', 'NONE');
#5299 = CARTESIAN_POINT ( 'NONE',  ( -44.99999999999966604, 8.592356338113384950, 6.069948737345426615 ) ) ;
#5300 = CARTESIAN_POINT ( 'NONE',  ( -59.54292637653379927, 9.058813317711329915, 2.943386871421369566 ) ) ;
#5301 = CIRCLE ( 'NONE', #52556, 4.499999999999997335 ) ;
#5302 = CARTESIAN_POINT ( 'NONE',  ( -60.70461754965442935, -8.499999999999994671, 2.168404344971008868E-16 ) ) ;
#5303 = AXIS2_PLACEMENT_3D ( 'NONE', #59009, #36571, #10824 ) ;
#5304 = FILL_AREA_STYLE_COLOUR ( '', #12879 ) ;
#5305 = ORIENTED_EDGE ( 'NONE', *, *, #41103, .T. ) ;
#5306 = CARTESIAN_POINT ( 'NONE',  ( -150.5049999999999955, -6.826472737025113702, -4.959722759717900331 ) ) ;
#5307 = EDGE_CURVE ( 'NONE', #29039, #37744, #53717, .T. ) ;
#5308 = AXIS2_PLACEMENT_3D ( 'NONE', #65029, #32338, #621 ) ;
#5309 = VERTEX_POINT ( 'NONE', #22070 ) ;
#5310 = CARTESIAN_POINT ( 'NONE',  ( 6.062177826491070398, 3.500000000000002665, 0.000000000000000000 ) ) ;
#5311 = CARTESIAN_POINT ( 'NONE',  ( -142.5570736234661808, -1.166476076187852838E-15, -9.524999999999991473 ) ) ;
#5313 = ORIENTED_EDGE ( 'NONE', *, *, #33898, .F. ) ;
#5312 = EDGE_CURVE ( 'NONE', #7443, #60790, #10485, .T. ) ;
#5314 = EDGE_CURVE ( 'NONE', #849, #69341, #17470, .T. ) ;
#5315 = LINE ( 'NONE', #52856, #18568 ) ;
#5316 = CARTESIAN_POINT ( 'NONE',  ( 3.094860106618431583, 120.0949999999999704, 9.525000000000000355 ) ) ;
#5317 = LINE ( 'NONE', #58807, #21620 ) ;
#5318 = ORIENTED_EDGE ( 'NONE', *, *, #14255, .T. ) ;
#5319 =( NAMED_UNIT ( * ) PLANE_ANGLE_UNIT ( ) SI_UNIT ( $, .RADIAN. ) );
#5321 = EDGE_CURVE ( 'NONE', #58314, #2782, #32055, .T. ) ;
#5320 = CARTESIAN_POINT ( 'NONE',  ( 10.01517768586949408, 121.8049999999999642, 1.839758294383810543E-15 ) ) ;
#5322 = CARTESIAN_POINT ( 'NONE',  ( -68.75499999999998124, 4.716976649647091513, -6.492361379858946790 ) ) ;
#5323 = CARTESIAN_POINT ( 'NONE',  ( -123.7449999999999903, 4.716976649647094177, 6.492361379858945902 ) ) ;
#5324 = CARTESIAN_POINT ( 'NONE',  ( 0.000000000000000000, 1.000000000000000222, 4.000000000000000000 ) ) ;
#5325 = ORIENTED_EDGE ( 'NONE', *, *, #52039, .T. ) ;
#5326 = CARTESIAN_POINT ( 'NONE',  ( 3.094860106618435136, 152.4049999999999443, -9.525000000000000355 ) ) ;
#5327 = UNCERTAINTY_MEASURE_WITH_UNIT (LENGTH_MEASURE( 1.000000000000000082E-05 ), #7640, 'distance_accuracy_value', 'NONE');
#5328 = MECHANICAL_DESIGN_GEOMETRIC_PRESENTATION_REPRESENTATION (  '', ( #51396 ), #787 ) ;
#5329 = SURFACE_SIDE_STYLE ('',( #32407 ) ) ;
#5331 = EDGE_CURVE ( 'NONE', #44875, #43499, #2786, .T. ) ;
#5330 = VECTOR ( 'NONE', #53120, 1000.000000000000000 ) ;
#5332 = CARTESIAN_POINT ( 'NONE',  ( -74.99999999999998579, 50.00000000000000000, -12.00000000000000000 ) ) ;
#5333 = FACE_BOUND ( 'NONE', #665, .T. ) ;
#5334 = FILL_AREA_STYLE ('',( #358 ) ) ;
#5335 = ORIENTED_EDGE ( 'NONE', *, *, #56471, .F. ) ;
#5336 = DIRECTION ( 'NONE',  ( 1.000000000000000000, -0.000000000000000000, -1.300977106640434891E-16 ) ) ;
#5337 = CARTESIAN_POINT ( 'NONE',  ( -170.3049999999999784, 8.437984349512085203, -1.550032578732815448E-15 ) ) ;
#5338 = ORIENTED_EDGE ( 'NONE', *, *, #36758, .T. ) ;
#5339 = CARTESIAN_POINT ( 'NONE',  ( -87.20707362346618652, 3.094860106618433360, 9.524999999999991473 ) ) ;
#5340 = UNCERTAINTY_MEASURE_WITH_UNIT (LENGTH_MEASURE( 1.000000000000000082E-05 ), #45102, 'distance_accuracy_value', 'NONE');
#5341 = DIRECTION ( 'NONE',  ( 0.000000000000000000, 0.000000000000000000, 1.000000000000000000 ) ) ;
#5342 = CARTESIAN_POINT ( 'NONE',  ( -71.50000000000000000, 50.00000000000000000, 7.500000000000000000 ) ) ;
#5343 = VERTEX_POINT ( 'NONE', #26956 ) ;
#5344 = CARTESIAN_POINT ( 'NONE',  ( -128.7570736234661695, -5.598654528085801552, 7.705886871421367523 ) ) ;
#5345 = CARTESIAN_POINT ( 'NONE',  ( 60.00000000000000000, 149.4999999999999716, 9.500000000000000000 ) ) ;
#5346 = CARTESIAN_POINT ( 'NONE',  ( -95.30499999999997840, 8.437984349512085203, -1.550032578732815448E-15 ) ) ;
#5347 = EDGE_LOOP ( 'NONE', ( #42508, #19590, #36681 ) ) ;
#5348 = CARTESIAN_POINT ( 'NONE',  ( 0.000000000000000000, 2.500000000000000000, 0.000000000000000000 ) ) ;
#5349 = DIRECTION ( 'NONE',  ( 1.000000000000000000, 0.000000000000000000, -0.000000000000000000 ) ) ;
#5350 = CARTESIAN_POINT ( 'NONE',  ( -129.5070736234661695, 8.102448949553176405, 5.886773742842740909 ) ) ;
#5351 = CARTESIAN_POINT ( 'NONE',  ( -60.00000000000000000, -2.024042244987997205E-14, 7.000000000000000000 ) ) ;
#5352 = CARTESIAN_POINT ( 'NONE',  ( -69.20707362346617231, 3.094860106618433360, 9.524999999999991473 ) ) ;
#5353 = TOROIDAL_SURFACE ( 'NONE', #45823, 1.000000000000000000, 0.5000000000000000000 ) ;
#5354 = DIRECTION ( 'NONE',  ( -1.000000000000000000, 0.000000000000000000, 0.000000000000000000 ) ) ;
#5355 = ORIENTED_EDGE ( 'NONE', *, *, #45159, .F. ) ;
#5356 = SURFACE_SIDE_STYLE ('',( #52893 ) ) ;
#5357 = AXIS2_PLACEMENT_3D ( 'NONE', #4735, #4361, #53622 ) ;
#5358 =( NAMED_UNIT ( * ) PLANE_ANGLE_UNIT ( ) SI_UNIT ( $, .RADIAN. ) );
#5359 = STYLED_ITEM ( 'NONE', ( #65322 ), #65984 ) ;
#5360 = CARTESIAN_POINT ( 'NONE',  ( -108.3549999999999898, -4.716976649647093289, -6.492361379858945902 ) ) ;
#5361 = CARTESIAN_POINT ( 'NONE',  ( 5.598654528085809545, 124.1449999999999960, -7.705886871421373741 ) ) ;
#5362 = CARTESIAN_POINT ( 'NONE',  ( -113.5449999999999875, -7.632228543268600340, -2.479861379858950166 ) ) ;
#5363 = DIRECTION ( 'NONE',  ( 0.000000000000000000, 0.000000000000000000, 1.000000000000000000 ) ) ;
#5365 =( NAMED_UNIT ( * ) PLANE_ANGLE_UNIT ( ) SI_UNIT ( $, .RADIAN. ) );
#5364 = SURFACE_STYLE_FILL_AREA ( #32126 ) ;
#5366 = VERTEX_POINT ( 'NONE', #38637 ) ;
#5367 = CARTESIAN_POINT ( 'NONE',  ( -164.2429263765338021, 5.598654528085804216, 7.705886871421366635 ) ) ;
#5368 = SHAPE_REPRESENTATION_RELATIONSHIP ( 'NONE' , 'NONE' ,  #22166, #175 ) ;
#5369 = CARTESIAN_POINT ( 'NONE',  ( -180.4449999999999932, 0.000000000000000000, 8.024999999999991473 ) ) ;
#5370 = CYLINDRICAL_SURFACE ( 'NONE', #25347, 8.025000000000000355 ) ;
#5371 = EDGE_CURVE ( 'NONE', #42163, #1442, #69555, .T. ) ;
#5372 = CARTESIAN_POINT ( 'NONE',  ( -43.24699869027381993, -14.00614972214689047, 0.7701856363860615229 ) ) ;
#5373 = CARTESIAN_POINT ( 'NONE',  ( -18.25000000000000711, 33.99999999999999289, -3.750000000000000000 ) ) ;
#5374 = VERTEX_POINT ( 'NONE', #49506 ) ;
#5375 = CARTESIAN_POINT ( 'NONE',  ( -75.29292637653381348, 3.094860106618428031, -9.524999999999993250 ) ) ;
#5376 = ITEM_DEFINED_TRANSFORMATION ( 'NONE', 'NONE', #49534,  #42840 ) ;
#5378 = ADVANCED_FACE ( 'NONE', ( #27312 ), #48495, .F. ) ;
#5377 = CARTESIAN_POINT ( 'NONE',  ( 19.49999999999999645, 8.000000000000000000, 4.000000000000000000 ) ) ;
#5379 =( NAMED_UNIT ( * ) SI_UNIT ( $, .STERADIAN. ) SOLID_ANGLE_UNIT ( ) );
#5380 =( NAMED_UNIT ( * ) PLANE_ANGLE_UNIT ( ) SI_UNIT ( $, .RADIAN. ) );
#5381 = CARTESIAN_POINT ( 'NONE',  ( 108.3664351561509278, 13.00000000000000178, 18.43563588791581154 ) ) ;
#5382 = CARTESIAN_POINT ( 'NONE',  ( -5.196152422706634688, -9.000000000000005329, 1.392304845413258052 ) ) ;
#5383 = EDGE_CURVE ( 'NONE', #33963, #27344, #51150, .T. ) ;
#5384 = CARTESIAN_POINT ( 'NONE',  ( -183.2050000000000125, -2.607480562269071545, -8.024999999999991473 ) ) ;
#5385 = EDGE_LOOP ( 'NONE', ( #45720, #20459, #23660, #56399 ) ) ;
#5386 = DIRECTION ( 'NONE',  ( 0.000000000000000000, -1.000000000000000000, 0.000000000000000000 ) ) ;
#5387 = DIRECTION ( 'NONE',  ( 0.000000000000000000, -0.000000000000000000, 1.000000000000000000 ) ) ;
#5388 = ADVANCED_FACE ( 'NONE', ( #54411, #194, #21718 ), #37949, .T. ) ;
#5389 = DIRECTION ( 'NONE',  ( 0.000000000000000000, -1.000000000000000000, 0.000000000000000000 ) ) ;
#5390 = AXIS2_PLACEMENT_3D ( 'NONE', #9681, #4004, #52248 ) ;
#5391 =( BOUNDED_CURVE ( )  B_SPLINE_CURVE ( 2, ( #16464, #59303, #11131, #523, #60019, #32580, #54043, #11486, #5847, #6213, #11831 ),
 .UNSPECIFIED., .F., .F. ) 
 B_SPLINE_CURVE_WITH_KNOTS ( ( 3, 2, 2, 2, 2, 3 ),
 ( 0.06521739130434632548, 0.06739130434782453216, 0.06956521739130275273, 0.07173913043478095941, 0.07391304347825917997, 0.07608695652173738666 ),
 .UNSPECIFIED. ) 
 CURVE ( )  GEOMETRIC_REPRESENTATION_ITEM ( )  RATIONAL_B_SPLINE_CURVE ( ( 1.000000000000033751, 0.9510565162951197804, 1.000000000000000000, 0.9510565162951535312, 1.000000000000000000, 0.9510565162951535312, 1.000000000000000000, 0.9510565162951535312, 1.000000000000000000, 0.9510565162951929441, 0.9999999999999605871 ) ) 
 REPRESENTATION_ITEM ( '' )  );
#5392 = SURFACE_SIDE_STYLE ('',( #59204 ) ) ;
#5393 = CARTESIAN_POINT ( 'NONE',  ( -4.716976649647098618, 146.2570736234661410, 6.492361379858953008 ) ) ;
#5394 = ORIENTED_EDGE ( 'NONE', *, *, #26451, .T. ) ;
#5396 = ADVANCED_FACE ( 'NONE', ( #23792 ), #61074, .T. ) ;
#5395 = CARTESIAN_POINT ( 'NONE',  ( 45.00000000000000000, 10.69371294336137623, -3.707106781186547906 ) ) ;
#5397 = CARTESIAN_POINT ( 'NONE',  ( -97.40499999999997272, -2.607480562269069768, 8.024999999999991473 ) ) ;
#5398 = UNCERTAINTY_MEASURE_WITH_UNIT (LENGTH_MEASURE( 1.000000000000000082E-05 ), #27204, 'distance_accuracy_value', 'NONE');
#5399 = VERTEX_POINT ( 'NONE', #66714 ) ;
#5400 = VECTOR ( 'NONE', #17434, 1000.000000000000000 ) ;
#5401 = CARTESIAN_POINT ( 'NONE',  ( -23.21231517720797655, 117.4999999999999716, 7.000000000000000000 ) ) ;
#5402 = DIRECTION ( 'NONE',  ( 0.000000000000000000, -1.000000000000000000, -0.000000000000000000 ) ) ;
#5403 = CARTESIAN_POINT ( 'NONE',  ( -33.89861118948983432, -9.947368421052626530, -2.264547950182262070 ) ) ;
#5404 = CARTESIAN_POINT ( 'NONE',  ( 1.802043943559354711, -2.359472279213376211, 9.000000000000003553 ) ) ;
#5405 = ORIENTED_EDGE ( 'NONE', *, *, #34309, .T. ) ;
#5406 = STYLED_ITEM ( 'NONE', ( #66658 ), #14177 ) ;
#5407 =( NAMED_UNIT ( * ) SI_UNIT ( $, .STERADIAN. ) SOLID_ANGLE_UNIT ( ) );
#5408 = CARTESIAN_POINT ( 'NONE',  ( -74.54499999999998749, -7.632228543268600340, -2.479861379858950166 ) ) ;
#5409 = ORIENTED_EDGE ( 'NONE', *, *, #19114, .F. ) ;
#5410 = PRESENTATION_LAYER_ASSIGNMENT (  '', '', ( #58257 ) ) ;
#5411 =( NAMED_UNIT ( * ) SI_UNIT ( $, .STERADIAN. ) SOLID_ANGLE_UNIT ( ) );
#5412 = DIRECTION ( 'NONE',  ( 0.000000000000000000, 0.3420201433256629953, -0.9396926207859104263 ) ) ;
#5413 = VERTEX_POINT ( 'NONE', #19189 ) ;
#5414 =( NAMED_UNIT ( * ) PLANE_ANGLE_UNIT ( ) SI_UNIT ( $, .RADIAN. ) );
#5415 = CARTESIAN_POINT ( 'NONE',  ( -124.1049999999999756, -6.826472737025115478, 4.959722759717900331 ) ) ;
#5416 = EDGE_LOOP ( 'NONE', ( #48385, #30225, #52911, #20775 ) ) ;
#5417 = CARTESIAN_POINT ( 'NONE',  ( -87.50000000000000000, -3.500000000000000000, 24.00000000000000000 ) ) ;
#5418 = VERTEX_POINT ( 'NONE', #40339 ) ;
#5419 = CARTESIAN_POINT ( 'NONE',  ( -160.7929263765341261, -3.094860106613354755, 9.525000000003679190 ) ) ;
#5420 = DIRECTION ( 'NONE',  ( 0.000000000000000000, -1.000000000000000000, 0.000000000000000000 ) ) ;
#5421 = DIRECTION ( 'NONE',  ( 0.000000000000000000, 0.000000000000000000, -1.000000000000000000 ) ) ;
#5422 = CARTESIAN_POINT ( 'NONE',  ( -162.6570736234661751, 9.058813317711329915, 2.943386871421369566 ) ) ;
#5423 = CARTESIAN_POINT ( 'NONE',  ( -8.102448949553179958, 125.4949999999999903, 5.886773742842747126 ) ) ;
#5424 = CARTESIAN_POINT ( 'NONE',  ( -98.90707362346618936, -3.094860106618429807, 9.524999999999991473 ) ) ;
#5425 = EDGE_CURVE ( 'NONE', #32302, #16942, #5123, .T. ) ;
#5426 = MECHANICAL_DESIGN_GEOMETRIC_PRESENTATION_REPRESENTATION (  '', ( #15576 ), #20052 ) ;
#5427 = EDGE_LOOP ( 'NONE', ( #53029, #27977, #45709, #59570 ) ) ;
#5429 = SURFACE_STYLE_FILL_AREA ( #64194 ) ;
#5428 = CARTESIAN_POINT ( 'NONE',  ( -84.49999999999997158, 50.00000000000000000, -10.49999999999999822 ) ) ;
#5430 = CIRCLE ( 'NONE', #32408, 0.2500000000000002220 ) ;
#5431 = CARTESIAN_POINT ( 'NONE',  ( -67.99999999999998579, -2.024042244987997205E-14, 12.00000000000000000 ) ) ;
#5432 = CARTESIAN_POINT ( 'NONE',  ( -137.3049999999999784, 8.437984349512085203, -1.550032578732815448E-15 ) ) ;
#5433 = CARTESIAN_POINT ( 'NONE',  ( -86.30707362346616662, -10.01517768586948698, 6.132527647946031529E-16 ) ) ;
#5434 = DIRECTION ( 'NONE',  ( -1.000000000000000000, 0.000000000000000000, 0.000000000000000000 ) ) ;
#5435 = SURFACE_STYLE_USAGE ( .BOTH. , #62548 ) ;
#5436 = CARTESIAN_POINT ( 'NONE',  ( -142.4949999999999761, 6.826472737025113702, -4.959722759717902107 ) ) ;
#5437 = VECTOR ( 'NONE', #2855, 1000.000000000000000 ) ;
#5438 = CARTESIAN_POINT ( 'NONE',  ( -138.5949999999999420, 2.607480562269072433, 8.024999999999991473 ) ) ;
#5439 = ORIENTED_EDGE ( 'NONE', *, *, #26963, .T. ) ;
#5440 =( LENGTH_UNIT ( ) NAMED_UNIT ( * ) SI_UNIT ( .MILLI., .METRE. ) );
#5441 = LINE ( 'NONE', #43513, #51910 ) ;
#5442 = CARTESIAN_POINT ( 'NONE',  ( -57.35499999999998977, -4.716976649647093289, -6.492361379858945902 ) ) ;
#5443 = CARTESIAN_POINT ( 'NONE',  ( -24.21231517720798010, 112.9999999999999858, 7.500000000000000000 ) ) ;
#5444 = AXIS2_PLACEMENT_3D ( 'NONE', #15971, #59521, #33165 ) ;
#5445 = EDGE_CURVE ( 'NONE', #40233, #30278, #42312, .T. ) ;
#5446 = EDGE_CURVE ( 'NONE', #40883, #21177, #44503, .T. ) ;
#5447 = SURFACE_STYLE_FILL_AREA ( #22352 ) ;
#5448 = CARTESIAN_POINT ( 'NONE',  ( 2.607480562269030688, 152.7070736234661581, 8.025000000000034106 ) ) ;
#5449 = AXIS2_PLACEMENT_3D ( 'NONE', #43447, #60250, #38502 ) ;
#5450 = DIRECTION ( 'NONE',  ( 1.000000000000000000, 0.000000000000000000, 0.000000000000000000 ) ) ;
#5451 = CARTESIAN_POINT ( 'NONE',  ( -102.5929263765337822, -3.094860106618431139, -9.524999999999991473 ) ) ;
#5452 = DIRECTION ( 'NONE',  ( -1.473213661637684706E-17, 1.473213661637684089E-17, 1.000000000000000000 ) ) ;
#5453 = EDGE_CURVE ( 'NONE', #8394, #4028, #18654, .T. ) ;
#5454 = CARTESIAN_POINT ( 'NONE',  ( -89.75707362346616947, -5.598654528085801552, 7.705886871421367523 ) ) ;
#5455 = CARTESIAN_POINT ( 'NONE',  ( -99.95707362346617231, 9.058813317711329915, -2.943386871421373119 ) ) ;
#5456 = STYLED_ITEM ( 'NONE', ( #17516 ), #68551 ) ;
#5457 =( LENGTH_UNIT ( ) NAMED_UNIT ( * ) SI_UNIT ( .MILLI., .METRE. ) );
#5458 = PRESENTATION_STYLE_ASSIGNMENT (( #4795 ) ) ;
#5459 = EDGE_CURVE ( 'NONE', #12723, #15255, #57976, .T. ) ;
#5460 = ORIENTED_EDGE ( 'NONE', *, *, #20519, .T. ) ;
#5461 = FACE_BOUND ( 'NONE', #34692, .T. ) ;
#5462 = CARTESIAN_POINT ( 'NONE',  ( 2.607480562269071989, 110.7070736234661723, 8.025000000000002132 ) ) ;
#5463 =( GEOMETRIC_REPRESENTATION_CONTEXT ( 3 ) GLOBAL_UNCERTAINTY_ASSIGNED_CONTEXT ( ( #53121 ) ) GLOBAL_UNIT_ASSIGNED_CONTEXT ( ( #67493, #13322, #51674 ) ) REPRESENTATION_CONTEXT ( 'NONE', 'WORKASPACE' ) );
#5464 = EDGE_CURVE ( 'NONE', #12869, #66608, #69170, .T. ) ;
#5465 = SURFACE_STYLE_FILL_AREA ( #37574 ) ;
#5466 = FILL_AREA_STYLE_COLOUR ( '', #22934 ) ;
#5467 = VERTEX_POINT ( 'NONE', #30794 ) ;
#5469 = ORIENTED_EDGE ( 'NONE', *, *, #49330, .F. ) ;
#5468 =( GEOMETRIC_REPRESENTATION_CONTEXT ( 3 ) GLOBAL_UNCERTAINTY_ASSIGNED_CONTEXT ( ( #68603 ) ) GLOBAL_UNIT_ASSIGNED_CONTEXT ( ( #56852, #42114, #19550 ) ) REPRESENTATION_CONTEXT ( 'NONE', 'WORKASPACE' ) );
#5470 = CARTESIAN_POINT ( 'NONE',  ( 65.00000000000000000, 1.797044900979284448E-15, -7.000000000000017764 ) ) ;
#5471 = FACE_OUTER_BOUND ( 'NONE', #61817, .T. ) ;
#5472 = DIRECTION ( 'NONE',  ( 1.189524669241239115E-16, 1.000000000000000000, 0.000000000000000000 ) ) ;
#5473 = ORIENTED_EDGE ( 'NONE', *, *, #65456, .T. ) ;
#5474 = CARTESIAN_POINT ( 'NONE',  ( 5.598654528085805993, 133.3549999999999898, 7.705886871421374629 ) ) ;
#5475 = PLANE ( 'NONE',  #28830 ) ;
#5476 = CARTESIAN_POINT ( 'NONE',  ( 75.00000000000000000, 19.99999999999997868, -6.000000000000000000 ) ) ;
#5477 =( GEOMETRIC_REPRESENTATION_CONTEXT ( 3 ) GLOBAL_UNCERTAINTY_ASSIGNED_CONTEXT ( ( #30606 ) ) GLOBAL_UNIT_ASSIGNED_CONTEXT ( ( #20747, #58717, #4895 ) ) REPRESENTATION_CONTEXT ( 'NONE', 'WORKASPACE' ) );
#5478 = DIRECTION ( 'NONE',  ( 1.000000000000000000, -0.000000000000000000, -1.300977106640434891E-16 ) ) ;
#5479 = CARTESIAN_POINT ( 'NONE',  ( -97.19499999999997897, 8.437984349512085203, -1.550032578732815448E-15 ) ) ;
#5480 = ORIENTED_EDGE ( 'NONE', *, *, #59212, .T. ) ;
#5481 = AXIS2_PLACEMENT_3D ( 'NONE', #38191, #37518, #43139 ) ;
#5482 =( BOUNDED_CURVE ( )  B_SPLINE_CURVE ( 2, ( #47867, #32641, #64677, #43942, #69267, #58698, #26324, #10523, #21063, #32301, #226 ),
 .UNSPECIFIED., .F., .F. ) 
 B_SPLINE_CURVE_WITH_KNOTS ( ( 3, 2, 2, 2, 2, 3 ),
 ( 0.5294117647058825815, 0.5352941176470590312, 0.5411764705882354809, 0.5470588235294120416, 0.5529411764705884913, 0.5588235294117649410 ),
 .UNSPECIFIED. ) 
 CURVE ( )  GEOMETRIC_REPRESENTATION_ITEM ( )  RATIONAL_B_SPLINE_CURVE ( ( 0.9999999999999981126, 0.9510565162951554186, 1.000000000000000000, 0.9510565162951535312, 1.000000000000000000, 0.9510565162951535312, 1.000000000000000000, 0.9510565162951535312, 1.000000000000000000, 0.9510565162951516438, 1.000000000000001776 ) ) 
 REPRESENTATION_ITEM ( '' )  );
#5483 = SURFACE_STYLE_FILL_AREA ( #54039 ) ;
#5484 = ORIENTED_EDGE ( 'NONE', *, *, #59951, .F. ) ;
#5485 = CARTESIAN_POINT ( 'NONE',  ( -7.632228543268608334, 150.8429263765338249, 2.479861379858952830 ) ) ;
#5486 = CIRCLE ( 'NONE', #68446, 0.2500000000000002220 ) ;
#5487 = LINE ( 'NONE', #50432, #19449 ) ;
#5488 = CYLINDRICAL_SURFACE ( 'NONE', #12782, 9.524999999999991473 ) ;
#5489 = VERTEX_POINT ( 'NONE', #67755 ) ;
#5490 = CARTESIAN_POINT ( 'NONE',  ( 10.00000000000000533, 43.00000000000000000, -45.61250543006183733 ) ) ;
#5491 = DIRECTION ( 'NONE',  ( -0.9486832980505138790, -0.3162277660168378857, 0.000000000000000000 ) ) ;
#5492 =( NAMED_UNIT ( * ) PLANE_ANGLE_UNIT ( ) SI_UNIT ( $, .RADIAN. ) );
#5494 = AXIS2_PLACEMENT_3D ( 'NONE', #37092, #389, #21919 ) ;
#5493 = CYLINDRICAL_SURFACE ( 'NONE', #41170, 9.524999999999991473 ) ;
#5495 =( NAMED_UNIT ( * ) PLANE_ANGLE_UNIT ( ) SI_UNIT ( $, .RADIAN. ) );
#5496 = COLOUR_RGB ( '', 0.72549020, 0.75294118, 0.79215686) ;
#5497 = FILL_AREA_STYLE ('',( #10814 ) ) ;
#5498 = ADVANCED_FACE ( 'NONE', ( #51572 ), #41050, .F. ) ;
#5499 =( NAMED_UNIT ( * ) SI_UNIT ( $, .STERADIAN. ) SOLID_ANGLE_UNIT ( ) );
#5500 = DIRECTION ( 'NONE',  ( -1.000000000000000000, 0.000000000000000000, 0.000000000000000000 ) ) ;
#5501 = DIRECTION ( 'NONE',  ( 0.000000000000000000, -1.000000000000000000, 0.000000000000000000 ) ) ;
#5502 = CARTESIAN_POINT ( 'NONE',  ( -114.7429263765338021, -5.598654528085803328, -7.705886871421366635 ) ) ;
#5503 = ORIENTED_EDGE ( 'NONE', *, *, #7396, .T. ) ;
#5504 = AXIS2_PLACEMENT_3D ( 'NONE', #67675, #67322, #3978 ) ;
#5505 = EDGE_LOOP ( 'NONE', ( #53290, #17646, #51894, #42608 ) ) ;
#5506 = LINE ( 'NONE', #5178, #16056 ) ;
#5507 = DIRECTION ( 'NONE',  ( 1.000000000000000000, 0.000000000000000000, 0.000000000000000000 ) ) ;
#5508 = CARTESIAN_POINT ( 'NONE',  ( -40.78947368421051323, 108.1536491499103505, 10.00000000000000000 ) ) ;
#5509 = CARTESIAN_POINT ( 'NONE',  ( -43.99999999999998579, 1.469576158976823356E-15, -11.99999999999999467 ) ) ;
#5510 = ORIENTED_EDGE ( 'NONE', *, *, #51804, .F. ) ;
#5511 = DIRECTION ( 'NONE',  ( 0.000000000000000000, -0.000000000000000000, 1.000000000000000000 ) ) ;
#5512 = CARTESIAN_POINT ( 'NONE',  ( -164.9049999999999443, 2.607480562269068880, -8.024999999999993250 ) ) ;
#5513 = LINE ( 'NONE', #53722, #61043 ) ;
#5514 = DIRECTION ( 'NONE',  ( 1.000000000000000000, 0.000000000000000000, -0.000000000000000000 ) ) ;
#5515 = CARTESIAN_POINT ( 'NONE',  ( -178.4949999999999477, 6.826472737025113702, -4.959722759717902107 ) ) ;
#5516 = CARTESIAN_POINT ( 'NONE',  ( -163.6449999999999818, 4.716976649647091513, -6.492361379858946790 ) ) ;
#5517 = AXIS2_PLACEMENT_3D ( 'NONE', #42433, #36083, #69132 ) ;
#5518 = MECHANICAL_DESIGN_GEOMETRIC_PRESENTATION_REPRESENTATION (  '', ( #28006 ), #44904 ) ;
#5519 = ORIENTED_EDGE ( 'NONE', *, *, #3137, .F. ) ;
#5520 = EDGE_CURVE ( 'NONE', #41879, #60408, #35406, .T. ) ;
#5522 =( LENGTH_UNIT ( ) NAMED_UNIT ( * ) SI_UNIT ( .MILLI., .METRE. ) );
#5521 =( GEOMETRIC_REPRESENTATION_CONTEXT ( 3 ) GLOBAL_UNCERTAINTY_ASSIGNED_CONTEXT ( ( #59975 ) ) GLOBAL_UNIT_ASSIGNED_CONTEXT ( ( #5040, #59178, #17000 ) ) REPRESENTATION_CONTEXT ( 'NONE', 'WORKASPACE' ) );
#5523 = CARTESIAN_POINT ( 'NONE',  ( -10.25964396124710021, 11.89359207642228533, -1.623549840978965930 ) ) ;
#5524 = EDGE_CURVE ( 'NONE', #61802, #68002, #20871, .T. ) ;
#5525 = CARTESIAN_POINT ( 'NONE',  ( -83.30500000000000682, 8.437984349512085203, -1.550032578732815448E-15 ) ) ;
#5526 = CARTESIAN_POINT ( 'NONE',  ( 0.000000000000000000, 154.5000000000000000, -9.524999999999998579 ) ) ;
#5527 = CARTESIAN_POINT ( 'NONE',  ( 21.02379604162863913, 110.4999999999999858, 10.00000000000000000 ) ) ;
#5528 = CARTESIAN_POINT ( 'NONE',  ( -74.93847439803357702, 36.28117515973496410, -9.953338452613744280 ) ) ;
#5529 = EDGE_CURVE ( 'NONE', #47886, #45514, #1246, .T. ) ;
#5530 = CARTESIAN_POINT ( 'NONE',  ( -77.84499999999998465, -7.632228543268599452, 2.479861379858951054 ) ) ;
#5531 = EDGE_CURVE ( 'NONE', #41269, #55073, #53895, .T. ) ;
#5532 = CARTESIAN_POINT ( 'NONE',  ( -8.102448949553181734, 141.6050000000000182, 5.886773742842747126 ) ) ;
#5533 = CARTESIAN_POINT ( 'NONE',  ( 0.000000000000000000, 125.9429263765338192, -8.025000000000000355 ) ) ;
#5534 = VECTOR ( 'NONE', #9742, 1000.000000000000000 ) ;
#5535 = AXIS2_PLACEMENT_3D ( 'NONE', #21699, #59665, #7261 ) ;
#5536 = CARTESIAN_POINT ( 'NONE',  ( -171.0570736234661808, 0.000000000000000000, 9.524999999999991473 ) ) ;
#5537 = CIRCLE ( 'NONE', #12270, 1.000000000000000888 ) ;
#5538 = AXIS2_PLACEMENT_3D ( 'NONE', #67662, #35658, #8918 ) ;
#5539 = CARTESIAN_POINT ( 'NONE',  ( -74.54292637653379927, 9.058813317711329915, 2.943386871421369566 ) ) ;
#5540 = CIRCLE ( 'NONE', #31358, 4.999999999999997335 ) ;
#5541 = SURFACE_STYLE_FILL_AREA ( #37635 ) ;
#5542 = VERTEX_POINT ( 'NONE', #53446 ) ;
#5543 = ADVANCED_FACE ( 'NONE', ( #21075, #63643 ), #64689, .T. ) ;
#5544 = CARTESIAN_POINT ( 'NONE',  ( 0.000000000000000000, 131.9429263765338192, -8.025000000000000355 ) ) ;
#5545 =( GEOMETRIC_REPRESENTATION_CONTEXT ( 3 ) GLOBAL_UNCERTAINTY_ASSIGNED_CONTEXT ( ( #31326 ) ) GLOBAL_UNIT_ASSIGNED_CONTEXT ( ( #60743, #1623, #45325 ) ) REPRESENTATION_CONTEXT ( 'NONE', 'WORKASPACE' ) );
#5546 = EDGE_CURVE ( 'NONE', #20411, #29207, #13420, .T. ) ;
#5547 = FILL_AREA_STYLE_COLOUR ( '', #56268 ) ;
#5548 = LINE ( 'NONE', #49454, #60671 ) ;
#5549 = DIRECTION ( 'NONE',  ( 0.000000000000000000, 0.000000000000000000, 1.000000000000000000 ) ) ;
#5550 = DIRECTION ( 'NONE',  ( 0.000000000000000000, 0.000000000000000000, 1.000000000000000000 ) ) ;
#5551 = ORIENTED_EDGE ( 'NONE', *, *, #4228, .T. ) ;
#5552 = COLOUR_RGB ( '', 0.08235294, 0.09019608, 0.10196078) ;
#5553 = ORIENTED_EDGE ( 'NONE', *, *, #53824, .T. ) ;
#5554 = CARTESIAN_POINT ( 'NONE',  ( 0.000000000000000000, -4.000000000000000000, 0.000000000000000000 ) ) ;
#5555 = DIRECTION ( 'NONE',  ( -0.000000000000000000, -0.000000000000000000, -1.000000000000000000 ) ) ;
#5556 =( LENGTH_UNIT ( ) NAMED_UNIT ( * ) SI_UNIT ( .MILLI., .METRE. ) );
#5557 = CIRCLE ( 'NONE', #1045, 5.000000000000004441 ) ;
#5558 = CARTESIAN_POINT ( 'NONE',  ( 22.00000000000001776, 43.00000000000000000, 45.61250543006183022 ) ) ;
#5559 = CYLINDRICAL_SURFACE ( 'NONE', #26221, 1.000000000000000888 ) ;
#5560 = ORIENTED_EDGE ( 'NONE', *, *, #21616, .F. ) ;
#5561 = CARTESIAN_POINT ( 'NONE',  ( -109.1049999999999898, -6.826472737025113702, 4.959722759717902107 ) ) ;
#5562 = ORIENTED_EDGE ( 'NONE', *, *, #64246, .T. ) ;
#5563 = CARTESIAN_POINT ( 'NONE',  ( 0.000000000000000000, -4.000000000000000000, 18.00000000000000000 ) ) ;
#5564 = CARTESIAN_POINT ( 'NONE',  ( -8.750000000000001776, 24.99999999999998579, 3.750000000000000000 ) ) ;
#5565 = ORIENTED_EDGE ( 'NONE', *, *, #8239, .T. ) ;
#5566 = CARTESIAN_POINT ( 'NONE',  ( -55.94292637653380496, 0.000000000000000000, 9.524999999999991473 ) ) ;
#5567 = CARTESIAN_POINT ( 'NONE',  ( -138.0570736234661808, 0.000000000000000000, 9.524999999999991473 ) ) ;
#5568 = VERTEX_POINT ( 'NONE', #59054 ) ;
#5570 = EDGE_CURVE ( 'NONE', #12708, #32796, #595, .T. ) ;
#5569 =( GEOMETRIC_REPRESENTATION_CONTEXT ( 3 ) GLOBAL_UNCERTAINTY_ASSIGNED_CONTEXT ( ( #32786 ) ) GLOBAL_UNIT_ASSIGNED_CONTEXT ( ( #39919, #8228, #44848 ) ) REPRESENTATION_CONTEXT ( 'NONE', 'WORKASPACE' ) );
#5572 = CARTESIAN_POINT ( 'NONE',  ( 10.39230484541326582, 1.107695154586738839, 1.440973567693753677E-18 ) ) ;
#5571 = CIRCLE ( 'NONE', #40469, 5.000000000000004441 ) ;
#5573 = CARTESIAN_POINT ( 'NONE',  ( 9.058813317711337021, 159.5449999999999875, 2.943386871421375783 ) ) ;
#5574 = FACE_OUTER_BOUND ( 'NONE', #32871, .T. ) ;
#5575 = EDGE_LOOP ( 'NONE', ( #36664, #51264, #47555, #64857 ) ) ;
#5576 =( NAMED_UNIT ( * ) SI_UNIT ( $, .STERADIAN. ) SOLID_ANGLE_UNIT ( ) );
#5577 = SURFACE_STYLE_USAGE ( .BOTH. , #16539 ) ;
#5578 = COLOUR_RGB ( '', 0.09019608, 0.27058824, 0.51372549) ;
#5579 = CARTESIAN_POINT ( 'NONE',  ( 8.000000000000001776, 31.24999999999998579, 3.750000000000000000 ) ) ;
#5580 = VERTEX_POINT ( 'NONE', #5564 ) ;
#5581 = CARTESIAN_POINT ( 'NONE',  ( 4.716976649647099507, 122.6429263765338220, -6.492361379858953008 ) ) ;
#5582 = CARTESIAN_POINT ( 'NONE',  ( 74.99999999999998579, 50.00000000000000000, 7.000000000000000000 ) ) ;
#5583 = FACE_OUTER_BOUND ( 'NONE', #20380, .T. ) ;
#5584 = CARTESIAN_POINT ( 'NONE',  ( 60.00000000000000000, 1.797044900979284448E-15, -11.50000000000000000 ) ) ;
#5585 = PRESENTATION_STYLE_ASSIGNMENT (( #59073 ) ) ;
#5586 = ORIENTED_EDGE ( 'NONE', *, *, #52985, .F. ) ;
#5587 = COLOUR_RGB ( '', 0.72549020, 0.75294118, 0.79215686) ;
#5588 = LINE ( 'NONE', #36976, #59886 ) ;
#5589 = ORIENTED_EDGE ( 'NONE', *, *, #48241, .T. ) ;
#5590 = CARTESIAN_POINT ( 'NONE',  ( -49.49292637653378790, -8.102448949553172852, 5.886773742842742685 ) ) ;
#5591 = STYLED_ITEM ( 'NONE', ( #449 ), #10891 ) ;
#5592 = DIRECTION ( 'NONE',  ( 0.000000000000000000, 1.000000000000000000, 0.000000000000000000 ) ) ;
#5593 = DIRECTION ( 'NONE',  ( 0.000000000000000000, 0.000000000000000000, -1.000000000000000000 ) ) ;
#5594 = CARTESIAN_POINT ( 'NONE',  ( -140.0049999999999386, 6.826472737025116366, 4.959722759717898555 ) ) ;
#5595 = STYLED_ITEM ( 'NONE', ( #10944 ), #34175 ) ;
#5596 = DIRECTION ( 'NONE',  ( 1.000000000000000000, 0.000000000000000000, 0.000000000000000000 ) ) ;
#5597 = CARTESIAN_POINT ( 'NONE',  ( -2.607480562269115509, 115.2070736234661865, -8.024999999999970157 ) ) ;
#5598 = STYLED_ITEM ( 'NONE', ( #40907 ), #33046 ) ;
#5599 = PRESENTATION_STYLE_ASSIGNMENT (( #32343 ) ) ;
#5600 = CARTESIAN_POINT ( 'NONE',  ( 41.21690152797561524, 107.8360404011451976, 3.444195824416762974 ) ) ;
#5601 = VERTEX_POINT ( 'NONE', #242 ) ;
#5602 = TOROIDAL_SURFACE ( 'NONE', #51679, 0.5000000000000000000, 0.2500000000000000000 ) ;
#5603 = ORIENTED_EDGE ( 'NONE', *, *, #68419, .F. ) ;
#5604 = CARTESIAN_POINT ( 'NONE',  ( -40.99999999999998579, 108.0000000000000000, -3.000000000000000444 ) ) ;
#5605 = CARTESIAN_POINT ( 'NONE',  ( -56.45499999999997698, 7.632228543268599452, -2.479861379858951942 ) ) ;
#5606 = ORIENTED_EDGE ( 'NONE', *, *, #31902, .F. ) ;
#5607 = DIRECTION ( 'NONE',  ( 1.000000000000000000, 0.000000000000000000, 0.000000000000000000 ) ) ;
#5608 = CARTESIAN_POINT ( 'NONE',  ( 71.99999999999998579, 119.9999999999997868, 7.500000000000000000 ) ) ;
#5609 = LINE ( 'NONE', #65049, #1998 ) ;
#5610 = FACE_OUTER_BOUND ( 'NONE', #10819, .T. ) ;
#5611 = DIRECTION ( 'NONE',  ( 0.000000000000000000, -1.000000000000000000, -0.000000000000000000 ) ) ;
#5612 = COLOUR_RGB ( '', 0.66274510, 0.83137255, 0.94901961) ;
#5613 = ORIENTED_EDGE ( 'NONE', *, *, #4428, .T. ) ;
#5614 = EDGE_CURVE ( 'NONE', #5967, #2421, #31650, .T. ) ;
#5615 = DIRECTION ( 'NONE',  ( -1.000000000000000000, 0.000000000000000000, 0.000000000000000000 ) ) ;
#5617 = CARTESIAN_POINT ( 'NONE',  ( -12.74999999999999822, -0.9999999999999995559, 7.000000000000001776 ) ) ;
#5616 = AXIS2_PLACEMENT_3D ( 'NONE', #36589, #31229, #67865 ) ;
#5618 = PRESENTATION_STYLE_ASSIGNMENT (( #16236 ) ) ;
#5619 = ADVANCED_FACE ( 'NONE', ( #26342 ), #17520, .T. ) ;
#5620 = CARTESIAN_POINT ( 'NONE',  ( -114.2949999999999875, -2.607480562269069768, 8.024999999999991473 ) ) ;
#5621 = CARTESIAN_POINT ( 'NONE',  ( 0.000000000000000000, 160.4449999999999932, -9.525000000000000355 ) ) ;
#5622 = CARTESIAN_POINT ( 'NONE',  ( -83.54499999999998749, -7.632228543268600340, -2.479861379858950166 ) ) ;
#5623 =( LENGTH_UNIT ( ) NAMED_UNIT ( * ) SI_UNIT ( .MILLI., .METRE. ) );
#5624 = CARTESIAN_POINT ( 'NONE',  ( 20.12916642283592950, 109.9999999999999858, 10.05319148936170137 ) ) ;
#5625 =( GEOMETRIC_REPRESENTATION_CONTEXT ( 3 ) GLOBAL_UNCERTAINTY_ASSIGNED_CONTEXT ( ( #57298 ) ) GLOBAL_UNIT_ASSIGNED_CONTEXT ( ( #219, #48522, #6257 ) ) REPRESENTATION_CONTEXT ( 'NONE', 'WORKASPACE' ) );
#5626 = DIRECTION ( 'NONE',  ( -1.000000000000000000, -6.938893903907221278E-15, -0.000000000000000000 ) ) ;
#5627 = CYLINDRICAL_SURFACE ( 'NONE', #58412, 13.99999999999999822 ) ;
#5629 = ORIENTED_EDGE ( 'NONE', *, *, #14798, .T. ) ;
#5628 = AXIS2_PLACEMENT_3D ( 'NONE', #24685, #45844, #18404 ) ;
#5630 = CARTESIAN_POINT ( 'NONE',  ( -131.5429263765338135, 9.058813317711329915, 2.943386871421369566 ) ) ;
#5631 = CARTESIAN_POINT ( 'NONE',  ( -144.2950000000000159, -2.607480562269069768, 8.024999999999991473 ) ) ;
#5632 = CARTESIAN_POINT ( 'NONE',  ( 23.71231517720798365, 112.9999999999999858, -9.500000000000000000 ) ) ;
#5633 = EDGE_CURVE ( 'NONE', #50095, #15159, #11210, .T. ) ;
#5634 = CARTESIAN_POINT ( 'NONE',  ( -47.99499999999998323, -6.826472737025113702, 4.959722759717902107 ) ) ;
#5635 = AXIS2_PLACEMENT_3D ( 'NONE', #47921, #9556, #26036 ) ;
#5636 = CARTESIAN_POINT ( 'NONE',  ( 1.000000000000000000, 42.00000000000000000, 80.00402776293826435 ) ) ;
#5637 = ORIENTED_EDGE ( 'NONE', *, *, #34773, .T. ) ;
#5638 = ORIENTED_EDGE ( 'NONE', *, *, #2960, .F. ) ;
#5639 = TOROIDAL_SURFACE ( 'NONE', #2222, 9.500000000000005329, 0.5000000000000000000 ) ;
#5640 = CARTESIAN_POINT ( 'NONE',  ( 68.99999999999998579, 36.75000000000000000, -3.000000000000000000 ) ) ;
#5641 = CARTESIAN_POINT ( 'NONE',  ( -13.25000000000000355, 28.24999999999998934, 3.750000000000000000 ) ) ;
#5642 = AXIS2_PLACEMENT_3D ( 'NONE', #53668, #11455, #58605 ) ;
#5643 = CARTESIAN_POINT ( 'NONE',  ( -15.98999599679679839, 118.4999999999999716, 10.00000000000000000 ) ) ;
#5644 = DIRECTION ( 'NONE',  ( 0.000000000000000000, 0.000000000000000000, 1.000000000000000000 ) ) ;
#5645 = CARTESIAN_POINT ( 'NONE',  ( -59.99292637653380211, 8.102448949553172852, -5.886773742842744461 ) ) ;
#5646 =( NAMED_UNIT ( * ) SI_UNIT ( $, .STERADIAN. ) SOLID_ANGLE_UNIT ( ) );
#5647 = FILL_AREA_STYLE ('',( #5304 ) ) ;
#5648 = VERTEX_POINT ( 'NONE', #50579 ) ;
#5649 = CARTESIAN_POINT ( 'NONE',  ( -155.1550000000000011, 7.632228543268600340, 2.479861379858949277 ) ) ;
#5650 = EDGE_CURVE ( 'NONE', #12618, #7642, #13199, .T. ) ;
#5651 = ORIENTED_EDGE ( 'NONE', *, *, #10981, .T. ) ;
#5652 = LINE ( 'NONE', #68673, #67230 ) ;
#5653 = DIRECTION ( 'NONE',  ( 0.000000000000000000, 1.000000000000000000, 0.000000000000000000 ) ) ;
#5654 = ORIENTED_EDGE ( 'NONE', *, *, #62423, .T. ) ;
#5655 = VECTOR ( 'NONE', #11194, 1000.000000000000114 ) ;
#5656 = VECTOR ( 'NONE', #18860, 1000.000000000000000 ) ;
#5657 = CARTESIAN_POINT ( 'NONE',  ( -54.93556801394916533, -8.762778093182603811, -2.500000000007031709 ) ) ;
#5658 = EDGE_CURVE ( 'NONE', #39399, #54750, #12579, .T. ) ;
#5659 = CARTESIAN_POINT ( 'NONE',  ( 9.058813317711338797, 120.8449999999999847, -2.943386871421372675 ) ) ;
#5660 = DIRECTION ( 'NONE',  ( -1.000000000000000000, -0.000000000000000000, -0.000000000000000000 ) ) ;
#5661 = MECHANICAL_DESIGN_GEOMETRIC_PRESENTATION_REPRESENTATION (  '', ( #43887 ), #22514 ) ;
#5662 = AXIS2_PLACEMENT_3D ( 'NONE', #27608, #814, #11450 ) ;
#5663 = ORIENTED_EDGE ( 'NONE', *, *, #65850, .T. ) ;
#5664 = CARTESIAN_POINT ( 'NONE',  ( -5.598654528085808657, 126.7549999999999812, 7.705886871421373741 ) ) ;
#5665 = CARTESIAN_POINT ( 'NONE',  ( -61.10499999999996845, -6.826472737025113702, 4.959722759717902107 ) ) ;
#5666 = CARTESIAN_POINT ( 'NONE',  ( -123.4449999999999932, 0.000000000000000000, 8.024999999999991473 ) ) ;
#5667 = DIRECTION ( 'NONE',  ( -1.000000000000000000, 0.000000000000000000, 0.000000000000000000 ) ) ;
#5668 = ORIENTED_EDGE ( 'NONE', *, *, #56144, .F. ) ;
#5669 = CARTESIAN_POINT ( 'NONE',  ( 0.000000000000000000, 152.5550000000000068, -9.525000000000000355 ) ) ;
#5670 = FACE_OUTER_BOUND ( 'NONE', #59898, .T. ) ;
#5671 = STYLED_ITEM ( 'NONE', ( #22012 ), #69676 ) ;
#5672 = DIRECTION ( 'NONE',  ( 1.000000000000000000, 0.000000000000000000, 0.000000000000000000 ) ) ;
#5673 = CYLINDRICAL_SURFACE ( 'NONE', #45209, 1.000000000000000888 ) ;
#5674 =( NAMED_UNIT ( * ) SI_UNIT ( $, .STERADIAN. ) SOLID_ANGLE_UNIT ( ) );
#5675 = DIRECTION ( 'NONE',  ( 0.000000000000000000, 0.000000000000000000, -1.000000000000000000 ) ) ;
#5676 = ORIENTED_EDGE ( 'NONE', *, *, #53086, .F. ) ;
#5677 = CARTESIAN_POINT ( 'NONE',  ( 48.74999999999999289, 24.99999999999998579, -3.750000000000000000 ) ) ;
#5679 = CARTESIAN_POINT ( 'NONE',  ( -171.8050000000000068, -8.437984349512085203, 5.166775262442717831E-16 ) ) ;
#5678 = MECHANICAL_DESIGN_GEOMETRIC_PRESENTATION_REPRESENTATION (  '', ( #30420 ), #65243 ) ;
#5680 = ORIENTED_EDGE ( 'NONE', *, *, #9323, .F. ) ;
#5681 = CYLINDRICAL_SURFACE ( 'NONE', #10377, 0.2500000000000002220 ) ;
#5682 = DIRECTION ( 'NONE',  ( 0.000000000000000000, 0.000000000000000000, -1.000000000000000000 ) ) ;
#5683 = VECTOR ( 'NONE', #61224, 1000.000000000000000 ) ;
#5684 = AXIS2_PLACEMENT_3D ( 'NONE', #6657, #49605, #1338 ) ;
#5685 =( LENGTH_UNIT ( ) NAMED_UNIT ( * ) SI_UNIT ( .MILLI., .METRE. ) );
#5686 = CARTESIAN_POINT ( 'NONE',  ( -44.99283348780034686, 9.603717787655236648, 3.208807429303570657 ) ) ;
#5687 = VERTEX_POINT ( 'NONE', #23164 ) ;
#5688 = LINE ( 'NONE', #23280, #66484 ) ;
#5689 = FACE_OUTER_BOUND ( 'NONE', #66185, .T. ) ;
#5690 = CARTESIAN_POINT ( 'NONE',  ( -83.90500000000000114, 2.607480562269068880, -8.024999999999993250 ) ) ;
#5691 = ORIENTED_EDGE ( 'NONE', *, *, #14288, .T. ) ;
#5692 = FACE_OUTER_BOUND ( 'NONE', #15423, .T. ) ;
#5693 = EDGE_CURVE ( 'NONE', #23198, #56887, #10766, .T. ) ;
#5694 = TOROIDAL_SURFACE ( 'NONE', #22534, 0.5000000000000000000, 0.2500000000000000000 ) ;
#5695 = CARTESIAN_POINT ( 'NONE',  ( -6.422934014168760974, 111.9999999999999858, 4.811085495980506721 ) ) ;
#5696 = CARTESIAN_POINT ( 'NONE',  ( 7.632228543268608334, 144.4570736234661581, -2.479861379858951942 ) ) ;
#5697 = DIRECTION ( 'NONE',  ( 0.000000000000000000, 0.000000000000000000, -1.000000000000000000 ) ) ;
#5698 = CARTESIAN_POINT ( 'NONE',  ( -62.90707362346616804, -3.094860106618429807, 9.524999999999991473 ) ) ;
#5699 = CIRCLE ( 'NONE', #24776, 5.499999999999976907 ) ;
#5700 =( NAMED_UNIT ( * ) SI_UNIT ( $, .STERADIAN. ) SOLID_ANGLE_UNIT ( ) );
#5701 = ORIENTED_EDGE ( 'NONE', *, *, #69502, .T. ) ;
#5702 = AXIS2_PLACEMENT_3D ( 'NONE', #19766, #61975, #14157 ) ;
#5703 = CARTESIAN_POINT ( 'NONE',  ( 92.41620014002536720, 5.000000000000000000, 24.00402776293825369 ) ) ;
#5705 =( LENGTH_UNIT ( ) NAMED_UNIT ( * ) SI_UNIT ( .MILLI., .METRE. ) );
#5704 =( LENGTH_UNIT ( ) NAMED_UNIT ( * ) SI_UNIT ( .MILLI., .METRE. ) );
#5706 = CARTESIAN_POINT ( 'NONE',  ( -105.2049999999999841, -2.607480562269071545, -8.024999999999991473 ) ) ;
#5707 = EDGE_CURVE ( 'NONE', #6066, #36322, #19747, .T. ) ;
#5708 = CARTESIAN_POINT ( 'NONE',  ( 3.094860106618431583, 132.0949999999999989, 9.525000000000000355 ) ) ;
#5709 = CARTESIAN_POINT ( 'NONE',  ( -115.9449999999999932, -9.827790563157499189E-16, -8.024999999999991473 ) ) ;
#5710 = MECHANICAL_DESIGN_GEOMETRIC_PRESENTATION_REPRESENTATION (  '', ( #43931 ), #18085 ) ;
#5711 = ADVANCED_FACE ( 'NONE', ( #28758 ), #59060, .T. ) ;
#5712 = CIRCLE ( 'NONE', #34958, 0.5000000000000004441 ) ;
#5714 = CARTESIAN_POINT ( 'NONE',  ( -153.9570736234661581, 9.058813317711329915, -2.943386871421373119 ) ) ;
#5713 = CARTESIAN_POINT ( 'NONE',  ( -33.71543202885159474, -9.630272336294959601, -3.117062350998871967 ) ) ;
#5715 = CARTESIAN_POINT ( 'NONE',  ( -163.1929263765338192, -10.01517768586948698, 6.132527647946031529E-16 ) ) ;
#5716 = MECHANICAL_DESIGN_GEOMETRIC_PRESENTATION_REPRESENTATION (  '', ( #49440 ), #32693 ) ;
#5717 = CARTESIAN_POINT ( 'NONE',  ( -176.6949999999999363, -8.437984349512085203, 5.166775262442717831E-16 ) ) ;
#5718 = ADVANCED_FACE ( 'NONE', ( #50243 ), #38686, .F. ) ;
#5719 = DIRECTION ( 'NONE',  ( -0.000000000000000000, -1.000000000000000000, 0.000000000000000000 ) ) ;
#5720 = DIRECTION ( 'NONE',  ( 0.000000000000000000, 0.000000000000000000, 1.000000000000000000 ) ) ;
#5721 = ORIENTED_EDGE ( 'NONE', *, *, #66820, .F. ) ;
#5722 = DIRECTION ( 'NONE',  ( 0.000000000000000000, 0.000000000000000000, -1.000000000000000000 ) ) ;
#5723 = ORIENTED_EDGE ( 'NONE', *, *, #36515, .T. ) ;
#5724 = VECTOR ( 'NONE', #60067, 1000.000000000000000 ) ;
#5725 = CARTESIAN_POINT ( 'NONE',  ( -73.79292637653378506, -3.094860106618429807, 9.524999999999991473 ) ) ;
#5726 = ITEM_DEFINED_TRANSFORMATION ( 'NONE', 'NONE', #12391,  #42840 ) ;
#5727 = CARTESIAN_POINT ( 'NONE',  ( 71.50000000000000000, 14.49137674618942562, 10.00000000000000000 ) ) ;
#5728 = DIRECTION ( 'NONE',  ( 0.000000000000000000, 0.000000000000000000, 1.000000000000000000 ) ) ;
#5729 = PRESENTATION_LAYER_ASSIGNMENT (  '', '', ( #7999 ) ) ;
#5730 = DIRECTION ( 'NONE',  ( 1.000000000000000000, 0.000000000000000000, -1.669238443041287922E-16 ) ) ;
#5731 = CARTESIAN_POINT ( 'NONE',  ( -195.0000000000000000, 0.000000000000000000, 0.000000000000000000 ) ) ;
#5732 = VECTOR ( 'NONE', #48870, 1000.000000000000000 ) ;
#5733 = CARTESIAN_POINT ( 'NONE',  ( -181.8549999999999898, 4.716976649647094177, 6.492361379858945902 ) ) ;
#5734 = EDGE_LOOP ( 'NONE', ( #31811, #12693, #52000, #2957 ) ) ;
#5735 = PRESENTATION_STYLE_ASSIGNMENT (( #37485 ) ) ;
#5736 = CYLINDRICAL_SURFACE ( 'NONE', #35435, 0.5000000000000004441 ) ;
#5737 = AXIS2_PLACEMENT_3D ( 'NONE', #62244, #45432, #14071 ) ;
#5738 = CARTESIAN_POINT ( 'NONE',  ( -75.05707362346616662, 0.000000000000000000, 9.524999999999991473 ) ) ;
#5739 = CARTESIAN_POINT ( 'NONE',  ( 72.49999999999998579, 1.797044900979284448E-15, -9.500000000000000000 ) ) ;
#5740 = STYLED_ITEM ( 'NONE', ( #61707 ), #34932 ) ;
#5741 = CARTESIAN_POINT ( 'NONE',  ( 39.74999999999999289, 16.24999999999997513, -4.000000000000000000 ) ) ;
#5742 = CARTESIAN_POINT ( 'NONE',  ( -4.716976649647097730, 142.3570736234661638, -6.492361379858953896 ) ) ;
#5743 = ORIENTED_EDGE ( 'NONE', *, *, #65281, .F. ) ;
#5744 = FILL_AREA_STYLE_COLOUR ( '', #39492 ) ;
#5745 = CARTESIAN_POINT ( 'NONE',  ( -93.20499999999998408, -2.607480562269071545, -8.024999999999991473 ) ) ;
#5746 = ORIENTED_EDGE ( 'NONE', *, *, #65191, .T. ) ;
#5747 = CARTESIAN_POINT ( 'NONE',  ( -92.45707362346617231, -9.058813317711329915, 2.943386871421371787 ) ) ;
#5748 = DIRECTION ( 'NONE',  ( -1.000000000000000000, -0.000000000000000000, -0.000000000000000000 ) ) ;
#5749 = FILL_AREA_STYLE_COLOUR ( '', #22741 ) ;
#5750 = ORIENTED_EDGE ( 'NONE', *, *, #50209, .T. ) ;
#5751 = FILL_AREA_STYLE_COLOUR ( '', #41850 ) ;
#5752 = CARTESIAN_POINT ( 'NONE',  ( -59.99499999999996902, -6.826472737025115478, 4.959722759717900331 ) ) ;
#5753 = VERTEX_POINT ( 'NONE', #12228 ) ;
#5754 = PRESENTATION_LAYER_ASSIGNMENT (  '', '', ( #15902 ) ) ;
#5755 = SURFACE_SIDE_STYLE ('',( #32172 ) ) ;
#5756 = LINE ( 'NONE', #59582, #8741 ) ;
#5757 = CARTESIAN_POINT ( 'NONE',  ( -44.99999999999977973, 146.4999999999999716, -7.500000000000000000 ) ) ;
#5758 = ORIENTED_EDGE ( 'NONE', *, *, #24437, .T. ) ;
#5759 = FILL_AREA_STYLE_COLOUR ( '', #42726 ) ;
#5760 = LINE ( 'NONE', #23017, #53893 ) ;
#5761 = ORIENTED_EDGE ( 'NONE', *, *, #50765, .T. ) ;
#5762 = MECHANICAL_DESIGN_GEOMETRIC_PRESENTATION_REPRESENTATION (  '', ( #47411 ), #50737 ) ;
#5763 = CARTESIAN_POINT ( 'NONE',  ( -108.4429263765338050, -1.166476076187852838E-15, -9.524999999999991473 ) ) ;
#5764 = CARTESIAN_POINT ( 'NONE',  ( 26.25000000000001066, 19.24999999999997868, -3.750000000000000000 ) ) ;
#5765 = CARTESIAN_POINT ( 'NONE',  ( -118.8549999999999898, 4.716976649647094177, 6.492361379858945902 ) ) ;
#5766 = ORIENTED_EDGE ( 'NONE', *, *, #41495, .T. ) ;
#5767 =( NAMED_UNIT ( * ) PLANE_ANGLE_UNIT ( ) SI_UNIT ( $, .RADIAN. ) );
#5768 = SURFACE_STYLE_FILL_AREA ( #53966 ) ;
#5769 = EDGE_CURVE ( 'NONE', #40899, #37680, #38922, .T. ) ;
#5770 = CARTESIAN_POINT ( 'NONE',  ( -71.75000000000000000, -4.000000000000000000, 18.00000000000000000 ) ) ;
#5771 = FACE_OUTER_BOUND ( 'NONE', #67341, .T. ) ;
#5772 = DIRECTION ( 'NONE',  ( 0.000000000000000000, 0.000000000000000000, 1.000000000000000000 ) ) ;
#5773 = CARTESIAN_POINT ( 'NONE',  ( -159.9570736234661865, 9.058813317711329915, -2.943386871421373119 ) ) ;
#5774 = AXIS2_PLACEMENT_3D ( 'NONE', #23642, #24334, #45511 ) ;
#5775 = CARTESIAN_POINT ( 'NONE',  ( -8.102448949553179958, 131.4950000000000045, 5.886773742842747126 ) ) ;
#5776 = ADVANCED_FACE ( 'NONE', ( #59742 ), #44991, .F. ) ;
#5777 = CARTESIAN_POINT ( 'NONE',  ( -98.60707362346616378, -8.102448949553172852, 5.886773742842742685 ) ) ;
#5778 = EDGE_CURVE ( 'NONE', #51323, #48755, #18555, .T. ) ;
#5779 = CIRCLE ( 'NONE', #68740, 0.5000000000000004441 ) ;
#5780 = SURFACE_STYLE_USAGE ( .BOTH. , #48073 ) ;
#5781 = EDGE_LOOP ( 'NONE', ( #12875, #53569, #45873, #69234 ) ) ;
#5782 = CYLINDRICAL_SURFACE ( 'NONE', #36350, 7.999999999999992895 ) ;
#5783 = EDGE_CURVE ( 'NONE', #10407, #9536, #13269, .T. ) ;
#5784 =( GEOMETRIC_REPRESENTATION_CONTEXT ( 3 ) GLOBAL_UNCERTAINTY_ASSIGNED_CONTEXT ( ( #44770 ) ) GLOBAL_UNIT_ASSIGNED_CONTEXT ( ( #20334, #21030, #31926 ) ) REPRESENTATION_CONTEXT ( 'NONE', 'WORKASPACE' ) );
#5785 = LINE ( 'NONE', #21636, #34349 ) ;
#5786 = CARTESIAN_POINT ( 'NONE',  ( -141.5049999999999955, -6.826472737025115478, -4.959722759717899443 ) ) ;
#5787 = ADVANCED_FACE ( 'NONE', ( #30842 ), #34723, .T. ) ;
#5788 = DIRECTION ( 'NONE',  ( -0.000000000000000000, -0.000000000000000000, -1.000000000000000000 ) ) ;
#5789 = CARTESIAN_POINT ( 'NONE',  ( -171.0570736234661808, 0.000000000000000000, 9.524999999999991473 ) ) ;
#5790 =( GEOMETRIC_REPRESENTATION_CONTEXT ( 3 ) GLOBAL_UNCERTAINTY_ASSIGNED_CONTEXT ( ( #58899 ) ) GLOBAL_UNIT_ASSIGNED_CONTEXT ( ( #3012, #67095, #40380 ) ) REPRESENTATION_CONTEXT ( 'NONE', 'WORKASPACE' ) );
#5791 = CARTESIAN_POINT ( 'NONE',  ( -142.3449999999999989, 7.632228543268599452, -2.479861379858951942 ) ) ;
#5792 = EDGE_CURVE ( 'NONE', #65139, #55052, #25226, .T. ) ;
#5793 = CARTESIAN_POINT ( 'NONE',  ( -136.1949999999999932, 8.437984349512086979, -1.550032578732815448E-15 ) ) ;
#5795 = EDGE_CURVE ( 'NONE', #62473, #21970, #19598, .T. ) ;
#5794 = TOROIDAL_SURFACE ( 'NONE', #33863, 9.499999999999996447, 0.5000000000000000000 ) ;
#5796 = ORIENTED_EDGE ( 'NONE', *, *, #1452, .F. ) ;
#5797 = AXIS2_PLACEMENT_3D ( 'NONE', #21085, #15839, #10199 ) ;
#5798 = CARTESIAN_POINT ( 'NONE',  ( 45.30708737912519979, 10.10236245970838453, -3.219298532130920432 ) ) ;
#5799 = SURFACE_SIDE_STYLE ('',( #61004 ) ) ;
#5800 = ADVANCED_FACE ( 'NONE', ( #35788 ), #68154, .F. ) ;
#5801 = UNCERTAINTY_MEASURE_WITH_UNIT (LENGTH_MEASURE( 1.000000000000000082E-05 ), #32473, 'distance_accuracy_value', 'NONE');
#5802 = CARTESIAN_POINT ( 'NONE',  ( -51.80499999999998550, -8.437984349512085203, 5.166775262442717831E-16 ) ) ;
#5803 = SURFACE_SIDE_STYLE ('',( #26568 ) ) ;
#5804 = CARTESIAN_POINT ( 'NONE',  ( -61.79499999999998039, 2.607480562269068880, -8.024999999999993250 ) ) ;
#5805 = VECTOR ( 'NONE', #39229, 1000.000000000000000 ) ;
#5806 = FACE_OUTER_BOUND ( 'NONE', #64115, .T. ) ;
#5807 = CARTESIAN_POINT ( 'NONE',  ( 24.00000000000000355, 36.75000000000000000, -3.000000000000000000 ) ) ;
#5808 = CIRCLE ( 'NONE', #28229, 0.2500000000000002220 ) ;
#5809 = DIRECTION ( 'NONE',  ( 1.000000000000000000, 1.156482317317866302E-16, 0.000000000000000000 ) ) ;
#5811 =( BOUNDED_CURVE ( )  B_SPLINE_CURVE ( 2, ( #13602, #56161, #67418, #18867, #40724, #51257, #19581, #45322, #62135, #8353, #2999 ),
 .UNSPECIFIED., .F., .F. ) 
 B_SPLINE_CURVE_WITH_KNOTS ( ( 3, 2, 2, 2, 2, 3 ),
 ( 0.1630434782608656819, 0.1652173913043438747, 0.1673913043478220952, 0.1695652173913003158, 0.1717391304347785363, 0.1739130434782567292 ),
 .UNSPECIFIED. ) 
 CURVE ( )  GEOMETRIC_REPRESENTATION_ITEM ( )  RATIONAL_B_SPLINE_CURVE ( ( 1.000000000000087486, 0.9510565162950660456, 1.000000000000000000, 0.9510565162951535312, 1.000000000000000000, 0.9510565162951535312, 1.000000000000000000, 0.9510565162951535312, 1.000000000000000000, 0.9510565162952466789, 0.9999999999999068523 ) ) 
 REPRESENTATION_ITEM ( '' )  );
#5810 = CARTESIAN_POINT ( 'NONE',  ( -103.3429263765338106, -9.058813317711329915, 2.943386871421371787 ) ) ;
#5812 = DIRECTION ( 'NONE',  ( -2.775557561562891043E-17, 0.9285714285714283811, 0.3711537444790455886 ) ) ;
#5813 = DIRECTION ( 'NONE',  ( 1.000000000000000000, 0.000000000000000000, 0.000000000000000000 ) ) ;
#5814 = VECTOR ( 'NONE', #68184, 1000.000000000000000 ) ;
#5815 = CARTESIAN_POINT ( 'NONE',  ( -88.55707362346616662, -1.166476076187852838E-15, -9.524999999999991473 ) ) ;
#5816 = FILL_AREA_STYLE ('',( #54014 ) ) ;
#5817 = CIRCLE ( 'NONE', #12549, 4.999999999999997335 ) ;
#5818 = DIRECTION ( 'NONE',  ( -1.000000000000000000, 0.000000000000000000, -0.000000000000000000 ) ) ;
#5819 = VERTEX_POINT ( 'NONE', #51274 ) ;
#5820 =( LENGTH_UNIT ( ) NAMED_UNIT ( * ) SI_UNIT ( .MILLI., .METRE. ) );
#5821 = DIRECTION ( 'NONE',  ( 1.000000000000000000, 0.000000000000000000, 0.000000000000000000 ) ) ;
#5822 = ORIENTED_EDGE ( 'NONE', *, *, #21152, .F. ) ;
#5823 = AXIS2_PLACEMENT_3D ( 'NONE', #15135, #36932, #67521 ) ;
#5824 = CARTESIAN_POINT ( 'NONE',  ( -6.826472737025120807, 109.5070736234661695, -4.959722759717907437 ) ) ;
#5825 = STYLED_ITEM ( 'NONE', ( #40161 ), #46256 ) ;
#5826 = VECTOR ( 'NONE', #60830, 1000.000000000000000 ) ;
#5827 = CARTESIAN_POINT ( 'NONE',  ( 2.755511676787088415, -7.000000000000004441, 0.5168645644872222888 ) ) ;
#5828 = CARTESIAN_POINT ( 'NONE',  ( 74.65399860055316594, 19.87094859200031394, -6.130873952096200341 ) ) ;
#5829 = AXIS2_PLACEMENT_3D ( 'NONE', #29090, #35459, #50585 ) ;
#5830 = FILL_AREA_STYLE ('',( #15730 ) ) ;
#5831 = ORIENTED_EDGE ( 'NONE', *, *, #32300, .T. ) ;
#5832 = ORIENTED_EDGE ( 'NONE', *, *, #21264, .F. ) ;
#5833 = CYLINDRICAL_SURFACE ( 'NONE', #30935, 0.2500000000000002220 ) ;
#5834 = FACE_OUTER_BOUND ( 'NONE', #15264, .T. ) ;
#5835 = ORIENTED_EDGE ( 'NONE', *, *, #61863, .T. ) ;
#5836 = CARTESIAN_POINT ( 'NONE',  ( 9.058813317711338797, 124.9549999999999841, -2.943386871421372675 ) ) ;
#5837 = DIRECTION ( 'NONE',  ( -0.000000000000000000, -0.000000000000000000, 1.000000000000000000 ) ) ;
#5838 = CARTESIAN_POINT ( 'NONE',  ( -195.0000000000000000, 1.166476076187852838E-15, -9.524999999999991473 ) ) ;
#5839 = COLOUR_RGB ( '', 0.66274510, 0.83137255, 0.94901961) ;
#5840 = STYLED_ITEM ( 'NONE', ( #24033 ), #35779 ) ;
#5841 = DIRECTION ( 'NONE',  ( -0.000000000000000000, 1.000000000000000000, -0.000000000000000000 ) ) ;
#5842 = CARTESIAN_POINT ( 'NONE',  ( -92.24499999999999034, -4.716976649647093289, -6.492361379858945902 ) ) ;
#5843 = ORIENTED_EDGE ( 'NONE', *, *, #29873, .T. ) ;
#5844 = DIRECTION ( 'NONE',  ( 0.000000000000000000, 0.000000000000000000, 1.000000000000000000 ) ) ;
#5845 = FACE_OUTER_BOUND ( 'NONE', #11804, .T. ) ;
#5846 = EDGE_LOOP ( 'NONE', ( #62894, #14954, #68417, #1778 ) ) ;
#5847 = CARTESIAN_POINT ( 'NONE',  ( -174.7429263765338305, -5.598654528085803328, -7.705886871421366635 ) ) ;
#5848 = SURFACE_STYLE_FILL_AREA ( #32957 ) ;
#5849 = CARTESIAN_POINT ( 'NONE',  ( 7.441974819423175624, -1.110121504110839430, 0.4967607073414704866 ) ) ;
#5850 =( GEOMETRIC_REPRESENTATION_CONTEXT ( 3 ) GLOBAL_UNCERTAINTY_ASSIGNED_CONTEXT ( ( #51124 ) ) GLOBAL_UNIT_ASSIGNED_CONTEXT ( ( #47660, #58495, #53234 ) ) REPRESENTATION_CONTEXT ( 'NONE', 'WORKASPACE' ) );
#5851 =( LENGTH_UNIT ( ) NAMED_UNIT ( * ) SI_UNIT ( .MILLI., .METRE. ) );
#5852 = ADVANCED_FACE ( 'NONE', ( #29456 ), #36159, .T. ) ;
#5853 = VERTEX_POINT ( 'NONE', #4807 ) ;
#5854 = CIRCLE ( 'NONE', #4715, 0.5000000000000004441 ) ;
#5855 = DIRECTION ( 'NONE',  ( 0.8660254037844385966, -0.5000000000000001110, 0.000000000000000000 ) ) ;
#5856 = VERTEX_POINT ( 'NONE', #47793 ) ;
#5857 = CARTESIAN_POINT ( 'NONE',  ( 27.99999999999999645, 5.000000000000000000, -24.00402776293821816 ) ) ;
#5858 = DIRECTION ( 'NONE',  ( 1.000000000000000000, 0.000000000000000000, 0.000000000000000000 ) ) ;
#5859 = DIRECTION ( 'NONE',  ( -0.000000000000000000, -1.000000000000000000, -0.000000000000000000 ) ) ;
#5860 = FILL_AREA_STYLE ('',( #16808 ) ) ;
#5861 = CARTESIAN_POINT ( 'NONE',  ( -126.4429263765338192, -1.166476076187852838E-15, -9.524999999999991473 ) ) ;
#5862 = ADVANCED_FACE ( 'NONE', ( #5471 ), #36863, .F. ) ;
#5863 = PRESENTATION_LAYER_ASSIGNMENT (  '', '', ( #17118 ) ) ;
#5864 = CARTESIAN_POINT ( 'NONE',  ( -0.9113929259990888321, 9.000000000000008882, 0.04319542563019723030 ) ) ;
#5865 = DIRECTION ( 'NONE',  ( 0.000000000000000000, -1.000000000000000000, 0.000000000000000000 ) ) ;
#5866 = CARTESIAN_POINT ( 'NONE',  ( -8.003604573459423221, 153.4245184585901427, -2.762566347670349476 ) ) ;
#5867 = ORIENTED_EDGE ( 'NONE', *, *, #49039, .F. ) ;
#5868 = CARTESIAN_POINT ( 'NONE',  ( -162.4429263765338192, -1.166476076187852838E-15, -9.524999999999991473 ) ) ;
#5869 = DIRECTION ( 'NONE',  ( 0.000000000000000000, 0.000000000000000000, -1.000000000000000000 ) ) ;
#5870 = DIRECTION ( 'NONE',  ( 0.000000000000000000, 1.000000000000000000, 0.000000000000000000 ) ) ;
#5871 =( NAMED_UNIT ( * ) PLANE_ANGLE_UNIT ( ) SI_UNIT ( $, .RADIAN. ) );
#5872 = ORIENTED_EDGE ( 'NONE', *, *, #64729, .T. ) ;
#5873 =( LENGTH_UNIT ( ) NAMED_UNIT ( * ) SI_UNIT ( .MILLI., .METRE. ) );
#5874 = CARTESIAN_POINT ( 'NONE',  ( -172.5549999999999784, 0.000000000000000000, 8.024999999999991473 ) ) ;
#5875 = CARTESIAN_POINT ( 'NONE',  ( 7.750000000000000000, 33.74999999999998579, 3.750000000000000000 ) ) ;
#5876 = CARTESIAN_POINT ( 'NONE',  ( 0.000000000000000000, 0.000000000000000000, 0.000000000000000000 ) ) ;
#5877 = CARTESIAN_POINT ( 'NONE',  ( -172.7950000000000159, 2.607480562269068880, -8.024999999999993250 ) ) ;
#5878 = ADVANCED_FACE ( 'NONE', ( #37916 ), #62330, .T. ) ;
#5879 = CIRCLE ( 'NONE', #45249, 4.999999999999997335 ) ;
#5880 =( GEOMETRIC_REPRESENTATION_CONTEXT ( 3 ) GLOBAL_UNCERTAINTY_ASSIGNED_CONTEXT ( ( #41859 ) ) GLOBAL_UNIT_ASSIGNED_CONTEXT ( ( #13610, #44303, #61111 ) ) REPRESENTATION_CONTEXT ( 'NONE', 'WORKASPACE' ) );
#5881 = CARTESIAN_POINT ( 'NONE',  ( -170.2450000000000045, -4.716976649647093289, -6.492361379858945902 ) ) ;
#5882 = ORIENTED_EDGE ( 'NONE', *, *, #2484, .T. ) ;
#5883 = DIRECTION ( 'NONE',  ( 0.000000000000000000, -1.000000000000000000, 0.000000000000000000 ) ) ;
#5884 = COLOUR_RGB ( '', 0.09019608, 0.27058824, 0.51372549) ;
#5885 = DIRECTION ( 'NONE',  ( -0.000000000000000000, -0.000000000000000000, -1.000000000000000000 ) ) ;
#5886 = EDGE_CURVE ( 'NONE', #51660, #32231, #46670, .T. ) ;
#5887 = FILL_AREA_STYLE_COLOUR ( '', #56307 ) ;
#5888 = CARTESIAN_POINT ( 'NONE',  ( -87.20499999999999829, -2.607480562269071545, -8.024999999999991473 ) ) ;
#5889 = DIRECTION ( 'NONE',  ( -1.000000000000000000, 0.000000000000000000, 0.000000000000000000 ) ) ;
#5890 = AXIS2_PLACEMENT_3D ( 'NONE', #13200, #7933, #29375 ) ;
#5891 =( NAMED_UNIT ( * ) SI_UNIT ( $, .STERADIAN. ) SOLID_ANGLE_UNIT ( ) );
#5892 = CARTESIAN_POINT ( 'NONE',  ( -78.59499999999998465, 2.607480562269072433, 8.024999999999991473 ) ) ;
#5893 = CARTESIAN_POINT ( 'NONE',  ( -9.058813317711338797, 135.4549999999999841, 2.943386871421373563 ) ) ;
#5894 = CARTESIAN_POINT ( 'NONE',  ( -134.9070736234667720, -3.094860106608412931, 9.525000000007270984 ) ) ;
#5895 =( GEOMETRIC_REPRESENTATION_CONTEXT ( 3 ) GLOBAL_UNCERTAINTY_ASSIGNED_CONTEXT ( ( #34841 ) ) GLOBAL_UNIT_ASSIGNED_CONTEXT ( ( #5003, #37064, #10641 ) ) REPRESENTATION_CONTEXT ( 'NONE', 'WORKASPACE' ) );
#5896 = CARTESIAN_POINT ( 'NONE',  ( -176.9929263765337737, 8.102448949553172852, -5.886773742842744461 ) ) ;
#5897 = UNCERTAINTY_MEASURE_WITH_UNIT (LENGTH_MEASURE( 1.000000000000000082E-05 ), #23210, 'distance_accuracy_value', 'NONE');
#5898 = DIRECTION ( 'NONE',  ( 0.000000000000000000, 0.000000000000000000, 1.000000000000000000 ) ) ;
#5899 =( NAMED_UNIT ( * ) PLANE_ANGLE_UNIT ( ) SI_UNIT ( $, .RADIAN. ) );
#5900 = ORIENTED_EDGE ( 'NONE', *, *, #58358, .T. ) ;
#5901 = CARTESIAN_POINT ( 'NONE',  ( 27.00000000000001776, 15.00000000000000000, -34.49999999999999289 ) ) ;
#5902 = CIRCLE ( 'NONE', #14939, 22.49999999999999645 ) ;
#5903 = PRESENTATION_LAYER_ASSIGNMENT (  '', '', ( #64375 ) ) ;
#5904 = DIRECTION ( 'NONE',  ( 0.000000000000000000, 0.000000000000000000, 1.000000000000000000 ) ) ;
#5905 = CIRCLE ( 'NONE', #4767, 1.000000000000000888 ) ;
#5906 =( NAMED_UNIT ( * ) SI_UNIT ( $, .STERADIAN. ) SOLID_ANGLE_UNIT ( ) );
#5907 = CARTESIAN_POINT ( 'NONE',  ( 24.21231517720798010, 117.4999999999999716, 7.000000000000000000 ) ) ;
#5908 = EDGE_LOOP ( 'NONE', ( #57302, #33687, #65213, #35487 ) ) ;
#5909 = EDGE_LOOP ( 'NONE', ( #66501, #67560, #27451, #36624 ) ) ;
#5910 =( BOUNDED_CURVE ( )  B_SPLINE_CURVE ( 2, ( #58259, #57935, #31159, #42142, #4414, #25889, #20631, #10083, #31511, #50484, #12134 ),
 .UNSPECIFIED., .F., .F. ) 
 B_SPLINE_CURVE_WITH_KNOTS ( ( 3, 2, 2, 2, 2, 3 ),
 ( 0.7282608695652174058, 0.7304347826086956541, 0.7326086956521739024, 0.7347826086956521507, 0.7369565217391303991, 0.7391304347826086474 ),
 .UNSPECIFIED. ) 
 CURVE ( )  GEOMETRIC_REPRESENTATION_ITEM ( )  RATIONAL_B_SPLINE_CURVE ( ( 1.000000000000000000, 0.9510565162951535312, 1.000000000000000000, 0.9510565162951535312, 1.000000000000000000, 0.9510565162951535312, 1.000000000000000000, 0.9510565162951535312, 1.000000000000000000, 0.9510565162951535312, 1.000000000000000000 ) ) 
 REPRESENTATION_ITEM ( '' )  );
#5911 = EDGE_CURVE ( 'NONE', #21950, #23421, #25556, .T. ) ;
#5912 = CIRCLE ( 'NONE', #231, 1.000000000000000888 ) ;
#5913 = ADVANCED_FACE ( 'NONE', ( #63215 ), #11117, .T. ) ;
#5914 = STYLED_ITEM ( 'NONE', ( #34177 ), #24846 ) ;
#5915 = CARTESIAN_POINT ( 'NONE',  ( -14.98999599679678951, 118.4999999999999716, -10.00000000000000000 ) ) ;
#5916 = ORIENTED_EDGE ( 'NONE', *, *, #55276, .F. ) ;
#5917 = CARTESIAN_POINT ( 'NONE',  ( -114.3549999999999898, -4.716976649647093289, -6.492361379858945902 ) ) ;
#5918 = ORIENTED_EDGE ( 'NONE', *, *, #45922, .T. ) ;
#5919 = SURFACE_STYLE_FILL_AREA ( #15825 ) ;
#5920 = ORIENTED_EDGE ( 'NONE', *, *, #40204, .T. ) ;
#5921 = DIRECTION ( 'NONE',  ( 0.000000000000000000, 0.000000000000000000, -1.000000000000000000 ) ) ;
#5922 = CARTESIAN_POINT ( 'NONE',  ( -68.15707362346616094, -9.058813317711329915, -2.943386871421370898 ) ) ;
#5923 = ORIENTED_EDGE ( 'NONE', *, *, #39512, .T. ) ;
#5924 = MECHANICAL_DESIGN_GEOMETRIC_PRESENTATION_REPRESENTATION (  '', ( #39663 ), #13830 ) ;
#5925 = MECHANICAL_DESIGN_GEOMETRIC_PRESENTATION_REPRESENTATION (  '', ( #55346 ), #26124 ) ;
#5926 = FACE_OUTER_BOUND ( 'NONE', #66123, .T. ) ;
#5927 = PRESENTATION_STYLE_ASSIGNMENT (( #12234 ) ) ;
#5928 = SURFACE_STYLE_USAGE ( .BOTH. , #22126 ) ;
#5929 = ORIENTED_EDGE ( 'NONE', *, *, #61667, .F. ) ;
#5930 = ORIENTED_EDGE ( 'NONE', *, *, #21765, .T. ) ;
#5931 = CIRCLE ( 'NONE', #50893, 10.00000000000000000 ) ;
#5932 = CARTESIAN_POINT ( 'NONE',  ( -195.0000000000000000, 0.000000000000000000, 9.524999999999991473 ) ) ;
#5933 = SURFACE_STYLE_FILL_AREA ( #59065 ) ;
#5934 = CARTESIAN_POINT ( 'NONE',  ( -13.37557077883746004, -11.02493375743656223, 4.740230301942971458 ) ) ;
#5935 = DIRECTION ( 'NONE',  ( 1.000000000000000000, 0.000000000000000000, 0.000000000000000000 ) ) ;
#5936 = ORIENTED_EDGE ( 'NONE', *, *, #26378, .T. ) ;
#5937 = CARTESIAN_POINT ( 'NONE',  ( -9.827790563157511022E-16, 133.4429263765338192, 8.025000000000000355 ) ) ;
#5938 = CARTESIAN_POINT ( 'NONE',  ( 45.07697505292422591, 10.02565835097472480, -3.091949714863345910 ) ) ;
#5939 = ADVANCED_FACE ( 'NONE', ( #52668 ), #58629, .F. ) ;
#5940 = FILL_AREA_STYLE_COLOUR ( '', #23869 ) ;
#5941 = SURFACE_STYLE_FILL_AREA ( #21094 ) ;
#5942 = ADVANCED_FACE ( 'NONE', ( #26593 ), #41796, .T. ) ;
#5943 = ORIENTED_EDGE ( 'NONE', *, *, #12857, .F. ) ;
#5944 = TOROIDAL_SURFACE ( 'NONE', #63257, 0.5000000000000000000, 0.2500000000000000000 ) ;
#5945 = PRESENTATION_STYLE_ASSIGNMENT (( #6622 ) ) ;
#5946 = EDGE_LOOP ( 'NONE', ( #16127, #10788 ) ) ;
#5947 = CARTESIAN_POINT ( 'NONE',  ( -50.69292637653379785, 10.01517768586948698, -1.839758294383808571E-15 ) ) ;
#5948 = CARTESIAN_POINT ( 'NONE',  ( -12.72792206135785698, 115.4999999999999574, 10.00000000000000000 ) ) ;
#5949 = DIRECTION ( 'NONE',  ( -0.000000000000000000, -0.000000000000000000, -1.000000000000000000 ) ) ;
#5950 = CARTESIAN_POINT ( 'NONE',  ( -145.8549999999999898, 4.716976649647094177, 6.492361379858945902 ) ) ;
#5951 = CIRCLE ( 'NONE', #20573, 0.2500000000000002220 ) ;
#5952 = DIRECTION ( 'NONE',  ( -0.000000000000000000, 1.000000000000000000, -0.000000000000000000 ) ) ;
#5953 = DIRECTION ( 'NONE',  ( 1.000000000000000000, 0.000000000000000000, 0.000000000000000000 ) ) ;
#5954 = UNCERTAINTY_MEASURE_WITH_UNIT (LENGTH_MEASURE( 1.000000000000000082E-05 ), #24085, 'distance_accuracy_value', 'NONE');
#5955 = VECTOR ( 'NONE', #47548, 1000.000000000000000 ) ;
#5956 = EDGE_CURVE ( 'NONE', #15190, #68534, #56717, .T. ) ;
#5957 = CARTESIAN_POINT ( 'NONE',  ( -105.4429263765338050, -1.166476076187852838E-15, -9.524999999999991473 ) ) ;
#5958 = AXIS2_PLACEMENT_3D ( 'NONE', #19329, #50323, #2775 ) ;
#5959 = ORIENTED_EDGE ( 'NONE', *, *, #66146, .F. ) ;
#5961 = EDGE_CURVE ( 'NONE', #28720, #39204, #2736, .T. ) ;
#5960 = ORIENTED_EDGE ( 'NONE', *, *, #36909, .T. ) ;
#5962 = CARTESIAN_POINT ( 'NONE',  ( 8.250000000000001776, 31.24999999999998579, -4.000000000000000000 ) ) ;
#5963 = MECHANICAL_DESIGN_GEOMETRIC_PRESENTATION_REPRESENTATION (  '', ( #44229 ), #26194 ) ;
#5964 = SURFACE_STYLE_FILL_AREA ( #36657 ) ;
#5965 = STYLED_ITEM ( 'NONE', ( #39439 ), #29512 ) ;
#5966 = CARTESIAN_POINT ( 'NONE',  ( -53.60499999999998977, 6.826472737025113702, -4.959722759717902107 ) ) ;
#5967 = VERTEX_POINT ( 'NONE', #50086 ) ;
#5968 = SURFACE_STYLE_USAGE ( .BOTH. , #44005 ) ;
#5969 = DIRECTION ( 'NONE',  ( -0.000000000000000000, -1.000000000000000000, -0.000000000000000000 ) ) ;
#5970 = COLOUR_RGB ( '', 0.40784314, 0.44705882, 0.49803922) ;
#5971 = ADVANCED_BREP_SHAPE_REPRESENTATION ( '', ( #3348, #42840 ), #43934 ) ;
#5972 = EDGE_CURVE ( 'NONE', #5413, #57180, #50767, .T. ) ;
#5973 = CARTESIAN_POINT ( 'NONE',  ( 12.25000000000000533, 28.24999999999998224, 4.000000000000000000 ) ) ;
#5974 = CARTESIAN_POINT ( 'NONE',  ( 23.50000000000041211, 24.55989583709592949, -27.18999999999997286 ) ) ;
#5975 = ORIENTED_EDGE ( 'NONE', *, *, #39998, .F. ) ;
#5976 = VECTOR ( 'NONE', #39069, 1000.000000000000000 ) ;
#5977 = DIRECTION ( 'NONE',  ( 0.000000000000000000, 1.000000000000000000, 1.734723475976805615E-16 ) ) ;
#5978 = EDGE_CURVE ( 'NONE', #46369, #33026, #11767, .T. ) ;
#5979 = DIRECTION ( 'NONE',  ( -0.7071067811865487940, 0.000000000000000000, 0.7071067811865463515 ) ) ;
#5980 = DIRECTION ( 'NONE',  ( -1.000000000000000000, 0.000000000000000000, 0.000000000000000000 ) ) ;
#5981 = FACE_OUTER_BOUND ( 'NONE', #29803, .T. ) ;
#5982 = CARTESIAN_POINT ( 'NONE',  ( -107.9949999999999761, -6.826472737025113702, 4.959722759717902107 ) ) ;
#5983 = CARTESIAN_POINT ( 'NONE',  ( 8.102448949553183510, 113.1049999999999898, -5.886773742842746238 ) ) ;
#5984 = CARTESIAN_POINT ( 'NONE',  ( -83.24499999999999034, -4.716976649647093289, -6.492361379858945902 ) ) ;
#5985 = CIRCLE ( 'NONE', #23968, 8.499999999999992895 ) ;
#5986 = AXIS2_PLACEMENT_3D ( 'NONE', #53935, #10697, #48721 ) ;
#5987 = DIRECTION ( 'NONE',  ( -1.000000000000000000, 0.000000000000000000, 0.000000000000000000 ) ) ;
#5988 = CARTESIAN_POINT ( 'NONE',  ( -166.8570736234661922, -5.598654528085803328, -7.705886871421366635 ) ) ;
#5989 = UNCERTAINTY_MEASURE_WITH_UNIT (LENGTH_MEASURE( 1.000000000000000082E-05 ), #54474, 'distance_accuracy_value', 'NONE');
#5991 = LINE ( 'NONE', #21841, #24689 ) ;
#5990 = APPLICATION_CONTEXT ( 'automotive_design' ) ;
#5992 = AXIS2_PLACEMENT_3D ( 'NONE', #46941, #18763, #3581 ) ;
#5993 = ORIENTED_EDGE ( 'NONE', *, *, #12746, .T. ) ;
#5994 = CARTESIAN_POINT ( 'NONE',  ( -126.7429263765338163, -5.598654528085803328, -7.705886871421366635 ) ) ;
#5995 = CARTESIAN_POINT ( 'NONE',  ( -147.2949999999999591, -2.607480562269069768, 8.024999999999991473 ) ) ;
#5996 = CARTESIAN_POINT ( 'NONE',  ( -1.744870598150812802, 7.000000000000005329, 0.2069669095365387901 ) ) ;
#5997 = CIRCLE ( 'NONE', #47653, 0.2500000000000002220 ) ;
#5998 = CARTESIAN_POINT ( 'NONE',  ( -66.65707362346616094, 9.058813317711329915, 2.943386871421369566 ) ) ;
#5999 = LINE ( 'NONE', #27438, #55239 ) ;
#6000 = ORIENTED_EDGE ( 'NONE', *, *, #62333, .T. ) ;
#6001 = ORIENTED_EDGE ( 'NONE', *, *, #33839, .F. ) ;
#6002 =( GEOMETRIC_REPRESENTATION_CONTEXT ( 3 ) GLOBAL_UNCERTAINTY_ASSIGNED_CONTEXT ( ( #29918 ) ) GLOBAL_UNIT_ASSIGNED_CONTEXT ( ( #25578, #20316, #69219 ) ) REPRESENTATION_CONTEXT ( 'NONE', 'WORKASPACE' ) );
#6003 = LINE ( 'NONE', #38059, #26910 ) ;
#6004 = SURFACE_STYLE_USAGE ( .BOTH. , #17956 ) ;
#6005 = VECTOR ( 'NONE', #58297, 1000.000000000000000 ) ;
#6006 = EDGE_CURVE ( 'NONE', #41477, #65971, #64598, .T. ) ;
#6007 = COLOUR_RGB ( '', 0.31764706, 0.68627451, 0.89019608) ;
#6008 = PRESENTATION_STYLE_ASSIGNMENT (( #23831 ) ) ;
#6009 = LINE ( 'NONE', #59825, #41755 ) ;
#6010 = CARTESIAN_POINT ( 'NONE',  ( -59.84292637653379643, 9.058813317711329915, -2.943386871421373119 ) ) ;
#6011 = CARTESIAN_POINT ( 'NONE',  ( -49.70707362346615810, -3.094860106618431139, -9.524999999999991473 ) ) ;
#6012 = AXIS2_PLACEMENT_3D ( 'NONE', #43625, #37321, #16541 ) ;
#6013 = CARTESIAN_POINT ( 'NONE',  ( 60.00000000000000000, 1.797044900979284448E-15, 6.500000000000000000 ) ) ;
#6014 = ORIENTED_EDGE ( 'NONE', *, *, #25812, .T. ) ;
#6015 = CARTESIAN_POINT ( 'NONE',  ( -137.0049999999999670, 6.826472737025115478, 4.959722759717899443 ) ) ;
#6016 = ORIENTED_EDGE ( 'NONE', *, *, #60829, .T. ) ;
#6017 = AXIS2_PLACEMENT_3D ( 'NONE', #4078, #24851, #46366 ) ;
#6018 = ORIENTED_EDGE ( 'NONE', *, *, #37709, .F. ) ;
#6019 = FACE_OUTER_BOUND ( 'NONE', #56263, .T. ) ;
#6020 = DIRECTION ( 'NONE',  ( 0.000000000000000000, 0.000000000000000000, -1.000000000000000000 ) ) ;
#6021 = ORIENTED_EDGE ( 'NONE', *, *, #12022, .T. ) ;
#6022 = VECTOR ( 'NONE', #22920, 1000.000000000000000 ) ;
#6023 =( NAMED_UNIT ( * ) SI_UNIT ( $, .STERADIAN. ) SOLID_ANGLE_UNIT ( ) );
#6024 = FACE_BOUND ( 'NONE', #62864, .T. ) ;
#6025 = CARTESIAN_POINT ( 'NONE',  ( 5.598654528085805993, 135.2450000000000045, 7.705886871421374629 ) ) ;
#6026 = ORIENTED_EDGE ( 'NONE', *, *, #54064, .T. ) ;
#6027 = PRESENTATION_LAYER_ASSIGNMENT (  '', '', ( #25114 ) ) ;
#6028 = ADVANCED_FACE ( 'NONE', ( #64928 ), #28928, .T. ) ;
#6029 = DIRECTION ( 'NONE',  ( -0.000000000000000000, -0.000000000000000000, -1.000000000000000000 ) ) ;
#6030 = CARTESIAN_POINT ( 'NONE',  ( 9.058813317711338797, 133.9549999999999841, -2.943386871421372675 ) ) ;
#6031 = CARTESIAN_POINT ( 'NONE',  ( -51.20499999999996277, -2.607480562269071545, -8.024999999999991473 ) ) ;
#6032 = CARTESIAN_POINT ( 'NONE',  ( -116.2449999999999903, -4.716976649647093289, -6.492361379858945902 ) ) ;
#6033 = DIRECTION ( 'NONE',  ( 1.000000000000000000, -0.000000000000000000, 0.000000000000000000 ) ) ;
#6034 = ORIENTED_EDGE ( 'NONE', *, *, #46279, .F. ) ;
#6035 = CARTESIAN_POINT ( 'NONE',  ( 8.102448949553181734, 145.5049999999999670, 5.886773742842750679 ) ) ;
#6036 = DIRECTION ( 'NONE',  ( 0.000000000000000000, -1.000000000000000000, 1.350863103983176297E-16 ) ) ;
#6037 = UNCERTAINTY_MEASURE_WITH_UNIT (LENGTH_MEASURE( 1.000000000000000082E-05 ), #21068, 'distance_accuracy_value', 'NONE');
#6038 = SURFACE_SIDE_STYLE ('',( #65475 ) ) ;
#6039 = EDGE_CURVE ( 'NONE', #1147, #12752, #38253, .T. ) ;
#6040 =( LENGTH_UNIT ( ) NAMED_UNIT ( * ) SI_UNIT ( .MILLI., .METRE. ) );
#6041 = DIRECTION ( 'NONE',  ( 0.000000000000000000, -1.000000000000000000, 0.000000000000000000 ) ) ;
#6042 = EDGE_CURVE ( 'NONE', #27715, #37052, #65613, .T. ) ;
#6043 = ORIENTED_EDGE ( 'NONE', *, *, #7814, .F. ) ;
#6044 = AXIS2_PLACEMENT_3D ( 'NONE', #2045, #45435, #7414 ) ;
#6045 = LINE ( 'NONE', #38460, #1857 ) ;
#6046 = CARTESIAN_POINT ( 'NONE',  ( -173.4549999999999841, 7.632228543268599452, -2.479861379858951942 ) ) ;
#6047 = ORIENTED_EDGE ( 'NONE', *, *, #15552, .T. ) ;
#6048 = FACE_OUTER_BOUND ( 'NONE', #14622, .T. ) ;
#6049 = UNCERTAINTY_MEASURE_WITH_UNIT (LENGTH_MEASURE( 1.000000000000000082E-05 ), #38544, 'distance_accuracy_value', 'NONE');
#6050 = PRESENTATION_LAYER_ASSIGNMENT (  '', '', ( #42058 ) ) ;
#6051 = EDGE_CURVE ( 'NONE', #47531, #58312, #69080, .T. ) ;
#6052 = FACE_OUTER_BOUND ( 'NONE', #57377, .T. ) ;
#6053 = CARTESIAN_POINT ( 'NONE',  ( 10.39230484541326582, -1.107695154586738839, 1.440973567693753677E-18 ) ) ;
#6054 = CARTESIAN_POINT ( 'NONE',  ( -77.24292637653380211, 5.598654528085804216, 7.705886871421366635 ) ) ;
#6055 = VERTEX_POINT ( 'NONE', #29286 ) ;
#6056 = EDGE_CURVE ( 'NONE', #24031, #5051, #47783, .T. ) ;
#6057 = CARTESIAN_POINT ( 'NONE',  ( -45.20191651604595506, 8.361204532447573001, -3.290978531522150696 ) ) ;
#6058 = CARTESIAN_POINT ( 'NONE',  ( -88.70499999999998408, 2.607480562269073321, 8.024999999999991473 ) ) ;
#6060 = ORIENTED_EDGE ( 'NONE', *, *, #13815, .F. ) ;
#6059 = CIRCLE ( 'NONE', #64463, 13.99999999999999822 ) ;
#6061 = CARTESIAN_POINT ( 'NONE',  ( -9.827790563157511022E-16, 112.4429263765338192, 8.025000000000000355 ) ) ;
#6062 = AXIS2_PLACEMENT_3D ( 'NONE', #56845, #57533, #58226 ) ;
#6063 = CARTESIAN_POINT ( 'NONE',  ( -60.80707362346617373, 10.01517768586948698, -1.839758294383808571E-15 ) ) ;
#6064 = STYLED_ITEM ( 'NONE', ( #64182 ), #55997 ) ;
#6065 = DIRECTION ( 'NONE',  ( 0.000000000000000000, 0.000000000000000000, 1.000000000000000000 ) ) ;
#6066 = VERTEX_POINT ( 'NONE', #509 ) ;
#6067 = CARTESIAN_POINT ( 'NONE',  ( 24.21231517720798010, 112.4999999999999858, 9.500000000000000000 ) ) ;
#6069 = CARTESIAN_POINT ( 'NONE',  ( 26.25000000000001066, 18.74999999999997868, 4.000000000000000000 ) ) ;
#6068 = CARTESIAN_POINT ( 'NONE',  ( 31.00000000000002132, 42.00000000000000000, 75.00000000000000000 ) ) ;
#6070 = AXIS2_PLACEMENT_3D ( 'NONE', #34908, #46199, #2498 ) ;
#6071 = CARTESIAN_POINT ( 'NONE',  ( -101.4549999999999841, 7.632228543268599452, -2.479861379858951942 ) ) ;
#6072 = ADVANCED_FACE ( 'NONE', ( #44827 ), #53187, .T. ) ;
#6073 = CARTESIAN_POINT ( 'NONE',  ( 8.102448949553183510, 126.9950000000000045, -5.886773742842746238 ) ) ;
#6074 = CARTESIAN_POINT ( 'NONE',  ( -114.4449999999999932, 0.000000000000000000, 8.024999999999991473 ) ) ;
#6075 = AXIS2_PLACEMENT_3D ( 'NONE', #61912, #56286, #23254 ) ;
#6076 = EDGE_CURVE ( 'NONE', #4894, #12034, #13457, .T. ) ;
#6077 = MECHANICAL_DESIGN_GEOMETRIC_PRESENTATION_REPRESENTATION (  '', ( #15109 ), #2665 ) ;
#6079 = PRESENTATION_STYLE_ASSIGNMENT (( #11007 ) ) ;
#6078 =( NAMED_UNIT ( * ) PLANE_ANGLE_UNIT ( ) SI_UNIT ( $, .RADIAN. ) );
#6080 = CIRCLE ( 'NONE', #66742, 3.000000000000000444 ) ;
#6081 = CARTESIAN_POINT ( 'NONE',  ( -155.0929263765337964, 3.094860106618433360, 9.524999999999991473 ) ) ;
#6082 = CARTESIAN_POINT ( 'NONE',  ( -178.0450000000000159, 7.632228543268600340, 2.479861379858949277 ) ) ;
#6083 = AXIS2_PLACEMENT_3D ( 'NONE', #28539, #39853, #12361 ) ;
#6084 = FILL_AREA_STYLE_COLOUR ( '', #15298 ) ;
#6085 = AXIS2_PLACEMENT_3D ( 'NONE', #43865, #22030, #65965 ) ;
#6087 = CARTESIAN_POINT ( 'NONE',  ( -44.40807425668157293, -12.16242975799924864, 3.182228584415367489 ) ) ;
#6086 =( GEOMETRIC_REPRESENTATION_CONTEXT ( 3 ) GLOBAL_UNCERTAINTY_ASSIGNED_CONTEXT ( ( #58019 ) ) GLOBAL_UNIT_ASSIGNED_CONTEXT ( ( #44649, #23834, #61789 ) ) REPRESENTATION_CONTEXT ( 'NONE', 'WORKASPACE' ) );
#6088 = ORIENTED_EDGE ( 'NONE', *, *, #66135, .T. ) ;
#6089 = FILL_AREA_STYLE ('',( #63101 ) ) ;
#6090 = CARTESIAN_POINT ( 'NONE',  ( 0.000000000000000000, 0.000000000000000000, 0.000000000000000000 ) ) ;
#6091 = ORIENTED_EDGE ( 'NONE', *, *, #62437, .T. ) ;
#6092 = CARTESIAN_POINT ( 'NONE',  ( -73.34292637653381064, -9.058813317711329915, 2.943386871421371787 ) ) ;
#6093 = PLANE ( 'NONE',  #57341 ) ;
#6094 = CARTESIAN_POINT ( 'NONE',  ( 1.000000000000000888, 43.00000000000000000, 74.38749456993816978 ) ) ;
#6095 = DIRECTION ( 'NONE',  ( 0.000000000000000000, 0.000000000000000000, 1.000000000000000000 ) ) ;
#6096 = PLANE ( 'NONE',  #6070 ) ;
#6097 = VERTEX_POINT ( 'NONE', #41622 ) ;
#6098 = CARTESIAN_POINT ( 'NONE',  ( -168.5049999999999955, -6.826472737025113702, -4.959722759717900331 ) ) ;
#6099 = CONICAL_SURFACE ( 'NONE', #30797, 9.000000000000000000, 0.7853981633974500554 ) ;
#6100 = ORIENTED_EDGE ( 'NONE', *, *, #60080, .F. ) ;
#6102 = CARTESIAN_POINT ( 'NONE',  ( -24.00000000000000355, 36.75000000000000000, -3.750000000000000000 ) ) ;
#6101 = ADVANCED_BREP_SHAPE_REPRESENTATION ( '', ( #28116, #42840 ), #4621 ) ;
#6104 = EDGE_CURVE ( 'NONE', #46312, #54047, #51815, .T. ) ;
#6103 = CARTESIAN_POINT ( 'NONE',  ( -43.75000000000000000, 0.000000000000000000, -3.499999999999997335 ) ) ;
#6105 = DIRECTION ( 'NONE',  ( 0.000000000000000000, -1.000000000000000000, 0.000000000000000000 ) ) ;
#6106 = CIRCLE ( 'NONE', #44379, 12.50000000000000355 ) ;
#6107 = CARTESIAN_POINT ( 'NONE',  ( -181.5570736234661808, -1.166476076187852838E-15, -9.524999999999991473 ) ) ;
#6108 = CARTESIAN_POINT ( 'NONE',  ( 0.000000000000000000, 151.0570736234661524, -8.025000000000000355 ) ) ;
#6109 = AXIS2_PLACEMENT_3D ( 'NONE', #4010, #9688, #63474 ) ;
#6110 = ORIENTED_EDGE ( 'NONE', *, *, #33736, .F. ) ;
#6111 = EDGE_CURVE ( 'NONE', #29727, #3314, #19787, .T. ) ;
#6112 = LINE ( 'NONE', #46574, #60828 ) ;
#6113 = CARTESIAN_POINT ( 'NONE',  ( -91.10499999999998977, -6.826472737025113702, 4.959722759717902107 ) ) ;
#6114 = CIRCLE ( 'NONE', #39857, 23.00000000000000000 ) ;
#6115 = UNCERTAINTY_MEASURE_WITH_UNIT (LENGTH_MEASURE( 1.000000000000000082E-05 ), #58706, 'distance_accuracy_value', 'NONE');
#6116 = CARTESIAN_POINT ( 'NONE',  ( 57.00000000000000000, 5.000000000000000000, -55.00402776293825724 ) ) ;
#6117 = EDGE_LOOP ( 'NONE', ( #63068, #22200, #15913, #23090, #48157 ) ) ;
#6118 = CARTESIAN_POINT ( 'NONE',  ( -91.55707362346616662, -1.166476076187852838E-15, -9.524999999999991473 ) ) ;
#6119 = CIRCLE ( 'NONE', #45494, 0.2499999999999997780 ) ;
#6120 = EDGE_CURVE ( 'NONE', #31091, #69107, #24709, .T. ) ;
#6121 = FACE_OUTER_BOUND ( 'NONE', #6609, .T. ) ;
#6122 = DIRECTION ( 'NONE',  ( 0.000000000000000000, 0.000000000000000000, 1.000000000000000000 ) ) ;
#6123 = FACE_OUTER_BOUND ( 'NONE', #15272, .T. ) ;
#6124 = EDGE_LOOP ( 'NONE', ( #50786, #16577, #55238, #3019 ) ) ;
#6125 = FILL_AREA_STYLE ('',( #38872 ) ) ;
#6126 = CARTESIAN_POINT ( 'NONE',  ( -60.74499999999997613, 4.716976649647094177, 6.492361379858945902 ) ) ;
#6127 = ORIENTED_EDGE ( 'NONE', *, *, #332, .F. ) ;
#6128 = CARTESIAN_POINT ( 'NONE',  ( -74.99999999999998579, 50.00000000000000000, -6.500000000000000000 ) ) ;
#6129 = PRESENTATION_LAYER_ASSIGNMENT (  '', '', ( #49938 ) ) ;
#6130 = DIRECTION ( 'NONE',  ( -1.000000000000000000, 0.000000000000000000, 0.000000000000000000 ) ) ;
#6131 = LINE ( 'NONE', #17740, #17365 ) ;
#6132 = ORIENTED_EDGE ( 'NONE', *, *, #22088, .F. ) ;
#6133 = CYLINDRICAL_SURFACE ( 'NONE', #4423, 0.5000000000000004441 ) ;
#6134 = CARTESIAN_POINT ( 'NONE',  ( -71.75000000000000000, 4.336808689942018722E-16, 20.00000000000000000 ) ) ;
#6135 = ORIENTED_EDGE ( 'NONE', *, *, #19275, .T. ) ;
#6136 = ADVANCED_FACE ( 'NONE', ( #41281 ), #68684, .F. ) ;
#6138 = LINE ( 'NONE', #48752, #44954 ) ;
#6137 = CIRCLE ( 'NONE', #33111, 0.2500000000000002220 ) ;
#6139 = CARTESIAN_POINT ( 'NONE',  ( -118.7049999999999699, 2.607480562269073321, 8.024999999999991473 ) ) ;
#6140 = ORIENTED_EDGE ( 'NONE', *, *, #52011, .F. ) ;
#6141 = CARTESIAN_POINT ( 'NONE',  ( 16.75000000000000711, 27.99999999999998224, -3.750000000000000000 ) ) ;
#6142 = CARTESIAN_POINT ( 'NONE',  ( 31.14385416795345307, 42.99999999999999289, -45.61250543006184444 ) ) ;
#6143 = FILL_AREA_STYLE ('',( #22320 ) ) ;
#6144 = PRESENTATION_STYLE_ASSIGNMENT (( #54668 ) ) ;
#6145 = SURFACE_SIDE_STYLE ('',( #32886 ) ) ;
#6146 = AXIS2_PLACEMENT_3D ( 'NONE', #8465, #24961, #41187 ) ;
#6147 = CARTESIAN_POINT ( 'NONE',  ( -148.8570736234661638, -5.598654528085803328, -7.705886871421366635 ) ) ;
#6148 = CARTESIAN_POINT ( 'NONE',  ( -8.102448949553179958, 128.4950000000000045, 5.886773742842747126 ) ) ;
#6149 = CARTESIAN_POINT ( 'NONE',  ( -97.40707362346614673, 3.094860106618428031, -9.524999999999993250 ) ) ;
#6150 = DIRECTION ( 'NONE',  ( 0.000000000000000000, 1.000000000000000000, -0.000000000000000000 ) ) ;
#6151 = ORIENTED_EDGE ( 'NONE', *, *, #47413, .F. ) ;
#6152 = SURFACE_STYLE_FILL_AREA ( #43150 ) ;
#6153 = AXIS2_PLACEMENT_3D ( 'NONE', #36986, #58399, #4929 ) ;
#6154 = CARTESIAN_POINT ( 'NONE',  ( -15.79964225816357626, 58.31681314173472686, 6.349999999999996092 ) ) ;
#6155 = CARTESIAN_POINT ( 'NONE',  ( -129.3549999999999898, -4.716976649647093289, -6.492361379858945902 ) ) ;
#6156 = DIRECTION ( 'NONE',  ( 0.000000000000000000, -1.000000000000000000, 0.000000000000000000 ) ) ;
#6157 = CARTESIAN_POINT ( 'NONE',  ( -14.98999599679678951, 146.4999999999999716, -10.00000000000000000 ) ) ;
#6158 = CARTESIAN_POINT ( 'NONE',  ( -144.1449999999999818, -4.716976649647092401, 6.492361379858946790 ) ) ;
#6159 = AXIS2_PLACEMENT_3D ( 'NONE', #22648, #17402, #38865 ) ;
#6160 = CARTESIAN_POINT ( 'NONE',  ( -126.8949999999999818, 6.826472737025115478, 4.959722759717899443 ) ) ;
#6161 = ORIENTED_EDGE ( 'NONE', *, *, #46750, .F. ) ;
#6162 = CIRCLE ( 'NONE', #64616, 10.99999999999995381 ) ;
#6163 = DIRECTION ( 'NONE',  ( 0.000000000000000000, 1.000000000000000000, 0.000000000000000000 ) ) ;
#6164 = FACE_OUTER_BOUND ( 'NONE', #27520, .T. ) ;
#6165 = COLOUR_RGB ( '', 0.66274510, 0.83137255, 0.94901961) ;
#6166 = CARTESIAN_POINT ( 'NONE',  ( -184.7929263765338135, -3.094860106618429807, 9.524999999999991473 ) ) ;
#6167 = FACE_OUTER_BOUND ( 'NONE', #41521, .T. ) ;
#6168 = CARTESIAN_POINT ( 'NONE',  ( -63.44499999999998607, 0.000000000000000000, 8.024999999999991473 ) ) ;
#6169 = CARTESIAN_POINT ( 'NONE',  ( -139.1929263765337907, -10.01517768586948698, 6.132527647946031529E-16 ) ) ;
#6170 = SPHERICAL_SURFACE ( 'NONE', #52688, 1.000000000000000000 ) ;
#6171 = SURFACE_STYLE_FILL_AREA ( #21298 ) ;
#6172 =( LENGTH_UNIT ( ) NAMED_UNIT ( * ) SI_UNIT ( .MILLI., .METRE. ) );
#6173 = CARTESIAN_POINT ( 'NONE',  ( -74.99999999999998579, 50.00000000000000000, 12.00000000000000000 ) ) ;
#6174 = CARTESIAN_POINT ( 'NONE',  ( -104.8429263765338106, 9.058813317711329915, -2.943386871421373119 ) ) ;
#6175 = DIRECTION ( 'NONE',  ( 1.665334536937734811E-16, -0.2825670446618928633, 0.9592475516106591105 ) ) ;
#6176 = TOROIDAL_SURFACE ( 'NONE', #1602, 0.7500000000000000000, 0.2500000000000000000 ) ;
#6177 = FACE_OUTER_BOUND ( 'NONE', #18580, .T. ) ;
#6178 = STYLED_ITEM ( 'NONE', ( #31908 ), #8013 ) ;
#6179 = CARTESIAN_POINT ( 'NONE',  ( -99.20707362346720970, 3.094860106635777264, 9.524999999987391774 ) ) ;
#6180 = COLOUR_RGB ( '', 0.66274510, 0.83137255, 0.94901961) ;
#6181 = CARTESIAN_POINT ( 'NONE',  ( 21.50000000000000711, 22.24999999999998224, 3.750000000000000000 ) ) ;
#6182 = ORIENTED_EDGE ( 'NONE', *, *, #8990, .F. ) ;
#6183 = CARTESIAN_POINT ( 'NONE',  ( 93.00000000000000000, 0.000000000000000000, 0.000000000000000000 ) ) ;
#6184 = ADVANCED_FACE ( 'NONE', ( #25747 ), #14505, .F. ) ;
#6186 = EDGE_LOOP ( 'NONE', ( #35211, #42911, #21981, #23585 ) ) ;
#6185 = PRESENTATION_LAYER_ASSIGNMENT (  '', '', ( #57877 ) ) ;
#6187 = DIRECTION ( 'NONE',  ( -0.000000000000000000, -0.000000000000000000, 1.000000000000000000 ) ) ;
#6188 = AXIS2_PLACEMENT_3D ( 'NONE', #62847, #14687, #8006 ) ;
#6189 = CARTESIAN_POINT ( 'NONE',  ( -2.607480562269075097, 113.4070736234661609, 8.025000000000000355 ) ) ;
#6190 = FACE_OUTER_BOUND ( 'NONE', #32555, .T. ) ;
#6191 =( NAMED_UNIT ( * ) SI_UNIT ( $, .STERADIAN. ) SOLID_ANGLE_UNIT ( ) );
#6192 = VERTEX_POINT ( 'NONE', #20845 ) ;
#6193 = ORIENTED_EDGE ( 'NONE', *, *, #5187, .F. ) ;
#6194 = CARTESIAN_POINT ( 'NONE',  ( -195.0000000000000000, 0.000000000000000000, 0.000000000000000000 ) ) ;
#6195 = EDGE_CURVE ( 'NONE', #4847, #51461, #43131, .T. ) ;
#6196 = LINE ( 'NONE', #33962, #52965 ) ;
#6197 = VERTEX_POINT ( 'NONE', #14882 ) ;
#6198 = FILL_AREA_STYLE_COLOUR ( '', #45704 ) ;
#6199 = CARTESIAN_POINT ( 'NONE',  ( -118.5570736234661808, -1.166476076187852838E-15, -9.524999999999991473 ) ) ;
#6200 = EDGE_CURVE ( 'NONE', #20172, #58654, #54263, .T. ) ;
#6201 = AXIS2_PLACEMENT_3D ( 'NONE', #55956, #34843, #50691 ) ;
#6202 = B_SPLINE_CURVE_WITH_KNOTS ( 'NONE', 3,
 ( #51728, #22131, #37670, #27379, #16879, #69293, #21087, #256 ),
 .UNSPECIFIED., .F., .F.,
 ( 4, 2, 2, 4 ),
 ( 2.544316211733585141E-07, 0.002094919859796804708, 0.003142252573884620707, 0.004189585287972436706 ),
 .UNSPECIFIED. ) ;
#6203 = EDGE_CURVE ( 'NONE', #17336, #19236, #57785, .T. ) ;
#6204 = DIRECTION ( 'NONE',  ( -0.000000000000000000, -0.000000000000000000, -1.000000000000000000 ) ) ;
#6205 = CARTESIAN_POINT ( 'NONE',  ( -87.44499999999999318, 0.000000000000000000, 8.024999999999991473 ) ) ;
#6206 = ORIENTED_EDGE ( 'NONE', *, *, #19056, .F. ) ;
#6207 = AXIS2_PLACEMENT_3D ( 'NONE', #62595, #14409, #24970 ) ;
#6208 = CARTESIAN_POINT ( 'NONE',  ( 25.75000000000001066, 21.74999999999998224, 3.750000000000000000 ) ) ;
#6209 = ADVANCED_FACE ( 'NONE', ( #63729 ), #39556, .F. ) ;
#6210 = DIRECTION ( 'NONE',  ( 0.000000000000000000, 0.000000000000000000, 1.000000000000000000 ) ) ;
#6211 = AXIS2_PLACEMENT_3D ( 'NONE', #28285, #29344, #49790 ) ;
#6212 = ORIENTED_EDGE ( 'NONE', *, *, #42310, .T. ) ;
#6213 = CARTESIAN_POINT ( 'NONE',  ( -174.5929263765339385, -3.094860106620549001, -9.524999999998453148 ) ) ;
#6214 =( BOUNDED_CURVE ( )  B_SPLINE_CURVE ( 2, ( #38396, #29143, #54839, #50631, #66097, #11953, #39763, #12635, #23535, #28808, #49958 ),
 .UNSPECIFIED., .F., .F. ) 
 B_SPLINE_CURVE_WITH_KNOTS ( ( 3, 2, 2, 2, 2, 3 ),
 ( 0.2717391304347762659, 0.2739130434782544588, 0.2760869565217327071, 0.2782608695652109554, 0.2804347826086891482, 0.2826086956521673410 ),
 .UNSPECIFIED. ) 
 CURVE ( )  GEOMETRIC_REPRESENTATION_ITEM ( )  RATIONAL_B_SPLINE_CURVE ( ( 1.000000000000142553, 0.9510565162950110896, 1.000000000000000000, 0.9510565162951535312, 1.000000000000000000, 0.9510565162951535312, 1.000000000000000000, 0.9510565162951535312, 1.000000000000000000, 0.9510565162953009688, 0.9999999999998525624 ) ) 
 REPRESENTATION_ITEM ( '' )  );
#6215 = FACE_OUTER_BOUND ( 'NONE', #15532, .T. ) ;
#6216 = CARTESIAN_POINT ( 'NONE',  ( 5.196152422706628471, 1.107695154586738173, -9.000000000000005329 ) ) ;
#6217 = ORIENTED_EDGE ( 'NONE', *, *, #43407, .T. ) ;
#6218 = DIRECTION ( 'NONE',  ( -1.000000000000000000, -1.099520432716498821E-15, 0.000000000000000000 ) ) ;
#6219 = ORIENTED_EDGE ( 'NONE', *, *, #37632, .F. ) ;
#6220 = CARTESIAN_POINT ( 'NONE',  ( -166.4070736234663741, 3.094860106615134221, -9.525000000002387779 ) ) ;
#6221 = CARTESIAN_POINT ( 'NONE',  ( 66.49999999999998579, 36.75000000000000000, -3.750000000000000000 ) ) ;
#6222 = CARTESIAN_POINT ( 'NONE',  ( 45.00000000000000000, -1.469576158976824618E-14, 10.00000000000000000 ) ) ;
#6223 = DIRECTION ( 'NONE',  ( -1.000000000000000000, 0.000000000000000000, -0.000000000000000000 ) ) ;
#6224 = B_SPLINE_CURVE_WITH_KNOTS ( 'NONE', 3,
 ( #52934, #64156, #16012, #69444, #58897, #42762, #42418, #52257 ),
 .UNSPECIFIED., .F., .F.,
 ( 4, 2, 2, 4 ),
 ( 4.596172765309288096E-15, 0.0008152109970724930607, 0.001630421994140389972, 0.003260843988276192467 ),
 .UNSPECIFIED. ) ;
#6225 = CARTESIAN_POINT ( 'NONE',  ( -10.74999999999999645, 4.336808689942018722E-16, 7.000000000000001776 ) ) ;
#6226 = COLOUR_RGB ( '', 0.40784314, 0.44705882, 0.49803922) ;
#6227 = DIRECTION ( 'NONE',  ( -0.000000000000000000, 0.000000000000000000, -1.000000000000000000 ) ) ;
#6228 = CARTESIAN_POINT ( 'NONE',  ( -6.946753979098152953, 153.3272276288669502, -4.645043913640976463 ) ) ;
#6229 = EDGE_LOOP ( 'NONE', ( #17991, #1390, #19875, #25266 ) ) ;
#6230 = DIRECTION ( 'NONE',  ( 0.000000000000000000, 0.000000000000000000, -1.000000000000000000 ) ) ;
#6231 =( NAMED_UNIT ( * ) SI_UNIT ( $, .STERADIAN. ) SOLID_ANGLE_UNIT ( ) );
#6233 = DIRECTION ( 'NONE',  ( 0.000000000000000000, 1.000000000000000000, 0.000000000000000000 ) ) ;
#6232 = AXIS2_PLACEMENT_3D ( 'NONE', #67676, #56417, #7541 ) ;
#6234 = ORIENTED_EDGE ( 'NONE', *, *, #2516, .F. ) ;
#6235 = CARTESIAN_POINT ( 'NONE',  ( -159.8049999999999784, -8.437984349512085203, 5.166775262442717831E-16 ) ) ;
#6236 = FACE_OUTER_BOUND ( 'NONE', #55636, .T. ) ;
#6237 = CARTESIAN_POINT ( 'NONE',  ( -183.6149733308552641, -5.710802470748983062, -6.846503224029541812 ) ) ;
#6238 = CARTESIAN_POINT ( 'NONE',  ( -170.5450000000000159, -7.632228543268600340, -2.479861379858950166 ) ) ;
#6239 = CIRCLE ( 'NONE', #39973, 0.5000000000000004441 ) ;
#6240 = CARTESIAN_POINT ( 'NONE',  ( -167.2450000000000045, -4.716976649647093289, -6.492361379858945902 ) ) ;
#6241 =( BOUNDED_CURVE ( )  B_SPLINE_CURVE ( 2, ( #29339, #39601, #24078, #56791, #19124, #35335, #34616, #61005, #55744, #18792, #7550 ),
 .UNSPECIFIED., .F., .F. ) 
 B_SPLINE_CURVE_WITH_KNOTS ( ( 3, 2, 2, 2, 2, 3 ),
 ( 0.4565217391304239314, 0.4586956521739021797, 0.4608695652173803725, 0.4630434782608585098, 0.4652173913043367026, 0.4673913043478149509 ),
 .UNSPECIFIED. ) 
 CURVE ( )  GEOMETRIC_REPRESENTATION_ITEM ( )  RATIONAL_B_SPLINE_CURVE ( ( 1.000000000000243805, 0.9510565162949098372, 1.000000000000000000, 0.9510565162951535312, 1.000000000000000000, 0.9510565162951535312, 1.000000000000000000, 0.9510565162951535312, 1.000000000000000000, 0.9510565162954047747, 0.9999999999997487565 ) ) 
 REPRESENTATION_ITEM ( '' )  );
#6242 = VERTEX_POINT ( 'NONE', #54217 ) ;
#6243 = CARTESIAN_POINT ( 'NONE',  ( 32.00000000000000000, 42.00000000000000000, -74.38749456993816978 ) ) ;
#6244 = CARTESIAN_POINT ( 'NONE',  ( -4.716976649647098618, 151.1429263765338078, 6.492361379858953008 ) ) ;
#6245 = CARTESIAN_POINT ( 'NONE',  ( -84.20499999999995566, -2.607480562269071545, -8.024999999999991473 ) ) ;
#6246 = PRESENTATION_STYLE_ASSIGNMENT (( #208 ) ) ;
#6247 = DIRECTION ( 'NONE',  ( 0.000000000000000000, 0.000000000000000000, 1.000000000000000000 ) ) ;
#6248 = CIRCLE ( 'NONE', #54549, 10.02500000000000568 ) ;
#6249 = CARTESIAN_POINT ( 'NONE',  ( -79.64499999999999602, 4.716976649647091513, -6.492361379858946790 ) ) ;
#6250 = CARTESIAN_POINT ( 'NONE',  ( 10.01517768586949231, 133.8049999999999784, 1.839758294383810543E-15 ) ) ;
#6251 = SURFACE_STYLE_USAGE ( .BOTH. , #48171 ) ;
#6252 = STYLED_ITEM ( 'NONE', ( #67208 ), #58207 ) ;
#6253 = VECTOR ( 'NONE', #37780, 1000.000000000000000 ) ;
#6254 = DIRECTION ( 'NONE',  ( 0.000000000000000000, -1.000000000000000000, 0.000000000000000000 ) ) ;
#6255 = AXIS2_PLACEMENT_3D ( 'NONE', #15155, #47887, #63649 ) ;
#6256 =( NAMED_UNIT ( * ) PLANE_ANGLE_UNIT ( ) SI_UNIT ( $, .RADIAN. ) );
#6257 =( NAMED_UNIT ( * ) SI_UNIT ( $, .STERADIAN. ) SOLID_ANGLE_UNIT ( ) );
#6258 = ORIENTED_EDGE ( 'NONE', *, *, #36330, .F. ) ;
#6259 = AXIS2_PLACEMENT_3D ( 'NONE', #9305, #52233, #52574 ) ;
#6260 = FACE_OUTER_BOUND ( 'NONE', #27726, .T. ) ;
#6261 = EDGE_CURVE ( 'NONE', #62586, #14708, #46492, .T. ) ;
#6262 = PLANE ( 'NONE',  #58857 ) ;
#6263 = SURFACE_SIDE_STYLE ('',( #65358 ) ) ;
#6264 = ORIENTED_EDGE ( 'NONE', *, *, #19914, .F. ) ;
#6265 = VERTEX_POINT ( 'NONE', #10965 ) ;
#6266 = CYLINDRICAL_SURFACE ( 'NONE', #21889, 15.00000000000000000 ) ;
#6267 = EDGE_CURVE ( 'NONE', #58659, #65395, #22858, .T. ) ;
#6268 = CIRCLE ( 'NONE', #24248, 0.2500000000000002220 ) ;
#6269 = SURFACE_SIDE_STYLE ('',( #58708 ) ) ;
#6270 = DIRECTION ( 'NONE',  ( 1.000000000000000000, 2.304236466203155263E-14, 0.000000000000000000 ) ) ;
#6271 = ORIENTED_EDGE ( 'NONE', *, *, #11480, .F. ) ;
#6272 = CARTESIAN_POINT ( 'NONE',  ( -117.2049999999999699, -2.607480562269071545, -8.024999999999991473 ) ) ;
#6273 = ORIENTED_EDGE ( 'NONE', *, *, #49262, .T. ) ;
#6274 = AXIS2_PLACEMENT_3D ( 'NONE', #3764, #57622, #9442 ) ;
#6275 = EDGE_LOOP ( 'NONE', ( #15555, #18332, #59764, #20222 ) ) ;
#6276 = CARTESIAN_POINT ( 'NONE',  ( -56.39292637653378648, 8.102448949553176405, 5.886773742842740909 ) ) ;
#6277 = CARTESIAN_POINT ( 'NONE',  ( -68.30707362346618083, -10.01517768586948698, 6.132527647946031529E-16 ) ) ;
#6278 = ORIENTED_EDGE ( 'NONE', *, *, #57839, .F. ) ;
#6279 = EDGE_CURVE ( 'NONE', #16530, #17308, #47976, .T. ) ;
#6280 = COLOUR_RGB ( '', 0.66274510, 0.83137255, 0.94901961) ;
#6281 = STYLED_ITEM ( 'NONE', ( #66064 ), #732 ) ;
#6282 = PRESENTATION_LAYER_ASSIGNMENT (  '', '', ( #36679 ) ) ;
#6283 = VERTEX_POINT ( 'NONE', #16287 ) ;
#6284 = ORIENTED_EDGE ( 'NONE', *, *, #13251, .F. ) ;
#6285 = FILL_AREA_STYLE ('',( #43301 ) ) ;
#6286 =( NAMED_UNIT ( * ) PLANE_ANGLE_UNIT ( ) SI_UNIT ( $, .RADIAN. ) );
#6287 = EDGE_CURVE ( 'NONE', #62679, #30440, #37414, .T. ) ;
#6288 = CARTESIAN_POINT ( 'NONE',  ( -45.00000000000000000, 9.708372675170618749, 3.611004237778676185 ) ) ;
#6289 = EDGE_LOOP ( 'NONE', ( #33546, #3585 ) ) ;
#6290 = CARTESIAN_POINT ( 'NONE',  ( 7.632228543268608334, 134.3429263765337964, -2.479861379858951942 ) ) ;
#6291 = CARTESIAN_POINT ( 'NONE',  ( 18.00000000000000711, 33.99999999999999289, 3.750000000000000000 ) ) ;
#6292 = CARTESIAN_POINT ( 'NONE',  ( -11.99999999999999822, -8.499999999999998224, 21.00000000000000000 ) ) ;
#6293 = DIRECTION ( 'NONE',  ( 1.000000000000000000, 0.000000000000000000, 0.000000000000000000 ) ) ;
#6294 = ORIENTED_EDGE ( 'NONE', *, *, #47050, .F. ) ;
#6295 = CARTESIAN_POINT ( 'NONE',  ( 10.99999999999999645, 11.99999999999999289, 4.000000000000000000 ) ) ;
#6296 = VERTEX_POINT ( 'NONE', #16621 ) ;
#6297 = AXIS2_PLACEMENT_3D ( 'NONE', #65133, #38469, #32101 ) ;
#6298 = SPHERICAL_SURFACE ( 'NONE', #4853, 0.2500000000000000000 ) ;
#6299 = CARTESIAN_POINT ( 'NONE',  ( 0.000000000000000000, 154.9999999999999716, 0.000000000000000000 ) ) ;
#6300 = CARTESIAN_POINT ( 'NONE',  ( -146.9049999999999727, 2.607480562269068880, -8.024999999999993250 ) ) ;
#6301 = FILL_AREA_STYLE_COLOUR ( '', #51030 ) ;
#6302 = DIRECTION ( 'NONE',  ( 0.000000000000000000, 0.000000000000000000, 1.000000000000000000 ) ) ;
#6303 = ORIENTED_EDGE ( 'NONE', *, *, #67345, .T. ) ;
#6304 = VECTOR ( 'NONE', #42769, 1000.000000000000000 ) ;
#6305 = CARTESIAN_POINT ( 'NONE',  ( -106.9429263765337907, 0.000000000000000000, 9.524999999999991473 ) ) ;
#6306 = CARTESIAN_POINT ( 'NONE',  ( 41.49999999999998579, 106.9282032302754857, 3.500000000000000888 ) ) ;
#6307 = ORIENTED_EDGE ( 'NONE', *, *, #64645, .T. ) ;
#6308 = EDGE_LOOP ( 'NONE', ( #61242, #8580, #31099, #47846 ) ) ;
#6309 = DIRECTION ( 'NONE',  ( 0.000000000000000000, 0.000000000000000000, 1.000000000000000000 ) ) ;
#6310 = CARTESIAN_POINT ( 'NONE',  ( 59.00000000000000000, 11.99999999999999822, 4.000000000000000000 ) ) ;
#6311 = CARTESIAN_POINT ( 'NONE',  ( -57.20499999999996987, -2.607480562269071545, -8.024999999999991473 ) ) ;
#6312 = ORIENTED_EDGE ( 'NONE', *, *, #22393, .F. ) ;
#6313 = FACE_BOUND ( 'NONE', #50082, .T. ) ;
#6314 = SURFACE_STYLE_FILL_AREA ( #954 ) ;
#6315 = CARTESIAN_POINT ( 'NONE',  ( -28.94093048474993779, -8.499999999999996447, 0.6846459046698460948 ) ) ;
#6316 = SURFACE_STYLE_FILL_AREA ( #31672 ) ;
#6317 = DIRECTION ( 'NONE',  ( -0.000000000000000000, -0.000000000000000000, -1.000000000000000000 ) ) ;
#6318 = DIRECTION ( 'NONE',  ( 0.000000000000000000, 0.000000000000000000, 1.000000000000000000 ) ) ;
#6319 = B_SPLINE_CURVE_WITH_KNOTS ( 'NONE', 3,
 ( #11135, #54045, #5849, #27292, #48831, #525, #22053, #2532 ),
 .UNSPECIFIED., .F., .F.,
 ( 4, 2, 2, 4 ),
 ( 2.544316211736855218E-07, 0.002094919859796806443, 0.003142252573884622875, 0.004189585287972439308 ),
 .UNSPECIFIED. ) ;
#6320 = ORIENTED_EDGE ( 'NONE', *, *, #56296, .F. ) ;
#6321 = EDGE_CURVE ( 'NONE', #65527, #61162, #66635, .T. ) ;
#6322 = DIRECTION ( 'NONE',  ( 0.000000000000000000, 0.000000000000000000, -1.000000000000000000 ) ) ;
#6323 = CARTESIAN_POINT ( 'NONE',  ( -6.020204320972970535, 1.861307952554190903, -7.572700244129129565 ) ) ;
#6324 =( NAMED_UNIT ( * ) SI_UNIT ( $, .STERADIAN. ) SOLID_ANGLE_UNIT ( ) );
#6325 = CARTESIAN_POINT ( 'NONE',  ( 0.000000000000000000, 0.000000000000000000, 1.000000000000000000 ) ) ;
#6326 = CARTESIAN_POINT ( 'NONE',  ( 23.50000000000001776, 24.55989583710066171, 27.18999999999999062 ) ) ;
#6327 = VECTOR ( 'NONE', #48924, 1000.000000000000000 ) ;
#6328 = CARTESIAN_POINT ( 'NONE',  ( -110.9949999999999903, -6.826472737025113702, 4.959722759717902107 ) ) ;
#6329 = CARTESIAN_POINT ( 'NONE',  ( 8.102448949553183510, 153.9950000000000045, -5.886773742842746238 ) ) ;
#6330 = AXIS2_PLACEMENT_3D ( 'NONE', #54122, #54472, #65385 ) ;
#6331 = CARTESIAN_POINT ( 'NONE',  ( -89.99499999999999034, -6.826472737025115478, 4.959722759717900331 ) ) ;
#6332 = AXIS2_PLACEMENT_3D ( 'NONE', #38090, #6377, #5672 ) ;
#6333 = CARTESIAN_POINT ( 'NONE',  ( 8.082903768654762899, -1.269775441351268174E-15, 1.082903768654759125 ) ) ;
#6334 = CARTESIAN_POINT ( 'NONE',  ( -9.908575283019912422E-16, -6.500000000000002665, 0.000000000000000000 ) ) ;
#6335 = DIRECTION ( 'NONE',  ( 0.000000000000000000, 0.000000000000000000, -1.000000000000000000 ) ) ;
#6336 =( BOUNDED_CURVE ( )  B_SPLINE_CURVE ( 2, ( #15462, #53076, #21745, #4870, #64301, #26313, #69582, #63950, #15797, #58679, #5536 ),
 .UNSPECIFIED., .F., .F. ) 
 B_SPLINE_CURVE_WITH_KNOTS ( ( 3, 2, 2, 2, 2, 3 ),
 ( 0.07608695652173741442, 0.07826086956521563498, 0.08043478260869382779, 0.08260869565217204835, 0.08478260869565025504, 0.08695652173912847560 ),
 .UNSPECIFIED. ) 
 CURVE ( )  GEOMETRIC_REPRESENTATION_ITEM ( )  RATIONAL_B_SPLINE_CURVE ( ( 1.000000000000038636, 0.9510565162951147844, 1.000000000000000000, 0.9510565162951535312, 1.000000000000000000, 0.9510565162951535312, 1.000000000000000000, 0.9510565162951535312, 1.000000000000000000, 0.9510565162951976070, 0.9999999999999559241 ) ) 
 REPRESENTATION_ITEM ( '' )  );
#6337 = VERTEX_POINT ( 'NONE', #33128 ) ;
#6338 = CARTESIAN_POINT ( 'NONE',  ( -120.2929263765337993, 3.094860106618428031, -9.524999999999993250 ) ) ;
#6339 = SHAPE_REPRESENTATION_RELATIONSHIP ( 'NONE' , 'NONE' ,  #67568, #11074 ) ;
#6340 = CARTESIAN_POINT ( 'NONE',  ( -146.8449999999999989, -7.632228543268599452, 2.479861379858951054 ) ) ;
#6341 = DIRECTION ( 'NONE',  ( -1.000000000000000000, -0.000000000000000000, -0.000000000000000000 ) ) ;
#6342 = EDGE_CURVE ( 'NONE', #51568, #29587, #31818, .T. ) ;
#6343 = AXIS2_PLACEMENT_3D ( 'NONE', #43881, #5837, #32570 ) ;
#6344 = EDGE_CURVE ( 'NONE', #57528, #54598, #51647, .T. ) ;
#6345 = CARTESIAN_POINT ( 'NONE',  ( -47.24499999999998323, -4.716976649647093289, -6.492361379858945902 ) ) ;
#6346 = DIRECTION ( 'NONE',  ( -1.000000000000000000, 0.000000000000000000, 0.000000000000000000 ) ) ;
#6347 = ORIENTED_EDGE ( 'NONE', *, *, #5163, .T. ) ;
#6348 = VERTEX_POINT ( 'NONE', #22565 ) ;
#6349 = LINE ( 'NONE', #17633, #53906 ) ;
#6350 = DIRECTION ( 'NONE',  ( 0.000000000000000000, 0.000000000000000000, 1.000000000000000000 ) ) ;
#6351 = EDGE_CURVE ( 'NONE', #14037, #6066, #38087, .T. ) ;
#6352 = ADVANCED_FACE ( 'NONE', ( #48997 ), #36344, .F. ) ;
#6353 = FACE_BOUND ( 'NONE', #52622, .T. ) ;
#6354 = CYLINDRICAL_SURFACE ( 'NONE', #48341, 9.524999999999991473 ) ;
#6355 = FACE_OUTER_BOUND ( 'NONE', #3639, .T. ) ;
#6356 = CARTESIAN_POINT ( 'NONE',  ( -151.1929263765338192, -10.01517768586948698, 6.132527647946031529E-16 ) ) ;
#6357 = ORIENTED_EDGE ( 'NONE', *, *, #33765, .T. ) ;
#6358 = CARTESIAN_POINT ( 'NONE',  ( -144.6549999999999727, -7.632228543268600340, -2.479861379858950166 ) ) ;
#6359 = ORIENTED_EDGE ( 'NONE', *, *, #43353, .F. ) ;
#6360 = ORIENTED_EDGE ( 'NONE', *, *, #65356, .F. ) ;
#6361 = DIRECTION ( 'NONE',  ( -1.000000000000000000, -0.000000000000000000, -0.000000000000000000 ) ) ;
#6362 = CARTESIAN_POINT ( 'NONE',  ( -195.0000000000000000, 0.000000000000000000, 9.524999999999991473 ) ) ;
#6363 = ORIENTED_EDGE ( 'NONE', *, *, #35427, .T. ) ;
#6364 = EDGE_CURVE ( 'NONE', #67303, #33055, #53206, .T. ) ;
#6365 = LINE ( 'NONE', #41195, #34331 ) ;
#6366 = CARTESIAN_POINT ( 'NONE',  ( -8.102448949553181734, 133.8950000000000102, -5.886773742842749790 ) ) ;
#6367 = ORIENTED_EDGE ( 'NONE', *, *, #56153, .F. ) ;
#6368 = FACE_OUTER_BOUND ( 'NONE', #66542, .T. ) ;
#6369 = CARTESIAN_POINT ( 'NONE',  ( -5.598654528085806881, 134.8549999999999898, -7.705886871421374629 ) ) ;
#6370 = CARTESIAN_POINT ( 'NONE',  ( -56.15499999999997982, 7.632228543268600340, 2.479861379858949277 ) ) ;
#6371 = CARTESIAN_POINT ( 'NONE',  ( -115.4949999999999903, 6.826472737025113702, -4.959722759717902107 ) ) ;
#6372 = EDGE_CURVE ( 'NONE', #24214, #52342, #48649, .T. ) ;
#6373 = CARTESIAN_POINT ( 'NONE',  ( -41.47746817312046375, 107.6230562796895356, -3.580135233559778030 ) ) ;
#6374 = VERTEX_POINT ( 'NONE', #34495 ) ;
#6375 = CARTESIAN_POINT ( 'NONE',  ( 5.598654528085809545, 155.2549999999999670, -7.705886871421373741 ) ) ;
#6376 = CARTESIAN_POINT ( 'NONE',  ( 3.062992266794108520, 51.20951172609373003, 7.099524902877636379 ) ) ;
#6377 = DIRECTION ( 'NONE',  ( 0.000000000000000000, 0.000000000000000000, 1.000000000000000000 ) ) ;
#6378 = CIRCLE ( 'NONE', #68153, 4.499999999999997335 ) ;
#6379 = DIRECTION ( 'NONE',  ( 1.300977106640434891E-16, 0.000000000000000000, 1.000000000000000000 ) ) ;
#6380 = DIRECTION ( 'NONE',  ( -1.000000000000000000, 0.000000000000000000, -0.000000000000000000 ) ) ;
#6381 = STYLED_ITEM ( 'NONE', ( #55434 ), #3348 ) ;
#6382 = CARTESIAN_POINT ( 'NONE',  ( 13.50000000000000533, 30.74999999999999289, -3.750000000000000000 ) ) ;
#6383 = PRESENTATION_LAYER_ASSIGNMENT (  '', '', ( #5272 ) ) ;
#6384 = ORIENTED_EDGE ( 'NONE', *, *, #12694, .T. ) ;
#6385 = FILL_AREA_STYLE_COLOUR ( '', #47554 ) ;
#6386 = CARTESIAN_POINT ( 'NONE',  ( -176.0049999999999670, 6.826472737025116366, 4.959722759717898555 ) ) ;
#6387 = ORIENTED_EDGE ( 'NONE', *, *, #36149, .T. ) ;
#6388 = CARTESIAN_POINT ( 'NONE',  ( -87.95707362346617231, 9.058813317711329915, -2.943386871421373119 ) ) ;
#6389 = SURFACE_STYLE_FILL_AREA ( #28873 ) ;
#6390 = DIRECTION ( 'NONE',  ( 0.000000000000000000, 0.000000000000000000, -1.000000000000000000 ) ) ;
#6391 = DIRECTION ( 'NONE',  ( 0.000000000000000000, -0.000000000000000000, 1.000000000000000000 ) ) ;
#6392 = ORIENTED_EDGE ( 'NONE', *, *, #50135, .F. ) ;
#6393 = CARTESIAN_POINT ( 'NONE',  ( -45.00000000000000000, 8.062885781073934055, -3.611004237778684178 ) ) ;
#6394 = CIRCLE ( 'NONE', #61410, 5.999999999999998224 ) ;
#6395 = DIRECTION ( 'NONE',  ( -0.000000000000000000, -0.000000000000000000, 1.000000000000000000 ) ) ;
#6396 = CARTESIAN_POINT ( 'NONE',  ( -84.20499999999995566, -2.607480562269071545, -8.024999999999991473 ) ) ;
#6397 = ORIENTED_EDGE ( 'NONE', *, *, #34328, .T. ) ;
#6398 = DIRECTION ( 'NONE',  ( 1.000000000000000000, 0.000000000000000000, 0.000000000000000000 ) ) ;
#6399 =( LENGTH_UNIT ( ) NAMED_UNIT ( * ) SI_UNIT ( .MILLI., .METRE. ) );
#6400 = CARTESIAN_POINT ( 'NONE',  ( 23.21231517720798010, 113.4999999999999858, -9.500000000000000000 ) ) ;
#6401 = CARTESIAN_POINT ( 'NONE',  ( -69.80707362346613820, 10.01517768586948698, -1.839758294383808571E-15 ) ) ;
#6402 = ADVANCED_FACE ( 'NONE', ( #50009 ), #44507, .F. ) ;
#6403 = CARTESIAN_POINT ( 'NONE',  ( -74.23245021955101208, 8.860682567649762476, -6.389379348043731532 ) ) ;
#6404 = ORIENTED_EDGE ( 'NONE', *, *, #5211, .T. ) ;
#6405 = CARTESIAN_POINT ( 'NONE',  ( -47.00571487472603138, -11.85301361210301607, 3.279042910798483312 ) ) ;
#6407 = DIRECTION ( 'NONE',  ( -0.000000000000000000, 0.000000000000000000, -1.000000000000000000 ) ) ;
#6406 = SURFACE_STYLE_USAGE ( .BOTH. , #54600 ) ;
#6408 = CARTESIAN_POINT ( 'NONE',  ( -99.35499999999998977, -4.716976649647093289, -6.492361379858945902 ) ) ;
#6409 = CARTESIAN_POINT ( 'NONE',  ( -9.058813317711338797, 134.3449999999999989, 2.943386871421373563 ) ) ;
#6410 = CARTESIAN_POINT ( 'NONE',  ( -120.2949999999999733, -2.607480562269069768, 8.024999999999991473 ) ) ;
#6411 = PRODUCT_DEFINITION ( 'UNKNOWN', '', #18035, #56437 ) ;
#6413 = CARTESIAN_POINT ( 'NONE',  ( -19.99982264573705493, 11.99992610239912949, 0.3333660036662020043 ) ) ;
#6412 = DIRECTION ( 'NONE',  ( -0.000000000000000000, -1.000000000000000000, 0.000000000000000000 ) ) ;
#6414 = ADVANCED_FACE ( 'NONE', ( #66872 ), #60195, .F. ) ;
#6415 = CARTESIAN_POINT ( 'NONE',  ( -149.2429263765338021, 5.598654528085804216, 7.705886871421366635 ) ) ;
#6416 = SURFACE_STYLE_USAGE ( .BOTH. , #43757 ) ;
#6417 = CARTESIAN_POINT ( 'NONE',  ( -175.9449999999999932, -9.827790563157499189E-16, -8.024999999999991473 ) ) ;
#6418 = VECTOR ( 'NONE', #63904, 1000.000000000000000 ) ;
#6419 = COLOUR_RGB ( '', 0.66274510, 0.83137255, 0.94901961) ;
#6420 = EDGE_CURVE ( 'NONE', #61213, #65002, #30708, .T. ) ;
#6421 = ADVANCED_FACE ( 'NONE', ( #50339 ), #61549, .F. ) ;
#6422 = AXIS2_PLACEMENT_3D ( 'NONE', #7766, #35565, #7091 ) ;
#6423 = LINE ( 'NONE', #1073, #33235 ) ;
#6424 = CARTESIAN_POINT ( 'NONE',  ( -41.30498680716012672, -13.80019380139175666, 0.8186576791469339920 ) ) ;
#6425 = VERTEX_POINT ( 'NONE', #39816 ) ;
#6426 = DIRECTION ( 'NONE',  ( 0.000000000000000000, -0.000000000000000000, 1.000000000000000000 ) ) ;
#6427 = CARTESIAN_POINT ( 'NONE',  ( 33.00000000000000000, 14.00000000000000000, -79.00402776293826435 ) ) ;
#6428 = VERTEX_POINT ( 'NONE', #50685 ) ;
#6429 = CARTESIAN_POINT ( 'NONE',  ( -65.69292637653380496, 10.01517768586948698, -1.839758294383808571E-15 ) ) ;
#6430 = CARTESIAN_POINT ( 'NONE',  ( 15.00000000000000000, 8.000000000000000000, -4.000000000000000000 ) ) ;
#6431 = EDGE_CURVE ( 'NONE', #29454, #5399, #17656, .T. ) ;
#6432 = DIRECTION ( 'NONE',  ( 1.000000000000000000, 0.000000000000000000, 0.000000000000000000 ) ) ;
#6433 = CARTESIAN_POINT ( 'NONE',  ( -142.0429263765338135, -9.058813317711329915, -2.943386871421370898 ) ) ;
#6434 = CARTESIAN_POINT ( 'NONE',  ( -13.75000000000000533, 30.74999999999999289, -3.750000000000000000 ) ) ;
#6435 = EDGE_CURVE ( 'NONE', #4028, #63980, #10504, .T. ) ;
#6436 = FACE_OUTER_BOUND ( 'NONE', #25939, .T. ) ;
#6437 = STYLED_ITEM ( 'NONE', ( #14336 ), #41280 ) ;
#6438 = EDGE_LOOP ( 'NONE', ( #28847, #35119, #36372, #63117 ) ) ;
#6439 = CARTESIAN_POINT ( 'NONE',  ( -171.6550000000000011, -7.632228543268600340, -2.479861379858950166 ) ) ;
#6440 = ORIENTED_EDGE ( 'NONE', *, *, #32109, .F. ) ;
#6441 = DIRECTION ( 'NONE',  ( -0.000000000000000000, -1.000000000000000000, -0.000000000000000000 ) ) ;
#6442 = DIRECTION ( 'NONE',  ( 0.000000000000000000, 1.000000000000000000, 0.000000000000000000 ) ) ;
#6443 = DIRECTION ( 'NONE',  ( 0.000000000000000000, 0.000000000000000000, 1.000000000000000000 ) ) ;
#6444 = CARTESIAN_POINT ( 'NONE',  ( 1.000000000000000000, 1.000000000000000000, -79.00402776293826435 ) ) ;
#6445 = FILL_AREA_STYLE_COLOUR ( '', #34231 ) ;
#6446 = CARTESIAN_POINT ( 'NONE',  ( 0.000000000000000000, 157.0570736234661524, -8.025000000000000355 ) ) ;
#6447 = ORIENTED_EDGE ( 'NONE', *, *, #24307, .T. ) ;
#6448 = CARTESIAN_POINT ( 'NONE',  ( -80.15499999999998693, 7.632228543268600340, 2.479861379858949277 ) ) ;
#6449 = FACE_OUTER_BOUND ( 'NONE', #7847, .T. ) ;
#6450 = LINE ( 'NONE', #44156, #12717 ) ;
#6451 =( NAMED_UNIT ( * ) PLANE_ANGLE_UNIT ( ) SI_UNIT ( $, .RADIAN. ) );
#6452 = ORIENTED_EDGE ( 'NONE', *, *, #68201, .T. ) ;
#6453 =( LENGTH_UNIT ( ) NAMED_UNIT ( * ) SI_UNIT ( .MILLI., .METRE. ) );
#6454 = ADVANCED_FACE ( 'NONE', ( #3116 ), #35555, .F. ) ;
#6455 = CARTESIAN_POINT ( 'NONE',  ( -61.94499999999998607, -9.827790563157499189E-16, -8.024999999999991473 ) ) ;
#6456 = ORIENTED_EDGE ( 'NONE', *, *, #64984, .T. ) ;
#6457 = FILL_AREA_STYLE_COLOUR ( '', #64911 ) ;
#6458 = CARTESIAN_POINT ( 'NONE',  ( -45.88773363194338373, 9.324829141677650313, -6.185705318536817821 ) ) ;
#6459 = STYLED_ITEM ( 'NONE', ( #7620 ), #67102 ) ;
#6460 = EDGE_LOOP ( 'NONE', ( #15947, #53978, #55917, #25630 ) ) ;
#6461 = CARTESIAN_POINT ( 'NONE',  ( 93.00000000000000000, 14.00000000000000000, 0.000000000000000000 ) ) ;
#6462 = EDGE_LOOP ( 'NONE', ( #9776, #10021, #25729 ) ) ;
#6463 = AXIS2_PLACEMENT_3D ( 'NONE', #35485, #34767, #14357 ) ;
#6464 = CARTESIAN_POINT ( 'NONE',  ( 25.75000000000001066, 21.74999999999998224, 3.750000000000000000 ) ) ;
#6465 = CARTESIAN_POINT ( 'NONE',  ( -74.50000000000000000, 7.768687147774684831, 6.500000000000004441 ) ) ;
#6466 = CARTESIAN_POINT ( 'NONE',  ( -114.2049999999999699, -2.607480562269071545, -8.024999999999991473 ) ) ;
#6467 = ORIENTED_EDGE ( 'NONE', *, *, #24963, .T. ) ;
#6468 = CARTESIAN_POINT ( 'NONE',  ( 12.34222745343792127, 114.9999999999999574, -10.18181818181818166 ) ) ;
#6469 = FILL_AREA_STYLE ('',( #33228 ) ) ;
#6470 = CIRCLE ( 'NONE', #24440, 0.5000000000000004441 ) ;
#6471 = CARTESIAN_POINT ( 'NONE',  ( -151.2570736234661979, 5.598654528085800663, -7.705886871421367523 ) ) ;
#6472 = PRODUCT_DEFINITION_SHAPE ( 'NONE', 'NONE',  #69710 ) ;
#6473 = CARTESIAN_POINT ( 'NONE',  ( 5.598654528085805993, 129.2450000000000045, 7.705886871421374629 ) ) ;
#6474 = CARTESIAN_POINT ( 'NONE',  ( -91.25707362346616947, 5.598654528085800663, -7.705886871421367523 ) ) ;
#6475 = CYLINDRICAL_SURFACE ( 'NONE', #18993, 4.999999999999997335 ) ;
#6476 = ORIENTED_EDGE ( 'NONE', *, *, #34768, .T. ) ;
#6477 = AXIS2_PLACEMENT_3D ( 'NONE', #16063, #9743, #5116 ) ;
#6478 = CARTESIAN_POINT ( 'NONE',  ( -132.9549999999999841, -7.632228543268599452, 2.479861379858951054 ) ) ;
#6479 = DIRECTION ( 'NONE',  ( 0.000000000000000000, 0.000000000000000000, -1.000000000000000000 ) ) ;
#6480 = CARTESIAN_POINT ( 'NONE',  ( -146.0929263765342796, 3.094860106626500240, 9.524999999994133049 ) ) ;
#6481 =( LENGTH_UNIT ( ) NAMED_UNIT ( * ) SI_UNIT ( .MILLI., .METRE. ) );
#6482 = CARTESIAN_POINT ( 'NONE',  ( -143.3949999999999818, -6.826472737025115478, -4.959722759717899443 ) ) ;
#6483 = CARTESIAN_POINT ( 'NONE',  ( -125.9949999999999903, -6.826472737025113702, 4.959722759717902107 ) ) ;
#6484 = ORIENTED_EDGE ( 'NONE', *, *, #68808, .F. ) ;
#6485 = PLANE ( 'NONE',  #8341 ) ;
#6486 = EDGE_CURVE ( 'NONE', #5687, #64812, #56653, .T. ) ;
#6487 = UNCERTAINTY_MEASURE_WITH_UNIT (LENGTH_MEASURE( 1.000000000000000082E-05 ), #51686, 'distance_accuracy_value', 'NONE');
#6488 = CARTESIAN_POINT ( 'NONE',  ( -180.4429263765338192, -1.166476076187852838E-15, -9.524999999999991473 ) ) ;
#6489 =( NAMED_UNIT ( * ) PLANE_ANGLE_UNIT ( ) SI_UNIT ( $, .RADIAN. ) );
#6490 = CARTESIAN_POINT ( 'NONE',  ( -55.04499999999998039, 7.632228543268600340, 2.479861379858949277 ) ) ;
#6491 = EDGE_CURVE ( 'NONE', #28358, #31294, #57700, .T. ) ;
#6492 = CARTESIAN_POINT ( 'NONE',  ( 11.00000000000001954, 17.23130743308432855, -3.198396408832238080E-15 ) ) ;
#6493 = DIRECTION ( 'NONE',  ( 0.000000000000000000, 1.000000000000000000, -0.000000000000000000 ) ) ;
#6494 = CARTESIAN_POINT ( 'NONE',  ( -4.041451884327380562, 2.500000000000000000, -7.000000000000003553 ) ) ;
#6495 = CYLINDRICAL_SURFACE ( 'NONE', #54762, 1.000000000000000888 ) ;
#6496 = CARTESIAN_POINT ( 'NONE',  ( -75.20707362346615810, 3.094860106618433360, 9.524999999999991473 ) ) ;
#6497 = CARTESIAN_POINT ( 'NONE',  ( -93.89292637653379359, -8.102448949553172852, -5.886773742842741797 ) ) ;
#6498 = PRODUCT_CONTEXT ( 'NONE', #13175, 'mechanical' ) ;
#6499 = CARTESIAN_POINT ( 'NONE',  ( 31.00000000000001066, 42.00000000000000000, -4.033029030585349936E-15 ) ) ;
#6500 = DIRECTION ( 'NONE',  ( -1.000000000000000000, -0.000000000000000000, -0.000000000000000000 ) ) ;
#6501 = CARTESIAN_POINT ( 'NONE',  ( 4.750000000000000000, 5.970153145843347347E-16, 1.000000000000000000 ) ) ;
#6502 = DIRECTION ( 'NONE',  ( -0.000000000000000000, -0.000000000000000000, -1.000000000000000000 ) ) ;
#6503 = CIRCLE ( 'NONE', #53669, 5.000000000000004441 ) ;
#6504 = ADVANCED_FACE ( 'NONE', ( #25326 ), #56579, .T. ) ;
#6505 = FACE_OUTER_BOUND ( 'NONE', #3884, .T. ) ;
#6506 = ORIENTED_EDGE ( 'NONE', *, *, #8191, .F. ) ;
#6507 = DIRECTION ( 'NONE',  ( -0.000000000000000000, -1.000000000000000000, -0.000000000000000000 ) ) ;
#6508 = LINE ( 'NONE', #2218, #13783 ) ;
#6509 = ORIENTED_EDGE ( 'NONE', *, *, #19367, .F. ) ;
#6510 = LINE ( 'NONE', #60338, #64495 ) ;
#6511 =( GEOMETRIC_REPRESENTATION_CONTEXT ( 3 ) GLOBAL_UNCERTAINTY_ASSIGNED_CONTEXT ( ( #65034 ) ) GLOBAL_UNIT_ASSIGNED_CONTEXT ( ( #58517, #37474, #10347 ) ) REPRESENTATION_CONTEXT ( 'NONE', 'WORKASPACE' ) );
#6512 = CARTESIAN_POINT ( 'NONE',  ( -9.827790563157511022E-16, 119.5570736234661524, 8.025000000000000355 ) ) ;
#6513 = DIRECTION ( 'NONE',  ( -1.000000000000000000, 0.000000000000000000, 0.000000000000000000 ) ) ;
#6514 = CARTESIAN_POINT ( 'NONE',  ( 75.00000000000000000, 19.90218225813118380, -6.307374275524009200 ) ) ;
#6515 = CARTESIAN_POINT ( 'NONE',  ( -23.21231517720797655, 117.4999999999999716, -7.000000000000000000 ) ) ;
#6516 = ORIENTED_EDGE ( 'NONE', *, *, #30720, .F. ) ;
#6517 = VERTEX_POINT ( 'NONE', #4185 ) ;
#6518 = DIRECTION ( 'NONE',  ( -2.312964634635740689E-15, 1.000000000000000000, 0.000000000000000000 ) ) ;
#6519 = SURFACE_SIDE_STYLE ('',( #65285 ) ) ;
#6520 = ORIENTED_EDGE ( 'NONE', *, *, #20586, .T. ) ;
#6521 = FACE_OUTER_BOUND ( 'NONE', #30175, .T. ) ;
#6522 = CARTESIAN_POINT ( 'NONE',  ( -119.3070736234661808, -10.01517768586948698, 6.132527647946031529E-16 ) ) ;
#6523 = CARTESIAN_POINT ( 'NONE',  ( -60.00000000000000000, -2.024042244987997205E-14, 6.000000000000000888 ) ) ;
#6524 = EDGE_CURVE ( 'NONE', #26545, #42069, #38659, .T. ) ;
#6525 = CARTESIAN_POINT ( 'NONE',  ( -87.29500000000000171, -2.607480562269069768, 8.024999999999991473 ) ) ;
#6526 = EDGE_LOOP ( 'NONE', ( #33985, #69508, #69587, #69521 ) ) ;
#6527 = CARTESIAN_POINT ( 'NONE',  ( -20.05202421861157447, 114.9999999999999432, -10.44839000960907960 ) ) ;
#6528 =( LENGTH_UNIT ( ) NAMED_UNIT ( * ) SI_UNIT ( .MILLI., .METRE. ) );
#6529 = DIRECTION ( 'NONE',  ( 0.000000000000000000, 1.000000000000000000, 0.000000000000000000 ) ) ;
#6530 = UNCERTAINTY_MEASURE_WITH_UNIT (LENGTH_MEASURE( 1.000000000000000082E-05 ), #156, 'distance_accuracy_value', 'NONE');
#6531 = ORIENTED_EDGE ( 'NONE', *, *, #46388, .F. ) ;
#6532 = DIRECTION ( 'NONE',  ( 0.000000000000000000, 1.000000000000000000, -0.000000000000000000 ) ) ;
#6533 = CARTESIAN_POINT ( 'NONE',  ( 57.00000000000000000, 13.00000000000000178, 60.00402776293827145 ) ) ;
#6534 = ORIENTED_EDGE ( 'NONE', *, *, #60276, .F. ) ;
#6535 = DIRECTION ( 'NONE',  ( 1.000000000000000000, 0.000000000000000000, 0.000000000000000000 ) ) ;
#6536 = ORIENTED_EDGE ( 'NONE', *, *, #886, .T. ) ;
#6537 = CARTESIAN_POINT ( 'NONE',  ( -166.1070736234661638, 8.102448949553172852, -5.886773742842744461 ) ) ;
#6538 = DIRECTION ( 'NONE',  ( 0.000000000000000000, 0.000000000000000000, -1.000000000000000000 ) ) ;
#6539 = DIRECTION ( 'NONE',  ( -0.000000000000000000, -0.000000000000000000, -1.000000000000000000 ) ) ;
#6540 = AXIS2_PLACEMENT_3D ( 'NONE', #44742, #6361, #27791 ) ;
#6541 = CARTESIAN_POINT ( 'NONE',  ( -174.5070736234661695, 8.102448949553176405, 5.886773742842740909 ) ) ;
#6542 = DIRECTION ( 'NONE',  ( -1.000000000000000000, 0.000000000000000000, 0.000000000000000000 ) ) ;
#6543 = DIRECTION ( 'NONE',  ( 0.000000000000000000, 1.000000000000000000, 0.000000000000000000 ) ) ;
#6544 = VECTOR ( 'NONE', #531, 1000.000000000000000 ) ;
#6545 = CARTESIAN_POINT ( 'NONE',  ( -68.54292637653379927, 9.058813317711329915, 2.943386871421369566 ) ) ;
#6546 = CARTESIAN_POINT ( 'NONE',  ( -1.518239866961766493, 153.0257666483763330, -7.925161578318726363 ) ) ;
#6547 = ORIENTED_EDGE ( 'NONE', *, *, #56652, .F. ) ;
#6548 = CARTESIAN_POINT ( 'NONE',  ( -71.49999999999998579, 64.07124727947029896, -7.500000000000000000 ) ) ;
#6549 = AXIS2_PLACEMENT_3D ( 'NONE', #40973, #8928, #40613 ) ;
#6550 = DIRECTION ( 'NONE',  ( 0.000000000000000000, 0.000000000000000000, -1.000000000000000000 ) ) ;
#6551 = CARTESIAN_POINT ( 'NONE',  ( -149.0070736234661979, -8.102448949553174629, -5.886773742842741797 ) ) ;
#6552 =( NAMED_UNIT ( * ) SI_UNIT ( $, .STERADIAN. ) SOLID_ANGLE_UNIT ( ) );
#6553 = ORIENTED_EDGE ( 'NONE', *, *, #36067, .F. ) ;
#6554 = CARTESIAN_POINT ( 'NONE',  ( -161.3050000000000068, 8.437984349512085203, -1.550032578732815448E-15 ) ) ;
#6555 = DIRECTION ( 'NONE',  ( 0.000000000000000000, -1.000000000000000000, 0.000000000000000000 ) ) ;
#6556 = FILL_AREA_STYLE_COLOUR ( '', #21196 ) ;
#6557 = EDGE_CURVE ( 'NONE', #11851, #39381, #1490, .T. ) ;
#6558 = CARTESIAN_POINT ( 'NONE',  ( -169.9449999999999932, -9.827790563157499189E-16, -8.024999999999991473 ) ) ;
#6559 = CIRCLE ( 'NONE', #57138, 0.2500000000000002220 ) ;
#6560 = CARTESIAN_POINT ( 'NONE',  ( -159.7450000000000045, 4.716976649647094177, 6.492361379858945902 ) ) ;
#6561 = AXIS2_PLACEMENT_3D ( 'NONE', #23854, #18595, #9080 ) ;
#6562 = VERTEX_POINT ( 'NONE', #20395 ) ;
#6563 = CIRCLE ( 'NONE', #45934, 0.2500000000000002220 ) ;
#6564 = CARTESIAN_POINT ( 'NONE',  ( -89.39292637653379359, 8.102448949553176405, 5.886773742842740909 ) ) ;
#6565 = FILL_AREA_STYLE ('',( #23450 ) ) ;
#6566 = FACE_OUTER_BOUND ( 'NONE', #9078, .T. ) ;
#6567 = CARTESIAN_POINT ( 'NONE',  ( -69.80499999999996419, -8.437984349512085203, 5.166775262442717831E-16 ) ) ;
#6568 = CARTESIAN_POINT ( 'NONE',  ( -36.30021781998517127, -10.34894320149787816, 4.110481005326708015 ) ) ;
#6570 = FILL_AREA_STYLE ('',( #54756 ) ) ;
#6569 = PRESENTATION_LAYER_ASSIGNMENT (  '', '', ( #20038 ) ) ;
#6571 = ADVANCED_FACE ( 'NONE', ( #4550 ), #19368, .F. ) ;
#6572 = CARTESIAN_POINT ( 'NONE',  ( -70.49499999999996191, 6.826472737025113702, -4.959722759717902107 ) ) ;
#6573 = CARTESIAN_POINT ( 'NONE',  ( 8.102448949553181734, 133.5049999999999670, 5.886773742842750679 ) ) ;
#6574 = CARTESIAN_POINT ( 'NONE',  ( 10.00000000000001776, 43.00000000000000000, -28.00000000000000000 ) ) ;
#6575 = EDGE_CURVE ( 'NONE', #10734, #34321, #6202, .T. ) ;
#6576 = CARTESIAN_POINT ( 'NONE',  ( -177.1429263765338078, 5.598654528085800663, -7.705886871421367523 ) ) ;
#6577 = UNCERTAINTY_MEASURE_WITH_UNIT (LENGTH_MEASURE( 1.000000000000000082E-05 ), #46786, 'distance_accuracy_value', 'NONE');
#6578 = FACE_OUTER_BOUND ( 'NONE', #58655, .T. ) ;
#6579 = DIRECTION ( 'NONE',  ( 0.000000000000000000, 0.000000000000000000, 1.000000000000000000 ) ) ;
#6580 = VERTEX_POINT ( 'NONE', #42945 ) ;
#6581 = EDGE_CURVE ( 'NONE', #62171, #45281, #35248, .T. ) ;
#6582 = DIRECTION ( 'NONE',  ( 1.000000000000000000, 0.000000000000000000, 0.000000000000000000 ) ) ;
#6583 = EDGE_CURVE ( 'NONE', #67626, #12224, #46344, .T. ) ;
#6584 = AXIS2_PLACEMENT_3D ( 'NONE', #60726, #7619, #24477 ) ;
#6585 = SURFACE_STYLE_FILL_AREA ( #17544 ) ;
#6586 = DIRECTION ( 'NONE',  ( 0.000000000000000000, 0.000000000000000000, 1.000000000000000000 ) ) ;
#6587 = VERTEX_POINT ( 'NONE', #31986 ) ;
#6588 = CIRCLE ( 'NONE', #26815, 1.000000000000000888 ) ;
#6589 = VERTEX_POINT ( 'NONE', #15840 ) ;
#6590 = DIRECTION ( 'NONE',  ( 1.000000000000000000, 0.000000000000000000, 0.000000000000000000 ) ) ;
#6591 = COLOUR_RGB ( '', 0.40784314, 0.44705882, 0.49803922) ;
#6592 = CARTESIAN_POINT ( 'NONE',  ( -6.062177826491071286, 3.500000000000000888, 0.000000000000000000 ) ) ;
#6593 = CARTESIAN_POINT ( 'NONE',  ( 2.999999999999994671, 0.000000000000000000, -24.00402776293822527 ) ) ;
#6594 =( BOUNDED_SURFACE ( )  B_SPLINE_SURFACE ( 3, 2, ( 
 ( #20054, #36295, #61929 ),
 ( #58072, #3865, #25349 ),
 ( #41220, #36652, #35217 ),
 ( #4570, #30609, #19370 ),
 ( #51754, #46508, #52112 ),
 ( #68620, #24999, #52461 ),
 ( #40518, #29931, #47199 ),
 ( #19008, #14115, #51393 ) ),
 .UNSPECIFIED., .F., .F., .F. ) 
 B_SPLINE_SURFACE_WITH_KNOTS ( ( 4, 2, 2, 4 ),
 ( 3, 3 ),
 ( 3.931838538365182600, 4.126976148870059369, 4.322113759374936137, 4.712388980384689674 ),
 ( 0.000000000000000000, 1.000000000000000000 ),
 .UNSPECIFIED. ) 
 GEOMETRIC_REPRESENTATION_ITEM ( )  RATIONAL_B_SPLINE_SURFACE ( (
 ( 1.000000000000000000, 0.8674236696762896992, 1.000000000000000000),
 ( 1.000000000000000000, 0.8861805033181393565, 1.000000000000000000),
 ( 1.000000000000000000, 0.9042436661781160234, 1.000000000000000000),
 ( 1.000000000000000000, 0.9367862960115010962, 1.000000000000000000),
 ( 1.000000000000000000, 0.9512556414921075065, 1.000000000000000000),
 ( 1.000000000000000000, 0.9868976895439577346, 1.000000000000000000),
 ( 1.000000000000000000, 1.000154660590251154, 1.000000000000000000),
 ( 1.000000000000000000, 1.000000000000000000, 1.000000000000000000) ) ) 
 REPRESENTATION_ITEM ( '' )  SURFACE ( )  );
#6595 =( GEOMETRIC_REPRESENTATION_CONTEXT ( 3 ) GLOBAL_UNCERTAINTY_ASSIGNED_CONTEXT ( ( #44548 ) ) GLOBAL_UNIT_ASSIGNED_CONTEXT ( ( #10763, #63530, #69167 ) ) REPRESENTATION_CONTEXT ( 'NONE', 'WORKASPACE' ) );
#6597 = CARTESIAN_POINT ( 'NONE',  ( -69.35707362346617799, 5.598654528085804216, 7.705886871421366635 ) ) ;
#6596 = MECHANICAL_DESIGN_GEOMETRIC_PRESENTATION_REPRESENTATION (  '', ( #65001 ), #38113 ) ;
#6598 = ORIENTED_EDGE ( 'NONE', *, *, #39046, .F. ) ;
#6599 = CARTESIAN_POINT ( 'NONE',  ( -114.2049999999999699, -2.607480562269071545, -8.024999999999991473 ) ) ;
#6600 = ORIENTED_EDGE ( 'NONE', *, *, #2516, .T. ) ;
#6601 = FACE_OUTER_BOUND ( 'NONE', #45853, .T. ) ;
#6602 = FILL_AREA_STYLE_COLOUR ( '', #46772 ) ;
#6603 = ORIENTED_EDGE ( 'NONE', *, *, #56069, .F. ) ;
#6604 = CARTESIAN_POINT ( 'NONE',  ( 43.75000000000000000, 18.99999999999998224, -3.750000000000000000 ) ) ;
#6605 = ORIENTED_EDGE ( 'NONE', *, *, #67628, .T. ) ;
#6606 = CARTESIAN_POINT ( 'NONE',  ( -8.102448949553181734, 158.4950000000000045, 5.886773742842747126 ) ) ;
#6607 = VERTEX_POINT ( 'NONE', #5579 ) ;
#6608 =( GEOMETRIC_REPRESENTATION_CONTEXT ( 3 ) GLOBAL_UNCERTAINTY_ASSIGNED_CONTEXT ( ( #4792 ) ) GLOBAL_UNIT_ASSIGNED_CONTEXT ( ( #53570, #48006, #26131 ) ) REPRESENTATION_CONTEXT ( 'NONE', 'WORKASPACE' ) );
#6609 = EDGE_LOOP ( 'NONE', ( #43291, #37212, #3983, #55136 ) ) ;
#6610 = CARTESIAN_POINT ( 'NONE',  ( 31.00000000000002132, 43.00000000000000000, 79.00402776293826435 ) ) ;
#6611 = CYLINDRICAL_SURFACE ( 'NONE', #61986, 0.5000000000000004441 ) ;
#6612 = CARTESIAN_POINT ( 'NONE',  ( -152.4570736234661581, -9.058813317711329915, 2.943386871421371787 ) ) ;
#6613 = DIRECTION ( 'NONE',  ( 0.000000000000000000, 0.000000000000000000, 1.000000000000000000 ) ) ;
#6614 = ORIENTED_EDGE ( 'NONE', *, *, #38592, .T. ) ;
#6615 = CARTESIAN_POINT ( 'NONE',  ( -4.716976649647098618, 136.1429263765338362, 6.492361379858953008 ) ) ;
#6616 = DIRECTION ( 'NONE',  ( 0.000000000000000000, 1.000000000000000000, 0.000000000000000000 ) ) ;
#6617 = DIRECTION ( 'NONE',  ( -1.300977106640434891E-16, 0.000000000000000000, -1.000000000000000000 ) ) ;
#6618 = CIRCLE ( 'NONE', #39217, 0.2500000000000002220 ) ;
#6619 = CARTESIAN_POINT ( 'NONE',  ( 7.632228543268607446, 125.0429263765337993, 2.479861379858954606 ) ) ;
#6620 = DIRECTION ( 'NONE',  ( 0.000000000000000000, 0.000000000000000000, -1.000000000000000000 ) ) ;
#6621 = ORIENTED_EDGE ( 'NONE', *, *, #67944, .T. ) ;
#6622 = SURFACE_STYLE_USAGE ( .BOTH. , #38364 ) ;
#6623 = ORIENTED_EDGE ( 'NONE', *, *, #61298, .F. ) ;
#6624 = FILL_AREA_STYLE_COLOUR ( '', #58508 ) ;
#6625 = CARTESIAN_POINT ( 'NONE',  ( 12.75000000000000533, 28.24999999999998224, -3.750000000000000000 ) ) ;
#6626 = DIRECTION ( 'NONE',  ( -1.000000000000000000, 0.000000000000000000, 0.000000000000000000 ) ) ;
#6627 = DIRECTION ( 'NONE',  ( -1.000000000000000000, -0.000000000000000000, -0.000000000000000000 ) ) ;
#6628 = CARTESIAN_POINT ( 'NONE',  ( -145.5549999999999784, 0.000000000000000000, 8.024999999999991473 ) ) ;
#6629 =( LENGTH_UNIT ( ) NAMED_UNIT ( * ) SI_UNIT ( .MILLI., .METRE. ) );
#6630 = UNCERTAINTY_MEASURE_WITH_UNIT (LENGTH_MEASURE( 1.000000000000000082E-05 ), #24819, 'distance_accuracy_value', 'NONE');
#6631 = VERTEX_POINT ( 'NONE', #26007 ) ;
#6632 = MECHANICAL_DESIGN_GEOMETRIC_PRESENTATION_REPRESENTATION (  '', ( #50498 ), #13423 ) ;
#6633 = CARTESIAN_POINT ( 'NONE',  ( -8.437984349512095861, 115.8070736234661524, -5.166775262442723748E-16 ) ) ;
#6634 = LINE ( 'NONE', #60793, #63116 ) ;
#6635 = CARTESIAN_POINT ( 'NONE',  ( 53.24999999999999289, 27.74999999999998579, -3.750000000000000000 ) ) ;
#6636 = ORIENTED_EDGE ( 'NONE', *, *, #65931, .F. ) ;
#6637 = ORIENTED_EDGE ( 'NONE', *, *, #44912, .F. ) ;
#6638 = DIRECTION ( 'NONE',  ( -0.000000000000000000, -0.000000000000000000, 1.000000000000000000 ) ) ;
#6639 =( LENGTH_UNIT ( ) NAMED_UNIT ( * ) SI_UNIT ( .MILLI., .METRE. ) );
#6640 = CARTESIAN_POINT ( 'NONE',  ( -60.05499999999998550, -9.827790563157499189E-16, -8.024999999999991473 ) ) ;
#6641 = ORIENTED_EDGE ( 'NONE', *, *, #13907, .F. ) ;
#6642 = LINE ( 'NONE', #49948, #29187 ) ;
#6643 = DIRECTION ( 'NONE',  ( 3.717264591378879477E-17, 0.000000000000000000, -1.000000000000000000 ) ) ;
#6644 = CARTESIAN_POINT ( 'NONE',  ( 7.500000000000000000, 9.184850993605147944E-16, 1.000000000000000000 ) ) ;
#6645 =( NAMED_UNIT ( * ) SI_UNIT ( $, .STERADIAN. ) SOLID_ANGLE_UNIT ( ) );
#6646 = EDGE_CURVE ( 'NONE', #24031, #35855, #58854, .T. ) ;
#6647 =( GEOMETRIC_REPRESENTATION_CONTEXT ( 3 ) GLOBAL_UNCERTAINTY_ASSIGNED_CONTEXT ( ( #64520 ) ) GLOBAL_UNIT_ASSIGNED_CONTEXT ( ( #33249, #59615, #26890 ) ) REPRESENTATION_CONTEXT ( 'NONE', 'WORKASPACE' ) );
#6648 =( LENGTH_UNIT ( ) NAMED_UNIT ( * ) SI_UNIT ( .MILLI., .METRE. ) );
#6649 = AXIS2_PLACEMENT_3D ( 'NONE', #21948, #21222, #15998 ) ;
#6650 = DIRECTION ( 'NONE',  ( -0.000000000000000000, 3.471511484687326312E-15, 1.000000000000000000 ) ) ;
#6651 = AXIS2_PLACEMENT_3D ( 'NONE', #50442, #7863, #24051 ) ;
#6653 = ADVANCED_FACE ( 'NONE', ( #47536 ), #43183, .T. ) ;
#6652 = VERTEX_POINT ( 'NONE', #63655 ) ;
#6654 = VECTOR ( 'NONE', #45603, 1000.000000000000000 ) ;
#6655 = EDGE_CURVE ( 'NONE', #66133, #66860, #38354, .T. ) ;
#6656 = CARTESIAN_POINT ( 'NONE',  ( -84.49999999999998579, -3.499999999999999556, 0.000000000000000000 ) ) ;
#6657 = CARTESIAN_POINT ( 'NONE',  ( -12.72792206135785698, 149.9999999999999716, -10.50000000000000000 ) ) ;
#6658 = CARTESIAN_POINT ( 'NONE',  ( 30.99999999999998579, 5.000000000000000000, 72.00402776293822171 ) ) ;
#6659 = LINE ( 'NONE', #54516, #38165 ) ;
#6660 = STYLED_ITEM ( 'NONE', ( #24945 ), #51466 ) ;
#6661 = CYLINDRICAL_SURFACE ( 'NONE', #3362, 0.5000000000000004441 ) ;
#6662 = EDGE_CURVE ( 'NONE', #29216, #25731, #58376, .T. ) ;
#6663 = EDGE_CURVE ( 'NONE', #45281, #62171, #36407, .T. ) ;
#6664 = CARTESIAN_POINT ( 'NONE',  ( -108.8949999999999960, 6.826472737025115478, 4.959722759717899443 ) ) ;
#6665 = CARTESIAN_POINT ( 'NONE',  ( 9.058813317711337021, 159.5449999999999875, 2.943386871421375783 ) ) ;
#6666 = CARTESIAN_POINT ( 'NONE',  ( -74.39499999999999602, -6.826472737025115478, -4.959722759717899443 ) ) ;
#6667 = EDGE_CURVE ( 'NONE', #60866, #29393, #28484, .T. ) ;
#6668 = CARTESIAN_POINT ( 'NONE',  ( -2.607480562269048896, 113.4070736234661467, 8.025000000000019895 ) ) ;
#6669 =( LENGTH_UNIT ( ) NAMED_UNIT ( * ) SI_UNIT ( .MILLI., .METRE. ) );
#6670 = ADVANCED_FACE ( 'NONE', ( #16193 ), #26685, .T. ) ;
#6671 = LINE ( 'NONE', #39086, #8119 ) ;
#6672 = UNCERTAINTY_MEASURE_WITH_UNIT (LENGTH_MEASURE( 1.000000000000000082E-05 ), #60024, 'distance_accuracy_value', 'NONE');
#6673 = VECTOR ( 'NONE', #9576, 1000.000000000000000 ) ;
#6674 =( NAMED_UNIT ( * ) PLANE_ANGLE_UNIT ( ) SI_UNIT ( $, .RADIAN. ) );
#6675 = CARTESIAN_POINT ( 'NONE',  ( 44.99999999999977973, 146.9999999999999716, 9.500000000000000000 ) ) ;
#6676 = ORIENTED_EDGE ( 'NONE', *, *, #8296, .F. ) ;
#6677 = EDGE_CURVE ( 'NONE', #68888, #35268, #51243, .T. ) ;
#6678 = CARTESIAN_POINT ( 'NONE',  ( -121.4929263765337879, -8.102448949553172852, 5.886773742842742685 ) ) ;
#6679 =( NAMED_UNIT ( * ) SI_UNIT ( $, .STERADIAN. ) SOLID_ANGLE_UNIT ( ) );
#6680 = CARTESIAN_POINT ( 'NONE',  ( -141.5950000000000273, 2.607480562269073321, 8.024999999999991473 ) ) ;
#6681 =( NAMED_UNIT ( * ) SI_UNIT ( $, .STERADIAN. ) SOLID_ANGLE_UNIT ( ) );
#6682 = TOROIDAL_SURFACE ( 'NONE', #23499, 1.000000000000000000, 0.5000000000000000000 ) ;
#6683 = DIRECTION ( 'NONE',  ( -0.000000000000000000, -1.000000000000000000, -0.000000000000000000 ) ) ;
#6684 = SURFACE_STYLE_FILL_AREA ( #53513 ) ;
#6685 = ORIENTED_EDGE ( 'NONE', *, *, #43497, .F. ) ;
#6686 = VERTEX_POINT ( 'NONE', #13282 ) ;
#6687 = MECHANICAL_DESIGN_GEOMETRIC_PRESENTATION_REPRESENTATION (  '', ( #19032 ), #34754 ) ;
#6688 = AXIS2_PLACEMENT_3D ( 'NONE', #29751, #67736, #19533 ) ;
#6689 = DIRECTION ( 'NONE',  ( 0.000000000000000000, -1.000000000000000000, 0.000000000000000000 ) ) ;
#6690 = LINE ( 'NONE', #50318, #11727 ) ;
#6691 = TOROIDAL_SURFACE ( 'NONE', #57262, 0.5000000000000000000, 0.2500000000000000000 ) ;
#6692 = DIRECTION ( 'NONE',  ( 0.000000000000000000, 1.000000000000000000, 0.000000000000000000 ) ) ;
#6693 = DIRECTION ( 'NONE',  ( 1.000000000000000000, 0.000000000000000000, 0.000000000000000000 ) ) ;
#6694 = AXIS2_PLACEMENT_3D ( 'NONE', #66267, #39233, #56409 ) ;
#6695 = CARTESIAN_POINT ( 'NONE',  ( -150.5929263765342512, -3.094860106625624052, -9.524999999994767208 ) ) ;
#6696 = ORIENTED_EDGE ( 'NONE', *, *, #35648, .T. ) ;
#6697 = CARTESIAN_POINT ( 'NONE',  ( -140.1550000000000011, 7.632228543268600340, 2.479861379858949277 ) ) ;
#6698 = ORIENTED_EDGE ( 'NONE', *, *, #37794, .T. ) ;
#6699 = ORIENTED_EDGE ( 'NONE', *, *, #69661, .F. ) ;
#6700 = DIRECTION ( 'NONE',  ( 1.000000000000000000, 0.000000000000000000, -0.000000000000000000 ) ) ;
#6701 = CARTESIAN_POINT ( 'NONE',  ( 60.00000000000000000, 1.797044900979284448E-15, 12.00000000000000000 ) ) ;
#6702 = ORIENTED_EDGE ( 'NONE', *, *, #25110, .T. ) ;
#6703 = AXIS2_PLACEMENT_3D ( 'NONE', #40464, #61882, #56620 ) ;
#6704 = PRESENTATION_LAYER_ASSIGNMENT (  '', '', ( #43818 ) ) ;
#6705 = PRESENTATION_STYLE_ASSIGNMENT (( #1386 ) ) ;
#6706 = PRESENTATION_LAYER_ASSIGNMENT (  '', '', ( #53908 ) ) ;
#6707 = CARTESIAN_POINT ( 'NONE',  ( 3.094860106618435136, 127.2949999999999875, -9.525000000000000355 ) ) ;
#6708 = CARTESIAN_POINT ( 'NONE',  ( 179.4098300562505415, 0.000000000000000000, 0.000000000000000000 ) ) ;
#6709 = EDGE_CURVE ( 'NONE', #11138, #44728, #12790, .T. ) ;
#6710 = ORIENTED_EDGE ( 'NONE', *, *, #48274, .F. ) ;
#6711 = CARTESIAN_POINT ( 'NONE',  ( -94.55707362346616662, -1.166476076187852838E-15, -9.524999999999991473 ) ) ;
#6712 = CARTESIAN_POINT ( 'NONE',  ( 0.000000000000000000, 128.5549999999999784, -9.525000000000000355 ) ) ;
#6713 = CARTESIAN_POINT ( 'NONE',  ( -59.60499999999998977, 6.826472737025113702, -4.959722759717902107 ) ) ;
#6714 = STYLED_ITEM ( 'NONE', ( #68356 ), #41731 ) ;
#6715 = DIRECTION ( 'NONE',  ( 0.000000000000000000, 0.000000000000000000, 1.000000000000000000 ) ) ;
#6716 = ORIENTED_EDGE ( 'NONE', *, *, #22736, .T. ) ;
#6717 = CARTESIAN_POINT ( 'NONE',  ( -10.01517768586949231, 159.3049999999999784, -6.132527647946036459E-16 ) ) ;
#6718 = UNCERTAINTY_MEASURE_WITH_UNIT (LENGTH_MEASURE( 1.000000000000000082E-05 ), #26995, 'distance_accuracy_value', 'NONE');
#6719 = SURFACE_STYLE_USAGE ( .BOTH. , #6038 ) ;
#6720 = DIRECTION ( 'NONE',  ( 0.000000000000000000, -1.000000000000000000, 0.000000000000000000 ) ) ;
#6721 =( NAMED_UNIT ( * ) SI_UNIT ( $, .STERADIAN. ) SOLID_ANGLE_UNIT ( ) );
#6722 = ORIENTED_EDGE ( 'NONE', *, *, #33756, .T. ) ;
#6723 =( NAMED_UNIT ( * ) PLANE_ANGLE_UNIT ( ) SI_UNIT ( $, .RADIAN. ) );
#6724 = VERTEX_POINT ( 'NONE', #65388 ) ;
#6725 = MECHANICAL_DESIGN_GEOMETRIC_PRESENTATION_REPRESENTATION (  '', ( #23545 ), #26885 ) ;
#6726 = DIRECTION ( 'NONE',  ( -1.000000000000000000, 0.000000000000000000, 0.000000000000000000 ) ) ;
#6727 = FACE_OUTER_BOUND ( 'NONE', #35001, .T. ) ;
#6728 = CARTESIAN_POINT ( 'NONE',  ( -171.5049999999999386, -6.826472737025115478, -4.959722759717899443 ) ) ;
#6729 = VERTEX_POINT ( 'NONE', #6288 ) ;
#6730 = PRESENTATION_STYLE_ASSIGNMENT (( #23273 ) ) ;
#6731 = UNCERTAINTY_MEASURE_WITH_UNIT (LENGTH_MEASURE( 1.000000000000000082E-05 ), #25907, 'distance_accuracy_value', 'NONE');
#6732 = STYLED_ITEM ( 'NONE', ( #17623 ), #16349 ) ;
#6733 =( GEOMETRIC_REPRESENTATION_CONTEXT ( 3 ) GLOBAL_UNCERTAINTY_ASSIGNED_CONTEXT ( ( #12130 ) ) GLOBAL_UNIT_ASSIGNED_CONTEXT ( ( #39093, #44723, #33092 ) ) REPRESENTATION_CONTEXT ( 'NONE', 'WORKASPACE' ) );
#6734 = SURFACE_SIDE_STYLE ('',( #65129 ) ) ;
#6735 = CYLINDRICAL_SURFACE ( 'NONE', #24849, 5.000000000000000000 ) ;
#6736 = CARTESIAN_POINT ( 'NONE',  ( -44.99680003617404367, 9.646670402630480368, 3.411693126523581032 ) ) ;
#6737 = ORIENTED_EDGE ( 'NONE', *, *, #34556, .T. ) ;
#6738 = ORIENTED_EDGE ( 'NONE', *, *, #60732, .T. ) ;
#6739 = CARTESIAN_POINT ( 'NONE',  ( -44.99626347754794153, 9.641092568915874850, -3.381901693660977593 ) ) ;
#6740 = CARTESIAN_POINT ( 'NONE',  ( -6.021969435454500363, 1.863712308906140258, 7.569642976165947168 ) ) ;
#6741 = CARTESIAN_POINT ( 'NONE',  ( -88.40499999999997272, -2.607480562269069768, 8.024999999999991473 ) ) ;
#6742 = VERTEX_POINT ( 'NONE', #1973 ) ;
#6743 = EDGE_CURVE ( 'NONE', #60681, #25577, #30057, .T. ) ;
#6744 = CARTESIAN_POINT ( 'NONE',  ( 8.437984349512095861, 144.3070736234661524, 1.550032578732816828E-15 ) ) ;
#6745 = CARTESIAN_POINT ( 'NONE',  ( -52.25707362346618368, 5.598654528085800663, -7.705886871421367523 ) ) ;
#6746 = ADVANCED_FACE ( 'NONE', ( #12593 ), #52148, .T. ) ;
#6747 =( BOUNDED_CURVE ( )  B_SPLINE_CURVE ( 2, ( #63740, #15588, #47985 ),
 .UNSPECIFIED., .F., .F. ) 
 B_SPLINE_CURVE_WITH_KNOTS ( ( 3, 3 ),
 ( 0.9891304347826086474, 0.9913043478260870067 ),
 .UNSPECIFIED. ) 
 CURVE ( )  GEOMETRIC_REPRESENTATION_ITEM ( )  RATIONAL_B_SPLINE_CURVE ( ( 1.000000000000000000, 0.9510565162951535312, 1.000000000000000000 ) ) 
 REPRESENTATION_ITEM ( '' )  );
#6748 = CIRCLE ( 'NONE', #48373, 2.000000000000003553 ) ;
#6749 = ORIENTED_EDGE ( 'NONE', *, *, #48408, .T. ) ;
#6750 = DIRECTION ( 'NONE',  ( -1.000000000000000000, 0.000000000000000000, 0.000000000000000000 ) ) ;
#6752 = FACE_OUTER_BOUND ( 'NONE', #48800, .T. ) ;
#6751 = DIRECTION ( 'NONE',  ( 1.000000000000000000, 0.000000000000000000, 0.000000000000000000 ) ) ;
#6753 = CARTESIAN_POINT ( 'NONE',  ( -8.102448949553181734, 124.8949999999999960, -5.886773742842749790 ) ) ;
#6754 = CARTESIAN_POINT ( 'NONE',  ( -103.0449999999999875, 7.632228543268600340, 2.479861379858949277 ) ) ;
#6755 = AXIS2_PLACEMENT_3D ( 'NONE', #4157, #21061, #42557 ) ;
#6756 = EDGE_CURVE ( 'NONE', #13502, #24967, #54803, .T. ) ;
#6757 = SURFACE_SIDE_STYLE ('',( #17361 ) ) ;
#6758 = CIRCLE ( 'NONE', #69684, 0.2500000000000002220 ) ;
#6760 = CARTESIAN_POINT ( 'NONE',  ( -15.00000000000000000, 10.90871211463571200, -5.000000000000000000 ) ) ;
#6759 = CARTESIAN_POINT ( 'NONE',  ( 21.50000000000001066, 24.74999999999998224, 3.750000000000000000 ) ) ;
#6761 = EDGE_CURVE ( 'NONE', #13621, #18297, #2806, .T. ) ;
#6762 = CARTESIAN_POINT ( 'NONE',  ( -154.1929263765338192, -10.01517768586948698, 6.132527647946031529E-16 ) ) ;
#6763 =( NAMED_UNIT ( * ) SI_UNIT ( $, .STERADIAN. ) SOLID_ANGLE_UNIT ( ) );
#6764 = CARTESIAN_POINT ( 'NONE',  ( -180.1450000000000102, -4.716976649647092401, 6.492361379858946790 ) ) ;
#6765 = AXIS2_PLACEMENT_3D ( 'NONE', #28994, #1541, #54699 ) ;
#6766 = CYLINDRICAL_SURFACE ( 'NONE', #39995, 6.000000000000005329 ) ;
#6767 = MECHANICAL_DESIGN_GEOMETRIC_PRESENTATION_REPRESENTATION (  '', ( #68557 ), #65165 ) ;
#6768 =( GEOMETRIC_REPRESENTATION_CONTEXT ( 3 ) GLOBAL_UNCERTAINTY_ASSIGNED_CONTEXT ( ( #38373 ) ) GLOBAL_UNIT_ASSIGNED_CONTEXT ( ( #61862, #35505, #51680 ) ) REPRESENTATION_CONTEXT ( 'NONE', 'WORKASPACE' ) );
#6769 = CARTESIAN_POINT ( 'NONE',  ( 4.041451884327376121, 7.000000000000007105, 7.500000000000000000 ) ) ;
#6770 = ORIENTED_EDGE ( 'NONE', *, *, #38267, .T. ) ;
#6771 = CARTESIAN_POINT ( 'NONE',  ( 26.25000000000001066, 19.24999999999997868, 3.750000000000000000 ) ) ;
#6772 = ORIENTED_EDGE ( 'NONE', *, *, #40622, .F. ) ;
#6773 = CARTESIAN_POINT ( 'NONE',  ( -64.94292637653380496, 0.000000000000000000, 9.524999999999991473 ) ) ;
#6774 = AXIS2_PLACEMENT_3D ( 'NONE', #37977, #15802, #36603 ) ;
#6775 = DIRECTION ( 'NONE',  ( 0.000000000000000000, 1.000000000000000000, 0.000000000000000000 ) ) ;
#6776 = FACE_OUTER_BOUND ( 'NONE', #64276, .T. ) ;
#6777 = PRODUCT_DEFINITION_FORMATION_WITH_SPECIFIED_SOURCE ( 'ANY', '', #32191, .NOT_KNOWN. ) ;
#6778 = DIRECTION ( 'NONE',  ( -0.000000000000000000, -1.000000000000000000, -0.000000000000000000 ) ) ;
#6779 = CARTESIAN_POINT ( 'NONE',  ( 44.91886116991580735, 9.999999999999980460, -3.201362207699240514 ) ) ;
#6780 = CIRCLE ( 'NONE', #67435, 4.999999999999997335 ) ;
#6781 = PLANE ( 'NONE',  #10602 ) ;
#6782 = ORIENTED_EDGE ( 'NONE', *, *, #66531, .F. ) ;
#6783 = CARTESIAN_POINT ( 'NONE',  ( -171.2049999999999557, -2.607480562269071545, -8.024999999999991473 ) ) ;
#6784 = EDGE_LOOP ( 'NONE', ( #59652, #48217, #48883, #67476, #11572, #20565, #68242, #39945 ) ) ;
#6785 = CARTESIAN_POINT ( 'NONE',  ( -112.1929263765338050, -10.01517768586948698, 6.132527647946031529E-16 ) ) ;
#6786 = DIRECTION ( 'NONE',  ( 0.000000000000000000, 0.000000000000000000, 1.000000000000000000 ) ) ;
#6787 = CIRCLE ( 'NONE', #3379, 3.100000000000001865 ) ;
#6788 =( NAMED_UNIT ( * ) PLANE_ANGLE_UNIT ( ) SI_UNIT ( $, .RADIAN. ) );
#6789 = CARTESIAN_POINT ( 'NONE',  ( -7.632228543268607446, 154.6570736234661467, -2.479861379858953718 ) ) ;
#6790 = ADVANCED_FACE ( 'NONE', ( #7342 ), #7665, .T. ) ;
#6791 = ORIENTED_EDGE ( 'NONE', *, *, #16162, .F. ) ;
#6792 = CIRCLE ( 'NONE', #39432, 9.000000000000000000 ) ;
#6793 = CARTESIAN_POINT ( 'NONE',  ( 6.826472737025121695, 137.4929263765338305, -4.959722759717905660 ) ) ;
#6794 =( GEOMETRIC_REPRESENTATION_CONTEXT ( 3 ) GLOBAL_UNCERTAINTY_ASSIGNED_CONTEXT ( ( #23611 ) ) GLOBAL_UNIT_ASSIGNED_CONTEXT ( ( #42378, #58501, #31751 ) ) REPRESENTATION_CONTEXT ( 'NONE', 'WORKASPACE' ) );
#6795 = CARTESIAN_POINT ( 'NONE',  ( -80.75499999999999545, 4.716976649647091513, -6.492361379858946790 ) ) ;
#6796 = UNCERTAINTY_MEASURE_WITH_UNIT (LENGTH_MEASURE( 1.000000000000000082E-05 ), #39712, 'distance_accuracy_value', 'NONE');
#6797 = FACE_OUTER_BOUND ( 'NONE', #43811, .T. ) ;
#6798 = CARTESIAN_POINT ( 'NONE',  ( -73.55707362346616662, -1.166476076187852838E-15, -9.524999999999991473 ) ) ;
#6799 = CARTESIAN_POINT ( 'NONE',  ( 93.00000000000000000, 5.000000000000000000, 0.000000000000000000 ) ) ;
#6800 = CARTESIAN_POINT ( 'NONE',  ( 13.25000000000000355, 27.74999999999998934, 4.000000000000000000 ) ) ;
#6801 = STYLED_ITEM ( 'NONE', ( #33522 ), #21316 ) ;
#6802 = DIRECTION ( 'NONE',  ( 1.300977106640434891E-16, -0.000000000000000000, 1.000000000000000000 ) ) ;
#6803 = ORIENTED_EDGE ( 'NONE', *, *, #63688, .F. ) ;
#6804 = CARTESIAN_POINT ( 'NONE',  ( -139.5570736234661808, -1.166476076187852838E-15, -9.524999999999991473 ) ) ;
#6805 = SURFACE_SIDE_STYLE ('',( #27558 ) ) ;
#6806 = CARTESIAN_POINT ( 'NONE',  ( -58.64499999999998892, 4.716976649647091513, -6.492361379858946790 ) ) ;
#6808 = ORIENTED_EDGE ( 'NONE', *, *, #64963, .T. ) ;
#6807 = VECTOR ( 'NONE', #9761, 1000.000000000000000 ) ;
#6809 = LINE ( 'NONE', #50101, #1938 ) ;
#6810 = CARTESIAN_POINT ( 'NONE',  ( -45.91398438485168043, 9.424559774107503785, -6.049830996511076364 ) ) ;
#6811 = ORIENTED_EDGE ( 'NONE', *, *, #38759, .F. ) ;
#6812 = SURFACE_STYLE_USAGE ( .BOTH. , #10724 ) ;
#6813 = DIRECTION ( 'NONE',  ( 0.7071067811865543451, 8.659560562355015442E-17, -0.7071067811865408004 ) ) ;
#6814 = PRESENTATION_LAYER_ASSIGNMENT (  '', '', ( #67477 ) ) ;
#6815 = ORIENTED_EDGE ( 'NONE', *, *, #40354, .T. ) ;
#6816 = ADVANCED_FACE ( 'NONE', ( #34738 ), #50254, .F. ) ;
#6817 = CARTESIAN_POINT ( 'NONE',  ( -74.33468449153457414, 8.455116999143504231, 6.464599779185707717 ) ) ;
#6818 = CARTESIAN_POINT ( 'NONE',  ( -110.4549999999999841, 7.632228543268599452, -2.479861379858951942 ) ) ;
#6819 = EDGE_LOOP ( 'NONE', ( #3535, #44575, #10526, #62835 ) ) ;
#6820 = EDGE_CURVE ( 'NONE', #54496, #39359, #44329, .T. ) ;
#6821 = LINE ( 'NONE', #53040, #54178 ) ;
#6822 = CARTESIAN_POINT ( 'NONE',  ( 32.00000000000000711, 42.24279663153597397, -45.14569480374318289 ) ) ;
#6823 = AXIS2_PLACEMENT_3D ( 'NONE', #44358, #50970, #22508 ) ;
#6824 = CARTESIAN_POINT ( 'NONE',  ( -75.00000000000000000, 67.00000000000000000, -6.500000000000000000 ) ) ;
#6825 = CARTESIAN_POINT ( 'NONE',  ( -195.0000000000000000, 1.166476076187852838E-15, -9.524999999999991473 ) ) ;
#6826 = SURFACE_STYLE_USAGE ( .BOTH. , #6145 ) ;
#6827 = CARTESIAN_POINT ( 'NONE',  ( -147.9570736234661581, 9.058813317711329915, -2.943386871421373119 ) ) ;
#6828 = CARTESIAN_POINT ( 'NONE',  ( 61.74999999999998579, 31.24999999999999289, -3.750000000000000000 ) ) ;
#6829 = CIRCLE ( 'NONE', #49533, 0.2500000000000002220 ) ;
#6830 = CARTESIAN_POINT ( 'NONE',  ( 5.598654528085805993, 135.2450000000000045, 7.705886871421374629 ) ) ;
#6831 = CARTESIAN_POINT ( 'NONE',  ( -81.65707362346617515, 9.058813317711329915, 2.943386871421369566 ) ) ;
#6832 = CARTESIAN_POINT ( 'NONE',  ( -175.8549999999999898, 4.716976649647094177, 6.492361379858945902 ) ) ;
#6833 = EDGE_CURVE ( 'NONE', #30766, #2723, #59937, .T. ) ;
#6834 = CARTESIAN_POINT ( 'NONE',  ( -53.18756747357344494, -10.02680648607920588, -3.499999999999313882 ) ) ;
#6835 = ORIENTED_EDGE ( 'NONE', *, *, #33679, .F. ) ;
#6836 = CIRCLE ( 'NONE', #21453, 18.53939201416945082 ) ;
#6837 = CYLINDRICAL_SURFACE ( 'NONE', #48255, 16.99999999999998579 ) ;
#6838 = ADVANCED_FACE ( 'NONE', ( #23850 ), #30855, .T. ) ;
#6840 = FILL_AREA_STYLE ('',( #45213 ) ) ;
#6839 = CARTESIAN_POINT ( 'NONE',  ( 179.4098300562505415, 0.000000000000000000, 0.000000000000000000 ) ) ;
#6841 = SURFACE_STYLE_USAGE ( .BOTH. , #12809 ) ;
#6842 = CARTESIAN_POINT ( 'NONE',  ( -127.4049999999999869, -2.607480562269069768, 8.024999999999991473 ) ) ;
#6843 = CARTESIAN_POINT ( 'NONE',  ( -164.2429263765338021, 5.598654528085804216, 7.705886871421366635 ) ) ;
#6844 = CARTESIAN_POINT ( 'NONE',  ( 21.02379604162863913, 109.9999999999999858, -9.500000000000000000 ) ) ;
#6845 = DIRECTION ( 'NONE',  ( 0.000000000000000000, -0.6691306063588592368, 0.7431448254773934670 ) ) ;
#6846 = CARTESIAN_POINT ( 'NONE',  ( -144.8949999999999818, 6.826472737025116366, 4.959722759717898555 ) ) ;
#6847 = EDGE_CURVE ( 'NONE', #51899, #44849, #3747, .T. ) ;
#6848 = CARTESIAN_POINT ( 'NONE',  ( -133.6449999999999818, 4.716976649647091513, -6.492361379858946790 ) ) ;
#6849 = ORIENTED_EDGE ( 'NONE', *, *, #36972, .F. ) ;
#6850 = CARTESIAN_POINT ( 'NONE',  ( 44.97464006314718432, 9.991546687716517994, -3.784415753861334331 ) ) ;
#6851 = DIRECTION ( 'NONE',  ( 1.000000000000000000, 0.000000000000000000, 0.000000000000000000 ) ) ;
#6852 = AXIS2_PLACEMENT_3D ( 'NONE', #23761, #28675, #59654 ) ;
#6853 = CARTESIAN_POINT ( 'NONE',  ( 30.50000000000000711, 18.99999999999997868, 3.750000000000000000 ) ) ;
#6854 = EDGE_CURVE ( 'NONE', #21703, #40244, #56550, .T. ) ;
#6855 = CARTESIAN_POINT ( 'NONE',  ( -179.9929263765337453, 8.102448949553171076, -5.886773742842744461 ) ) ;
#6856 = SURFACE_STYLE_FILL_AREA ( #43843 ) ;
#6857 = CARTESIAN_POINT ( 'NONE',  ( -63.59499999999997755, 2.607480562269073321, 8.024999999999991473 ) ) ;
#6858 = VECTOR ( 'NONE', #43595, 1000.000000000000000 ) ;
#6859 =( NAMED_UNIT ( * ) PLANE_ANGLE_UNIT ( ) SI_UNIT ( $, .RADIAN. ) );
#6860 = FACE_OUTER_BOUND ( 'NONE', #45436, .T. ) ;
#6861 = CARTESIAN_POINT ( 'NONE',  ( -55.09822643348442028, -8.922505785858549032, -1.646890977621942254 ) ) ;
#6862 = CARTESIAN_POINT ( 'NONE',  ( -75.95707362346617231, 9.058813317711329915, -2.943386871421373119 ) ) ;
#6863 = AXIS2_PLACEMENT_3D ( 'NONE', #37132, #68769, #37492 ) ;
#6864 = CARTESIAN_POINT ( 'NONE',  ( -91.34292637653381064, -9.058813317711329915, 2.943386871421371787 ) ) ;
#6865 = APPLICATION_PROTOCOL_DEFINITION ( 'draft international standard', 'automotive_design', 1998, #57672 ) ;
#6866 = CARTESIAN_POINT ( 'NONE',  ( -103.5570736234661808, -1.166476076187852838E-15, -9.524999999999991473 ) ) ;
#6867 = DIRECTION ( 'NONE',  ( 0.000000000000000000, 0.000000000000000000, 1.000000000000000000 ) ) ;
#6868 = CIRCLE ( 'NONE', #10306, 14.00000000000000533 ) ;
#6869 = DIRECTION ( 'NONE',  ( -0.000000000000000000, 1.000000000000000000, -0.000000000000000000 ) ) ;
#6870 = CARTESIAN_POINT ( 'NONE',  ( -79.25707362346618368, 5.598654528085800663, -7.705886871421367523 ) ) ;
#6871 = VECTOR ( 'NONE', #26421, 1000.000000000000000 ) ;
#6872 = CARTESIAN_POINT ( 'NONE',  ( -91.55707362346616662, -1.166476076187852838E-15, -9.524999999999991473 ) ) ;
#6873 = EDGE_LOOP ( 'NONE', ( #59411, #18653, #45529, #52071, #19636, #63820, #39133, #42843, #35291, #42896, #20298, #40169, #15137, #47208, #58021, #54180, #55801, #44993, #8857, #11785, #68496, #14007, #12956, #19187, #3423, #11631, #35076, #61315, #48548, #23159, #57346, #22367, #2058, #21614 ) ) ;
#6874 = CIRCLE ( 'NONE', #13597, 1.000000000000000888 ) ;
#6875 = PRESENTATION_STYLE_ASSIGNMENT (( #39968 ) ) ;
#6876 = DIRECTION ( 'NONE',  ( -1.000000000000000000, 0.000000000000000000, 0.000000000000000000 ) ) ;
#6877 = EDGE_LOOP ( 'NONE', ( #10533, #2815, #11339, #38314 ) ) ;
#6878 = DIRECTION ( 'NONE',  ( 0.000000000000000000, 0.000000000000000000, 1.000000000000000000 ) ) ;
#6879 = AXIS2_PLACEMENT_3D ( 'NONE', #59548, #412, #55312 ) ;
#6880 = CARTESIAN_POINT ( 'NONE',  ( -6.826472737025120807, 128.1070736234661354, 4.959722759717906548 ) ) ;
#6881 = DIRECTION ( 'NONE',  ( 1.000000000000000000, -0.000000000000000000, 0.000000000000000000 ) ) ;
#6882 =( LENGTH_UNIT ( ) NAMED_UNIT ( * ) SI_UNIT ( .MILLI., .METRE. ) );
#6883 = CIRCLE ( 'NONE', #13607, 5.000000000000000000 ) ;
#6884 = CARTESIAN_POINT ( 'NONE',  ( 25.00000000000000355, 36.75000000000000000, 4.000000000000000000 ) ) ;
#6885 = ORIENTED_EDGE ( 'NONE', *, *, #31606, .F. ) ;
#6886 = CARTESIAN_POINT ( 'NONE',  ( -116.7570736234661695, -5.598654528085801552, 7.705886871421367523 ) ) ;
#6887 = CARTESIAN_POINT ( 'NONE',  ( 57.00000000000000000, 13.00000000000000178, 79.00402776293826435 ) ) ;
#6888 = ORIENTED_EDGE ( 'NONE', *, *, #53915, .T. ) ;
#6889 = CARTESIAN_POINT ( 'NONE',  ( 16.75000000000000711, 27.74999999999998224, -3.750000000000000000 ) ) ;
#6890 = LINE ( 'NONE', #17481, #13128 ) ;
#6891 = CIRCLE ( 'NONE', #60806, 16.99999999999998579 ) ;
#6892 = DIRECTION ( 'NONE',  ( 0.000000000000000000, 0.000000000000000000, 1.000000000000000000 ) ) ;
#6893 = CARTESIAN_POINT ( 'NONE',  ( -94.94499999999999318, -9.827790563157499189E-16, -8.024999999999991473 ) ) ;
#6894 = VERTEX_POINT ( 'NONE', #62170 ) ;
#6895 = CARTESIAN_POINT ( 'NONE',  ( -7.632228543268608334, 123.8429263765338249, 2.479861379858952830 ) ) ;
#6896 = EDGE_CURVE ( 'NONE', #67189, #19250, #56194, .T. ) ;
#6897 = PRESENTATION_LAYER_ASSIGNMENT (  '', '', ( #58576 ) ) ;
#6898 = CARTESIAN_POINT ( 'NONE',  ( 69.99999999999998579, 8.572527594031471415E-15, 4.000000000000000000 ) ) ;
#6899 = EDGE_LOOP ( 'NONE', ( #44931, #46945, #27793, #23962 ) ) ;
#6900 = DIRECTION ( 'NONE',  ( -0.000000000000000000, 1.000000000000000000, -0.000000000000000000 ) ) ;
#6901 = EDGE_CURVE ( 'NONE', #51449, #52352, #53246, .T. ) ;
#6902 = VECTOR ( 'NONE', #40611, 1000.000000000000000 ) ;
#6903 = EDGE_CURVE ( 'NONE', #32066, #41197, #68170, .T. ) ;
#6904 = DIRECTION ( 'NONE',  ( 1.000000000000000000, 0.000000000000000000, 0.000000000000000000 ) ) ;
#6905 = ORIENTED_EDGE ( 'NONE', *, *, #58494, .F. ) ;
#6906 = ADVANCED_FACE ( 'NONE', ( #50942 ), #68510, .F. ) ;
#6907 =( NAMED_UNIT ( * ) SI_UNIT ( $, .STERADIAN. ) SOLID_ANGLE_UNIT ( ) );
#6908 = ORIENTED_EDGE ( 'NONE', *, *, #36890, .T. ) ;
#6909 = CARTESIAN_POINT ( 'NONE',  ( 44.99999999999977973, 146.9999999999999716, -9.500000000000000000 ) ) ;
#6910 = DIRECTION ( 'NONE',  ( 0.000000000000000000, 0.000000000000000000, -1.000000000000000000 ) ) ;
#6911 = CARTESIAN_POINT ( 'NONE',  ( -4.357963766315032572, -1.733608113333017453, 6.451785339198141678 ) ) ;
#6912 =( GEOMETRIC_REPRESENTATION_CONTEXT ( 3 ) GLOBAL_UNCERTAINTY_ASSIGNED_CONTEXT ( ( #22222 ) ) GLOBAL_UNIT_ASSIGNED_CONTEXT ( ( #65194, #60590, #44493 ) ) REPRESENTATION_CONTEXT ( 'NONE', 'WORKASPACE' ) );
#6913 = CARTESIAN_POINT ( 'NONE',  ( 15.98999599679679839, 118.4999999999999716, 7.000000000000000000 ) ) ;
#6914 = DIRECTION ( 'NONE',  ( -1.000000000000000000, -0.000000000000000000, 1.300977106640434891E-16 ) ) ;
#6915 = CARTESIAN_POINT ( 'NONE',  ( -114.6570736234661751, 9.058813317711329915, 2.943386871421369566 ) ) ;
#6916 = AXIS2_PLACEMENT_3D ( 'NONE', #32927, #43528, #54362 ) ;
#6917 = CARTESIAN_POINT ( 'NONE',  ( -45.91547277936962246, 9.430195807687212550, -3.611004237778682402 ) ) ;
#6918 = CARTESIAN_POINT ( 'NONE',  ( 8.319377385370872346, -3.000000000000000888, 2.000000000000000000 ) ) ;
#6919 = VERTEX_POINT ( 'NONE', #20304 ) ;
#6920 = CIRCLE ( 'NONE', #50722, 3.000000000000000444 ) ;
#6921 = DIRECTION ( 'NONE',  ( 0.000000000000000000, 1.000000000000000000, 0.000000000000000000 ) ) ;
#6922 = DIRECTION ( 'NONE',  ( 0.000000000000000000, 0.000000000000000000, 1.000000000000000000 ) ) ;
#6923 = EDGE_CURVE ( 'NONE', #23187, #51098, #39153, .T. ) ;
#6924 = CARTESIAN_POINT ( 'NONE',  ( -71.50000000000000000, 14.49137674618942562, 7.500000000000000000 ) ) ;
#6925 = ORIENTED_EDGE ( 'NONE', *, *, #67963, .T. ) ;
#6926 = CARTESIAN_POINT ( 'NONE',  ( -161.1550000000000011, 7.632228543268600340, 2.479861379858949277 ) ) ;
#6927 = LINE ( 'NONE', #7968, #9464 ) ;
#6928 = LINE ( 'NONE', #34688, #67307 ) ;
#6929 =( GEOMETRIC_REPRESENTATION_CONTEXT ( 3 ) GLOBAL_UNCERTAINTY_ASSIGNED_CONTEXT ( ( #25047 ) ) GLOBAL_UNIT_ASSIGNED_CONTEXT ( ( #12026, #706, #16643 ) ) REPRESENTATION_CONTEXT ( 'NONE', 'WORKASPACE' ) );
#6930 = CARTESIAN_POINT ( 'NONE',  ( -177.2950000000000159, -2.607480562269069768, 8.024999999999991473 ) ) ;
#6931 = CARTESIAN_POINT ( 'NONE',  ( -158.8449999999999989, -7.632228543268599452, 2.479861379858951054 ) ) ;
#6932 = ORIENTED_EDGE ( 'NONE', *, *, #61683, .F. ) ;
#6933 = CYLINDRICAL_SURFACE ( 'NONE', #18948, 4.000000000000000000 ) ;
#6934 = CARTESIAN_POINT ( 'NONE',  ( 45.00000000011531398, 10.00000000003077716, 3.953713388244146199 ) ) ;
#6935 = CARTESIAN_POINT ( 'NONE',  ( -52.50000000000000000, -2.024042244987997205E-14, 12.00000000000000000 ) ) ;
#6936 = CARTESIAN_POINT ( 'NONE',  ( -68.60499999999996135, 6.826472737025113702, -4.959722759717902107 ) ) ;
#6937 = CARTESIAN_POINT ( 'NONE',  ( -35.96227966833271239, -10.14840438130919331, 4.278652250189864503 ) ) ;
#6938 = VECTOR ( 'NONE', #7031, 1000.000000000000000 ) ;
#6939 = DIRECTION ( 'NONE',  ( 0.000000000000000000, 1.000000000000000000, 0.000000000000000000 ) ) ;
#6940 = CARTESIAN_POINT ( 'NONE',  ( -69.29499999999998749, -2.607480562269069768, 8.024999999999991473 ) ) ;
#6941 = CARTESIAN_POINT ( 'NONE',  ( 10.01517768586949231, 142.8049999999999500, 1.839758294383810543E-15 ) ) ;
#6942 = EDGE_CURVE ( 'NONE', #34386, #443, #19613, .T. ) ;
#6943 = CARTESIAN_POINT ( 'NONE',  ( 62.10000000000000142, 11.99999999999999822, 4.000000000000000000 ) ) ;
#6944 = AXIS2_PLACEMENT_3D ( 'NONE', #34807, #7044, #1719 ) ;
#6945 = CARTESIAN_POINT ( 'NONE',  ( -177.4429263765338192, -1.166476076187852838E-15, -9.524999999999991473 ) ) ;
#6946 = EDGE_CURVE ( 'NONE', #65906, #26318, #13802, .T. ) ;
#6947 = SHAPE_REPRESENTATION ( '2. Support', ( #42840 ), #2244 ) ;
#6948 = SURFACE_SIDE_STYLE ('',( #1620 ) ) ;
#6950 = EDGE_LOOP ( 'NONE', ( #49253, #53968, #33211 ) ) ;
#6949 = COLOUR_RGB ( '', 0.66274510, 0.83137255, 0.94901961) ;
#6951 = VECTOR ( 'NONE', #40988, 1000.000000000000000 ) ;
#6952 = PRESENTATION_STYLE_ASSIGNMENT (( #7311 ) ) ;
#6953 = AXIS2_PLACEMENT_3D ( 'NONE', #65979, #1565, #12155 ) ;
#6954 = PRESENTATION_LAYER_ASSIGNMENT (  '', '', ( #65353 ) ) ;
#6955 = CYLINDRICAL_SURFACE ( 'NONE', #36061, 0.2500000000000002220 ) ;
#6956 = AXIS2_PLACEMENT_3D ( 'NONE', #13903, #51198, #39623 ) ;
#6957 = ORIENTED_EDGE ( 'NONE', *, *, #42525, .T. ) ;
#6958 = ORIENTED_EDGE ( 'NONE', *, *, #28495, .T. ) ;
#6959 = CARTESIAN_POINT ( 'NONE',  ( -11.99999999999999822, -8.499999999999998224, 21.00000000000000000 ) ) ;
#6960 = STYLED_ITEM ( 'NONE', ( #54967 ), #35309 ) ;
#6961 = AXIS2_PLACEMENT_3D ( 'NONE', #4002, #25472, #41693 ) ;
#6962 = DIRECTION ( 'NONE',  ( 0.000000000000000000, 0.000000000000000000, 1.000000000000000000 ) ) ;
#6963 = SURFACE_STYLE_FILL_AREA ( #22454 ) ;
#6964 = AXIS2_PLACEMENT_3D ( 'NONE', #52577, #53922, #5722 ) ;
#6965 = DIRECTION ( 'NONE',  ( 0.000000000000000000, 1.000000000000000000, -0.000000000000000000 ) ) ;
#6966 = DIRECTION ( 'NONE',  ( 0.000000000000000000, -1.000000000000000000, 0.000000000000000000 ) ) ;
#6967 = ORIENTED_EDGE ( 'NONE', *, *, #55908, .T. ) ;
#6968 = CARTESIAN_POINT ( 'NONE',  ( -111.6549999999999869, -7.632228543268600340, -2.479861379858950166 ) ) ;
#6969 = ORIENTED_EDGE ( 'NONE', *, *, #17028, .T. ) ;
#6970 = CARTESIAN_POINT ( 'NONE',  ( 98.00000000000000000, 16.00000000000000000, 0.000000000000000000 ) ) ;
#6971 = CONICAL_SURFACE ( 'NONE', #49683, 5.000000000000004441, 0.7853981633974587151 ) ;
#6972 = VERTEX_POINT ( 'NONE', #35101 ) ;
#6973 = DIRECTION ( 'NONE',  ( 0.000000000000000000, 0.000000000000000000, -1.000000000000000000 ) ) ;
#6974 = DIRECTION ( 'NONE',  ( 0.000000000000000000, 0.000000000000000000, -1.000000000000000000 ) ) ;
#6975 = VERTEX_POINT ( 'NONE', #10465 ) ;
#6976 = VECTOR ( 'NONE', #40424, 1000.000000000000000 ) ;
#6977 = ADVANCED_FACE ( 'NONE', ( #32578 ), #43212, .T. ) ;
#6978 = CARTESIAN_POINT ( 'NONE',  ( -41.49999999999997868, 10.49999999999998401, 3.000000000000000000 ) ) ;
#6979 = FACE_OUTER_BOUND ( 'NONE', #47446, .T. ) ;
#6980 = EDGE_LOOP ( 'NONE', ( #49282, #34470, #11907, #17667 ) ) ;
#6981 = VERTEX_POINT ( 'NONE', #42178 ) ;
#6982 = VECTOR ( 'NONE', #14199, 1000.000000000000000 ) ;
#6983 = CARTESIAN_POINT ( 'NONE',  ( -8.874979192299518260, 110.5000000000000142, -3.486497148140166313 ) ) ;
#6984 = DIRECTION ( 'NONE',  ( 0.000000000000000000, 0.000000000000000000, 1.000000000000000000 ) ) ;
#6985 = CYLINDRICAL_SURFACE ( 'NONE', #12570, 0.2500000000000002220 ) ;
#6986 = EDGE_CURVE ( 'NONE', #64475, #35776, #18283, .T. ) ;
#6987 = CARTESIAN_POINT ( 'NONE',  ( -71.62068965517239860, 36.41396814395972115, -7.000000000000000000 ) ) ;
#6988 = ORIENTED_EDGE ( 'NONE', *, *, #51155, .F. ) ;
#6989 = CARTESIAN_POINT ( 'NONE',  ( -8.437984349512095861, 135.6929263765338192, -5.166775262442723748E-16 ) ) ;
#6990 = DIRECTION ( 'NONE',  ( 0.000000000000000000, 1.000000000000000000, 0.000000000000000000 ) ) ;
#6991 = DIRECTION ( 'NONE',  ( -1.000000000000000000, -0.000000000000000000, -0.000000000000000000 ) ) ;
#6992 = STYLED_ITEM ( 'NONE', ( #59499 ), #24837 ) ;
#6993 = EDGE_CURVE ( 'NONE', #56449, #17121, #1400, .T. ) ;
#6994 = DIRECTION ( 'NONE',  ( -1.000000000000000000, 0.000000000000000000, 0.000000000000000000 ) ) ;
#6995 = ORIENTED_EDGE ( 'NONE', *, *, #16087, .F. ) ;
#6996 = DIRECTION ( 'NONE',  ( -0.000000000000000000, 0.000000000000000000, -1.000000000000000000 ) ) ;
#6997 = ORIENTED_EDGE ( 'NONE', *, *, #4924, .F. ) ;
#6998 = PRESENTATION_STYLE_ASSIGNMENT (( #45021 ) ) ;
#6999 = DIRECTION ( 'NONE',  ( 0.000000000000000000, 0.000000000000000000, 1.000000000000000000 ) ) ;
#7000 = DIRECTION ( 'NONE',  ( -0.000000000000000000, -1.000000000000000000, -0.000000000000000000 ) ) ;
#7001 = CARTESIAN_POINT ( 'NONE',  ( -138.0549999999999784, -9.827790563157499189E-16, -8.024999999999991473 ) ) ;
#7002 = CARTESIAN_POINT ( 'NONE',  ( -75.50000000000000000, 64.49137674618943095, -9.500000000000001776 ) ) ;
#7003 = CARTESIAN_POINT ( 'NONE',  ( 11.00000000000001776, -35.45414562583513884, -57.63767942241966580 ) ) ;
#7004 = ORIENTED_EDGE ( 'NONE', *, *, #28513, .F. ) ;
#7005 = COLOUR_RGB ( '', 0.40784314, 0.44705882, 0.49803922) ;
#7006 = CARTESIAN_POINT ( 'NONE',  ( 28.00000000000002132, 34.36176364315826248, 80.00402776293826435 ) ) ;
#7007 =( NAMED_UNIT ( * ) PLANE_ANGLE_UNIT ( ) SI_UNIT ( $, .RADIAN. ) );
#7008 = CARTESIAN_POINT ( 'NONE',  ( -45.00000000000000000, 9.585819622309035282, -6.373651444779981468 ) ) ;
#7009 = ORIENTED_EDGE ( 'NONE', *, *, #30853, .T. ) ;
#7010 = PRESENTATION_LAYER_ASSIGNMENT (  '', '', ( #1323 ) ) ;
#7011 = EDGE_LOOP ( 'NONE', ( #40780, #45304, #65041, #37862 ) ) ;
#7012 = CARTESIAN_POINT ( 'NONE',  ( -71.99999999999998579, 64.07124727947029896, 7.000000000000000000 ) ) ;
#7013 = EDGE_CURVE ( 'NONE', #4733, #29677, #53027, .T. ) ;
#7014 = CARTESIAN_POINT ( 'NONE',  ( -51.50499999999999545, -6.826472737025115478, -4.959722759717899443 ) ) ;
#7015 = ORIENTED_EDGE ( 'NONE', *, *, #28386, .T. ) ;
#7016 = DIRECTION ( 'NONE',  ( 0.000000000000000000, 0.000000000000000000, 1.000000000000000000 ) ) ;
#7017 = LINE ( 'NONE', #55895, #53200 ) ;
#7018 = MECHANICAL_DESIGN_GEOMETRIC_PRESENTATION_REPRESENTATION (  '', ( #19356 ), #18266 ) ;
#7019 = DIRECTION ( 'NONE',  ( -1.000000000000000000, 0.000000000000000000, 0.000000000000000000 ) ) ;
#7020 = ORIENTED_EDGE ( 'NONE', *, *, #49659, .F. ) ;
#7021 = CARTESIAN_POINT ( 'NONE',  ( -12.74999999999999822, -3.000000000000000000, 6.000000000000001776 ) ) ;
#7022 = COLOUR_RGB ( '', 0.31764706, 0.68627451, 0.89019608) ;
#7023 = DIRECTION ( 'NONE',  ( -0.000000000000000000, -0.000000000000000000, 1.000000000000000000 ) ) ;
#7024 = DIRECTION ( 'NONE',  ( -1.000000000000000000, 0.000000000000000000, 0.000000000000000000 ) ) ;
#7025 = FACE_OUTER_BOUND ( 'NONE', #24268, .T. ) ;
#7026 = CARTESIAN_POINT ( 'NONE',  ( -103.1949999999999932, 8.437984349512086979, -1.550032578732815448E-15 ) ) ;
#7027 = CARTESIAN_POINT ( 'NONE',  ( 10.01517768586949231, 115.8049999999999784, 1.839758294383810543E-15 ) ) ;
#7028 = CARTESIAN_POINT ( 'NONE',  ( -81.14499999999998181, -4.716976649647092401, 6.492361379858946790 ) ) ;
#7029 = CIRCLE ( 'NONE', #28333, 0.2500000000000002220 ) ;
#7030 = FILL_AREA_STYLE ('',( #14049 ) ) ;
#7031 = DIRECTION ( 'NONE',  ( 0.000000000000000000, 0.000000000000000000, -1.000000000000000000 ) ) ;
#7032 = CARTESIAN_POINT ( 'NONE',  ( 15.98999599679679839, 117.9999999999999716, -7.500000000000000000 ) ) ;
#7033 = DIRECTION ( 'NONE',  ( 1.000000000000000000, 0.000000000000000000, 0.000000000000000000 ) ) ;
#7034 =( NAMED_UNIT ( * ) SI_UNIT ( $, .STERADIAN. ) SOLID_ANGLE_UNIT ( ) );
#7035 = DIRECTION ( 'NONE',  ( 0.000000000000000000, 0.000000000000000000, 1.000000000000000000 ) ) ;
#7036 = ORIENTED_EDGE ( 'NONE', *, *, #50534, .F. ) ;
#7038 = CIRCLE ( 'NONE', #232, 0.5000000000000004441 ) ;
#7037 = CARTESIAN_POINT ( 'NONE',  ( -119.6929263765338192, 10.01517768586948698, -1.839758294383808571E-15 ) ) ;
#7039 =( BOUNDED_CURVE ( )  B_SPLINE_CURVE ( 3, ( #37337, #54139, #69633, #16212 ),
 .UNSPECIFIED., .F., .F. ) 
 B_SPLINE_CURVE_WITH_KNOTS ( ( 4, 4 ),
 ( 4.712388980384690562, 5.445427266222309548 ),
 .UNSPECIFIED. ) 
 CURVE ( )  GEOMETRIC_REPRESENTATION_ITEM ( )  RATIONAL_B_SPLINE_CURVE ( ( 1.000000000000000000, 0.9557202843314677176, 0.9557202843314677176, 1.000000000000000000 ) ) 
 REPRESENTATION_ITEM ( '' )  );
#7040 = CARTESIAN_POINT ( 'NONE',  ( -141.4449999999999932, 0.000000000000000000, 8.024999999999991473 ) ) ;
#7041 = FILL_AREA_STYLE ('',( #13344 ) ) ;
#7042 = AXIS2_PLACEMENT_3D ( 'NONE', #48577, #59774, #5596 ) ;
#7043 = CARTESIAN_POINT ( 'NONE',  ( -11.74999999999999645, -0.9999999999999995559, 19.00000000000000000 ) ) ;
#7044 = DIRECTION ( 'NONE',  ( 0.000000000000000000, 0.000000000000000000, 1.000000000000000000 ) ) ;
#7045 = ORIENTED_EDGE ( 'NONE', *, *, #5633, .T. ) ;
#7047 = ORIENTED_EDGE ( 'NONE', *, *, #35012, .T. ) ;
#7046 = VECTOR ( 'NONE', #6227, 1000.000000000000000 ) ;
#7048 = STYLED_ITEM ( 'NONE', ( #5134 ), #60917 ) ;
#7049 = CARTESIAN_POINT ( 'NONE',  ( 8.000000000000000000, 33.99999999999998579, 4.000000000000000000 ) ) ;
#7050 = STYLED_ITEM ( 'NONE', ( #63661 ), #46308 ) ;
#7051 = CARTESIAN_POINT ( 'NONE',  ( 19.89974874213239886, 114.9999999999999574, 10.49999999999999645 ) ) ;
#7052 =( LENGTH_UNIT ( ) NAMED_UNIT ( * ) SI_UNIT ( .MILLI., .METRE. ) );
#7053 = MECHANICAL_DESIGN_GEOMETRIC_PRESENTATION_REPRESENTATION (  '', ( #46416 ), #47542 ) ;
#7054 = CARTESIAN_POINT ( 'NONE',  ( -9.827790563157511022E-16, 143.5570736234661524, 8.025000000000000355 ) ) ;
#7055 = FILL_AREA_STYLE_COLOUR ( '', #9093 ) ;
#7056 = ORIENTED_EDGE ( 'NONE', *, *, #33865, .T. ) ;
#7057 = CARTESIAN_POINT ( 'NONE',  ( -142.5549999999999784, 0.000000000000000000, 8.024999999999991473 ) ) ;
#7058 = VERTEX_POINT ( 'NONE', #15749 ) ;
#7059 = ORIENTED_EDGE ( 'NONE', *, *, #46420, .T. ) ;
#7060 = CARTESIAN_POINT ( 'NONE',  ( -44.99999999999977973, 146.9999999999999716, -7.500000000000000000 ) ) ;
#7061 = DIRECTION ( 'NONE',  ( 1.000000000000000000, 0.000000000000000000, 0.000000000000000000 ) ) ;
#7062 = MECHANICAL_DESIGN_GEOMETRIC_PRESENTATION_REPRESENTATION (  '', ( #37457 ), #29553 ) ;
#7063 = ORIENTED_EDGE ( 'NONE', *, *, #32733, .T. ) ;
#7064 = ADVANCED_FACE ( 'NONE', ( #37230 ), #521, .T. ) ;
#7065 = PRODUCT_DEFINITION_SHAPE ( 'NONE', 'NONE',  #69718 ) ;
#7066 = CARTESIAN_POINT ( 'NONE',  ( -56.00691142449380777, -8.176804786315972962, -1.751816976611608512 ) ) ;
#7067 =( GEOMETRIC_REPRESENTATION_CONTEXT ( 3 ) GLOBAL_UNCERTAINTY_ASSIGNED_CONTEXT ( ( #55952 ) ) GLOBAL_UNIT_ASSIGNED_CONTEXT ( ( #56752, #35293, #13464 ) ) REPRESENTATION_CONTEXT ( 'NONE', 'WORKASPACE' ) );
#7068 =( NAMED_UNIT ( * ) SI_UNIT ( $, .STERADIAN. ) SOLID_ANGLE_UNIT ( ) );
#7069 = CARTESIAN_POINT ( 'NONE',  ( 5.598654528085805993, 132.2450000000000045, 7.705886871421374629 ) ) ;
#7070 = DIRECTION ( 'NONE',  ( -1.000000000000000000, -0.000000000000000000, -0.000000000000000000 ) ) ;
#7071 = COLOUR_RGB ( '', 0.31764706, 0.68627451, 0.89019608) ;
#7072 = ORIENTED_EDGE ( 'NONE', *, *, #68020, .T. ) ;
#7073 = DIRECTION ( 'NONE',  ( -0.000000000000000000, -0.000000000000000000, -1.000000000000000000 ) ) ;
#7074 = CARTESIAN_POINT ( 'NONE',  ( -8.102448949553179958, 126.6049999999999898, 5.886773742842747126 ) ) ;
#7075 = CARTESIAN_POINT ( 'NONE',  ( -54.80499999999999261, -8.437984349512086979, 5.166775262442717831E-16 ) ) ;
#7076 = CARTESIAN_POINT ( 'NONE',  ( 40.82708550458274033, 108.1272155206430483, -3.301554093733430228 ) ) ;
#7077 = ORIENTED_EDGE ( 'NONE', *, *, #2589, .F. ) ;
#7078 = CARTESIAN_POINT ( 'NONE',  ( 8.102448949553181734, 160.5049999999999386, 5.886773742842750679 ) ) ;
#7079 = LINE ( 'NONE', #38785, #55849 ) ;
#7080 = ADVANCED_FACE ( 'NONE', ( #5845 ), #58755, .T. ) ;
#7081 = CARTESIAN_POINT ( 'NONE',  ( -11.74999999999999645, 4.336808689942018722E-16, 5.000000000000001776 ) ) ;
#7082 = AXIS2_PLACEMENT_3D ( 'NONE', #54041, #31188, #26934 ) ;
#7083 = AXIS2_PLACEMENT_3D ( 'NONE', #10918, #59421, #960 ) ;
#7084 =( NAMED_UNIT ( * ) PLANE_ANGLE_UNIT ( ) SI_UNIT ( $, .RADIAN. ) );
#7085 = EDGE_CURVE ( 'NONE', #57872, #61983, #9303, .T. ) ;
#7086 = DIRECTION ( 'NONE',  ( -1.000000000000000000, 0.000000000000000000, 0.000000000000000000 ) ) ;
#7087 = MECHANICAL_DESIGN_GEOMETRIC_PRESENTATION_REPRESENTATION (  '', ( #43042 ), #66642 ) ;
#7088 = ORIENTED_EDGE ( 'NONE', *, *, #23304, .T. ) ;
#7089 = ADVANCED_FACE ( 'NONE', ( #17145 ), #12868, .F. ) ;
#7090 = ORIENTED_EDGE ( 'NONE', *, *, #24067, .T. ) ;
#7091 = DIRECTION ( 'NONE',  ( -0.000000000000000000, 0.000000000000000000, 1.000000000000000000 ) ) ;
#7092 = CYLINDRICAL_SURFACE ( 'NONE', #12628, 0.2500000000000002220 ) ;
#7093 = CARTESIAN_POINT ( 'NONE',  ( -158.7549999999999670, 4.716976649647091513, -6.492361379858946790 ) ) ;
#7095 = VERTEX_POINT ( 'NONE', #7590 ) ;
#7094 = ADVANCED_FACE ( 'NONE', ( #16795 ), #22744, .T. ) ;
#7096 = VECTOR ( 'NONE', #45730, 1000.000000000000000 ) ;
#7097 = ADVANCED_FACE ( 'NONE', ( #60016 ), #34333, .F. ) ;
#7098 = PRESENTATION_STYLE_ASSIGNMENT (( #27821 ) ) ;
#7099 = DIRECTION ( 'NONE',  ( 0.000000000000000000, 1.000000000000000000, 0.000000000000000000 ) ) ;
#7100 = LINE ( 'NONE', #56675, #69183 ) ;
#7101 = ORIENTED_EDGE ( 'NONE', *, *, #68629, .T. ) ;
#7102 = ORIENTED_EDGE ( 'NONE', *, *, #53904, .T. ) ;
#7103 = CARTESIAN_POINT ( 'NONE',  ( -57.44292637653381206, -1.166476076187852838E-15, -9.524999999999991473 ) ) ;
#7104 = DIRECTION ( 'NONE',  ( 0.000000000000000000, -1.000000000000000000, 0.000000000000000000 ) ) ;
#7105 = CARTESIAN_POINT ( 'NONE',  ( -89.45499999999999829, 7.632228543268599452, -2.479861379858951942 ) ) ;
#7106 = VERTEX_POINT ( 'NONE', #45272 ) ;
#7107 = FACE_OUTER_BOUND ( 'NONE', #910, .T. ) ;
#7108 = VECTOR ( 'NONE', #56489, 1000.000000000000000 ) ;
#7109 = MECHANICAL_DESIGN_GEOMETRIC_PRESENTATION_REPRESENTATION (  '', ( #20555 ), #46462 ) ;
#7110 = CARTESIAN_POINT ( 'NONE',  ( -151.1070736234661638, 8.102448949553172852, -5.886773742842744461 ) ) ;
#7111 = DIRECTION ( 'NONE',  ( -0.000000000000000000, -0.000000000000000000, 1.000000000000000000 ) ) ;
#7112 = EDGE_LOOP ( 'NONE', ( #27139, #13434, #17810, #5355 ) ) ;
#7113 = CARTESIAN_POINT ( 'NONE',  ( 1.401671290772265266, 7.000000000000007105, 0.1093172352041303641 ) ) ;
#7115 = PLANE ( 'NONE',  #29155 ) ;
#7114 = DIRECTION ( 'NONE',  ( 4.336808689941999001E-16, -1.000000000000000000, -0.000000000000000000 ) ) ;
#7116 = AXIS2_PLACEMENT_3D ( 'NONE', #17019, #50395, #11366 ) ;
#7117 = CARTESIAN_POINT ( 'NONE',  ( 5.598654528085805993, 129.2450000000000045, 7.705886871421374629 ) ) ;
#7118 = CARTESIAN_POINT ( 'NONE',  ( -109.7950000000000017, 2.607480562269068880, -8.024999999999993250 ) ) ;
#7119 = AXIS2_PLACEMENT_3D ( 'NONE', #33717, #54486, #43318 ) ;
#7120 = DIRECTION ( 'NONE',  ( -1.000000000000000000, 0.000000000000000000, 0.000000000000000000 ) ) ;
#7121 = AXIS2_PLACEMENT_3D ( 'NONE', #4561, #26015, #47188 ) ;
#7123 =( NAMED_UNIT ( * ) SI_UNIT ( $, .STERADIAN. ) SOLID_ANGLE_UNIT ( ) );
#7122 = FACE_OUTER_BOUND ( 'NONE', #39514, .T. ) ;
#7124 = CARTESIAN_POINT ( 'NONE',  ( -152.0929263765338249, 3.094860106618433360, 9.524999999999991473 ) ) ;
#7125 = AXIS2_PLACEMENT_3D ( 'NONE', #31619, #20738, #15480 ) ;
#7126 =( NAMED_UNIT ( * ) SI_UNIT ( $, .STERADIAN. ) SOLID_ANGLE_UNIT ( ) );
#7127 = CARTESIAN_POINT ( 'NONE',  ( -162.7450000000000045, 4.716976649647094177, 6.492361379858945902 ) ) ;
#7128 = AXIS2_PLACEMENT_3D ( 'NONE', #51002, #45071, #35163 ) ;
#7129 = CARTESIAN_POINT ( 'NONE',  ( 57.74999999999998579, 30.74999999999999289, -3.750000000000000000 ) ) ;
#7130 = ORIENTED_EDGE ( 'NONE', *, *, #66467, .T. ) ;
#7131 = SURFACE_SIDE_STYLE ('',( #12742 ) ) ;
#7132 = ORIENTED_EDGE ( 'NONE', *, *, #65186, .F. ) ;
#7133 = CARTESIAN_POINT ( 'NONE',  ( -70.94292637653380496, 0.000000000000000000, 9.524999999999991473 ) ) ;
#7134 = CARTESIAN_POINT ( 'NONE',  ( -45.79655366757389601, 8.974374905500285493, 6.364158535394770055 ) ) ;
#7135 = DIRECTION ( 'NONE',  ( 1.000000000000000000, 0.000000000000000000, 0.000000000000000000 ) ) ;
#7136 = AXIS2_PLACEMENT_3D ( 'NONE', #48851, #10141, #31574 ) ;
#7137 = AXIS2_PLACEMENT_3D ( 'NONE', #37199, #58262, #10086 ) ;
#7138 = CARTESIAN_POINT ( 'NONE',  ( -44.99154893936433552, 9.591540374752312914, 3.000000000000000000 ) ) ;
#7139 = CARTESIAN_POINT ( 'NONE',  ( 66.74999999999998579, 37.00000000000000000, 3.750000000000000000 ) ) ;
#7140 = DIRECTION ( 'NONE',  ( 1.000000000000000000, -0.000000000000000000, -0.000000000000000000 ) ) ;
#7141 = CARTESIAN_POINT ( 'NONE',  ( 21.00000000000001776, 15.00000000000000000, -29.68999999999999417 ) ) ;
#7142 = ORIENTED_EDGE ( 'NONE', *, *, #1217, .T. ) ;
#7143 = CARTESIAN_POINT ( 'NONE',  ( -167.4549999999999841, 7.632228543268599452, -2.479861379858951942 ) ) ;
#7144 = STYLED_ITEM ( 'NONE', ( #33205 ), #62484 ) ;
#7145 = ORIENTED_EDGE ( 'NONE', *, *, #21079, .F. ) ;
#7146 = DIRECTION ( 'NONE',  ( 0.7071067811865549002, 0.000000000000000000, 0.7071067811865402453 ) ) ;
#7147 = CARTESIAN_POINT ( 'NONE',  ( 15.98999599679679839, 146.4999999999999716, -10.00000000000000000 ) ) ;
#7148 = CARTESIAN_POINT ( 'NONE',  ( -9.000000000000003553, 27.99999999999998934, 3.750000000000000000 ) ) ;
#7149 = ADVANCED_FACE ( 'NONE', ( #32954 ), #22797, .T. ) ;
#7150 = AXIS2_PLACEMENT_3D ( 'NONE', #56525, #41083, #35443 ) ;
#7151 = CIRCLE ( 'NONE', #10527, 0.2500000000000002220 ) ;
#7152 = PLANE ( 'NONE',  #28641 ) ;
#7153 = CARTESIAN_POINT ( 'NONE',  ( 7.632228543268607446, 150.1570736234661751, 2.479861379858954606 ) ) ;
#7154 = ADVANCED_FACE ( 'NONE', ( #27638 ), #39634, .F. ) ;
#7155 = VECTOR ( 'NONE', #56037, 1000.000000000000000 ) ;
#7156 = ORIENTED_EDGE ( 'NONE', *, *, #18874, .F. ) ;
#7157 = TOROIDAL_SURFACE ( 'NONE', #35229, 1.000000000000000000, 0.5000000000000000000 ) ;
#7158 = CARTESIAN_POINT ( 'NONE',  ( -87.20499999999998408, -2.607480562269071545, -8.024999999999991473 ) ) ;
#7159 = DIRECTION ( 'NONE',  ( -1.000000000000000000, -0.000000000000000000, -0.000000000000000000 ) ) ;
#7160 = CARTESIAN_POINT ( 'NONE',  ( 5.598654528085805993, 130.3549999999999898, 7.705886871421374629 ) ) ;
#7161 = DIRECTION ( 'NONE',  ( -1.387778780781444413E-14, -1.000000000000000000, 0.000000000000000000 ) ) ;
#7162 = FILL_AREA_STYLE ('',( #67290 ) ) ;
#7163 = DIRECTION ( 'NONE',  ( -1.156482317317873451E-16, -1.000000000000000000, 0.000000000000000000 ) ) ;
#7164 =( GEOMETRIC_REPRESENTATION_CONTEXT ( 3 ) GLOBAL_UNCERTAINTY_ASSIGNED_CONTEXT ( ( #45456 ) ) GLOBAL_UNIT_ASSIGNED_CONTEXT ( ( #56003, #29629, #52156 ) ) REPRESENTATION_CONTEXT ( 'NONE', 'WORKASPACE' ) );
#7165 = CARTESIAN_POINT ( 'NONE',  ( 23.21231517720797655, 117.4999999999999716, 9.500000000000000000 ) ) ;
#7166 = CYLINDRICAL_SURFACE ( 'NONE', #17562, 0.5000000000000004441 ) ;
#7167 = EDGE_CURVE ( 'NONE', #37329, #61605, #68850, .T. ) ;
#7168 = SURFACE_STYLE_USAGE ( .BOTH. , #49736 ) ;
#7169 = ORIENTED_EDGE ( 'NONE', *, *, #9108, .T. ) ;
#7170 = CARTESIAN_POINT ( 'NONE',  ( -139.8570736234661638, -5.598654528085803328, -7.705886871421366635 ) ) ;
#7171 = CYLINDRICAL_SURFACE ( 'NONE', #21664, 0.5000000000000004441 ) ;
#7172 = CARTESIAN_POINT ( 'NONE',  ( -62.69499999999998607, -8.437984349512085203, 5.166775262442717831E-16 ) ) ;
#7173 = ORIENTED_EDGE ( 'NONE', *, *, #65103, .F. ) ;
#7174 = CARTESIAN_POINT ( 'NONE',  ( -25.00000000000000000, -9.376883653928695991E-17, -3.000000000000000000 ) ) ;
#7175 = SURFACE_STYLE_FILL_AREA ( #1124 ) ;
#7176 = CARTESIAN_POINT ( 'NONE',  ( -44.99999999999999289, 8.382277537376673138, -5.549490760430606073 ) ) ;
#7177 = ADVANCED_FACE ( 'NONE', ( #49483 ), #12159, .F. ) ;
#7178 = CARTESIAN_POINT ( 'NONE',  ( 72.50000000000000000, 36.32520566882265456, 9.500000000000000000 ) ) ;
#7179 = ORIENTED_EDGE ( 'NONE', *, *, #14976, .T. ) ;
#7180 = CARTESIAN_POINT ( 'NONE',  ( -52.31798797533910061, -11.10405175802884159, 3.489986028532363171 ) ) ;
#7181 = CARTESIAN_POINT ( 'NONE',  ( -51.29499999999997328, -2.607480562269069768, 8.024999999999991473 ) ) ;
#7182 = DIRECTION ( 'NONE',  ( 0.000000000000000000, 0.000000000000000000, 1.000000000000000000 ) ) ;
#7183 = ORIENTED_EDGE ( 'NONE', *, *, #48140, .F. ) ;
#7184 = AXIS2_PLACEMENT_3D ( 'NONE', #39718, #49217, #40076 ) ;
#7185 = STYLED_ITEM ( 'NONE', ( #48529 ), #29705 ) ;
#7186 = DIRECTION ( 'NONE',  ( 1.156482317317873451E-16, 1.000000000000000000, -0.000000000000000000 ) ) ;
#7187 = CARTESIAN_POINT ( 'NONE',  ( -110.3049999999999926, 8.437984349512085203, -1.550032578732815448E-15 ) ) ;
#7188 = ORIENTED_EDGE ( 'NONE', *, *, #43920, .F. ) ;
#7189 = SURFACE_SIDE_STYLE ('',( #55364 ) ) ;
#7190 = DIRECTION ( 'NONE',  ( -1.000000000000000000, 0.000000000000000000, 0.000000000000000000 ) ) ;
#7191 = CARTESIAN_POINT ( 'NONE',  ( 11.00000000000001776, 42.00000000000000000, 28.38386403503541899 ) ) ;
#7192 = DIRECTION ( 'NONE',  ( 0.000000000000000000, 0.000000000000000000, -1.000000000000000000 ) ) ;
#7193 = CARTESIAN_POINT ( 'NONE',  ( -155.0070736234661695, -8.102448949553172852, -5.886773742842741797 ) ) ;
#7194 = LINE ( 'NONE', #1846, #54171 ) ;
#7195 = CARTESIAN_POINT ( 'NONE',  ( 3.094860106618431583, 135.0949999999999704, 9.525000000000000355 ) ) ;
#7196 = CARTESIAN_POINT ( 'NONE',  ( -82.25707362346616947, 5.598654528085800663, -7.705886871421367523 ) ) ;
#7197 = COLOUR_RGB ( '', 0.31764706, 0.68627451, 0.89019608) ;
#7198 = VECTOR ( 'NONE', #15345, 999.9999999999998863 ) ;
#7199 = CARTESIAN_POINT ( 'NONE',  ( -95.84292637653379643, 9.058813317711329915, -2.943386871421373119 ) ) ;
#7200 = ORIENTED_EDGE ( 'NONE', *, *, #45078, .F. ) ;
#7201 = CARTESIAN_POINT ( 'NONE',  ( -15.75000000000000000, -3.000000000000000000, 19.00000000000000000 ) ) ;
#7202 =( LENGTH_UNIT ( ) NAMED_UNIT ( * ) SI_UNIT ( .MILLI., .METRE. ) );
#7203 = AXIS2_PLACEMENT_3D ( 'NONE', #56130, #7956, #19886 ) ;
#7204 = CARTESIAN_POINT ( 'NONE',  ( -128.6049999999999898, 6.826472737025113702, -4.959722759717902107 ) ) ;
#7205 = CARTESIAN_POINT ( 'NONE',  ( -165.2929263765340693, 3.094860106614496065, -9.525000000002851408 ) ) ;
#7206 =( LENGTH_UNIT ( ) NAMED_UNIT ( * ) SI_UNIT ( .MILLI., .METRE. ) );
#7207 = FILL_AREA_STYLE ('',( #65941 ) ) ;
#7208 = CARTESIAN_POINT ( 'NONE',  ( -139.7950000000000159, 2.607480562269068880, -8.024999999999993250 ) ) ;
#7209 = AXIS2_PLACEMENT_3D ( 'NONE', #66316, #28310, #18142 ) ;
#7210 = CARTESIAN_POINT ( 'NONE',  ( -129.8949999999999818, 6.826472737025115478, 4.959722759717899443 ) ) ;
#7211 = LINE ( 'NONE', #34973, #8922 ) ;
#7212 = ORIENTED_EDGE ( 'NONE', *, *, #55617, .F. ) ;
#7213 = EDGE_CURVE ( 'NONE', #33977, #15830, #5902, .T. ) ;
#7214 = CARTESIAN_POINT ( 'NONE',  ( -65.49999999999998579, 50.00000000000000000, -9.999999999999998224 ) ) ;
#7215 = CARTESIAN_POINT ( 'NONE',  ( 10.00000000000001954, 50.00000000000000000, 46.00000000000000000 ) ) ;
#7216 = CARTESIAN_POINT ( 'NONE',  ( -184.9429263765338192, 0.000000000000000000, 9.524999999999991473 ) ) ;
#7217 = DIRECTION ( 'NONE',  ( 0.000000000000000000, 0.000000000000000000, 1.000000000000000000 ) ) ;
#7218 = CARTESIAN_POINT ( 'NONE',  ( -47.39499999999998181, -6.826472737025115478, -4.959722759717899443 ) ) ;
#7219 = FILL_AREA_STYLE_COLOUR ( '', #55650 ) ;
#7220 = CARTESIAN_POINT ( 'NONE',  ( -9.000000000000003553, 25.24999999999998934, 3.750000000000000000 ) ) ;
#7221 =( LENGTH_UNIT ( ) NAMED_UNIT ( * ) SI_UNIT ( .MILLI., .METRE. ) );
#7222 = CIRCLE ( 'NONE', #35292, 1.000000000000000888 ) ;
#7223 = LINE ( 'NONE', #43521, #60397 ) ;
#7224 = CARTESIAN_POINT ( 'NONE',  ( 45.00000000000000000, 99.99999999999992895, -9.500000000000000000 ) ) ;
#7225 = CARTESIAN_POINT ( 'NONE',  ( -98.24292637653380211, 5.598654528085804216, 7.705886871421366635 ) ) ;
#7226 = APPLICATION_PROTOCOL_DEFINITION ( 'draft international standard', 'automotive_design', 1998, #13175 ) ;
#7227 = CARTESIAN_POINT ( 'NONE',  ( 0.000000000000000000, 87.30187232391182306, 0.000000000000000000 ) ) ;
#7228 = VECTOR ( 'NONE', #17934, 1000.000000000000000 ) ;
#7229 = DIRECTION ( 'NONE',  ( -1.000000000000000000, 0.000000000000000000, 0.000000000000000000 ) ) ;
#7230 = CARTESIAN_POINT ( 'NONE',  ( -41.49999999999998579, 106.9282032302754999, 3.500000000000000000 ) ) ;
#7231 = ADVANCED_FACE ( 'NONE', ( #39994 ), #34657, .T. ) ;
#7232 = VECTOR ( 'NONE', #41424, 1000.000000000000000 ) ;
#7233 = EDGE_CURVE ( 'NONE', #28073, #24442, #50859, .T. ) ;
#7234 = ORIENTED_EDGE ( 'NONE', *, *, #48728, .F. ) ;
#7235 = DIRECTION ( 'NONE',  ( 1.000000000000000000, 0.000000000000000000, 0.000000000000000000 ) ) ;
#7236 = ORIENTED_EDGE ( 'NONE', *, *, #26668, .F. ) ;
#7237 = DIRECTION ( 'NONE',  ( 0.000000000000000000, -1.000000000000000000, 0.000000000000000000 ) ) ;
#7238 = CARTESIAN_POINT ( 'NONE',  ( 2.607480562269071989, 119.7070736234661723, 8.025000000000002132 ) ) ;
#7239 = CIRCLE ( 'NONE', #65628, 0.2500000000000002220 ) ;
#7240 = VECTOR ( 'NONE', #34753, 1000.000000000000000 ) ;
#7241 = EDGE_CURVE ( 'NONE', #22515, #35027, #2955, .T. ) ;
#7242 = FILL_AREA_STYLE ('',( #33956 ) ) ;
#7243 = CARTESIAN_POINT ( 'NONE',  ( 16.00000000000001776, 43.00000000000000000, 35.68999999999999062 ) ) ;
#7244 =( LENGTH_UNIT ( ) NAMED_UNIT ( * ) SI_UNIT ( .MILLI., .METRE. ) );
#7245 = ORIENTED_EDGE ( 'NONE', *, *, #42146, .T. ) ;
#7246 = CARTESIAN_POINT ( 'NONE',  ( -115.5570736234661808, -1.166476076187852838E-15, -9.524999999999991473 ) ) ;
#7247 = AXIS2_PLACEMENT_3D ( 'NONE', #38479, #60228, #48680 ) ;
#7248 = DIRECTION ( 'NONE',  ( 1.000000000000000000, 0.000000000000000000, -0.000000000000000000 ) ) ;
#7249 = VERTEX_POINT ( 'NONE', #2619 ) ;
#7250 = DIRECTION ( 'NONE',  ( -1.000000000000000000, 0.000000000000000000, 0.000000000000000000 ) ) ;
#7251 = SURFACE_STYLE_USAGE ( .BOTH. , #35011 ) ;
#7252 = EDGE_CURVE ( 'NONE', #18813, #19277, #67887, .T. ) ;
#7253 = AXIS2_PLACEMENT_3D ( 'NONE', #43469, #22291, #16016 ) ;
#7254 = DIRECTION ( 'NONE',  ( 1.000000000000000000, 0.000000000000000000, 0.000000000000000000 ) ) ;
#7255 = CARTESIAN_POINT ( 'NONE',  ( -96.14499999999999602, -4.716976649647092401, 6.492361379858946790 ) ) ;
#7256 = VERTEX_POINT ( 'NONE', #40314 ) ;
#7257 = CARTESIAN_POINT ( 'NONE',  ( 0.8118891587097655238, 154.3723208332566514, -9.397320833256809891 ) ) ;
#7258 = SURFACE_STYLE_USAGE ( .BOTH. , #33631 ) ;
#7259 = ADVANCED_FACE ( 'NONE', ( #56837 ), #24118, .F. ) ;
#7260 = ORIENTED_EDGE ( 'NONE', *, *, #33659, .T. ) ;
#7261 = DIRECTION ( 'NONE',  ( 1.000000000000000000, 0.000000000000000000, 0.000000000000000000 ) ) ;
#7262 = DIRECTION ( 'NONE',  ( 0.000000000000000000, 0.000000000000000000, -1.000000000000000000 ) ) ;
#7263 = AXIS2_PLACEMENT_3D ( 'NONE', #22758, #34346, #55451 ) ;
#7264 = DIRECTION ( 'NONE',  ( 0.000000000000000000, 1.000000000000000000, 0.000000000000000000 ) ) ;
#7265 = VERTEX_POINT ( 'NONE', #47731 ) ;
#7266 = DIRECTION ( 'NONE',  ( 1.000000000000000000, 0.000000000000000000, -1.300977106640435137E-16 ) ) ;
#7267 = ORIENTED_EDGE ( 'NONE', *, *, #37229, .F. ) ;
#7268 =( LENGTH_UNIT ( ) NAMED_UNIT ( * ) SI_UNIT ( .MILLI., .METRE. ) );
#7269 = DIRECTION ( 'NONE',  ( -0.000000000000000000, -0.000000000000000000, 1.000000000000000000 ) ) ;
#7270 = CARTESIAN_POINT ( 'NONE',  ( 2.755156416437880562, -1.983268963961026810, 7.000000000000000000 ) ) ;
#7271 = AXIS2_PLACEMENT_3D ( 'NONE', #55719, #17424, #1497 ) ;
#7272 = CARTESIAN_POINT ( 'NONE',  ( -179.3070736234661524, -10.01517768586948698, 6.132527647946031529E-16 ) ) ;
#7273 = CARTESIAN_POINT ( 'NONE',  ( -44.50000000000000000, 10.49999999999998579, 3.000000000000000000 ) ) ;
#7274 = DIRECTION ( 'NONE',  ( 0.000000000000000000, 0.000000000000000000, 1.000000000000000000 ) ) ;
#7275 = AXIS2_PLACEMENT_3D ( 'NONE', #56677, #8830, #67576 ) ;
#7276 = CARTESIAN_POINT ( 'NONE',  ( -109.7070736234661581, -3.094860106618431139, -9.524999999999991473 ) ) ;
#7277 = CARTESIAN_POINT ( 'NONE',  ( -4.041451884327378785, 1.417096231345241542, 7.000000000000000000 ) ) ;
#7278 = VECTOR ( 'NONE', #46445, 1000.000000000000000 ) ;
#7279 = CARTESIAN_POINT ( 'NONE',  ( -85.40707362346616094, 3.094860106618428031, -9.524999999999993250 ) ) ;
#7280 = ORIENTED_EDGE ( 'NONE', *, *, #60652, .T. ) ;
#7281 = CARTESIAN_POINT ( 'NONE',  ( 0.08961491207242036627, 42.48853761352472702, 45.29557347147078872 ) ) ;
#7282 = SURFACE_STYLE_USAGE ( .BOTH. , #29409 ) ;
#7283 = DIRECTION ( 'NONE',  ( 0.000000000000000000, 0.000000000000000000, -1.000000000000000000 ) ) ;
#7284 =( NAMED_UNIT ( * ) SI_UNIT ( $, .STERADIAN. ) SOLID_ANGLE_UNIT ( ) );
#7285 = ORIENTED_EDGE ( 'NONE', *, *, #24038, .T. ) ;
#7286 = CARTESIAN_POINT ( 'NONE',  ( -157.5550000000000068, 0.000000000000000000, 8.024999999999991473 ) ) ;
#7287 = CARTESIAN_POINT ( 'NONE',  ( 4.000000000000002665, 38.70020753820971748, -89.00000000000000000 ) ) ;
#7288 = CARTESIAN_POINT ( 'NONE',  ( -183.7648598996489113, -7.758193185839872719, -4.080356100732527302 ) ) ;
#7289 = CARTESIAN_POINT ( 'NONE',  ( -162.5949999999999704, 2.607480562269073321, 8.024999999999991473 ) ) ;
#7290 = CARTESIAN_POINT ( 'NONE',  ( -156.7450000000000045, 4.716976649647094177, 6.492361379858945902 ) ) ;
#7291 = ORIENTED_EDGE ( 'NONE', *, *, #6420, .T. ) ;
#7292 = EDGE_CURVE ( 'NONE', #443, #59509, #42097, .T. ) ;
#7293 = CARTESIAN_POINT ( 'NONE',  ( -67.94292637653380496, 0.000000000000000000, 9.524999999999991473 ) ) ;
#7294 = AXIS2_PLACEMENT_3D ( 'NONE', #7896, #34981, #51174 ) ;
#7295 = CARTESIAN_POINT ( 'NONE',  ( 71.50000000000000000, 35.92875272052971525, 7.000000000000000000 ) ) ;
#7296 = CARTESIAN_POINT ( 'NONE',  ( -73.70499999999998408, 2.607480562269073321, 8.024999999999991473 ) ) ;
#7297 = CYLINDRICAL_SURFACE ( 'NONE', #49488, 0.2500000000000002220 ) ;
#7298 = CARTESIAN_POINT ( 'NONE',  ( 15.48999599679679662, 146.4999999999999716, 7.500000000000000000 ) ) ;
#7299 = AXIS2_PLACEMENT_3D ( 'NONE', #57639, #3786, #9462 ) ;
#7300 = CARTESIAN_POINT ( 'NONE',  ( -75.74499999999999034, 4.716976649647094177, 6.492361379858945902 ) ) ;
#7301 = CARTESIAN_POINT ( 'NONE',  ( 9.058813317711337021, 148.6549999999999727, 2.943386871421375783 ) ) ;
#7302 = CARTESIAN_POINT ( 'NONE',  ( -4.041451884327380562, 1.417096231345237545, -7.000000000000003553 ) ) ;
#7303 = CIRCLE ( 'NONE', #62382, 0.5000000000000004441 ) ;
#7304 =( GEOMETRIC_REPRESENTATION_CONTEXT ( 3 ) GLOBAL_UNCERTAINTY_ASSIGNED_CONTEXT ( ( #20717 ) ) GLOBAL_UNIT_ASSIGNED_CONTEXT ( ( #1473, #60951, #34570 ) ) REPRESENTATION_CONTEXT ( 'NONE', 'WORKASPACE' ) );
#7305 = STYLED_ITEM ( 'NONE', ( #15734 ), #5862 ) ;
#7306 = CARTESIAN_POINT ( 'NONE',  ( 48.50000000000000000, 99.99999999999992895, -7.000000000000000000 ) ) ;
#7307 = UNCERTAINTY_MEASURE_WITH_UNIT (LENGTH_MEASURE( 1.000000000000000082E-05 ), #37353, 'distance_accuracy_value', 'NONE');
#7308 =( LENGTH_UNIT ( ) NAMED_UNIT ( * ) SI_UNIT ( .MILLI., .METRE. ) );
#7309 = CARTESIAN_POINT ( 'NONE',  ( 16.00000000000001776, 15.00000000000000000, 29.68999999999999417 ) ) ;
#7310 = ADVANCED_FACE ( 'NONE', ( #48391 ), #3788, .T. ) ;
#7311 = SURFACE_STYLE_USAGE ( .BOTH. , #1944 ) ;
#7312 = EDGE_CURVE ( 'NONE', #51526, #5648, #32494, .T. ) ;
#7313 = CIRCLE ( 'NONE', #2799, 0.2500000000000002220 ) ;
#7314 = DIRECTION ( 'NONE',  ( 1.000000000000000000, 0.000000000000000000, 0.000000000000000000 ) ) ;
#7315 = EDGE_CURVE ( 'NONE', #30440, #42106, #68788, .T. ) ;
#7316 = CARTESIAN_POINT ( 'NONE',  ( -119.5429263765338135, 9.058813317711329915, 2.943386871421369566 ) ) ;
#7317 = PRESENTATION_STYLE_ASSIGNMENT (( #24169 ) ) ;
#7318 = ORIENTED_EDGE ( 'NONE', *, *, #38319, .F. ) ;
#7319 = ORIENTED_EDGE ( 'NONE', *, *, #3780, .T. ) ;
#7320 = CARTESIAN_POINT ( 'NONE',  ( -2.607480562269115509, 135.0929263765338249, -8.024999999999970157 ) ) ;
#7321 = DIRECTION ( 'NONE',  ( 0.000000000000000000, 0.000000000000000000, -1.000000000000000000 ) ) ;
#7322 = EDGE_CURVE ( 'NONE', #9977, #60808, #58866, .T. ) ;
#7323 = CARTESIAN_POINT ( 'NONE',  ( 26.25000000000001066, 18.99999999999997868, 4.000000000000000000 ) ) ;
#7324 = FILL_AREA_STYLE_COLOUR ( '', #1485 ) ;
#7325 = CYLINDRICAL_SURFACE ( 'NONE', #27413, 0.5000000000000004441 ) ;
#7326 = EDGE_CURVE ( 'NONE', #5309, #54365, #28502, .T. ) ;
#7327 = ORIENTED_EDGE ( 'NONE', *, *, #10519, .F. ) ;
#7328 = CARTESIAN_POINT ( 'NONE',  ( -102.5049999999999812, -6.826472737025113702, -4.959722759717900331 ) ) ;
#7329 = ORIENTED_EDGE ( 'NONE', *, *, #68891, .T. ) ;
#7330 = CARTESIAN_POINT ( 'NONE',  ( 31.00000000000000711, 15.00000000000000711, -36.50000000000000000 ) ) ;
#7331 = ORIENTED_EDGE ( 'NONE', *, *, #35180, .T. ) ;
#7332 = CARTESIAN_POINT ( 'NONE',  ( 0.000000000000000000, 110.5549999999999926, -9.525000000000000355 ) ) ;
#7333 = CARTESIAN_POINT ( 'NONE',  ( -68.75707362346616947, -5.598654528085801552, 7.705886871421367523 ) ) ;
#7334 = ORIENTED_EDGE ( 'NONE', *, *, #12935, .F. ) ;
#7335 = CARTESIAN_POINT ( 'NONE',  ( -9.000000000000003553, 27.74999999999998934, -3.750000000000000000 ) ) ;
#7336 = ORIENTED_EDGE ( 'NONE', *, *, #41987, .T. ) ;
#7337 =( GEOMETRIC_REPRESENTATION_CONTEXT ( 3 ) GLOBAL_UNCERTAINTY_ASSIGNED_CONTEXT ( ( #58818 ) ) GLOBAL_UNIT_ASSIGNED_CONTEXT ( ( #53224, #15952, #59504 ) ) REPRESENTATION_CONTEXT ( 'NONE', 'WORKASPACE' ) );
#7338 = ORIENTED_EDGE ( 'NONE', *, *, #47948, .T. ) ;
#7339 = CARTESIAN_POINT ( 'NONE',  ( -74.13095319853044884, 9.253562910438322575, -6.241030289661791741 ) ) ;
#7340 = CARTESIAN_POINT ( 'NONE',  ( -13.75000000000000533, 30.74999999999999289, 4.000000000000000000 ) ) ;
#7341 = PLANE ( 'NONE',  #2449 ) ;
#7342 = FACE_OUTER_BOUND ( 'NONE', #52596, .T. ) ;
#7343 = EDGE_LOOP ( 'NONE', ( #49691, #5233, #33704, #53413 ) ) ;
#7344 = B_SPLINE_CURVE_WITH_KNOTS ( 'NONE', 3,
 ( #6094, #17381, #22981, #23651, #45157, #23312, #28911, #49055 ),
 .UNSPECIFIED., .F., .F.,
 ( 4, 2, 2, 4 ),
 ( 1.301042606982605321E-18, 0.0004249208466734727776, 0.0008498416933469442542, 0.001699683386693887207 ),
 .UNSPECIFIED. ) ;
#7345 = CARTESIAN_POINT ( 'NONE',  ( 6.826472737025119919, 136.8929263765338362, 4.959722759717908325 ) ) ;
#7346 = FACE_OUTER_BOUND ( 'NONE', #59226, .T. ) ;
#7347 = DIRECTION ( 'NONE',  ( 1.000000000000000000, 0.000000000000000000, 0.000000000000000000 ) ) ;
#7348 = PRESENTATION_LAYER_ASSIGNMENT (  '', '', ( #544 ) ) ;
#7349 = CARTESIAN_POINT ( 'NONE',  ( -24.00000000000000000, 0.000000000000000000, 3.000000000000000000 ) ) ;
#7350 = EDGE_CURVE ( 'NONE', #55574, #54295, #58426, .T. ) ;
#7351 = ORIENTED_EDGE ( 'NONE', *, *, #24941, .F. ) ;
#7352 = ORIENTED_EDGE ( 'NONE', *, *, #9176, .F. ) ;
#7353 = DIRECTION ( 'NONE',  ( 0.000000000000000000, 0.000000000000000000, 1.000000000000000000 ) ) ;
#7354 = COLOUR_RGB ( '', 0.66274510, 0.83137255, 0.94901961) ;
#7355 = FACE_OUTER_BOUND ( 'NONE', #49634, .T. ) ;
#7356 =( LENGTH_UNIT ( ) NAMED_UNIT ( * ) SI_UNIT ( .MILLI., .METRE. ) );
#7357 = CARTESIAN_POINT ( 'NONE',  ( 0.000000000000000000, 87.30187232391182306, 8.025000000000000355 ) ) ;
#7358 = CONICAL_SURFACE ( 'NONE', #54538, 9.000000000000007105, 0.7853981633974500554 ) ;
#7359 = CARTESIAN_POINT ( 'NONE',  ( -136.4050000000000296, -2.607480562269069768, 8.024999999999991473 ) ) ;
#7360 = DIRECTION ( 'NONE',  ( 1.000000000000000000, 0.000000000000000000, 0.000000000000000000 ) ) ;
#7361 = ADVANCED_FACE ( 'NONE', ( #36800 ), #16379, .T. ) ;
#7362 = ORIENTED_EDGE ( 'NONE', *, *, #21038, .T. ) ;
#7363 = DIRECTION ( 'NONE',  ( -1.000000000000000000, -0.000000000000000000, -0.000000000000000000 ) ) ;
#7364 = CARTESIAN_POINT ( 'NONE',  ( -45.00000000000000000, 9.027015924850157802, -6.778771685250380763 ) ) ;
#7365 = ORIENTED_EDGE ( 'NONE', *, *, #25323, .T. ) ;
#7366 = ORIENTED_EDGE ( 'NONE', *, *, #66820, .T. ) ;
#7367 = LINE ( 'NONE', #55887, #31686 ) ;
#7368 = CYLINDRICAL_SURFACE ( 'NONE', #31160, 113.0000000000000284 ) ;
#7369 = CARTESIAN_POINT ( 'NONE',  ( -51.35499999999998266, -4.716976649647093289, -6.492361379858945902 ) ) ;
#7371 = ORIENTED_EDGE ( 'NONE', *, *, #15052, .T. ) ;
#7370 = TOROIDAL_SURFACE ( 'NONE', #23137, 0.5000000000000000000, 0.2500000000000000000 ) ;
#7372 = CARTESIAN_POINT ( 'NONE',  ( 3.728548500389067488, 7.000000000000006217, 0.9264520766856050304 ) ) ;
#7373 = CARTESIAN_POINT ( 'NONE',  ( -49.75000000000000000, 4.336808689942018722E-16, 16.97056274847714974 ) ) ;
#7374 = B_SPLINE_CURVE_WITH_KNOTS ( 'NONE', 3,
 ( #17533, #23813, #51253, #1614, #23140, #18864, #44630, #66027, #7302 ),
 .UNSPECIFIED., .F., .F.,
 ( 4, 2, 1, 2, 4 ),
 ( 0.008420575619166656769, 0.008943833652465342163, 0.009467091685764029291, 0.01051360775236140181, 0.01260663988555614685 ),
 .UNSPECIFIED. ) ;
#7375 = DIRECTION ( 'NONE',  ( 0.5000000000000000000, 0.000000000000000000, -0.8660254037844385966 ) ) ;
#7376 = ORIENTED_EDGE ( 'NONE', *, *, #39756, .T. ) ;
#7377 =( BOUNDED_CURVE ( )  B_SPLINE_CURVE ( 3, ( #20532, #14933, #68374, #57832 ),
 .UNSPECIFIED., .F., .F. ) 
 B_SPLINE_CURVE_WITH_KNOTS ( ( 4, 4 ),
 ( 4.712388980384689674, 6.283185307179586232 ),
 .UNSPECIFIED. ) 
 CURVE ( )  GEOMETRIC_REPRESENTATION_ITEM ( )  RATIONAL_B_SPLINE_CURVE ( ( 1.000000000000000000, 0.8047378541243649375, 0.8047378541243649375, 1.000000000000000000 ) ) 
 REPRESENTATION_ITEM ( '' )  );
#7378 = SURFACE_STYLE_FILL_AREA ( #2740 ) ;
#7379 = CARTESIAN_POINT ( 'NONE',  ( 30.25000000000000711, 18.99999999999997868, 4.000000000000000000 ) ) ;
#7380 =( GEOMETRIC_REPRESENTATION_CONTEXT ( 3 ) GLOBAL_UNCERTAINTY_ASSIGNED_CONTEXT ( ( #4643 ) ) GLOBAL_UNIT_ASSIGNED_CONTEXT ( ( #54692, #22017, #61357 ) ) REPRESENTATION_CONTEXT ( 'NONE', 'WORKASPACE' ) );
#7381 = CARTESIAN_POINT ( 'NONE',  ( -6.667623377008405683, 2.231456886122025196, -6.451337545287480602 ) ) ;
#7382 = CARTESIAN_POINT ( 'NONE',  ( 4.630149463674436916, 154.5000000000001137, -8.335376919559424280 ) ) ;
#7383 = CARTESIAN_POINT ( 'NONE',  ( 0.000000000000000000, 1.999999999999998668, 0.000000000000000000 ) ) ;
#7384 = DIRECTION ( 'NONE',  ( -1.000000000000000000, 9.376883653928687363E-17, 0.000000000000000000 ) ) ;
#7385 = CARTESIAN_POINT ( 'NONE',  ( -101.0949999999999847, -2.607480562269071545, -8.024999999999991473 ) ) ;
#7386 = CARTESIAN_POINT ( 'NONE',  ( -10.01517768586949231, 114.3049999999999926, -6.132527647946036459E-16 ) ) ;
#7387 = CARTESIAN_POINT ( 'NONE',  ( -82.64499999999998181, 4.716976649647091513, -6.492361379858946790 ) ) ;
#7388 = EDGE_CURVE ( 'NONE', #67224, #23974, #26852, .T. ) ;
#7389 =( NAMED_UNIT ( * ) SI_UNIT ( $, .STERADIAN. ) SOLID_ANGLE_UNIT ( ) );
#7390 = CARTESIAN_POINT ( 'NONE',  ( 66.24999999999998579, 33.99999999999999289, -3.750000000000000000 ) ) ;
#7391 = CARTESIAN_POINT ( 'NONE',  ( 52.75000000000000000, 25.24999999999998579, 3.750000000000000000 ) ) ;
#7392 = UNCERTAINTY_MEASURE_WITH_UNIT (LENGTH_MEASURE( 1.000000000000000082E-05 ), #22652, 'distance_accuracy_value', 'NONE');
#7393 = FACE_OUTER_BOUND ( 'NONE', #27656, .T. ) ;
#7394 = CIRCLE ( 'NONE', #68061, 0.2500000000000002220 ) ;
#7395 = EDGE_LOOP ( 'NONE', ( #1992, #5668, #21505, #62412 ) ) ;
#7396 = EDGE_CURVE ( 'NONE', #65503, #62949, #6131, .T. ) ;
#7397 = CARTESIAN_POINT ( 'NONE',  ( -118.1929263765337907, -10.01517768586948698, 6.132527647946031529E-16 ) ) ;
#7398 = SURFACE_SIDE_STYLE ('',( #38414 ) ) ;
#7399 = CARTESIAN_POINT ( 'NONE',  ( -139.1950000000000216, 8.437984349512085203, -1.550032578732815448E-15 ) ) ;
#7400 =( LENGTH_UNIT ( ) NAMED_UNIT ( * ) SI_UNIT ( .MILLI., .METRE. ) );
#7401 = AXIS2_PLACEMENT_3D ( 'NONE', #31331, #21135, #4233 ) ;
#7402 = EDGE_CURVE ( 'NONE', #57125, #39571, #56148, .T. ) ;
#7403 = FILL_AREA_STYLE ('',( #12657 ) ) ;
#7404 = STYLED_ITEM ( 'NONE', ( #41709 ), #49780 ) ;
#7405 = FILL_AREA_STYLE ('',( #45757 ) ) ;
#7406 = ORIENTED_EDGE ( 'NONE', *, *, #33745, .T. ) ;
#7407 = VERTEX_POINT ( 'NONE', #44510 ) ;
#7408 = PRESENTATION_LAYER_ASSIGNMENT (  '', '', ( #68073 ) ) ;
#7409 = CARTESIAN_POINT ( 'NONE',  ( 24.21231517720798010, 99.99999999999998579, -7.000000000000000000 ) ) ;
#7410 = CARTESIAN_POINT ( 'NONE',  ( 0.000000000000000000, 87.30187232391182306, 0.000000000000000000 ) ) ;
#7411 =( LENGTH_UNIT ( ) NAMED_UNIT ( * ) SI_UNIT ( .MILLI., .METRE. ) );
#7412 = CARTESIAN_POINT ( 'NONE',  ( -24.21231517720798010, 113.4999999999999858, 9.500000000000000000 ) ) ;
#7413 = LINE ( 'NONE', #23569, #50909 ) ;
#7414 = DIRECTION ( 'NONE',  ( 0.000000000000000000, 0.000000000000000000, 1.000000000000000000 ) ) ;
#7416 = ADVANCED_FACE ( 'NONE', ( #11401 ), #3093, .T. ) ;
#7415 = DIRECTION ( 'NONE',  ( -0.000000000000000000, -1.000000000000000000, 0.000000000000000000 ) ) ;
#7417 = ORIENTED_EDGE ( 'NONE', *, *, #62251, .F. ) ;
#7418 = CARTESIAN_POINT ( 'NONE',  ( -138.3550000000000182, -4.716976649647093289, -6.492361379858945902 ) ) ;
#7419 = ORIENTED_EDGE ( 'NONE', *, *, #24557, .T. ) ;
#7420 = MECHANICAL_DESIGN_GEOMETRIC_PRESENTATION_REPRESENTATION (  '', ( #24220 ), #8530 ) ;
#7421 = ORIENTED_EDGE ( 'NONE', *, *, #14706, .F. ) ;
#7422 = FACE_OUTER_BOUND ( 'NONE', #49574, .T. ) ;
#7423 = DIRECTION ( 'NONE',  ( 1.000000000000000000, 0.000000000000000000, 0.000000000000000000 ) ) ;
#7424 = EDGE_LOOP ( 'NONE', ( #63041, #68779, #10791, #8802 ) ) ;
#7425 = CIRCLE ( 'NONE', #620, 0.5000000000000004441 ) ;
#7426 = DIRECTION ( 'NONE',  ( 0.000000000000000000, 0.000000000000000000, -1.000000000000000000 ) ) ;
#7427 = SURFACE_SIDE_STYLE ('',( #45445 ) ) ;
#7428 = CARTESIAN_POINT ( 'NONE',  ( -5.598654528085808657, 134.6449999999999818, 7.705886871421373741 ) ) ;
#7429 = SURFACE_STYLE_FILL_AREA ( #12678 ) ;
#7430 = CIRCLE ( 'NONE', #34378, 0.2500000000000002220 ) ;
#7431 = ORIENTED_EDGE ( 'NONE', *, *, #65749, .T. ) ;
#7432 = SURFACE_STYLE_USAGE ( .BOTH. , #28503 ) ;
#7433 = CARTESIAN_POINT ( 'NONE',  ( -5.598654528085808657, 141.7549999999999955, 7.705886871421373741 ) ) ;
#7434 = CARTESIAN_POINT ( 'NONE',  ( -54.20499999999997698, -2.607480562269071545, -8.024999999999991473 ) ) ;
#7435 = SURFACE_STYLE_FILL_AREA ( #2063 ) ;
#7436 = VERTEX_POINT ( 'NONE', #19451 ) ;
#7437 = CARTESIAN_POINT ( 'NONE',  ( 9.058813317711337021, 157.6550000000000011, 2.943386871421375783 ) ) ;
#7438 = DIRECTION ( 'NONE',  ( -1.000000000000000000, 0.000000000000000000, 0.000000000000000000 ) ) ;
#7439 = UNCERTAINTY_MEASURE_WITH_UNIT (LENGTH_MEASURE( 1.000000000000000082E-05 ), #17248, 'distance_accuracy_value', 'NONE');
#7440 = SURFACE_SIDE_STYLE ('',( #7758 ) ) ;
#7441 = FACE_OUTER_BOUND ( 'NONE', #53953, .T. ) ;
#7442 = ORIENTED_EDGE ( 'NONE', *, *, #10436, .T. ) ;
#7443 = VERTEX_POINT ( 'NONE', #51138 ) ;
#7444 = SURFACE_STYLE_USAGE ( .BOTH. , #23268 ) ;
#7445 = DIRECTION ( 'NONE',  ( -0.000000000000000000, -0.000000000000000000, 1.000000000000000000 ) ) ;
#7446 = CARTESIAN_POINT ( 'NONE',  ( -51.51031159759250500, -10.16650056460914087, 4.260379760314384257 ) ) ;
#7447 = CARTESIAN_POINT ( 'NONE',  ( -166.1049999999999898, -6.826472737025115478, 4.959722759717900331 ) ) ;
#7448 = ORIENTED_EDGE ( 'NONE', *, *, #48281, .T. ) ;
#7449 = EDGE_CURVE ( 'NONE', #24594, #58716, #4973, .T. ) ;
#7450 = SURFACE_STYLE_FILL_AREA ( #2082 ) ;
#7451 = UNCERTAINTY_MEASURE_WITH_UNIT (LENGTH_MEASURE( 1.000000000000000082E-05 ), #28264, 'distance_accuracy_value', 'NONE');
#7452 = CIRCLE ( 'NONE', #52405, 14.49999999999999822 ) ;
#7453 = CARTESIAN_POINT ( 'NONE',  ( 1.709458476932651091E-14, 43.00000000000000000, 35.50000000000000000 ) ) ;
#7454 = VERTEX_POINT ( 'NONE', #62691 ) ;
#7455 = EDGE_LOOP ( 'NONE', ( #8315, #32600, #10237, #38297 ) ) ;
#7456 = DIRECTION ( 'NONE',  ( 0.000000000000000000, 0.000000000000000000, 1.000000000000000000 ) ) ;
#7457 = CARTESIAN_POINT ( 'NONE',  ( -77.90500000000000114, 2.607480562269068880, -8.024999999999993250 ) ) ;
#7458 = ORIENTED_EDGE ( 'NONE', *, *, #67795, .T. ) ;
#7459 = DIRECTION ( 'NONE',  ( -0.000000000000000000, -1.000000000000000000, -0.000000000000000000 ) ) ;
#7460 = CARTESIAN_POINT ( 'NONE',  ( -84.05707362346618083, 0.000000000000000000, 9.524999999999991473 ) ) ;
#7461 = CARTESIAN_POINT ( 'NONE',  ( 0.000000000000000000, -2.500000000000000000, 0.000000000000000000 ) ) ;
#7462 = ORIENTED_EDGE ( 'NONE', *, *, #36515, .F. ) ;
#7463 = FILL_AREA_STYLE_COLOUR ( '', #3385 ) ;
#7465 = CARTESIAN_POINT ( 'NONE',  ( 12.72792206135785698, 149.9999999999999716, 10.00000000000000000 ) ) ;
#7464 = FILL_AREA_STYLE_COLOUR ( '', #18818 ) ;
#7466 = CIRCLE ( 'NONE', #26526, 5.499999999999976907 ) ;
#7467 = CARTESIAN_POINT ( 'NONE',  ( 3.094860106618431583, 141.0949999999999989, 9.525000000000000355 ) ) ;
#7468 = CARTESIAN_POINT ( 'NONE',  ( -104.8449999999999989, -7.632228543268599452, 2.479861379858951054 ) ) ;
#7469 = EDGE_CURVE ( 'NONE', #34188, #24855, #61317, .T. ) ;
#7470 =( NAMED_UNIT ( * ) PLANE_ANGLE_UNIT ( ) SI_UNIT ( $, .RADIAN. ) );
#7472 = DIRECTION ( 'NONE',  ( -1.000000000000000000, -0.000000000000000000, -0.000000000000000000 ) ) ;
#7471 = DIRECTION ( 'NONE',  ( -1.000000000000000000, 0.000000000000000000, 0.000000000000000000 ) ) ;
#7473 = CARTESIAN_POINT ( 'NONE',  ( -155.9929263765338021, 8.102448949553171076, -5.886773742842744461 ) ) ;
#7474 = CARTESIAN_POINT ( 'NONE',  ( -163.9449999999999932, -9.827790563157499189E-16, -8.024999999999991473 ) ) ;
#7475 = ADVANCED_FACE ( 'NONE', ( #50781 ), #40952, .F. ) ;
#7476 =( LENGTH_UNIT ( ) NAMED_UNIT ( * ) SI_UNIT ( .MILLI., .METRE. ) );
#7477 = ORIENTED_EDGE ( 'NONE', *, *, #28739, .T. ) ;
#7478 = DIRECTION ( 'NONE',  ( 0.000000000000000000, 0.000000000000000000, -1.000000000000000000 ) ) ;
#7479 = VERTEX_POINT ( 'NONE', #13837 ) ;
#7480 = EDGE_CURVE ( 'NONE', #8394, #24181, #7515, .T. ) ;
#7481 = CARTESIAN_POINT ( 'NONE',  ( -65.24292637653380211, 5.598654528085804216, 7.705886871421366635 ) ) ;
#7482 = CARTESIAN_POINT ( 'NONE',  ( 12.50000000000000355, 30.74999999999998579, 3.750000000000000000 ) ) ;
#7483 = EDGE_CURVE ( 'NONE', #54909, #36200, #46233, .T. ) ;
#7484 = CARTESIAN_POINT ( 'NONE',  ( -141.4429263765337907, -1.166476076187852838E-15, -9.524999999999991473 ) ) ;
#7485 = LINE ( 'NONE', #66211, #24628 ) ;
#7486 = CARTESIAN_POINT ( 'NONE',  ( -9.827790563157511022E-16, 143.5570736234661524, 8.025000000000000355 ) ) ;
#7487 = VECTOR ( 'NONE', #58569, 1000.000000000000000 ) ;
#7488 = EDGE_CURVE ( 'NONE', #37840, #1408, #4925, .T. ) ;
#7489 = EDGE_LOOP ( 'NONE', ( #55344, #33433, #240 ) ) ;
#7490 = CARTESIAN_POINT ( 'NONE',  ( -168.8049999999999500, -8.437984349512086979, 5.166775262442717831E-16 ) ) ;
#7491 = VECTOR ( 'NONE', #63051, 1000.000000000000000 ) ;
#7492 = EDGE_LOOP ( 'NONE', ( #37708, #39844, #19222, #26498 ) ) ;
#7493 = TOROIDAL_SURFACE ( 'NONE', #6332, 1.000000000000000000, 0.5000000000000000000 ) ;
#7494 = B_SPLINE_CURVE_WITH_KNOTS ( 'NONE', 3,
 ( #12222, #2304, #40054, #18572, #44648, #23479 ),
 .UNSPECIFIED., .F., .F.,
 ( 4, 2, 4 ),
 ( 0.004189585287972439308, 0.006269578072783813308, 0.008349570857595188175 ),
 .UNSPECIFIED. ) ;
#7495 = CARTESIAN_POINT ( 'NONE',  ( 6.826472737025121695, 150.6070736234661069, -4.959722759717905660 ) ) ;
#7496 = ORIENTED_EDGE ( 'NONE', *, *, #60988, .F. ) ;
#7497 = CARTESIAN_POINT ( 'NONE',  ( 8.102448949553179958, 112.5049999999999670, 5.886773742842750679 ) ) ;
#7498 = CARTESIAN_POINT ( 'NONE',  ( -87.95499999999999829, -7.632228543268599452, 2.479861379858951054 ) ) ;
#7499 = SURFACE_SIDE_STYLE ('',( #18057 ) ) ;
#7500 = CARTESIAN_POINT ( 'NONE',  ( -3.094860106618434248, 132.9050000000000011, 9.525000000000000355 ) ) ;
#7501 = UNCERTAINTY_MEASURE_WITH_UNIT (LENGTH_MEASURE( 1.000000000000000082E-05 ), #9904, 'distance_accuracy_value', 'NONE');
#7502 = PLANE ( 'NONE',  #41022 ) ;
#7503 = SURFACE_SIDE_STYLE ('',( #13460 ) ) ;
#7504 = COLOUR_RGB ( '', 0.09019608, 0.27058824, 0.51372549) ;
#7505 = FILL_AREA_STYLE ('',( #65901 ) ) ;
#7506 = DIRECTION ( 'NONE',  ( -0.000000000000000000, -1.000000000000000000, -0.000000000000000000 ) ) ;
#7507 = DIRECTION ( 'NONE',  ( -0.2413793103448194644, -0.9704308468600220117, 0.000000000000000000 ) ) ;
#7508 = ORIENTED_EDGE ( 'NONE', *, *, #56153, .T. ) ;
#7509 = SURFACE_STYLE_FILL_AREA ( #60958 ) ;
#7510 = DIRECTION ( 'NONE',  ( -1.156482317317873451E-16, 1.000000000000000000, 0.000000000000000000 ) ) ;
#7511 = CARTESIAN_POINT ( 'NONE',  ( -54.44499999999999318, 0.000000000000000000, 8.024999999999991473 ) ) ;
#7512 = EDGE_LOOP ( 'NONE', ( #39055, #59637 ) ) ;
#7513 = CARTESIAN_POINT ( 'NONE',  ( -71.50000000000000000, 35.92875272052971525, -7.500000000000000000 ) ) ;
#7514 = DIRECTION ( 'NONE',  ( 0.000000000000000000, -1.000000000000000000, 1.734723475976805615E-16 ) ) ;
#7515 = LINE ( 'NONE', #62370, #19526 ) ;
#7516 = FACE_OUTER_BOUND ( 'NONE', #35631, .T. ) ;
#7517 = VERTEX_POINT ( 'NONE', #23690 ) ;
#7518 = CYLINDRICAL_SURFACE ( 'NONE', #49417, 8.025000000000000355 ) ;
#7519 = CARTESIAN_POINT ( 'NONE',  ( -55.04499999999998039, 7.632228543268600340, 2.479861379858949277 ) ) ;
#7520 =( NAMED_UNIT ( * ) PLANE_ANGLE_UNIT ( ) SI_UNIT ( $, .RADIAN. ) );
#7521 = ORIENTED_EDGE ( 'NONE', *, *, #62499, .T. ) ;
#7522 = CARTESIAN_POINT ( 'NONE',  ( -75.00000000000000000, 8.674606743306283008, 5.942398972768304866 ) ) ;
#7523 = CARTESIAN_POINT ( 'NONE',  ( -105.3549999999999898, -4.716976649647093289, -6.492361379858945902 ) ) ;
#7524 = ORIENTED_EDGE ( 'NONE', *, *, #14362, .F. ) ;
#7525 = DIRECTION ( 'NONE',  ( 0.000000000000000000, 0.000000000000000000, 1.000000000000000000 ) ) ;
#7526 = DIRECTION ( 'NONE',  ( -0.000000000000000000, -0.000000000000000000, 1.000000000000000000 ) ) ;
#7527 = CARTESIAN_POINT ( 'NONE',  ( -152.7570736234661979, -5.598654528085801552, 7.705886871421367523 ) ) ;
#7528 = CARTESIAN_POINT ( 'NONE',  ( -59.00707362346617657, -8.102448949553174629, -5.886773742842741797 ) ) ;
#7529 = CARTESIAN_POINT ( 'NONE',  ( -5.598654528085808657, 146.6450000000000102, 7.705886871421373741 ) ) ;
#7530 = CARTESIAN_POINT ( 'NONE',  ( -80.60707362346614957, -8.102448949553172852, 5.886773742842742685 ) ) ;
#7531 = PRODUCT_DEFINITION_SHAPE ( 'NONE', 'NONE',  #69700 ) ;
#7532 = FACE_OUTER_BOUND ( 'NONE', #45004, .T. ) ;
#7533 = ORIENTED_EDGE ( 'NONE', *, *, #35912, .F. ) ;
#7534 = DIRECTION ( 'NONE',  ( -0.000000000000000000, -0.000000000000000000, -1.000000000000000000 ) ) ;
#7535 = SURFACE_SIDE_STYLE ('',( #60989 ) ) ;
#7536 = AXIS2_PLACEMENT_3D ( 'NONE', #44176, #53970, #5772 ) ;
#7537 = CARTESIAN_POINT ( 'NONE',  ( -135.6550000000000011, -7.632228543268600340, -2.479861379858950166 ) ) ;
#7538 = DIRECTION ( 'NONE',  ( 0.000000000000000000, -1.000000000000000000, 0.000000000000000000 ) ) ;
#7539 = AXIS2_PLACEMENT_3D ( 'NONE', #46934, #8305, #68695 ) ;
#7540 = CARTESIAN_POINT ( 'NONE',  ( -147.4429263765338192, -1.166476076187852838E-15, -9.524999999999991473 ) ) ;
#7541 = DIRECTION ( 'NONE',  ( 0.000000000000000000, 0.000000000000000000, 1.000000000000000000 ) ) ;
#7542 = CARTESIAN_POINT ( 'NONE',  ( -139.4949999999999761, 6.826472737025113702, -4.959722759717902107 ) ) ;
#7543 = EDGE_CURVE ( 'NONE', #42377, #35623, #33057, .T. ) ;
#7544 = CARTESIAN_POINT ( 'NONE',  ( -125.0949999999999847, -2.607480562269071545, -8.024999999999991473 ) ) ;
#7545 = CARTESIAN_POINT ( 'NONE',  ( 45.00000000000000000, -1.469576158976824618E-14, -9.500000000000000000 ) ) ;
#7546 = ORIENTED_EDGE ( 'NONE', *, *, #69121, .T. ) ;
#7547 = EDGE_CURVE ( 'NONE', #31166, #57680, #8522, .T. ) ;
#7548 = CARTESIAN_POINT ( 'NONE',  ( 10.00000000000000533, 50.00000000000000000, -46.00000000000000000 ) ) ;
#7549 = EDGE_CURVE ( 'NONE', #28212, #46059, #34581, .T. ) ;
#7550 = CARTESIAN_POINT ( 'NONE',  ( -120.4429263765338050, -1.166476076187852838E-15, -9.524999999999991473 ) ) ;
#7551 = CARTESIAN_POINT ( 'NONE',  ( -178.3429263765338249, -9.058813317711329915, 2.943386871421371787 ) ) ;
#7552 = CARTESIAN_POINT ( 'NONE',  ( -51.44499999999999318, 0.000000000000000000, 8.024999999999991473 ) ) ;
#7553 = EDGE_CURVE ( 'NONE', #16526, #22006, #6080, .T. ) ;
#7554 = AXIS2_PLACEMENT_3D ( 'NONE', #689, #37766, #4022 ) ;
#7555 = EDGE_CURVE ( 'NONE', #63218, #16463, #44294, .T. ) ;
#7556 = DIRECTION ( 'NONE',  ( 0.000000000000000000, 0.000000000000000000, 1.000000000000000000 ) ) ;
#7557 = EDGE_CURVE ( 'NONE', #1034, #61310, #3224, .T. ) ;
#7558 = DIRECTION ( 'NONE',  ( 0.000000000000000000, 0.000000000000000000, 1.000000000000000000 ) ) ;
#7559 = PRESENTATION_STYLE_ASSIGNMENT (( #23059 ) ) ;
#7560 = CARTESIAN_POINT ( 'NONE',  ( -99.89292637653380780, -8.102448949553172852, -5.886773742842741797 ) ) ;
#7561 = SHAPE_DEFINITION_REPRESENTATION ( #68685, #10054 ) ;
#7562 = CARTESIAN_POINT ( 'NONE',  ( 15.00000000000000000, 8.000000000000000000, -3.500000000000017764 ) ) ;
#7563 = CARTESIAN_POINT ( 'NONE',  ( 7.399999999999989697, 11.99999999999999289, -4.000000000000000000 ) ) ;
#7564 = ADVANCED_FACE ( 'NONE', ( #67651 ), #61644, .T. ) ;
#7565 = CYLINDRICAL_SURFACE ( 'NONE', #19107, 4.999999999999997335 ) ;
#7566 = FILL_AREA_STYLE ('',( #12482 ) ) ;
#7567 = CARTESIAN_POINT ( 'NONE',  ( -40.99999999999998579, 108.0041655821620168, 3.000000000000000888 ) ) ;
#7568 = DIRECTION ( 'NONE',  ( 1.000000000000000000, 0.000000000000000000, 0.000000000000000000 ) ) ;
#7569 = ORIENTED_EDGE ( 'NONE', *, *, #9138, .F. ) ;
#7570 = DIRECTION ( 'NONE',  ( -1.073081856240828813E-16, 0.000000000000000000, 1.000000000000000000 ) ) ;
#7571 = DIRECTION ( 'NONE',  ( 0.000000000000000000, 1.000000000000000000, 0.000000000000000000 ) ) ;
#7572 = DIRECTION ( 'NONE',  ( 0.000000000000000000, 0.000000000000000000, 1.000000000000000000 ) ) ;
#7573 = ORIENTED_EDGE ( 'NONE', *, *, #35279, .T. ) ;
#7574 = DIRECTION ( 'NONE',  ( -1.000000000000000000, 0.000000000000000000, 0.000000000000000000 ) ) ;
#7575 = CARTESIAN_POINT ( 'NONE',  ( -2.607480562269073765, 124.2070736234661581, -8.025000000000000355 ) ) ;
#7576 = SURFACE_STYLE_USAGE ( .BOTH. , #38941 ) ;
#7577 = DIRECTION ( 'NONE',  ( -1.000000000000000000, -0.000000000000000000, -0.000000000000000000 ) ) ;
#7578 = TOROIDAL_SURFACE ( 'NONE', #56997, 8.500000000000012434, 0.5000000000000000000 ) ;
#7579 = EDGE_LOOP ( 'NONE', ( #44012, #33343, #27416, #16439 ) ) ;
#7580 =( GEOMETRIC_REPRESENTATION_CONTEXT ( 3 ) GLOBAL_UNCERTAINTY_ASSIGNED_CONTEXT ( ( #6577 ) ) GLOBAL_UNIT_ASSIGNED_CONTEXT ( ( #46786, #50618, #30173 ) ) REPRESENTATION_CONTEXT ( 'NONE', 'WORKASPACE' ) );
#7581 = CARTESIAN_POINT ( 'NONE',  ( -94.49292637653380211, -8.102448949553174629, 5.886773742842742685 ) ) ;
#7582 = DIRECTION ( 'NONE',  ( -1.000000000000000000, -0.000000000000000000, 1.300977106640434891E-16 ) ) ;
#7583 = AXIS2_PLACEMENT_3D ( 'NONE', #14108, #13748, #56667 ) ;
#7584 = SURFACE_STYLE_FILL_AREA ( #12861 ) ;
#7585 = DIRECTION ( 'NONE',  ( 0.000000000000000000, 1.000000000000000000, -0.000000000000000000 ) ) ;
#7586 = CARTESIAN_POINT ( 'NONE',  ( -83.84499999999998465, -7.632228543268599452, 2.479861379858951054 ) ) ;
#7587 = ORIENTED_EDGE ( 'NONE', *, *, #28974, .F. ) ;
#7588 = EDGE_CURVE ( 'NONE', #19233, #45842, #15111, .T. ) ;
#7589 = CARTESIAN_POINT ( 'NONE',  ( -6.826472737025120807, 123.3929263765338078, -4.959722759717907437 ) ) ;
#7590 = CARTESIAN_POINT ( 'NONE',  ( 0.000000000000000000, 122.9429263765338192, -8.025000000000000355 ) ) ;
#7591 = ORIENTED_EDGE ( 'NONE', *, *, #96, .F. ) ;
#7592 = SPHERICAL_SURFACE ( 'NONE', #51602, 0.5000000000000000000 ) ;
#7593 = FILL_AREA_STYLE ('',( #13207 ) ) ;
#7594 = AXIS2_PLACEMENT_3D ( 'NONE', #65730, #49568, #1662 ) ;
#7595 = DIRECTION ( 'NONE',  ( 0.000000000000000000, 0.000000000000000000, -1.000000000000000000 ) ) ;
#7596 = VERTEX_POINT ( 'NONE', #31654 ) ;
#7597 = CARTESIAN_POINT ( 'NONE',  ( -15.98999599679679839, 117.9999999999999716, -7.500000000000000000 ) ) ;
#7598 = ORIENTED_EDGE ( 'NONE', *, *, #29025, .T. ) ;
#7599 = DIRECTION ( 'NONE',  ( -0.000000000000000000, 1.000000000000000000, -0.000000000000000000 ) ) ;
#7600 =( NAMED_UNIT ( * ) SI_UNIT ( $, .STERADIAN. ) SOLID_ANGLE_UNIT ( ) );
#7601 = DIRECTION ( 'NONE',  ( -1.000000000000000000, -7.709882115452468306E-16, 0.000000000000000000 ) ) ;
#7602 = CARTESIAN_POINT ( 'NONE',  ( -177.5070736234661979, 8.102448949553176405, 5.886773742842740909 ) ) ;
#7603 = DIRECTION ( 'NONE',  ( 0.000000000000000000, 0.000000000000000000, -1.000000000000000000 ) ) ;
#7604 = CARTESIAN_POINT ( 'NONE',  ( -114.8070736234661808, 10.01517768586948698, -1.839758294383808571E-15 ) ) ;
#7605 = DIRECTION ( 'NONE',  ( -1.000000000000000000, 0.000000000000000000, 0.000000000000000000 ) ) ;
#7606 = ORIENTED_EDGE ( 'NONE', *, *, #45146, .T. ) ;
#7607 = CARTESIAN_POINT ( 'NONE',  ( -83.49999999999998579, 4.336808689942018722E-16, 24.00000000000000000 ) ) ;
#7608 = DIRECTION ( 'NONE',  ( 0.000000000000000000, -1.000000000000000000, 0.000000000000000000 ) ) ;
#7609 = CARTESIAN_POINT ( 'NONE',  ( -24.00000000000000355, 37.00000000000000000, -3.000000000000000000 ) ) ;
#7610 = ORIENTED_EDGE ( 'NONE', *, *, #51926, .F. ) ;
#7611 = CARTESIAN_POINT ( 'NONE',  ( -160.5550000000000068, 0.000000000000000000, 8.024999999999991473 ) ) ;
#7612 = EDGE_CURVE ( 'NONE', #23616, #13621, #55749, .T. ) ;
#7613 = CARTESIAN_POINT ( 'NONE',  ( -74.75000000000000000, -3.000000000000000000, 6.000000000000001776 ) ) ;
#7614 = DIRECTION ( 'NONE',  ( -0.000000000000000000, 0.3420201433256629953, 0.9396926207859104263 ) ) ;
#7615 = CARTESIAN_POINT ( 'NONE',  ( -167.6949999999999363, -8.437984349512085203, 5.166775262442717831E-16 ) ) ;
#7616 = CARTESIAN_POINT ( 'NONE',  ( -161.3949999999999818, -6.826472737025113702, -4.959722759717900331 ) ) ;
#7617 = ORIENTED_EDGE ( 'NONE', *, *, #43345, .T. ) ;
#7618 = ADVANCED_FACE ( 'NONE', ( #54138 ), #273, .T. ) ;
#7619 = DIRECTION ( 'NONE',  ( 0.000000000000000000, 0.000000000000000000, 1.000000000000000000 ) ) ;
#7620 = PRESENTATION_STYLE_ASSIGNMENT (( #38300 ) ) ;
#7621 = CIRCLE ( 'NONE', #63762, 0.5000000000000004441 ) ;
#7622 = DIRECTION ( 'NONE',  ( -1.000000000000000000, -0.000000000000000000, -0.000000000000000000 ) ) ;
#7623 = CARTESIAN_POINT ( 'NONE',  ( -72.50499999999998124, -6.826472737025115478, -4.959722759717899443 ) ) ;
#7624 = FACE_OUTER_BOUND ( 'NONE', #49803, .T. ) ;
#7625 = FILL_AREA_STYLE ('',( #13954 ) ) ;
#7626 = AXIS2_PLACEMENT_3D ( 'NONE', #27562, #17061, #11400 ) ;
#7627 = CARTESIAN_POINT ( 'NONE',  ( -67.94499999999999318, -9.827790563157499189E-16, -8.024999999999991473 ) ) ;
#7628 = CARTESIAN_POINT ( 'NONE',  ( -5.598654528085806881, 143.8549999999999898, -7.705886871421374629 ) ) ;
#7629 = DIRECTION ( 'NONE',  ( 1.000000000000000000, 0.000000000000000000, 0.000000000000000000 ) ) ;
#7630 = EDGE_CURVE ( 'NONE', #19619, #41595, #29667, .T. ) ;
#7631 =( GEOMETRIC_REPRESENTATION_CONTEXT ( 3 ) GLOBAL_UNCERTAINTY_ASSIGNED_CONTEXT ( ( #53795 ) ) GLOBAL_UNIT_ASSIGNED_CONTEXT ( ( #32214, #47404, #11093 ) ) REPRESENTATION_CONTEXT ( 'NONE', 'WORKASPACE' ) );
#7632 = LINE ( 'NONE', #2285, #59277 ) ;
#7633 = CARTESIAN_POINT ( 'NONE',  ( -9.000000000000007105, 0.000000000000000000, 0.000000000000000000 ) ) ;
#7634 = PRESENTATION_STYLE_ASSIGNMENT (( #1260 ) ) ;
#7635 = EDGE_CURVE ( 'NONE', #5374, #24854, #5255, .T. ) ;
#7636 = SURFACE_STYLE_USAGE ( .BOTH. , #50911 ) ;
#7637 = COLOUR_RGB ( '', 0.08235294, 0.09019608, 0.10196078) ;
#7638 = AXIS2_PLACEMENT_3D ( 'NONE', #46681, #45956, #62452 ) ;
#7639 = DIRECTION ( 'NONE',  ( 1.000000000000000000, 0.000000000000000000, 0.000000000000000000 ) ) ;
#7640 =( LENGTH_UNIT ( ) NAMED_UNIT ( * ) SI_UNIT ( .MILLI., .METRE. ) );
#7641 = CARTESIAN_POINT ( 'NONE',  ( -14.98999599679679662, 146.4999999999999716, 9.500000000000000000 ) ) ;
#7642 = VERTEX_POINT ( 'NONE', #16893 ) ;
#7643 = VERTEX_POINT ( 'NONE', #69307 ) ;
#7644 = CARTESIAN_POINT ( 'NONE',  ( 4.383776131304280455, 1.496531397472844693, 9.000000000000003553 ) ) ;
#7645 = CARTESIAN_POINT ( 'NONE',  ( -9.250000000000003553, 25.24999999999998934, -3.750000000000000000 ) ) ;
#7646 = EDGE_LOOP ( 'NONE', ( #9050, #60160, #58101, #9662 ) ) ;
#7647 = ORIENTED_EDGE ( 'NONE', *, *, #32560, .F. ) ;
#7648 = FILL_AREA_STYLE_COLOUR ( '', #20817 ) ;
#7649 = CARTESIAN_POINT ( 'NONE',  ( 6.021969435454503028, -7.569642976165943615, 0.6362876910938544128 ) ) ;
#7650 = ORIENTED_EDGE ( 'NONE', *, *, #65995, .F. ) ;
#7651 = CARTESIAN_POINT ( 'NONE',  ( -1.166476076187854022E-15, 112.0549999999999926, 9.525000000000000355 ) ) ;
#7652 = DIRECTION ( 'NONE',  ( 1.000000000000000000, 0.000000000000000000, 0.000000000000000000 ) ) ;
#7653 = EDGE_LOOP ( 'NONE', ( #56692, #42268, #19459, #45343 ) ) ;
#7654 = PRESENTATION_LAYER_ASSIGNMENT (  '', '', ( #24514 ) ) ;
#7655 =( NAMED_UNIT ( * ) PLANE_ANGLE_UNIT ( ) SI_UNIT ( $, .RADIAN. ) );
#7656 =( BOUNDED_CURVE ( )  B_SPLINE_CURVE ( 2, ( #5868, #865, #65320, #48843, #69554, #38636, #541, #64960, #59684, #60040, #11852 ),
 .UNSPECIFIED., .F., .F. ) 
 B_SPLINE_CURVE_WITH_KNOTS ( ( 3, 2, 2, 2, 2, 3 ),
 ( 0.1630434782608656263, 0.1652173913043438191, 0.1673913043478220397, 0.1695652173913002603, 0.1717391304347784808, 0.1739130434782566736 ),
 .UNSPECIFIED. ) 
 CURVE ( )  GEOMETRIC_REPRESENTATION_ITEM ( )  RATIONAL_B_SPLINE_CURVE ( ( 1.000000000000088818, 0.9510565162950648244, 1.000000000000000000, 0.9510565162951535312, 1.000000000000000000, 0.9510565162951535312, 1.000000000000000000, 0.9510565162951535312, 1.000000000000000000, 0.9510565162952479001, 0.9999999999999056310 ) ) 
 REPRESENTATION_ITEM ( '' )  );
#7657 = CYLINDRICAL_SURFACE ( 'NONE', #5829, 0.2499999999999997780 ) ;
#7658 = CARTESIAN_POINT ( 'NONE',  ( -118.9449999999999932, -9.827790563157499189E-16, -8.024999999999991473 ) ) ;
#7659 = VERTEX_POINT ( 'NONE', #26375 ) ;
#7660 =( GEOMETRIC_REPRESENTATION_CONTEXT ( 3 ) GLOBAL_UNCERTAINTY_ASSIGNED_CONTEXT ( ( #14262 ) ) GLOBAL_UNIT_ASSIGNED_CONTEXT ( ( #2712, #24203, #45711 ) ) REPRESENTATION_CONTEXT ( 'NONE', 'WORKASPACE' ) );
#7661 = EDGE_CURVE ( 'NONE', #64274, #47479, #26352, .T. ) ;
#7662 = ORIENTED_EDGE ( 'NONE', *, *, #64592, .F. ) ;
#7663 = LINE ( 'NONE', #60771, #40735 ) ;
#7664 = CARTESIAN_POINT ( 'NONE',  ( -10.04082649006660155, -11.98303716040044264, -0.6588920121501417038 ) ) ;
#7665 = PLANE ( 'NONE',  #45383 ) ;
#7666 = ORIENTED_EDGE ( 'NONE', *, *, #24363, .T. ) ;
#7667 = CARTESIAN_POINT ( 'NONE',  ( 4.716976649647096842, 142.7429263765338305, 6.492361379858953896 ) ) ;
#7668 =( LENGTH_UNIT ( ) NAMED_UNIT ( * ) SI_UNIT ( .MILLI., .METRE. ) );
#7669 = FILL_AREA_STYLE ('',( #3750 ) ) ;
#7670 = AXIS2_PLACEMENT_3D ( 'NONE', #30024, #50125, #44864 ) ;
#7671 = DIRECTION ( 'NONE',  ( 1.000000000000000000, 0.000000000000000000, 0.000000000000000000 ) ) ;
#7672 = ORIENTED_EDGE ( 'NONE', *, *, #10669, .F. ) ;
#7673 = DIRECTION ( 'NONE',  ( -1.000000000000000000, -1.224646799147353207E-16, -0.000000000000000000 ) ) ;
#7674 = ORIENTED_EDGE ( 'NONE', *, *, #17439, .T. ) ;
#7675 = CARTESIAN_POINT ( 'NONE',  ( -72.00000000000000000, 14.49137674618942562, 7.000000000000000000 ) ) ;
#7677 = PRESENTATION_LAYER_ASSIGNMENT (  '', '', ( #38057 ) ) ;
#7676 = CARTESIAN_POINT ( 'NONE',  ( 41.45364736693642982, 107.0151787721003842, -3.500000000000000444 ) ) ;
#7678 = CARTESIAN_POINT ( 'NONE',  ( -134.9050000000000011, 2.607480562269068880, -8.024999999999993250 ) ) ;
#7679 =( LENGTH_UNIT ( ) NAMED_UNIT ( * ) SI_UNIT ( .MILLI., .METRE. ) );
#7680 = SURFACE_SIDE_STYLE ('',( #55169 ) ) ;
#7681 = EDGE_LOOP ( 'NONE', ( #50539, #17231, #26337, #65318 ) ) ;
#7682 = VECTOR ( 'NONE', #36178, 1000.000000000000000 ) ;
#7683 = PRODUCT_DEFINITION ( 'UNKNOWN', '', #14680, #29713 ) ;
#7684 = EDGE_CURVE ( 'NONE', #4847, #31418, #37621, .T. ) ;
#7685 = CARTESIAN_POINT ( 'NONE',  ( 22.50000000000000711, 34.24999999999999289, -3.750000000000000000 ) ) ;
#7686 = CARTESIAN_POINT ( 'NONE',  ( -157.6429263765338078, -5.598654528085801552, 7.705886871421367523 ) ) ;
#7687 = ORIENTED_EDGE ( 'NONE', *, *, #11696, .T. ) ;
#7688 = VERTEX_POINT ( 'NONE', #42960 ) ;
#7689 =( NAMED_UNIT ( * ) PLANE_ANGLE_UNIT ( ) SI_UNIT ( $, .RADIAN. ) );
#7690 = CARTESIAN_POINT ( 'NONE',  ( -32.02155123813385273, -8.772721419152789579, -1.279060632649535290 ) ) ;
#7691 = FACE_OUTER_BOUND ( 'NONE', #12900, .T. ) ;
#7692 = EDGE_CURVE ( 'NONE', #39893, #197, #2719, .T. ) ;
#7693 = CARTESIAN_POINT ( 'NONE',  ( -49.10499999999998977, -6.826472737025115478, 4.959722759717900331 ) ) ;
#7694 = ORIENTED_EDGE ( 'NONE', *, *, #9558, .T. ) ;
#7695 = CARTESIAN_POINT ( 'NONE',  ( -124.1070736234661638, 8.102448949553172852, -5.886773742842744461 ) ) ;
#7696 = ADVANCED_FACE ( 'NONE', ( #2344 ), #30822, .F. ) ;
#7697 =( NAMED_UNIT ( * ) PLANE_ANGLE_UNIT ( ) SI_UNIT ( $, .RADIAN. ) );
#7698 = DIRECTION ( 'NONE',  ( -1.000000000000000000, 0.000000000000000000, 0.000000000000000000 ) ) ;
#7699 = FILL_AREA_STYLE ('',( #29509 ) ) ;
#7700 =( NAMED_UNIT ( * ) PLANE_ANGLE_UNIT ( ) SI_UNIT ( $, .RADIAN. ) );
#7701 = ORIENTED_EDGE ( 'NONE', *, *, #15758, .T. ) ;
#7702 = CARTESIAN_POINT ( 'NONE',  ( 23.50000000000001776, 42.00000000000000000, 29.68999999999999417 ) ) ;
#7703 = EDGE_CURVE ( 'NONE', #19696, #2945, #23191, .T. ) ;
#7705 = CONICAL_SURFACE ( 'NONE', #62729, 8.025000000000000355, 0.7853981633974421728 ) ;
#7704 = DIRECTION ( 'NONE',  ( -0.000000000000000000, -0.000000000000000000, -1.000000000000000000 ) ) ;
#7706 = CARTESIAN_POINT ( 'NONE',  ( 8.437984349512095861, 117.3070736234661666, 1.550032578732816828E-15 ) ) ;
#7707 = CARTESIAN_POINT ( 'NONE',  ( -101.7549999999999812, 4.716976649647091513, -6.492361379858946790 ) ) ;
#7708 = CARTESIAN_POINT ( 'NONE',  ( 0.8807004131023399296, 154.4999999999999716, -9.494441468940317819 ) ) ;
#7709 = FILL_AREA_STYLE ('',( #40113 ) ) ;
#7710 = DIRECTION ( 'NONE',  ( 1.000000000000000000, 2.312964634635740689E-15, -0.000000000000000000 ) ) ;
#7711 = EDGE_CURVE ( 'NONE', #16182, #41197, #5025, .T. ) ;
#7712 = CARTESIAN_POINT ( 'NONE',  ( -103.6449999999999818, 4.716976649647091513, -6.492361379858946790 ) ) ;
#7713 = CARTESIAN_POINT ( 'NONE',  ( 9.058813317711338797, 118.9549999999999983, -2.943386871421372675 ) ) ;
#7714 = CARTESIAN_POINT ( 'NONE',  ( -76.34499999999998465, 7.632228543268599452, -2.479861379858951942 ) ) ;
#7715 = PRESENTATION_LAYER_ASSIGNMENT (  '', '', ( #32412 ) ) ;
#7716 = EDGE_CURVE ( 'NONE', #52417, #1012, #57816, .T. ) ;
#7717 = VECTOR ( 'NONE', #55236, 1000.000000000000000 ) ;
#7718 = CARTESIAN_POINT ( 'NONE',  ( -183.0000000000000000, 0.000000000000000000, 0.000000000000000000 ) ) ;
#7719 = CARTESIAN_POINT ( 'NONE',  ( 0.000000000000000000, 0.000000000000000000, -12.50000000000000000 ) ) ;
#7720 = VECTOR ( 'NONE', #62787, 1000.000000000000000 ) ;
#7721 = CYLINDRICAL_SURFACE ( 'NONE', #33690, 1.000000000000000888 ) ;
#7722 = CARTESIAN_POINT ( 'NONE',  ( 26.00000000000001066, 21.99999999999998224, 4.000000000000000000 ) ) ;
#7723 = ORIENTED_EDGE ( 'NONE', *, *, #32096, .T. ) ;
#7724 = CARTESIAN_POINT ( 'NONE',  ( -119.3929263765337794, 8.102448949553176405, 5.886773742842740909 ) ) ;
#7725 = ADVANCED_FACE ( 'NONE', ( #44682 ), #13298, .T. ) ;
#7726 = CARTESIAN_POINT ( 'NONE',  ( -134.0949999999999420, -2.607480562269071545, -8.024999999999991473 ) ) ;
#7727 = FILL_AREA_STYLE_COLOUR ( '', #11134 ) ;
#7728 = COLOUR_RGB ( '', 0.31764706, 0.68627451, 0.89019608) ;
#7729 = FILL_AREA_STYLE_COLOUR ( '', #15721 ) ;
#7730 = SURFACE_STYLE_FILL_AREA ( #7403 ) ;
#7731 = ORIENTED_EDGE ( 'NONE', *, *, #37471, .F. ) ;
#7732 = VECTOR ( 'NONE', #45974, 1000.000000000000000 ) ;
#7733 = ORIENTED_EDGE ( 'NONE', *, *, #39187, .F. ) ;
#7734 = SURFACE_STYLE_USAGE ( .BOTH. , #42147 ) ;
#7735 = FACE_OUTER_BOUND ( 'NONE', #17708, .T. ) ;
#7736 = CIRCLE ( 'NONE', #47100, 0.2500000000000002220 ) ;
#7737 = AXIS2_PLACEMENT_3D ( 'NONE', #24473, #51576, #30801 ) ;
#7738 = CARTESIAN_POINT ( 'NONE',  ( -6.759171781091402487, -2.292771058063873379, 0.1074872947962660502 ) ) ;
#7739 = CARTESIAN_POINT ( 'NONE',  ( -126.8070736234661666, 10.01517768586948698, -1.839758294383808966E-15 ) ) ;
#7740 = EDGE_LOOP ( 'NONE', ( #48842, #5721, #50466, #69691 ) ) ;
#7741 = CARTESIAN_POINT ( 'NONE',  ( -136.4049999999999727, -2.607480562269069768, 8.024999999999991473 ) ) ;
#7742 = ORIENTED_EDGE ( 'NONE', *, *, #16175, .T. ) ;
#7743 = ORIENTED_EDGE ( 'NONE', *, *, #64819, .F. ) ;
#7744 = CARTESIAN_POINT ( 'NONE',  ( -171.4429263765337907, -1.166476076187852838E-15, -9.524999999999991473 ) ) ;
#7745 = CARTESIAN_POINT ( 'NONE',  ( 0.000000000000000000, 42.00000000000000000, 75.00000000000001421 ) ) ;
#7746 = EDGE_LOOP ( 'NONE', ( #15675, #60966, #50918, #12535 ) ) ;
#7747 = DIRECTION ( 'NONE',  ( -0.000000000000000000, -0.000000000000000000, 1.000000000000000000 ) ) ;
#7748 = CYLINDRICAL_SURFACE ( 'NONE', #41085, 8.025000000000000355 ) ;
#7749 = CARTESIAN_POINT ( 'NONE',  ( -1.166476076187854022E-15, 143.9449999999999932, 9.525000000000000355 ) ) ;
#7750 = ORIENTED_EDGE ( 'NONE', *, *, #25353, .T. ) ;
#7751 = CARTESIAN_POINT ( 'NONE',  ( -3.094860106618434248, 144.9050000000000011, 9.525000000000000355 ) ) ;
#7752 = CARTESIAN_POINT ( 'NONE',  ( -49.10499999999998266, -6.826472737025113702, 4.959722759717902107 ) ) ;
#7753 = STYLED_ITEM ( 'NONE', ( #61856 ), #43560 ) ;
#7754 = CARTESIAN_POINT ( 'NONE',  ( 41.03152803655225966, 107.9804733857993284, -3.206774974533878719 ) ) ;
#7755 = VERTEX_POINT ( 'NONE', #23866 ) ;
#7756 = CARTESIAN_POINT ( 'NONE',  ( 6.826472737025121695, 116.4929263765338021, -4.959722759717905660 ) ) ;
#7757 = DIRECTION ( 'NONE',  ( 0.000000000000000000, 0.000000000000000000, 1.000000000000000000 ) ) ;
#7758 = SURFACE_STYLE_FILL_AREA ( #55954 ) ;
#7759 = FILL_AREA_STYLE_COLOUR ( '', #6949 ) ;
#7760 = PLANE ( 'NONE',  #12918 ) ;
#7761 = ORIENTED_EDGE ( 'NONE', *, *, #55682, .T. ) ;
#7762 = LINE ( 'NONE', #12695, #29513 ) ;
#7763 = VERTEX_POINT ( 'NONE', #66078 ) ;
#7764 = CARTESIAN_POINT ( 'NONE',  ( 12.72792206135785698, 115.4999999999999574, 10.50000000000000000 ) ) ;
#7765 =( GEOMETRIC_REPRESENTATION_CONTEXT ( 3 ) GLOBAL_UNCERTAINTY_ASSIGNED_CONTEXT ( ( #50356 ) ) GLOBAL_UNIT_ASSIGNED_CONTEXT ( ( #50179, #40318, #18833 ) ) REPRESENTATION_CONTEXT ( 'NONE', 'WORKASPACE' ) );
#7766 = CARTESIAN_POINT ( 'NONE',  ( -190.0000000000000000, 5.499999999999984901, 0.000000000000000000 ) ) ;
#7767 = DIRECTION ( 'NONE',  ( 0.000000000000000000, 0.000000000000000000, 1.000000000000000000 ) ) ;
#7768 = CARTESIAN_POINT ( 'NONE',  ( -166.2549999999999955, -4.716976649647092401, 6.492361379858946790 ) ) ;
#7769 = ORIENTED_EDGE ( 'NONE', *, *, #16469, .T. ) ;
#7770 = AXIS2_PLACEMENT_3D ( 'NONE', #11801, #54700, #44212 ) ;
#7771 =( NAMED_UNIT ( * ) SI_UNIT ( $, .STERADIAN. ) SOLID_ANGLE_UNIT ( ) );
#7772 = COLOUR_RGB ( '', 0.66274510, 0.83137255, 0.94901961) ;
#7773 =( BOUNDED_CURVE ( )  B_SPLINE_CURVE ( 3, ( #50054, #11350, #54258, #27512 ),
 .UNSPECIFIED., .F., .F. ) 
 B_SPLINE_CURVE_WITH_KNOTS ( ( 4, 4 ),
 ( 3.141592653589794004, 4.280198172320947236 ),
 .UNSPECIFIED. ) 
 CURVE ( )  GEOMETRIC_REPRESENTATION_ITEM ( )  RATIONAL_B_SPLINE_CURVE ( ( 1.000000000000000000, 0.8948513492540270953, 0.8948513492540270953, 1.000000000000000000 ) ) 
 REPRESENTATION_ITEM ( '' )  );
#7774 = ADVANCED_FACE ( 'NONE', ( #49934 ), #18492, .T. ) ;
#7775 = DIRECTION ( 'NONE',  ( -0.000000000000000000, -0.000000000000000000, 1.000000000000000000 ) ) ;
#7776 = LINE ( 'NONE', #40172, #43850 ) ;
#7777 = SURFACE_SIDE_STYLE ('',( #45118 ) ) ;
#7778 = EDGE_LOOP ( 'NONE', ( #59862, #62005, #12499, #57393 ) ) ;
#7779 = ORIENTED_EDGE ( 'NONE', *, *, #54395, .T. ) ;
#7780 = CARTESIAN_POINT ( 'NONE',  ( 32.00000000000000711, 42.00000000000000000, -35.50000000000000000 ) ) ;
#7782 = EDGE_CURVE ( 'NONE', #38988, #1652, #54422, .T. ) ;
#7781 = DIRECTION ( 'NONE',  ( 0.000000000000000000, 0.000000000000000000, 1.000000000000000000 ) ) ;
#7783 = CARTESIAN_POINT ( 'NONE',  ( -74.15499999999998693, 7.632228543268600340, 2.479861379858949277 ) ) ;
#7784 = ORIENTED_EDGE ( 'NONE', *, *, #51887, .T. ) ;
#7785 = SURFACE_STYLE_FILL_AREA ( #28537 ) ;
#7786 = PRESENTATION_LAYER_ASSIGNMENT (  '', '', ( #15649 ) ) ;
#7787 = CARTESIAN_POINT ( 'NONE',  ( -63.80707362346617373, 10.01517768586948698, -1.839758294383808966E-15 ) ) ;
#7788 = LINE ( 'NONE', #29237, #62274 ) ;
#7789 = VECTOR ( 'NONE', #41582, 1000.000000000000000 ) ;
#7790 = CARTESIAN_POINT ( 'NONE',  ( -75.00000000000000000, 7.967232421023206612, -7.000000003139141391 ) ) ;
#7791 = EDGE_LOOP ( 'NONE', ( #34712, #52892, #44410, #41643 ) ) ;
#7792 = SURFACE_SIDE_STYLE ('',( #17690 ) ) ;
#7793 = AXIS2_PLACEMENT_3D ( 'NONE', #33579, #55735, #28267 ) ;
#7794 = DIRECTION ( 'NONE',  ( 0.000000000000000000, 0.000000000000000000, 1.000000000000000000 ) ) ;
#7795 = ADVANCED_FACE ( 'NONE', ( #60121 ), #19582, .T. ) ;
#7796 = CARTESIAN_POINT ( 'NONE',  ( -3.094860106618432471, 136.5949999999999989, -9.525000000000000355 ) ) ;
#7797 = CARTESIAN_POINT ( 'NONE',  ( -106.6449999999999960, 4.716976649647091513, -6.492361379858946790 ) ) ;
#7798 = DIRECTION ( 'NONE',  ( 0.000000000000000000, 0.000000000000000000, 1.000000000000000000 ) ) ;
#7799 =( LENGTH_UNIT ( ) NAMED_UNIT ( * ) SI_UNIT ( .MILLI., .METRE. ) );
#7800 = VECTOR ( 'NONE', #18508, 1000.000000000000000 ) ;
#7802 = SURFACE_STYLE_FILL_AREA ( #59179 ) ;
#7801 = FILL_AREA_STYLE_COLOUR ( '', #60456 ) ;
#7803 =( GEOMETRIC_REPRESENTATION_CONTEXT ( 3 ) GLOBAL_UNCERTAINTY_ASSIGNED_CONTEXT ( ( #4403 ) ) GLOBAL_UNIT_ASSIGNED_CONTEXT ( ( #53576, #63777, #15623 ) ) REPRESENTATION_CONTEXT ( 'NONE', 'WORKASPACE' ) );
#7804 = CARTESIAN_POINT ( 'NONE',  ( -147.2929263765338135, 3.094860106618428031, -9.524999999999993250 ) ) ;
#7805 = CARTESIAN_POINT ( 'NONE',  ( -162.4449999999999932, 0.000000000000000000, 8.024999999999991473 ) ) ;
#7806 = ADVANCED_FACE ( 'NONE', ( #1990 ), #61823, .F. ) ;
#7807 = FILL_AREA_STYLE ('',( #50389 ) ) ;
#7808 = AXIS2_PLACEMENT_3D ( 'NONE', #55923, #19317, #13704 ) ;
#7809 = CIRCLE ( 'NONE', #61717, 3.499999999999999556 ) ;
#7810 = CYLINDRICAL_SURFACE ( 'NONE', #54034, 9.524999999999991473 ) ;
#7811 = ORIENTED_EDGE ( 'NONE', *, *, #32189, .F. ) ;
#7812 = DIRECTION ( 'NONE',  ( 0.000000000000000000, 0.000000000000000000, 1.000000000000000000 ) ) ;
#7813 = VERTEX_POINT ( 'NONE', #33720 ) ;
#7814 = EDGE_CURVE ( 'NONE', #68588, #25847, #19628, .T. ) ;
#7815 = AXIS2_PLACEMENT_3D ( 'NONE', #27862, #69102, #16352 ) ;
#7816 = CARTESIAN_POINT ( 'NONE',  ( -74.50000000000001421, 1.735173206890468129E-14, 9.500000000000000000 ) ) ;
#7817 = PRESENTATION_LAYER_ASSIGNMENT (  '', '', ( #42671 ) ) ;
#7818 = MECHANICAL_DESIGN_GEOMETRIC_PRESENTATION_REPRESENTATION (  '', ( #61726 ), #69480 ) ;
#7819 = CARTESIAN_POINT ( 'NONE',  ( -9.827790563157511022E-16, 119.5570736234661524, 8.025000000000000355 ) ) ;
#7820 = DIRECTION ( 'NONE',  ( -0.000000000000000000, 0.000000000000000000, -1.000000000000000000 ) ) ;
#7821 = DIRECTION ( 'NONE',  ( -1.000000000000000000, 0.000000000000000000, 0.000000000000000000 ) ) ;
#7822 =( GEOMETRIC_REPRESENTATION_CONTEXT ( 3 ) GLOBAL_UNCERTAINTY_ASSIGNED_CONTEXT ( ( #18716 ) ) GLOBAL_UNIT_ASSIGNED_CONTEXT ( ( #55486, #23464, #39341 ) ) REPRESENTATION_CONTEXT ( 'NONE', 'WORKASPACE' ) );
#7823 = CARTESIAN_POINT ( 'NONE',  ( -4.716976649647098618, 143.2570736234661410, 6.492361379858953008 ) ) ;
#7824 = ORIENTED_EDGE ( 'NONE', *, *, #21352, .F. ) ;
#7825 = CARTESIAN_POINT ( 'NONE',  ( -164.0049999999999955, 6.826472737025115478, 4.959722759717899443 ) ) ;
#7826 = ORIENTED_EDGE ( 'NONE', *, *, #44143, .T. ) ;
#7827 = CARTESIAN_POINT ( 'NONE',  ( -20.17679519342876304, 115.4776649671489963, -10.00000000000000000 ) ) ;
#7828 = PRESENTATION_STYLE_ASSIGNMENT (( #33861 ) ) ;
#7829 = COLOUR_RGB ( '', 0.09019608, 0.27058824, 0.51372549) ;
#7830 = DIRECTION ( 'NONE',  ( 1.000000000000000000, 0.000000000000000000, 0.000000000000000000 ) ) ;
#7831 = SURFACE_STYLE_USAGE ( .BOTH. , #66945 ) ;
#7832 = CARTESIAN_POINT ( 'NONE',  ( -3.094860106618434248, 113.7950000000000017, 9.525000000000000355 ) ) ;
#7833 = MECHANICAL_DESIGN_GEOMETRIC_PRESENTATION_REPRESENTATION (  '', ( #29158 ), #2134 ) ;
#7834 = VERTEX_POINT ( 'NONE', #46408 ) ;
#7835 = CARTESIAN_POINT ( 'NONE',  ( 23.50000000000001776, 43.00000000000000000, -29.68999999999999417 ) ) ;
#7836 = CARTESIAN_POINT ( 'NONE',  ( 5.598654528085805993, 115.3549999999999898, 7.705886871421374629 ) ) ;
#7837 = CARTESIAN_POINT ( 'NONE',  ( -86.30499999999997840, 8.437984349512086979, -1.550032578732815448E-15 ) ) ;
#7838 = CARTESIAN_POINT ( 'NONE',  ( 0.000000000000000000, 125.5550000000000068, -9.525000000000000355 ) ) ;
#7839 = STYLED_ITEM ( 'NONE', ( #68207 ), #69257 ) ;
#7840 = FACE_OUTER_BOUND ( 'NONE', #35722, .T. ) ;
#7841 = CARTESIAN_POINT ( 'NONE',  ( 20.86663389611626229, 115.0293260623345475, 10.00000000000000000 ) ) ;
#7842 = CARTESIAN_POINT ( 'NONE',  ( -43.75000000000000000, 0.000000000000000000, -5.000000000000000000 ) ) ;
#7843 = EDGE_CURVE ( 'NONE', #18409, #40144, #64945, .T. ) ;
#7844 = CARTESIAN_POINT ( 'NONE',  ( -71.49999999999998579, 64.07124727947029896, -9.500000000000000000 ) ) ;
#7845 = ORIENTED_EDGE ( 'NONE', *, *, #42603, .T. ) ;
#7846 = CARTESIAN_POINT ( 'NONE',  ( -54.14499999999999602, -4.716976649647092401, 6.492361379858946790 ) ) ;
#7847 = EDGE_LOOP ( 'NONE', ( #69084, #66413, #13279 ) ) ;
#7848 = DIRECTION ( 'NONE',  ( -8.881784197001252323E-16, 0.000000000000000000, 1.000000000000000000 ) ) ;
#7849 = CARTESIAN_POINT ( 'NONE',  ( -4.000000000000000000, -3.499999999999999556, 0.000000000000000000 ) ) ;
#7850 = TOROIDAL_SURFACE ( 'NONE', #26903, 18.99999999999998934, 1.000000000000000000 ) ;
#7851 = DIRECTION ( 'NONE',  ( 0.000000000000000000, -1.000000000000000000, 0.000000000000000000 ) ) ;
#7852 = ORIENTED_EDGE ( 'NONE', *, *, #5956, .T. ) ;
#7853 = DIRECTION ( 'NONE',  ( 1.000000000000000000, 0.000000000000000000, 0.000000000000000000 ) ) ;
#7854 = CARTESIAN_POINT ( 'NONE',  ( -50.09499999999996334, -2.607480562269071545, -8.024999999999991473 ) ) ;
#7855 = FILL_AREA_STYLE ('',( #13134 ) ) ;
#7856 = EDGE_LOOP ( 'NONE', ( #6967, #21600, #52062, #20675 ) ) ;
#7858 = ADVANCED_FACE ( 'NONE', ( #41127 ), #62869, .F. ) ;
#7857 = CARTESIAN_POINT ( 'NONE',  ( -75.00000000000000000, 9.025366258634575090, 6.779481487458411060 ) ) ;
#7859 = CARTESIAN_POINT ( 'NONE',  ( -109.2549999999999955, -4.716976649647092401, 6.492361379858946790 ) ) ;
#7860 = VERTEX_POINT ( 'NONE', #8400 ) ;
#7861 =( LENGTH_UNIT ( ) NAMED_UNIT ( * ) SI_UNIT ( .MILLI., .METRE. ) );
#7862 = PRESENTATION_LAYER_ASSIGNMENT (  '', '', ( #24722 ) ) ;
#7863 = DIRECTION ( 'NONE',  ( 0.000000000000000000, 1.000000000000000000, 0.000000000000000000 ) ) ;
#7864 = CARTESIAN_POINT ( 'NONE',  ( 0.000000000000000000, 0.000000000000000000, 52.50000000000000000 ) ) ;
#7865 = AXIS2_PLACEMENT_3D ( 'NONE', #11597, #27054, #289 ) ;
#7866 = CARTESIAN_POINT ( 'NONE',  ( -137.6070736234661922, -8.102448949553172852, 5.886773742842742685 ) ) ;
#7867 = CIRCLE ( 'NONE', #52840, 26.99999999999999645 ) ;
#7868 = FILL_AREA_STYLE ('',( #18444 ) ) ;
#7869 = CARTESIAN_POINT ( 'NONE',  ( -8.102448949553179958, 142.8949999999999818, -5.886773742842749790 ) ) ;
#7870 = CARTESIAN_POINT ( 'NONE',  ( -80.15707362346617515, -9.058813317711329915, -2.943386871421370898 ) ) ;
#7871 = AXIS2_PLACEMENT_3D ( 'NONE', #23465, #49885, #40727 ) ;
#7872 = CARTESIAN_POINT ( 'NONE',  ( -94.94292637653380496, 0.000000000000000000, 9.524999999999991473 ) ) ;
#7873 = FILL_AREA_STYLE_COLOUR ( '', #50750 ) ;
#7874 = PRESENTATION_LAYER_ASSIGNMENT (  '', '', ( #38247 ) ) ;
#7875 = DIRECTION ( 'NONE',  ( -0.000000000000000000, -1.000000000000000000, -0.000000000000000000 ) ) ;
#7877 = DIRECTION ( 'NONE',  ( 0.000000000000000000, 0.000000000000000000, 1.000000000000000000 ) ) ;
#7876 = CARTESIAN_POINT ( 'NONE',  ( -21.02379604162864268, 1.797044900979284448E-15, 10.00000000000000000 ) ) ;
#7878 = ADVANCED_FACE ( 'NONE', ( #31202, #56567 ), #29835, .F. ) ;
#7879 = CARTESIAN_POINT ( 'NONE',  ( -117.8050000000000068, -8.437984349512085203, 5.166775262442717831E-16 ) ) ;
#7880 = DIRECTION ( 'NONE',  ( -0.000000000000000000, -0.000000000000000000, -1.000000000000000000 ) ) ;
#7881 = FACE_OUTER_BOUND ( 'NONE', #40422, .T. ) ;
#7882 = CARTESIAN_POINT ( 'NONE',  ( 8.102448949553183510, 114.9949999999999903, -5.886773742842746238 ) ) ;
#7883 = CARTESIAN_POINT ( 'NONE',  ( -135.1449999999999818, -4.716976649647092401, 6.492361379858946790 ) ) ;
#7884 = AXIS2_PLACEMENT_3D ( 'NONE', #10915, #31669, #53807 ) ;
#7885 = CONICAL_SURFACE ( 'NONE', #31475, 7.000000000000000888, 0.7853981633974500554 ) ;
#7886 = CARTESIAN_POINT ( 'NONE',  ( -118.9449999999999932, -9.827790563157499189E-16, -8.024999999999991473 ) ) ;
#7887 = CARTESIAN_POINT ( 'NONE',  ( 0.000000000000000000, 2.299999999999999822, -10.00000000000000000 ) ) ;
#7888 = ORIENTED_EDGE ( 'NONE', *, *, #31362, .F. ) ;
#7889 = CARTESIAN_POINT ( 'NONE',  ( -146.4570736234661865, -9.058813317711329915, 2.943386871421371787 ) ) ;
#7890 = MECHANICAL_DESIGN_GEOMETRIC_PRESENTATION_REPRESENTATION (  '', ( #30308 ), #34856 ) ;
#7891 = FILL_AREA_STYLE_COLOUR ( '', #54826 ) ;
#7892 = CARTESIAN_POINT ( 'NONE',  ( -75.48275862068965125, 36.00832590023089352, -6.499999999999999112 ) ) ;
#7893 = CARTESIAN_POINT ( 'NONE',  ( -176.5429263765338135, 9.058813317711329915, 2.943386871421369566 ) ) ;
#7894 =( NAMED_UNIT ( * ) SI_UNIT ( $, .STERADIAN. ) SOLID_ANGLE_UNIT ( ) );
#7895 = TOROIDAL_SURFACE ( 'NONE', #43894, 0.5000000000000000000, 0.2500000000000000000 ) ;
#7896 = CARTESIAN_POINT ( 'NONE',  ( 9.250000000000003553, 27.74999999999998934, -3.750000000000000000 ) ) ;
#7897 = CARTESIAN_POINT ( 'NONE',  ( 48.25000000000000000, 22.24999999999998579, -3.750000000000000000 ) ) ;
#7898 = CARTESIAN_POINT ( 'NONE',  ( 5.196152422706636465, -9.000000000000005329, 7.500000000000000000 ) ) ;
#7899 = DIRECTION ( 'NONE',  ( -0.000000000000000000, -1.000000000000000000, 0.000000000000000000 ) ) ;
#7900 = CARTESIAN_POINT ( 'NONE',  ( -2.755190520427473366, -7.000000000000002665, 0.4949495880430740402 ) ) ;
#7901 = CIRCLE ( 'NONE', #21402, 0.2500000000000002220 ) ;
#7902 = PRODUCT_DEFINITION_CONTEXT ( 'detailed design', #63519, 'design' ) ;
#7903 = CARTESIAN_POINT ( 'NONE',  ( -92.69292637653377653, 10.01517768586948698, -1.839758294383808571E-15 ) ) ;
#7904 = APPLICATION_PROTOCOL_DEFINITION ( 'draft international standard', 'automotive_design', 1998, #24878 ) ;
#7905 = DIRECTION ( 'NONE',  ( 0.000000000000000000, -1.000000000000000000, 0.000000000000000000 ) ) ;
#7906 =( GEOMETRIC_REPRESENTATION_CONTEXT ( 3 ) GLOBAL_UNCERTAINTY_ASSIGNED_CONTEXT ( ( #33253 ) ) GLOBAL_UNIT_ASSIGNED_CONTEXT ( ( #49269, #28822, #34457 ) ) REPRESENTATION_CONTEXT ( 'NONE', 'WORKASPACE' ) );
#7907 =( NAMED_UNIT ( * ) PLANE_ANGLE_UNIT ( ) SI_UNIT ( $, .RADIAN. ) );
#7908 =( NAMED_UNIT ( * ) SI_UNIT ( $, .STERADIAN. ) SOLID_ANGLE_UNIT ( ) );
#7909 = CARTESIAN_POINT ( 'NONE',  ( -40.95793942983048197, 108.0317815798968866, 3.561444987364583259 ) ) ;
#7910 = CARTESIAN_POINT ( 'NONE',  ( 60.00000000000000000, 1.797044900979284448E-15, 10.00000000000000000 ) ) ;
#7911 = VERTEX_POINT ( 'NONE', #62187 ) ;
#7912 =( NAMED_UNIT ( * ) SI_UNIT ( $, .STERADIAN. ) SOLID_ANGLE_UNIT ( ) );
#7913 =( NAMED_UNIT ( * ) PLANE_ANGLE_UNIT ( ) SI_UNIT ( $, .RADIAN. ) );
#7914 = TOROIDAL_SURFACE ( 'NONE', #11332, 8.499999999999998224, 0.5000000000000000000 ) ;
#7915 = DIRECTION ( 'NONE',  ( 0.000000000000000000, -0.000000000000000000, 1.000000000000000000 ) ) ;
#7916 =( GEOMETRIC_REPRESENTATION_CONTEXT ( 3 ) GLOBAL_UNCERTAINTY_ASSIGNED_CONTEXT ( ( #12345 ) ) GLOBAL_UNIT_ASSIGNED_CONTEXT ( ( #30522, #47836, #42206 ) ) REPRESENTATION_CONTEXT ( 'NONE', 'WORKASPACE' ) );
#7917 = ORIENTED_EDGE ( 'NONE', *, *, #46184, .F. ) ;
#7918 = CARTESIAN_POINT ( 'NONE',  ( -64.79292637653379927, -3.094860106618429807, 9.524999999999991473 ) ) ;
#7919 = PRESENTATION_LAYER_ASSIGNMENT (  '', '', ( #32609 ) ) ;
#7920 = CARTESIAN_POINT ( 'NONE',  ( 7.632228543268608334, 132.4570736234661581, -2.479861379858951942 ) ) ;
#7922 = AXIS2_PLACEMENT_3D ( 'NONE', #61108, #62138, #13252 ) ;
#7921 =( NAMED_UNIT ( * ) SI_UNIT ( $, .STERADIAN. ) SOLID_ANGLE_UNIT ( ) );
#7923 = CARTESIAN_POINT ( 'NONE',  ( -15.98999599679679839, 146.4999999999999716, -7.000000000000000000 ) ) ;
#7924 = AXIS2_PLACEMENT_3D ( 'NONE', #18037, #64836, #39522 ) ;
#7925 = CARTESIAN_POINT ( 'NONE',  ( 30.75000000000001066, 16.24999999999997513, 3.750000000000000000 ) ) ;
#7926 = VERTEX_POINT ( 'NONE', #35476 ) ;
#7927 = LINE ( 'NONE', #35372, #9637 ) ;
#7928 = DIRECTION ( 'NONE',  ( -0.000000000000000000, -0.000000000000000000, 1.000000000000000000 ) ) ;
#7929 = SURFACE_STYLE_FILL_AREA ( #34651 ) ;
#7930 = FILL_AREA_STYLE ('',( #18500 ) ) ;
#7931 = MECHANICAL_DESIGN_GEOMETRIC_PRESENTATION_REPRESENTATION (  '', ( #19164 ), #65224 ) ;
#7932 = EDGE_CURVE ( 'NONE', #50329, #69192, #30164, .T. ) ;
#7933 = DIRECTION ( 'NONE',  ( -1.000000000000000000, 0.000000000000000000, -0.000000000000000000 ) ) ;
#7934 = CARTESIAN_POINT ( 'NONE',  ( -79.64499999999999602, 4.716976649647091513, -6.492361379858946790 ) ) ;
#7935 = ORIENTED_EDGE ( 'NONE', *, *, #45166, .T. ) ;
#7936 = VECTOR ( 'NONE', #21055, 1000.000000000000000 ) ;
#7937 = EDGE_CURVE ( 'NONE', #37066, #33115, #20681, .T. ) ;
#7938 = PRESENTATION_LAYER_ASSIGNMENT (  '', '', ( #26989 ) ) ;
#7939 = LINE ( 'NONE', #49827, #61356 ) ;
#7940 = SURFACE_STYLE_USAGE ( .BOTH. , #56116 ) ;
#7941 = UNCERTAINTY_MEASURE_WITH_UNIT (LENGTH_MEASURE( 1.000000000000000082E-05 ), #36733, 'distance_accuracy_value', 'NONE');
#7942 = VERTEX_POINT ( 'NONE', #10813 ) ;
#7943 = CARTESIAN_POINT ( 'NONE',  ( -76.04292637653379927, -9.058813317711329915, -2.943386871421370898 ) ) ;
#7944 =( GEOMETRIC_REPRESENTATION_CONTEXT ( 3 ) GLOBAL_UNCERTAINTY_ASSIGNED_CONTEXT ( ( #24161 ) ) GLOBAL_UNIT_ASSIGNED_CONTEXT ( ( #18113, #45584, #9301 ) ) REPRESENTATION_CONTEXT ( 'NONE', 'WORKASPACE' ) );
#7945 = CARTESIAN_POINT ( 'NONE',  ( -6.062177826491072175, -3.499999999999998668, 0.000000000000000000 ) ) ;
#7946 = ADVANCED_FACE ( 'NONE', ( #54055 ), #36508, .T. ) ;
#7947 = VERTEX_POINT ( 'NONE', #32260 ) ;
#7948 = EDGE_CURVE ( 'NONE', #5853, #51660, #32969, .T. ) ;
#7949 = VERTEX_POINT ( 'NONE', #16476 ) ;
#7950 = DIRECTION ( 'NONE',  ( 0.000000000000000000, 0.000000000000000000, 1.000000000000000000 ) ) ;
#7951 =( NAMED_UNIT ( * ) PLANE_ANGLE_UNIT ( ) SI_UNIT ( $, .RADIAN. ) );
#7952 = DIRECTION ( 'NONE',  ( 0.000000000000000000, 0.000000000000000000, 1.000000000000000000 ) ) ;
#7953 = CARTESIAN_POINT ( 'NONE',  ( -177.6570736234662036, 9.058813317711329915, 2.943386871421369566 ) ) ;
#7954 = CONICAL_SURFACE ( 'NONE', #47322, 9.000000000000007105, 0.7853981633974500554 ) ;
#7955 = EDGE_CURVE ( 'NONE', #57229, #9516, #54471, .T. ) ;
#7956 = DIRECTION ( 'NONE',  ( 0.000000000000000000, 0.000000000000000000, -1.000000000000000000 ) ) ;
#7957 = CARTESIAN_POINT ( 'NONE',  ( -110.3070736234661808, -10.01517768586948698, 6.132527647946031529E-16 ) ) ;
#7958 = VECTOR ( 'NONE', #21156, 1000.000000000000000 ) ;
#7959 = CARTESIAN_POINT ( 'NONE',  ( 25.00000000000001421, 42.00000000000000000, -34.49999999999999289 ) ) ;
#7960 = ADVANCED_FACE ( 'NONE', ( #21349 ), #16121, .F. ) ;
#7961 = VECTOR ( 'NONE', #54841, 999.9999999999998863 ) ;
#7962 = CARTESIAN_POINT ( 'NONE',  ( -84.80707362346619504, 10.01517768586948698, -1.839758294383808966E-15 ) ) ;
#7963 = ORIENTED_EDGE ( 'NONE', *, *, #67861, .F. ) ;
#7964 = CARTESIAN_POINT ( 'NONE',  ( 15.00000000000000000, 8.000000000000000000, 4.000000000000000000 ) ) ;
#7966 = STYLED_ITEM ( 'NONE', ( #60398 ), #13842 ) ;
#7965 = CARTESIAN_POINT ( 'NONE',  ( 13.75000000000000533, 30.74999999999999289, -3.750000000000000000 ) ) ;
#7967 = CARTESIAN_POINT ( 'NONE',  ( -154.5550000000000068, 0.000000000000000000, 8.024999999999991473 ) ) ;
#7968 = CARTESIAN_POINT ( 'NONE',  ( 25.00000000000000355, 37.00000000000000000, -3.000000000000000000 ) ) ;
#7969 = CARTESIAN_POINT ( 'NONE',  ( -8.300844275602472067, 111.4071313305642263, -2.350466666536774607 ) ) ;
#7970 = COLOUR_RGB ( '', 0.09019608, 0.27058824, 0.51372549) ;
#7971 = CARTESIAN_POINT ( 'NONE',  ( -167.0949999999999704, -2.607480562269071545, -8.024999999999991473 ) ) ;
#7972 = CARTESIAN_POINT ( 'NONE',  ( -157.7949999999999875, 2.607480562269069324, -8.024999999999993250 ) ) ;
#7973 = AXIS2_PLACEMENT_3D ( 'NONE', #11810, #17130, #6513 ) ;
#7974 = ORIENTED_EDGE ( 'NONE', *, *, #37047, .T. ) ;
#7975 = STYLED_ITEM ( 'NONE', ( #57572 ), #53924 ) ;
#7976 = DIRECTION ( 'NONE',  ( -1.000000000000000000, 0.000000000000000000, 0.000000000000000000 ) ) ;
#7977 = LINE ( 'NONE', #30809, #12085 ) ;
#7978 =( LENGTH_UNIT ( ) NAMED_UNIT ( * ) SI_UNIT ( .MILLI., .METRE. ) );
#7979 = CARTESIAN_POINT ( 'NONE',  ( -77.45499999999998408, 7.632228543268599452, -2.479861379858951942 ) ) ;
#7980 = CARTESIAN_POINT ( 'NONE',  ( -38.31544721422453392, -11.26485886809405557, 3.523166290182464966 ) ) ;
#7981 = VECTOR ( 'NONE', #66752, 1000.000000000000000 ) ;
#7982 = CARTESIAN_POINT ( 'NONE',  ( -168.2929263765340124, 3.094860106615100914, -9.525000000002410872 ) ) ;
#7983 = CARTESIAN_POINT ( 'NONE',  ( -72.14499999999998181, -4.716976649647092401, 6.492361379858946790 ) ) ;
#7984 = CARTESIAN_POINT ( 'NONE',  ( -1.166476076187854022E-15, 142.0549999999999784, 9.525000000000000355 ) ) ;
#7985 = PLANE ( 'NONE',  #14057 ) ;
#7986 = VECTOR ( 'NONE', #19623, 1000.000000000000000 ) ;
#7987 = DIRECTION ( 'NONE',  ( 1.000000000000000000, -0.000000000000000000, -0.000000000000000000 ) ) ;
#7988 = UNCERTAINTY_MEASURE_WITH_UNIT (LENGTH_MEASURE( 1.000000000000000082E-05 ), #17776, 'distance_accuracy_value', 'NONE');
#7989 = FILL_AREA_STYLE_COLOUR ( '', #45096 ) ;
#7990 = CARTESIAN_POINT ( 'NONE',  ( 69.99999999999998579, 36.75000000000000000, -3.000000000000000000 ) ) ;
#7991 = PRESENTATION_LAYER_ASSIGNMENT (  '', '', ( #38380 ) ) ;
#7992 = CARTESIAN_POINT ( 'NONE',  ( 8.021777294149467608, 2.499999999999998224, -4.105874159530731760 ) ) ;
#7993 =( NAMED_UNIT ( * ) PLANE_ANGLE_UNIT ( ) SI_UNIT ( $, .RADIAN. ) );
#7994 = CARTESIAN_POINT ( 'NONE',  ( -74.99999999999998579, 50.00000000000000000, 12.00000000000000000 ) ) ;
#7995 = PRESENTATION_STYLE_ASSIGNMENT (( #12213 ) ) ;
#7996 = ORIENTED_EDGE ( 'NONE', *, *, #59623, .F. ) ;
#7997 = ORIENTED_EDGE ( 'NONE', *, *, #55595, .T. ) ;
#7998 = AXIS2_PLACEMENT_3D ( 'NONE', #47603, #3910, #9586 ) ;
#7999 = STYLED_ITEM ( 'NONE', ( #30445 ), #12707 ) ;
#8000 = CARTESIAN_POINT ( 'NONE',  ( 7.750000000000000000, 33.74999999999998579, -3.750000000000000000 ) ) ;
#8001 = PLANE ( 'NONE',  #57730 ) ;
#8002 = ORIENTED_EDGE ( 'NONE', *, *, #65124, .T. ) ;
#8003 = TOROIDAL_SURFACE ( 'NONE', #59723, 0.7500000000000000000, 0.2500000000000000000 ) ;
#8004 = ORIENTED_EDGE ( 'NONE', *, *, #58882, .F. ) ;
#8005 =( NAMED_UNIT ( * ) PLANE_ANGLE_UNIT ( ) SI_UNIT ( $, .RADIAN. ) );
#8006 = DIRECTION ( 'NONE',  ( 1.000000000000000000, 0.000000000000000000, 0.000000000000000000 ) ) ;
#8007 = EDGE_CURVE ( 'NONE', #12301, #37934, #49987, .T. ) ;
#8008 = ORIENTED_EDGE ( 'NONE', *, *, #62717, .T. ) ;
#8009 = CARTESIAN_POINT ( 'NONE',  ( -3.094860106618432471, 113.7049999999999699, -9.525000000000000355 ) ) ;
#8010 = DIRECTION ( 'NONE',  ( -1.000000000000000000, -0.000000000000000000, -0.000000000000000000 ) ) ;
#8011 = ORIENTED_EDGE ( 'NONE', *, *, #42771, .T. ) ;
#8012 = AXIS2_PLACEMENT_3D ( 'NONE', #65366, #6962, #33015 ) ;
#8013 = ADVANCED_FACE ( 'NONE', ( #21020 ), #43225, .T. ) ;
#8014 = DIRECTION ( 'NONE',  ( -1.000000000000000000, 0.000000000000000000, 0.000000000000000000 ) ) ;
#8015 = LINE ( 'NONE', #2693, #61978 ) ;
#8016 = CARTESIAN_POINT ( 'NONE',  ( -107.9949999999999761, -6.826472737025115478, 4.959722759717900331 ) ) ;
#8017 = ORIENTED_EDGE ( 'NONE', *, *, #43009, .T. ) ;
#8018 = ADVANCED_FACE ( 'NONE', ( #44601 ), #31909, .T. ) ;
#8019 = CARTESIAN_POINT ( 'NONE',  ( -0.9109038252169192607, 2.456844516558473135, 9.000000000000001776 ) ) ;
#8020 = CARTESIAN_POINT ( 'NONE',  ( 72.49999999999998579, 119.9999999999997868, 10.00000000000000000 ) ) ;
#8021 = CARTESIAN_POINT ( 'NONE',  ( -11.94445006289030786, -11.32557150108030619, 3.970945727933070657 ) ) ;
#8022 = CARTESIAN_POINT ( 'NONE',  ( -75.00000000000000000, -2.215169945516535778E-14, 6.999999999999999112 ) ) ;
#8023 = ORIENTED_EDGE ( 'NONE', *, *, #42401, .T. ) ;
#8024 = CARTESIAN_POINT ( 'NONE',  ( 6.826472737025119919, 145.8929263765338362, 4.959722759717908325 ) ) ;
#8025 =( NAMED_UNIT ( * ) SI_UNIT ( $, .STERADIAN. ) SOLID_ANGLE_UNIT ( ) );
#8026 = CIRCLE ( 'NONE', #27085, 0.5000000000000004441 ) ;
#8027 = FILL_AREA_STYLE_COLOUR ( '', #31749 ) ;
#8028 = SURFACE_STYLE_USAGE ( .BOTH. , #40762 ) ;
#8029 = EDGE_LOOP ( 'NONE', ( #4664, #41570, #25015, #39109 ) ) ;
#8030 = AXIS2_PLACEMENT_3D ( 'NONE', #19376, #24637, #2816 ) ;
#8031 = CARTESIAN_POINT ( 'NONE',  ( 1.000000000000000000, 0.9999999999999991118, 79.00402776293826435 ) ) ;
#8032 = EDGE_CURVE ( 'NONE', #69517, #65703, #47823, .T. ) ;
#8033 = ORIENTED_EDGE ( 'NONE', *, *, #61104, .F. ) ;
#8034 =( NAMED_UNIT ( * ) SI_UNIT ( $, .STERADIAN. ) SOLID_ANGLE_UNIT ( ) );
#8035 = CARTESIAN_POINT ( 'NONE',  ( -2.607480562269200330, 140.4070736234661751, 8.024999999999911537 ) ) ;
#8036 = CARTESIAN_POINT ( 'NONE',  ( -10.39230484541327293, 3.364658241569156409E-15, 1.392304845413260939 ) ) ;
#8037 = CARTESIAN_POINT ( 'NONE',  ( -137.1550000000000011, 7.632228543268600340, 2.479861379858949277 ) ) ;
#8038 = DIRECTION ( 'NONE',  ( 0.000000000000000000, 0.000000000000000000, 1.000000000000000000 ) ) ;
#8039 = CYLINDRICAL_SURFACE ( 'NONE', #33885, 5.000000000000004441 ) ;
#8040 = EDGE_LOOP ( 'NONE', ( #9526, #13445, #65812 ) ) ;
#8041 = CARTESIAN_POINT ( 'NONE',  ( -44.99999999999977973, 149.9999999999999716, 10.00000000000000000 ) ) ;
#8042 = CIRCLE ( 'NONE', #57505, 1.000000000000000888 ) ;
#8043 = CARTESIAN_POINT ( 'NONE',  ( 39.24999999999999289, 16.24999999999997513, 4.000000000000000000 ) ) ;
#8044 = ADVANCED_FACE ( 'NONE', ( #40274 ), #23728, .F. ) ;
#8045 = CARTESIAN_POINT ( 'NONE',  ( -157.9429263765338192, 0.000000000000000000, 9.524999999999991473 ) ) ;
#8046 = ORIENTED_EDGE ( 'NONE', *, *, #2090, .T. ) ;
#8047 = MECHANICAL_DESIGN_GEOMETRIC_PRESENTATION_REPRESENTATION (  '', ( #30464 ), #9174 ) ;
#8048 = ORIENTED_EDGE ( 'NONE', *, *, #7547, .T. ) ;
#8049 = CARTESIAN_POINT ( 'NONE',  ( -32.34737067114478037, -8.620612969373077306, -2.355895588769170157 ) ) ;
#8050 = SURFACE_STYLE_USAGE ( .BOTH. , #56583 ) ;
#8051 = ORIENTED_EDGE ( 'NONE', *, *, #54693, .T. ) ;
#8052 = DIRECTION ( 'NONE',  ( -0.000000000000000000, -1.000000000000000000, -0.000000000000000000 ) ) ;
#8053 = CARTESIAN_POINT ( 'NONE',  ( -13.23915246117191025, 52.65078610323165265, 2.000000000000000000 ) ) ;
#8054 = DIRECTION ( 'NONE',  ( 0.000000000000000000, 0.000000000000000000, -1.000000000000000000 ) ) ;
#8055 = CARTESIAN_POINT ( 'NONE',  ( -59.15707362346617515, -9.058813317711329915, -2.943386871421370898 ) ) ;
#8056 = CIRCLE ( 'NONE', #10332, 12.50000000000000178 ) ;
#8057 = LINE ( 'NONE', #7373, #48655 ) ;
#8058 = CARTESIAN_POINT ( 'NONE',  ( -178.1070736234661638, 8.102448949553172852, -5.886773742842744461 ) ) ;
#8059 = VERTEX_POINT ( 'NONE', #61681 ) ;
#8060 = CARTESIAN_POINT ( 'NONE',  ( -160.7070736234664423, -3.094860106623137153, -9.524999999996571987 ) ) ;
#8061 = DIRECTION ( 'NONE',  ( 0.000000000000000000, 0.000000000000000000, 1.000000000000000000 ) ) ;
#8062 = CARTESIAN_POINT ( 'NONE',  ( 24.00000000000000355, 36.75000000000000000, -4.000000000000000000 ) ) ;
#8063 = CARTESIAN_POINT ( 'NONE',  ( -104.9049999999999869, 2.607480562269068880, -8.024999999999993250 ) ) ;
#8064 = CARTESIAN_POINT ( 'NONE',  ( -28.91386553845895335, -7.667674748043721955, -0.3278848047015802680 ) ) ;
#8065 = AXIS2_PLACEMENT_3D ( 'NONE', #15741, #4814, #47077 ) ;
#8066 =( NAMED_UNIT ( * ) PLANE_ANGLE_UNIT ( ) SI_UNIT ( $, .RADIAN. ) );
#8067 = PRESENTATION_LAYER_ASSIGNMENT (  '', '', ( #1104 ) ) ;
#8068 = CARTESIAN_POINT ( 'NONE',  ( -104.3949999999999818, -6.826472737025113702, -4.959722759717900331 ) ) ;
#8069 = CARTESIAN_POINT ( 'NONE',  ( 5.598654528085805993, 118.3549999999999898, 7.705886871421374629 ) ) ;
#8070 = CARTESIAN_POINT ( 'NONE',  ( -82.04499999999998749, 7.632228543268600340, 2.479861379858949277 ) ) ;
#8071 = MECHANICAL_DESIGN_GEOMETRIC_PRESENTATION_REPRESENTATION (  '', ( #17036 ), #65306 ) ;
#8072 = CYLINDRICAL_SURFACE ( 'NONE', #16252, 16.00000000000000000 ) ;
#8073 = CARTESIAN_POINT ( 'NONE',  ( -2.607480562268949420, 142.2929263765338135, 8.025000000000090949 ) ) ;
#8074 = DIRECTION ( 'NONE',  ( 0.000000000000000000, 1.000000000000000000, 0.000000000000000000 ) ) ;
#8075 = TOROIDAL_SURFACE ( 'NONE', #40687, 8.499999999999994671, 0.5000000000000000000 ) ;
#8076 = UNCERTAINTY_MEASURE_WITH_UNIT (LENGTH_MEASURE( 1.000000000000000082E-05 ), #65736, 'distance_accuracy_value', 'NONE');
#8077 = EDGE_CURVE ( 'NONE', #31383, #12003, #53392, .T. ) ;
#8078 = MECHANICAL_DESIGN_GEOMETRIC_PRESENTATION_REPRESENTATION (  '', ( #13697 ), #21538 ) ;
#8079 = CARTESIAN_POINT ( 'NONE',  ( -75.50000000000000000, 64.49137674618943095, -41.30495168499704306 ) ) ;
#8080 = CARTESIAN_POINT ( 'NONE',  ( -14.98999599679679662, 117.9999999999999716, 10.00000000000000000 ) ) ;
#8081 = VERTEX_POINT ( 'NONE', #19127 ) ;
#8082 = CARTESIAN_POINT ( 'NONE',  ( -117.1429263765337936, 5.598654528085800663, -7.705886871421367523 ) ) ;
#8083 = CARTESIAN_POINT ( 'NONE',  ( -133.7949999999999875, 2.607480562269068880, -8.024999999999993250 ) ) ;
#8084 = DIRECTION ( 'NONE',  ( 0.000000000000000000, 0.000000000000000000, -1.000000000000000000 ) ) ;
#8085 = VECTOR ( 'NONE', #26950, 1000.000000000000000 ) ;
#8086 = CARTESIAN_POINT ( 'NONE',  ( 45.50000000000000000, 99.99999999999992895, 9.500000000000000000 ) ) ;
#8087 =( NAMED_UNIT ( * ) PLANE_ANGLE_UNIT ( ) SI_UNIT ( $, .RADIAN. ) );
#8088 = DIRECTION ( 'NONE',  ( 0.000000000000000000, 0.000000000000000000, 1.000000000000000000 ) ) ;
#8089 = ORIENTED_EDGE ( 'NONE', *, *, #9243, .T. ) ;
#8090 = ORIENTED_EDGE ( 'NONE', *, *, #52589, .T. ) ;
#8091 =( BOUNDED_CURVE ( )  B_SPLINE_CURVE ( 3, ( #23524, #55891, #24549, #45035 ),
 .UNSPECIFIED., .F., .F. ) 
 B_SPLINE_CURVE_WITH_KNOTS ( ( 4, 4 ),
 ( 5.683226373146454513, 6.380992534147263306 ),
 .UNSPECIFIED. ) 
 CURVE ( )  GEOMETRIC_REPRESENTATION_ITEM ( )  RATIONAL_B_SPLINE_CURVE ( ( 1.000000000000000000, 0.9598367440515259696, 0.9598367440515259696, 1.000000000000000000 ) ) 
 REPRESENTATION_ITEM ( '' )  );
#8092 = CARTESIAN_POINT ( 'NONE',  ( 0.000000000000000000, 36.75000000000000000, 4.000000000000000000 ) ) ;
#8093 = CARTESIAN_POINT ( 'NONE',  ( -62.09292637653379643, 3.094860106618433360, 9.524999999999991473 ) ) ;
#8094 = VECTOR ( 'NONE', #18441, 1000.000000000000000 ) ;
#8095 = DIRECTION ( 'NONE',  ( -0.000000000000000000, 0.000000000000000000, -1.000000000000000000 ) ) ;
#8096 = FACE_OUTER_BOUND ( 'NONE', #15808, .T. ) ;
#8097 = CIRCLE ( 'NONE', #4726, 8.000000000000000000 ) ;
#8098 = FACE_OUTER_BOUND ( 'NONE', #67364, .T. ) ;
#8099 = VERTEX_POINT ( 'NONE', #40630 ) ;
#8100 = CARTESIAN_POINT ( 'NONE',  ( -128.9050000000000011, 2.607480562269069324, -8.024999999999993250 ) ) ;
#8102 = EDGE_CURVE ( 'NONE', #18929, #13202, #36037, .T. ) ;
#8101 = ORIENTED_EDGE ( 'NONE', *, *, #67820, .F. ) ;
#8103 = CARTESIAN_POINT ( 'NONE',  ( -44.99999999999977973, 146.9999999999999716, 9.500000000000000000 ) ) ;
#8104 = CARTESIAN_POINT ( 'NONE',  ( -119.7570736234661695, -5.598654528085801552, 7.705886871421367523 ) ) ;
#8105 = EDGE_CURVE ( 'NONE', #31257, #4018, #14938, .T. ) ;
#8106 = EDGE_LOOP ( 'NONE', ( #60871, #8304, #65910, #12780 ) ) ;
#8107 = CARTESIAN_POINT ( 'NONE',  ( -172.9429263765337907, 0.000000000000000000, 9.524999999999991473 ) ) ;
#8108 = FILL_AREA_STYLE_COLOUR ( '', #34323 ) ;
#8109 = VERTEX_POINT ( 'NONE', #4316 ) ;
#8110 = AXIS2_PLACEMENT_3D ( 'NONE', #66746, #1949, #39690 ) ;
#8111 = CARTESIAN_POINT ( 'NONE',  ( 9.212945446956389617, 3.316355128537251229, 12.15026236960284400 ) ) ;
#8112 = DIRECTION ( 'NONE',  ( -0.000000000000000000, -1.000000000000000000, 0.000000000000000000 ) ) ;
#8113 = CARTESIAN_POINT ( 'NONE',  ( -8.102448949553181734, 139.8950000000000102, -5.886773742842749790 ) ) ;
#8114 = FACE_OUTER_BOUND ( 'NONE', #68280, .T. ) ;
#8115 = EDGE_LOOP ( 'NONE', ( #17394, #24792, #34954, #32266 ) ) ;
#8116 = COLOUR_RGB ( '', 0.09019608, 0.27058824, 0.51372549) ;
#8118 = EDGE_CURVE ( 'NONE', #50919, #12618, #39845, .T. ) ;
#8117 = CARTESIAN_POINT ( 'NONE',  ( 8.102448949553179958, 136.5049999999999670, 5.886773742842750679 ) ) ;
#8119 = VECTOR ( 'NONE', #39428, 1000.000000000000000 ) ;
#8120 = DIRECTION ( 'NONE',  ( 1.000000000000000000, 0.000000000000000000, 0.000000000000000000 ) ) ;
#8121 = SURFACE_SIDE_STYLE ('',( #7435 ) ) ;
#8122 = ORIENTED_EDGE ( 'NONE', *, *, #34896, .F. ) ;
#8123 = CARTESIAN_POINT ( 'NONE',  ( 2.607480562269076430, 113.7929263765338277, -8.025000000000000355 ) ) ;
#8124 = CARTESIAN_POINT ( 'NONE',  ( -34.99999999999992895, 112.9999999999999858, -9.500000000000000000 ) ) ;
#8125 = UNCERTAINTY_MEASURE_WITH_UNIT (LENGTH_MEASURE( 1.000000000000000082E-05 ), #40651, 'distance_accuracy_value', 'NONE');
#8126 = FILL_AREA_STYLE_COLOUR ( '', #33310 ) ;
#8127 = ADVANCED_FACE ( 'NONE', ( #30365 ), #46632, .F. ) ;
#8128 = FILL_AREA_STYLE ('',( #1404 ) ) ;
#8129 = EDGE_LOOP ( 'NONE', ( #48185, #53169, #30687, #54656 ) ) ;
#8130 = CIRCLE ( 'NONE', #13693, 0.5000000000000004441 ) ;
#8131 = DIRECTION ( 'NONE',  ( 0.000000000000000000, 0.000000000000000000, 1.000000000000000000 ) ) ;
#8132 = EDGE_CURVE ( 'NONE', #67977, #26061, #15301, .T. ) ;
#8133 = ORIENTED_EDGE ( 'NONE', *, *, #7549, .T. ) ;
#8134 = DIRECTION ( 'NONE',  ( 0.000000000000000000, 0.000000000000000000, 1.000000000000000000 ) ) ;
#8135 = LINE ( 'NONE', #51048, #52472 ) ;
#8136 = DIRECTION ( 'NONE',  ( -0.000000000000000000, -1.000000000000000000, -0.000000000000000000 ) ) ;
#8137 = CARTESIAN_POINT ( 'NONE',  ( -164.9049999999999443, 2.607480562269068880, -8.024999999999993250 ) ) ;
#8139 = VERTEX_POINT ( 'NONE', #26146 ) ;
#8138 = VECTOR ( 'NONE', #26605, 1000.000000000000000 ) ;
#8140 =( LENGTH_UNIT ( ) NAMED_UNIT ( * ) SI_UNIT ( .MILLI., .METRE. ) );
#8141 = UNCERTAINTY_MEASURE_WITH_UNIT (LENGTH_MEASURE( 1.000000000000000082E-05 ), #54065, 'distance_accuracy_value', 'NONE');
#8142 = VECTOR ( 'NONE', #16540, 1000.000000000000000 ) ;
#8143 = CARTESIAN_POINT ( 'NONE',  ( -60.00000000000000000, -2.024042244987997205E-14, -9.500000000000000000 ) ) ;
#8144 = EDGE_CURVE ( 'NONE', #2770, #3825, #11799, .T. ) ;
#8145 = SURFACE_SIDE_STYLE ('',( #34181 ) ) ;
#8146 = DIRECTION ( 'NONE',  ( 0.000000000000000000, 0.000000000000000000, -1.000000000000000000 ) ) ;
#8147 = LINE ( 'NONE', #34182, #29854 ) ;
#8148 = ORIENTED_EDGE ( 'NONE', *, *, #25372, .F. ) ;
#8149 = VERTEX_POINT ( 'NONE', #41328 ) ;
#8150 = CYLINDRICAL_SURFACE ( 'NONE', #49624, 9.524999999999991473 ) ;
#8151 = DIRECTION ( 'NONE',  ( 1.000000000000000000, 0.000000000000000000, -1.300977106640435384E-16 ) ) ;
#8152 = DIRECTION ( 'NONE',  ( 0.000000000000000000, 0.000000000000000000, 1.000000000000000000 ) ) ;
#8153 = AXIS2_PLACEMENT_3D ( 'NONE', #32801, #21552, #33487 ) ;
#8154 = CARTESIAN_POINT ( 'NONE',  ( -75.35499999999998977, -4.716976649647093289, -6.492361379858945902 ) ) ;
#8155 = ORIENTED_EDGE ( 'NONE', *, *, #15916, .T. ) ;
#8156 = SURFACE_STYLE_USAGE ( .BOTH. , #50037 ) ;
#8157 = CARTESIAN_POINT ( 'NONE',  ( -64.10707362346616378, 8.102448949553172852, -5.886773742842744461 ) ) ;
#8158 = CARTESIAN_POINT ( 'NONE',  ( -150.6570736234661751, 9.058813317711329915, 2.943386871421369566 ) ) ;
#8159 = VECTOR ( 'NONE', #15960, 1000.000000000000000 ) ;
#8160 = ORIENTED_EDGE ( 'NONE', *, *, #29739, .T. ) ;
#8161 = CARTESIAN_POINT ( 'NONE',  ( 10.00000000000002309, 43.00000000000000000, 90.00000000000000000 ) ) ;
#8162 = CIRCLE ( 'NONE', #22715, 5.000000000000004441 ) ;
#8163 = CARTESIAN_POINT ( 'NONE',  ( -13.25000000000000355, 28.24999999999998934, 4.000000000000000000 ) ) ;
#8164 = CARTESIAN_POINT ( 'NONE',  ( -8.102448949553181734, 137.4950000000000045, 5.886773742842747126 ) ) ;
#8165 = CARTESIAN_POINT ( 'NONE',  ( -103.4949999999999761, 6.826472737025113702, -4.959722759717902107 ) ) ;
#8166 = VECTOR ( 'NONE', #36516, 1000.000000000000000 ) ;
#8167 = FACE_OUTER_BOUND ( 'NONE', #36640, .T. ) ;
#8168 = UNCERTAINTY_MEASURE_WITH_UNIT (LENGTH_MEASURE( 1.000000000000000082E-05 ), #54097, 'distance_accuracy_value', 'NONE');
#8169 = ADVANCED_FACE ( 'NONE', ( #53260 ), #61086, .T. ) ;
#8171 = DIRECTION ( 'NONE',  ( -0.000000000000000000, -0.000000000000000000, 1.000000000000000000 ) ) ;
#8170 = CARTESIAN_POINT ( 'NONE',  ( -9.827790563157511022E-16, 148.4429263765338476, 8.025000000000000355 ) ) ;
#8172 = STYLED_ITEM ( 'NONE', ( #69299 ), #46275 ) ;
#8173 = CARTESIAN_POINT ( 'NONE',  ( -147.7429263765338021, -5.598654528085803328, -7.705886871421366635 ) ) ;
#8174 = CARTESIAN_POINT ( 'NONE',  ( -169.6449999999999818, 4.716976649647091513, -6.492361379858946790 ) ) ;
#8175 =( GEOMETRIC_REPRESENTATION_CONTEXT ( 3 ) GLOBAL_UNCERTAINTY_ASSIGNED_CONTEXT ( ( #53284 ) ) GLOBAL_UNIT_ASSIGNED_CONTEXT ( ( #23336, #44838, #2878 ) ) REPRESENTATION_CONTEXT ( 'NONE', 'WORKASPACE' ) );
#8176 = CLOSED_SHELL ( 'NONE', ( #59305, #46605, #11355, #35910, #16438, #1715, #62884, #23066, #42851, #41720, #23044, #35090, #2485, #37379, #19521, #33490, #55726, #27197, #59492, #13173, #61829, #40855, #64943, #17949, #22466 ) ) ;
#8177 = FACE_OUTER_BOUND ( 'NONE', #10625, .T. ) ;
#8178 = VECTOR ( 'NONE', #20837, 999.9999999999998863 ) ;
#8179 = FILL_AREA_STYLE_COLOUR ( '', #37280 ) ;
#8180 = ORIENTED_EDGE ( 'NONE', *, *, #50153, .F. ) ;
#8181 = CARTESIAN_POINT ( 'NONE',  ( 0.000000000000000000, -2.500000000000000000, 0.000000000000000000 ) ) ;
#8182 = ORIENTED_EDGE ( 'NONE', *, *, #41816, .T. ) ;
#8183 = STYLED_ITEM ( 'NONE', ( #16633 ), #35959 ) ;
#8184 = CIRCLE ( 'NONE', #65466, 0.2500000000000002220 ) ;
#8185 = EDGE_CURVE ( 'NONE', #2399, #60757, #8091, .T. ) ;
#8186 = SURFACE_STYLE_USAGE ( .BOTH. , #14483 ) ;
#8187 = DIRECTION ( 'NONE',  ( -0.000000000000000000, -0.6691306063588591257, -0.7431448254773933559 ) ) ;
#8188 = CARTESIAN_POINT ( 'NONE',  ( -4.716976649647097730, 142.3570736234661638, -6.492361379858953896 ) ) ;
#8189 = EDGE_LOOP ( 'NONE', ( #16874, #29935, #62768 ) ) ;
#8190 = CARTESIAN_POINT ( 'NONE',  ( -164.7549999999999955, 4.716976649647091513, -6.492361379858946790 ) ) ;
#8191 = EDGE_CURVE ( 'NONE', #36332, #49909, #23876, .T. ) ;
#8192 = ADVANCED_FACE ( 'NONE', ( #34435 ), #3898, .T. ) ;
#8193 = ORIENTED_EDGE ( 'NONE', *, *, #50823, .T. ) ;
#8194 = PRESENTATION_LAYER_ASSIGNMENT (  '', '', ( #12692 ) ) ;
#8195 = CARTESIAN_POINT ( 'NONE',  ( -20.04013953308945162, 115.4999999999999432, -10.00000000000000000 ) ) ;
#8196 =( LENGTH_UNIT ( ) NAMED_UNIT ( * ) SI_UNIT ( .MILLI., .METRE. ) );
#8197 = VERTEX_POINT ( 'NONE', #12621 ) ;
#8198 = FACE_OUTER_BOUND ( 'NONE', #63656, .T. ) ;
#8199 = DIRECTION ( 'NONE',  ( -0.07898106964430656740, -0.9968761159932768567, 0.000000000000000000 ) ) ;
#8200 = CARTESIAN_POINT ( 'NONE',  ( -4.716976649647098618, 158.2570736234661695, 6.492361379858953008 ) ) ;
#8201 =( BOUNDED_CURVE ( )  B_SPLINE_CURVE ( 2, ( #5121, #58252, #16425, #37188, #25883, #31500, #15383, #9747, #4070, #42135, #58953 ),
 .UNSPECIFIED., .F., .F. ) 
 B_SPLINE_CURVE_WITH_KNOTS ( ( 3, 2, 2, 2, 2, 3 ),
 ( 0.9565217391304348116, 0.9586956521739130599, 0.9608695652173913082, 0.9630434782608695565, 0.9652173913043478048, 0.9673913043478260532 ),
 .UNSPECIFIED. ) 
 CURVE ( )  GEOMETRIC_REPRESENTATION_ITEM ( )  RATIONAL_B_SPLINE_CURVE ( ( 1.000000000000000000, 0.9510565162951535312, 1.000000000000000000, 0.9510565162951535312, 1.000000000000000000, 0.9510565162951535312, 1.000000000000000000, 0.9510565162951535312, 1.000000000000000000, 0.9510565162951535312, 1.000000000000000000 ) ) 
 REPRESENTATION_ITEM ( '' )  );
#8202 = STYLED_ITEM ( 'NONE', ( #30976 ), #26115 ) ;
#8203 = ORIENTED_EDGE ( 'NONE', *, *, #38980, .T. ) ;
#8204 = CARTESIAN_POINT ( 'NONE',  ( -4.500000000000002665, 22.24999999999998579, -3.750000000000000000 ) ) ;
#8206 = EDGE_CURVE ( 'NONE', #24259, #8394, #51137, .T. ) ;
#8205 = CARTESIAN_POINT ( 'NONE',  ( -5.598654528085806881, 110.8549999999999756, -7.705886871421374629 ) ) ;
#8207 = CARTESIAN_POINT ( 'NONE',  ( -75.20499999999996987, -2.607480562269071545, -8.024999999999991473 ) ) ;
#8208 =( NAMED_UNIT ( * ) PLANE_ANGLE_UNIT ( ) SI_UNIT ( $, .RADIAN. ) );
#8209 = CARTESIAN_POINT ( 'NONE',  ( 3.094860106618435136, 134.4049999999999443, -9.525000000000000355 ) ) ;
#8210 = UNCERTAINTY_MEASURE_WITH_UNIT (LENGTH_MEASURE( 1.000000000000000082E-05 ), #25308, 'distance_accuracy_value', 'NONE');
#8211 = DIRECTION ( 'NONE',  ( -0.000000000000000000, 0.000000000000000000, 1.000000000000000000 ) ) ;
#8212 = EDGE_CURVE ( 'NONE', #582, #15864, #56758, .T. ) ;
#8213 = CARTESIAN_POINT ( 'NONE',  ( -4.500000000000002665, 24.99999999999998579, 4.000000000000000000 ) ) ;
#8214 = CARTESIAN_POINT ( 'NONE',  ( 0.000000000000000000, 115.4999999999999574, 10.50000000000000000 ) ) ;
#8215 = EDGE_LOOP ( 'NONE', ( #29141, #57818, #15672, #62002, #29969 ) ) ;
#8216 = AXIS2_PLACEMENT_3D ( 'NONE', #45028, #18253, #8405 ) ;
#8217 = PRESENTATION_LAYER_ASSIGNMENT (  '', '', ( #20555 ) ) ;
#8218 = CARTESIAN_POINT ( 'NONE',  ( -49.49499999999997613, 6.826472737025113702, -4.959722759717902107 ) ) ;
#8219 = ORIENTED_EDGE ( 'NONE', *, *, #49110, .F. ) ;
#8220 = DIRECTION ( 'NONE',  ( -0.000000000000000000, -1.000000000000000000, -0.000000000000000000 ) ) ;
#8221 = AXIS2_PLACEMENT_3D ( 'NONE', #60965, #11488, #58991 ) ;
#8222 = CARTESIAN_POINT ( 'NONE',  ( 8.082903768654761123, 1.417096231345241097, 9.294316082458970795E-16 ) ) ;
#8223 = CARTESIAN_POINT ( 'NONE',  ( -21.02379604162863558, 114.4999999999999574, -10.50000000000000000 ) ) ;
#8224 = DIRECTION ( 'NONE',  ( -0.000000000000000000, -1.000000000000000000, -0.000000000000000000 ) ) ;
#8225 = EDGE_LOOP ( 'NONE', ( #62327, #58215, #58624 ) ) ;
#8226 = DIRECTION ( 'NONE',  ( -0.000000000000000000, 1.000000000000000000, -0.000000000000000000 ) ) ;
#8227 = CARTESIAN_POINT ( 'NONE',  ( -52.79499999999997328, 2.607480562269069324, -8.024999999999993250 ) ) ;
#8228 =( NAMED_UNIT ( * ) PLANE_ANGLE_UNIT ( ) SI_UNIT ( $, .RADIAN. ) );
#8229 = VERTEX_POINT ( 'NONE', #29845 ) ;
#8230 = DIRECTION ( 'NONE',  ( -0.000000000000000000, -0.000000000000000000, -1.000000000000000000 ) ) ;
#8231 = CARTESIAN_POINT ( 'NONE',  ( -104.0049999999999812, 6.826472737025116366, 4.959722759717898555 ) ) ;
#8232 = ORIENTED_EDGE ( 'NONE', *, *, #27291, .T. ) ;
#8233 = ADVANCED_FACE ( 'NONE', ( #34769 ), #23203, .F. ) ;
#8235 = AXIS2_PLACEMENT_3D ( 'NONE', #23171, #16873, #38347 ) ;
#8234 = CARTESIAN_POINT ( 'NONE',  ( 30.75000000000001066, 15.74999999999997513, -4.000000000000000000 ) ) ;
#8236 = DIRECTION ( 'NONE',  ( -0.000000000000000000, -1.000000000000000000, -0.000000000000000000 ) ) ;
#8237 = CARTESIAN_POINT ( 'NONE',  ( -142.7070736234662149, -3.094860106618431139, -9.524999999999991473 ) ) ;
#8238 = MECHANICAL_DESIGN_GEOMETRIC_PRESENTATION_REPRESENTATION (  '', ( #13849 ), #19463 ) ;
#8239 = EDGE_CURVE ( 'NONE', #30440, #35956, #69111, .T. ) ;
#8240 = DIRECTION ( 'NONE',  ( -0.000000000000000000, -1.000000000000000000, 0.000000000000000000 ) ) ;
#8241 = CARTESIAN_POINT ( 'NONE',  ( -8.102448949553179958, 145.8949999999999818, -5.886773742842749790 ) ) ;
#8242 = CARTESIAN_POINT ( 'NONE',  ( -87.95707362346617231, 9.058813317711329915, -2.943386871421373119 ) ) ;
#8243 = VECTOR ( 'NONE', #933, 1000.000000000000000 ) ;
#8244 =( LENGTH_UNIT ( ) NAMED_UNIT ( * ) SI_UNIT ( .MILLI., .METRE. ) );
#8245 = COLOUR_RGB ( '', 0.66274510, 0.83137255, 0.94901961) ;
#8246 = DIRECTION ( 'NONE',  ( 0.000000000000000000, 0.000000000000000000, 1.000000000000000000 ) ) ;
#8247 = SURFACE_SIDE_STYLE ('',( #2182 ) ) ;
#8248 = CARTESIAN_POINT ( 'NONE',  ( 6.826472737025121695, 120.6070736234661354, -4.959722759717905660 ) ) ;
#8249 = PRESENTATION_LAYER_ASSIGNMENT (  '', '', ( #34086 ) ) ;
#8250 = CARTESIAN_POINT ( 'NONE',  ( -124.1049999999999756, -6.826472737025115478, 4.959722759717900331 ) ) ;
#8251 = CARTESIAN_POINT ( 'NONE',  ( -158.8429263765337964, 9.058813317711329915, -2.943386871421373119 ) ) ;
#8252 = CARTESIAN_POINT ( 'NONE',  ( 5.598654528085809545, 112.1449999999999818, -7.705886871421373741 ) ) ;
#8253 = CARTESIAN_POINT ( 'NONE',  ( -130.9449999999999648, -9.827790563157499189E-16, -8.024999999999991473 ) ) ;
#8254 = CARTESIAN_POINT ( 'NONE',  ( -115.3449999999999847, 7.632228543268599452, -2.479861379858951942 ) ) ;
#8255 = CARTESIAN_POINT ( 'NONE',  ( 62.10000000000000142, 11.99999999999999822, 3.499999999999992895 ) ) ;
#8256 = EDGE_LOOP ( 'NONE', ( #36198, #24335, #18800, #18838 ) ) ;
#8257 = DIRECTION ( 'NONE',  ( -0.000000000000000000, -1.000000000000000000, -0.000000000000000000 ) ) ;
#8258 = VECTOR ( 'NONE', #59330, 1000.000000000000000 ) ;
#8259 = CARTESIAN_POINT ( 'NONE',  ( 28.00000000000000000, 38.70020753820971748, -89.00000000000000000 ) ) ;
#8260 = CARTESIAN_POINT ( 'NONE',  ( -167.9929263765338021, 8.102448949553171076, -5.886773742842744461 ) ) ;
#8261 = CARTESIAN_POINT ( 'NONE',  ( -50.24499999999998323, -4.716976649647093289, -6.492361379858945902 ) ) ;
#8262 = CARTESIAN_POINT ( 'NONE',  ( 0.000000000000000000, 115.4999999999999574, 10.50000000000000000 ) ) ;
#8263 = ADVANCED_FACE ( 'NONE', ( #46787 ), #47834, .F. ) ;
#8264 =( GEOMETRIC_REPRESENTATION_CONTEXT ( 3 ) GLOBAL_UNCERTAINTY_ASSIGNED_CONTEXT ( ( #52981 ) ) GLOBAL_UNIT_ASSIGNED_CONTEXT ( ( #22403, #1230, #5499 ) ) REPRESENTATION_CONTEXT ( 'NONE', 'WORKASPACE' ) );
#8266 = AXIS2_PLACEMENT_3D ( 'NONE', #33878, #45181, #44834 ) ;
#8265 = CIRCLE ( 'NONE', #18403, 6.999999999999997335 ) ;
#8267 = LINE ( 'NONE', #8611, #67190 ) ;
#8268 = CARTESIAN_POINT ( 'NONE',  ( -1.403516486455608892, -7.000000000000002665, 0.1310752030855618366 ) ) ;
#8269 = ORIENTED_EDGE ( 'NONE', *, *, #27286, .T. ) ;
#8270 = CARTESIAN_POINT ( 'NONE',  ( -86.54292637653379927, 9.058813317711329915, 2.943386871421369566 ) ) ;
#8271 = SURFACE_SIDE_STYLE ('',( #14963 ) ) ;
#8272 = PLANE ( 'NONE',  #21493 ) ;
#8273 = AXIS2_PLACEMENT_3D ( 'NONE', #24042, #7851, #14193 ) ;
#8274 = AXIS2_PLACEMENT_3D ( 'NONE', #29651, #50083, #34921 ) ;
#8275 = EDGE_CURVE ( 'NONE', #16942, #53214, #35417, .T. ) ;
#8276 = DIRECTION ( 'NONE',  ( -1.000000000000000000, -0.000000000000000000, -0.000000000000000000 ) ) ;
#8277 = FILL_AREA_STYLE ('',( #36434 ) ) ;
#8278 = CARTESIAN_POINT ( 'NONE',  ( -163.4929263765338021, -8.102448949553174629, 5.886773742842742685 ) ) ;
#8279 =( NAMED_UNIT ( * ) SI_UNIT ( $, .STERADIAN. ) SOLID_ANGLE_UNIT ( ) );
#8280 = EDGE_CURVE ( 'NONE', #56786, #50847, #15324, .T. ) ;
#8281 = EDGE_LOOP ( 'NONE', ( #2437, #63920, #67103, #56614 ) ) ;
#8282 = CARTESIAN_POINT ( 'NONE',  ( 36.00000000000002842, 0.000000000000000000, 29.00402776293825724 ) ) ;
#8283 = CARTESIAN_POINT ( 'NONE',  ( 69.99999999999998579, 1.000000000000008660, -3.000000000000000000 ) ) ;
#8284 = ORIENTED_EDGE ( 'NONE', *, *, #7843, .T. ) ;
#8285 = CARTESIAN_POINT ( 'NONE',  ( -2.607480562269115509, 133.2070736234661581, -8.024999999999970157 ) ) ;
#8286 = VECTOR ( 'NONE', #61153, 1000.000000000000000 ) ;
#8287 = CARTESIAN_POINT ( 'NONE',  ( 6.826472737025121695, 135.6070736234661638, -4.959722759717905660 ) ) ;
#8288 =( GEOMETRIC_REPRESENTATION_CONTEXT ( 3 ) GLOBAL_UNCERTAINTY_ASSIGNED_CONTEXT ( ( #6672 ) ) GLOBAL_UNIT_ASSIGNED_CONTEXT ( ( #60024, #12166, #6907 ) ) REPRESENTATION_CONTEXT ( 'NONE', 'WORKASPACE' ) );
#8289 = CARTESIAN_POINT ( 'NONE',  ( 0.000000000000000000, 24.74999999999998579, 4.000000000000000000 ) ) ;
#8291 = LINE ( 'NONE', #18141, #61984 ) ;
#8290 = AXIS2_PLACEMENT_3D ( 'NONE', #54785, #17216, #236 ) ;
#8292 = DIRECTION ( 'NONE',  ( 1.000000000000000000, 0.000000000000000000, 0.000000000000000000 ) ) ;
#8293 = ORIENTED_EDGE ( 'NONE', *, *, #9003, .T. ) ;
#8294 = MECHANICAL_DESIGN_GEOMETRIC_PRESENTATION_REPRESENTATION (  '', ( #42034 ), #2604 ) ;
#8295 = CARTESIAN_POINT ( 'NONE',  ( -15.98999599679679839, 146.4999999999999716, 7.500000000000000000 ) ) ;
#8296 = EDGE_CURVE ( 'NONE', #38837, #60182, #537, .T. ) ;
#8297 = CIRCLE ( 'NONE', #45386, 0.2500000000000002220 ) ;
#8298 = CARTESIAN_POINT ( 'NONE',  ( 43.75000000000000000, 19.24999999999998224, 4.000000000000000000 ) ) ;
#8299 = CARTESIAN_POINT ( 'NONE',  ( 0.000000000000000000, 21.74999999999998579, 3.750000000000000000 ) ) ;
#8300 = DIRECTION ( 'NONE',  ( 1.000000000000000000, 0.000000000000000000, 0.000000000000000000 ) ) ;
#8301 = STYLED_ITEM ( 'NONE', ( #25657 ), #2910 ) ;
#8302 = PRESENTATION_STYLE_ASSIGNMENT (( #46305 ) ) ;
#8303 = CARTESIAN_POINT ( 'NONE',  ( -77.84499999999998465, -7.632228543268599452, 2.479861379858951054 ) ) ;
#8304 = ORIENTED_EDGE ( 'NONE', *, *, #46454, .F. ) ;
#8305 = DIRECTION ( 'NONE',  ( 0.000000000000000000, 0.000000000000000000, -1.000000000000000000 ) ) ;
#8306 = MECHANICAL_DESIGN_GEOMETRIC_PRESENTATION_REPRESENTATION (  '', ( #25114 ), #50978 ) ;
#8307 = CYLINDRICAL_SURFACE ( 'NONE', #23266, 0.9999999999999997780 ) ;
#8308 = PRESENTATION_STYLE_ASSIGNMENT (( #57521 ) ) ;
#8309 = EDGE_LOOP ( 'NONE', ( #9633, #22822, #60974, #46385 ) ) ;
#8310 = CARTESIAN_POINT ( 'NONE',  ( 23.21231517720797655, 117.9999999999999716, 9.500000000000000000 ) ) ;
#8311 = SURFACE_STYLE_FILL_AREA ( #59304 ) ;
#8312 = CARTESIAN_POINT ( 'NONE',  ( -6.759171781091402487, -2.292771058063873379, 0.1074872947962660502 ) ) ;
#8313 = ORIENTED_EDGE ( 'NONE', *, *, #65772, .T. ) ;
#8314 = FACE_OUTER_BOUND ( 'NONE', #52578, .T. ) ;
#8315 = ORIENTED_EDGE ( 'NONE', *, *, #58464, .F. ) ;
#8316 = CYLINDRICAL_SURFACE ( 'NONE', #48784, 9.524999999999991473 ) ;
#8317 = CARTESIAN_POINT ( 'NONE',  ( 2.418047948263830627, -2.101261491288919814, 7.000000000000000000 ) ) ;
#8318 = PRESENTATION_LAYER_ASSIGNMENT (  '', '', ( #361 ) ) ;
#8319 = AXIS2_PLACEMENT_3D ( 'NONE', #33282, #32939, #505 ) ;
#8320 = CARTESIAN_POINT ( 'NONE',  ( -170.9070736234662036, -3.094860106618429807, 9.524999999999991473 ) ) ;
#8321 = PLANE ( 'NONE',  #34219 ) ;
#8322 = CARTESIAN_POINT ( 'NONE',  ( 5.598654528085809545, 115.1449999999999818, -7.705886871421373741 ) ) ;
#8323 = CARTESIAN_POINT ( 'NONE',  ( -113.1570736234661751, -9.058813317711329915, -2.943386871421370898 ) ) ;
#8324 = COLOUR_RGB ( '', 0.40784314, 0.44705882, 0.49803922) ;
#8325 = CARTESIAN_POINT ( 'NONE',  ( -3.414270897520785386, 1.730686724748536021, 7.000000000000000000 ) ) ;
#8326 = DIRECTION ( 'NONE',  ( 0.000000000000000000, 0.000000000000000000, 1.000000000000000000 ) ) ;
#8327 = ORIENTED_EDGE ( 'NONE', *, *, #23731, .T. ) ;
#8328 = LINE ( 'NONE', #23791, #65433 ) ;
#8329 = CARTESIAN_POINT ( 'NONE',  ( 60.00000000000000000, 1.797044900979284448E-15, 10.00000000000000000 ) ) ;
#8330 = CARTESIAN_POINT ( 'NONE',  ( 68.00000000000000000, 2.776762340297169183E-15, -10.49999999999999822 ) ) ;
#8331 = CARTESIAN_POINT ( 'NONE',  ( -154.8549999999999898, 4.716976649647094177, 6.492361379858945902 ) ) ;
#8332 = SURFACE_SIDE_STYLE ('',( #18848 ) ) ;
#8333 = CARTESIAN_POINT ( 'NONE',  ( -164.8449999999999989, -7.632228543268599452, 2.479861379858951054 ) ) ;
#8334 = TOROIDAL_SURFACE ( 'NONE', #58891, 14.49999999999999822, 0.5000000000000000000 ) ;
#8335 = CARTESIAN_POINT ( 'NONE',  ( -150.4449999999999932, 0.000000000000000000, 8.024999999999991473 ) ) ;
#8336 = ORIENTED_EDGE ( 'NONE', *, *, #26539, .T. ) ;
#8337 = AXIS2_PLACEMENT_3D ( 'NONE', #36087, #4745, #26200 ) ;
#8338 =( NAMED_UNIT ( * ) PLANE_ANGLE_UNIT ( ) SI_UNIT ( $, .RADIAN. ) );
#8339 = FILL_AREA_STYLE ('',( #62124 ) ) ;
#8340 = CARTESIAN_POINT ( 'NONE',  ( -122.5429263765337993, 9.058813317711329915, 2.943386871421369566 ) ) ;
#8341 = AXIS2_PLACEMENT_3D ( 'NONE', #8519, #55022, #66913 ) ;
#8342 = CARTESIAN_POINT ( 'NONE',  ( -67.10499999999997556, -6.826472737025115478, 4.959722759717900331 ) ) ;
#8343 = LINE ( 'NONE', #35760, #2200 ) ;
#8344 = LINE ( 'NONE', #44961, #34732 ) ;
#8345 = COLOUR_RGB ( '', 0.09019608, 0.27058824, 0.51372549) ;
#8346 = CARTESIAN_POINT ( 'NONE',  ( -58.79499999999998749, 2.607480562269069324, -8.024999999999993250 ) ) ;
#8347 = CARTESIAN_POINT ( 'NONE',  ( -5.598654528085808657, 147.7549999999999955, 7.705886871421373741 ) ) ;
#8348 = DIRECTION ( 'NONE',  ( 0.000000000000000000, 0.000000000000000000, 1.000000000000000000 ) ) ;
#8349 = EDGE_CURVE ( 'NONE', #31691, #5568, #42260, .T. ) ;
#8350 = AXIS2_PLACEMENT_3D ( 'NONE', #3933, #36361, #4262 ) ;
#8351 = DIRECTION ( 'NONE',  ( -1.000000000000000000, -0.000000000000000000, -0.000000000000000000 ) ) ;
#8352 = CIRCLE ( 'NONE', #37573, 1.000000000000000888 ) ;
#8353 = CARTESIAN_POINT ( 'NONE',  ( -159.2070736234664423, 3.094860106623441798, 9.524999999996355271 ) ) ;
#8354 = DIRECTION ( 'NONE',  ( 1.000000000000000000, 0.000000000000000000, 0.000000000000000000 ) ) ;
#8355 = AXIS2_PLACEMENT_3D ( 'NONE', #13204, #41371, #13917 ) ;
#8356 = CARTESIAN_POINT ( 'NONE',  ( -183.4449999999999932, 0.000000000000000000, 8.024999999999991473 ) ) ;
#8357 = SURFACE_STYLE_FILL_AREA ( #1624 ) ;
#8358 = CIRCLE ( 'NONE', #65634, 0.2500000000000002220 ) ;
#8359 = SURFACE_STYLE_FILL_AREA ( #67423 ) ;
#8360 = ADVANCED_FACE ( 'NONE', ( #8747 ), #27543, .T. ) ;
#8361 = EDGE_CURVE ( 'NONE', #62857, #4894, #34302, .T. ) ;
#8362 = FACE_OUTER_BOUND ( 'NONE', #42527, .T. ) ;
#8363 = DIRECTION ( 'NONE',  ( 0.000000000000000000, 1.000000000000000000, 0.000000000000000000 ) ) ;
#8364 = EDGE_LOOP ( 'NONE', ( #35451, #25054, #29546, #42946 ) ) ;
#8366 = ORIENTED_EDGE ( 'NONE', *, *, #43143, .T. ) ;
#8365 = AXIS2_PLACEMENT_3D ( 'NONE', #34642, #18489, #7574 ) ;
#8367 = VECTOR ( 'NONE', #45257, 1000.000000000000000 ) ;
#8368 = SURFACE_STYLE_USAGE ( .BOTH. , #67792 ) ;
#8369 = EDGE_CURVE ( 'NONE', #57600, #60182, #62417, .T. ) ;
#8370 = CARTESIAN_POINT ( 'NONE',  ( 4.750000000000002665, 24.99999999999998579, -3.750000000000000000 ) ) ;
#8371 = EDGE_CURVE ( 'NONE', #23306, #54975, #24189, .T. ) ;
#8372 = EDGE_LOOP ( 'NONE', ( #38710, #60409, #9449, #65594 ) ) ;
#8373 = EDGE_LOOP ( 'NONE', ( #67523, #10531, #1458, #56323 ) ) ;
#8374 = DIRECTION ( 'NONE',  ( -0.000000000000000000, -1.000000000000000000, -0.000000000000000000 ) ) ;
#8375 = ADVANCED_FACE ( 'NONE', ( #59011 ), #26959, .F. ) ;
#8376 = DIRECTION ( 'NONE',  ( 0.000000000000000000, 0.000000000000000000, -1.000000000000000000 ) ) ;
#8377 = ORIENTED_EDGE ( 'NONE', *, *, #67053, .F. ) ;
#8378 = CARTESIAN_POINT ( 'NONE',  ( -9.058813317711337021, 114.1549999999999869, -2.943386871421374895 ) ) ;
#8379 = CARTESIAN_POINT ( 'NONE',  ( -3.414918479307655907, 7.000000000000006217, 0.7696370661449007944 ) ) ;
#8380 = VERTEX_POINT ( 'NONE', #37609 ) ;
#8381 = FILL_AREA_STYLE_COLOUR ( '', #15985 ) ;
#8382 = CARTESIAN_POINT ( 'NONE',  ( -106.7949999999999733, 2.607480562269068880, -8.024999999999993250 ) ) ;
#8383 = ORIENTED_EDGE ( 'NONE', *, *, #27452, .T. ) ;
#8384 = CARTESIAN_POINT ( 'NONE',  ( -9.190687389602119950, 110.4999999999999858, 2.539151240794934150 ) ) ;
#8385 =( NAMED_UNIT ( * ) PLANE_ANGLE_UNIT ( ) SI_UNIT ( $, .RADIAN. ) );
#8386 = CARTESIAN_POINT ( 'NONE',  ( 24.58159228739605950, 26.69105118024819490, -27.43537399302963919 ) ) ;
#8387 = FILL_AREA_STYLE_COLOUR ( '', #7022 ) ;
#8388 = VECTOR ( 'NONE', #46808, 1000.000000000000000 ) ;
#8389 = ORIENTED_EDGE ( 'NONE', *, *, #19312, .F. ) ;
#8390 = CARTESIAN_POINT ( 'NONE',  ( -2.607480562269075097, 148.2929263765338419, 8.025000000000000355 ) ) ;
#8391 = CARTESIAN_POINT ( 'NONE',  ( -106.5570736234661666, -1.166476076187852838E-15, -9.524999999999991473 ) ) ;
#8392 = CARTESIAN_POINT ( 'NONE',  ( 48.00000000000000000, 14.49137674618942562, 7.000000000000000000 ) ) ;
#8393 = CARTESIAN_POINT ( 'NONE',  ( 0.000000000000000000, -2.500000000000000000, -5.500000000000005329 ) ) ;
#8394 = VERTEX_POINT ( 'NONE', #54413 ) ;
#8395 = VERTEX_POINT ( 'NONE', #59326 ) ;
#8396 = SURFACE_SIDE_STYLE ('',( #35113 ) ) ;
#8397 = DIRECTION ( 'NONE',  ( -8.673617379884040402E-17, 0.000000000000000000, -1.000000000000000000 ) ) ;
#8398 = FACE_OUTER_BOUND ( 'NONE', #65119, .T. ) ;
#8399 = CARTESIAN_POINT ( 'NONE',  ( -134.3050000000000352, 8.437984349512085203, -1.550032578732815448E-15 ) ) ;
#8400 = CARTESIAN_POINT ( 'NONE',  ( 23.71231517720798010, 117.4999999999999716, 7.500000000000000000 ) ) ;
#8401 = DIRECTION ( 'NONE',  ( 0.000000000000000000, 0.000000000000000000, 1.000000000000000000 ) ) ;
#8402 = EDGE_LOOP ( 'NONE', ( #17058, #65125, #67459, #40947 ) ) ;
#8403 = CIRCLE ( 'NONE', #44347, 0.2500000000000002220 ) ;
#8404 = STYLED_ITEM ( 'NONE', ( #40086 ), #7806 ) ;
#8405 = DIRECTION ( 'NONE',  ( 0.000000000000000000, -0.000000000000000000, -1.000000000000000000 ) ) ;
#8406 = SURFACE_STYLE_USAGE ( .BOTH. , #56575 ) ;
#8407 =( LENGTH_UNIT ( ) NAMED_UNIT ( * ) SI_UNIT ( .MILLI., .METRE. ) );
#8408 = VERTEX_POINT ( 'NONE', #5509 ) ;
#8409 = ORIENTED_EDGE ( 'NONE', *, *, #60364, .F. ) ;
#8410 = CARTESIAN_POINT ( 'NONE',  ( -19.89974874213240597, 115.4999999999999574, 10.00000000000000000 ) ) ;
#8411 = CYLINDRICAL_SURFACE ( 'NONE', #35672, 0.2500000000000002220 ) ;
#8413 = PRESENTATION_STYLE_ASSIGNMENT (( #8050 ) ) ;
#8412 = VECTOR ( 'NONE', #5611, 1000.000000000000000 ) ;
#8414 = ORIENTED_EDGE ( 'NONE', *, *, #20160, .F. ) ;
#8415 = CARTESIAN_POINT ( 'NONE',  ( -182.4550000000000125, 7.632228543268599452, -2.479861379858951942 ) ) ;
#8416 = FILL_AREA_STYLE_COLOUR ( '', #11651 ) ;
#8417 = FILL_AREA_STYLE_COLOUR ( '', #38127 ) ;
#8418 = CARTESIAN_POINT ( 'NONE',  ( -55.40707362346616094, 3.094860106618428031, -9.524999999999993250 ) ) ;
#8419 = AXIS2_PLACEMENT_3D ( 'NONE', #56979, #8793, #63975 ) ;
#8420 =( GEOMETRIC_REPRESENTATION_CONTEXT ( 3 ) GLOBAL_UNCERTAINTY_ASSIGNED_CONTEXT ( ( #52403 ) ) GLOBAL_UNIT_ASSIGNED_CONTEXT ( ( #26838, #64159, #43112 ) ) REPRESENTATION_CONTEXT ( 'NONE', 'WORKASPACE' ) );
#8421 = COLOUR_RGB ( '', 0.31764706, 0.68627451, 0.89019608) ;
#8422 = CARTESIAN_POINT ( 'NONE',  ( -176.0949999999999704, -2.607480562269071545, -8.024999999999991473 ) ) ;
#8423 = CARTESIAN_POINT ( 'NONE',  ( -178.2570736234661695, 5.598654528085800663, -7.705886871421367523 ) ) ;
#8424 = ORIENTED_EDGE ( 'NONE', *, *, #37926, .F. ) ;
#8425 = DIRECTION ( 'NONE',  ( 0.000000000000000000, 0.000000000000000000, 1.000000000000000000 ) ) ;
#8426 = CARTESIAN_POINT ( 'NONE',  ( -22.25000000000000711, 33.74999999999999289, 4.000000000000000000 ) ) ;
#8427 = CARTESIAN_POINT ( 'NONE',  ( 25.75000000000001066, 19.24999999999997868, -4.000000000000000000 ) ) ;
#8428 = CARTESIAN_POINT ( 'NONE',  ( -91.10500000000000398, -6.826472737025115478, 4.959722759717900331 ) ) ;
#8429 = CARTESIAN_POINT ( 'NONE',  ( -28.94829758246651252, -8.499999999999996447, -0.1896701972874017816 ) ) ;
#8430 = CARTESIAN_POINT ( 'NONE',  ( -168.9570736234661865, 9.058813317711329915, -2.943386871421373119 ) ) ;
#8431 = DIRECTION ( 'NONE',  ( -1.000000000000000000, 0.000000000000000000, 0.000000000000000000 ) ) ;
#8432 = AXIS2_PLACEMENT_3D ( 'NONE', #7273, #6542, #16218 ) ;
#8433 = AXIS2_PLACEMENT_3D ( 'NONE', #27539, #26163, #26511 ) ;
#8434 = CARTESIAN_POINT ( 'NONE',  ( -100.6449999999999818, 4.716976649647091513, -6.492361379858946790 ) ) ;
#8435 = CARTESIAN_POINT ( 'NONE',  ( -3.094860106618434248, 114.9049999999999727, 9.525000000000000355 ) ) ;
#8436 = CARTESIAN_POINT ( 'NONE',  ( -69.74499999999999034, 4.716976649647094177, 6.492361379858945902 ) ) ;
#8437 = LINE ( 'NONE', #55568, #10647 ) ;
#8438 = VECTOR ( 'NONE', #7506, 1000.000000000000000 ) ;
#8439 = ADVANCED_FACE ( 'NONE', ( #22768 ), #42887, .T. ) ;
#8440 = PLANE ( 'NONE',  #52922 ) ;
#8441 = STYLED_ITEM ( 'NONE', ( #29278 ), #56464 ) ;
#8442 = ADVANCED_FACE ( 'NONE', ( #11856 ), #11847, .T. ) ;
#8443 = CARTESIAN_POINT ( 'NONE',  ( 3.000000000000000444, 3.673940397442060361E-16, 7.500000000000000000 ) ) ;
#8444 = FILL_AREA_STYLE_COLOUR ( '', #24755 ) ;
#8445 = ORIENTED_EDGE ( 'NONE', *, *, #24228, .T. ) ;
#8446 = CARTESIAN_POINT ( 'NONE',  ( -116.3929263765338220, 8.102448949553176405, 5.886773742842740909 ) ) ;
#8447 = CARTESIAN_POINT ( 'NONE',  ( -131.9949999999999477, -6.826472737025115478, 4.959722759717900331 ) ) ;
#8448 = ADVANCED_FACE ( 'NONE', ( #32976 ), #1237, .T. ) ;
#8449 = LINE ( 'NONE', #29884, #57277 ) ;
#8450 = ADVANCED_FACE ( 'NONE', ( #44613 ), #51234, .T. ) ;
#8452 = LINE ( 'NONE', #57308, #37157 ) ;
#8451 = DIRECTION ( 'NONE',  ( 0.000000000000000000, 0.000000000000000000, -1.000000000000000000 ) ) ;
#8453 = ORIENTED_EDGE ( 'NONE', *, *, #57178, .F. ) ;
#8454 = ORIENTED_EDGE ( 'NONE', *, *, #36279, .T. ) ;
#8455 = CARTESIAN_POINT ( 'NONE',  ( -2.139492287038055877E-14, 27.74999999999994316, 3.750000000000000000 ) ) ;
#8456 = STYLED_ITEM ( 'NONE', ( #68053 ), #8127 ) ;
#8457 = EDGE_CURVE ( 'NONE', #5084, #41694, #26462, .T. ) ;
#8458 = FACE_OUTER_BOUND ( 'NONE', #2778, .T. ) ;
#8459 = CARTESIAN_POINT ( 'NONE',  ( 4.041451884327377897, 1.417096231345241319, 7.000000000000000888 ) ) ;
#8460 = LINE ( 'NONE', #45083, #1435 ) ;
#8461 = CARTESIAN_POINT ( 'NONE',  ( -126.6570736234661751, 9.058813317711329915, 2.943386871421369566 ) ) ;
#8462 = VERTEX_POINT ( 'NONE', #23794 ) ;
#8463 = CARTESIAN_POINT ( 'NONE',  ( -133.8549999999999898, 4.716976649647094177, 6.492361379858945902 ) ) ;
#8464 = ORIENTED_EDGE ( 'NONE', *, *, #2193, .T. ) ;
#8465 = CARTESIAN_POINT ( 'NONE',  ( -184.0000000000000000, 9.524999999999982592, 0.000000000000000000 ) ) ;
#8466 = CARTESIAN_POINT ( 'NONE',  ( -120.3570736234661780, 5.598654528085804216, 7.705886871421366635 ) ) ;
#8467 = ORIENTED_EDGE ( 'NONE', *, *, #32025, .F. ) ;
#8468 = CARTESIAN_POINT ( 'NONE',  ( 7.999999999999992895, 5.000000000000000000, -24.00402776293826079 ) ) ;
#8469 = CARTESIAN_POINT ( 'NONE',  ( 12.72792206135785698, 114.9999999999999574, -10.50000000000000000 ) ) ;
#8470 = EDGE_LOOP ( 'NONE', ( #56009, #36635, #19947 ) ) ;
#8471 = VECTOR ( 'NONE', #15149, 1000.000000000000114 ) ;
#8472 = VECTOR ( 'NONE', #26625, 1000.000000000000000 ) ;
#8473 = DIRECTION ( 'NONE',  ( -0.000000000000000000, -0.000000000000000000, 1.000000000000000000 ) ) ;
#8474 = CARTESIAN_POINT ( 'NONE',  ( -9.058813317711338797, 137.3449999999999989, 2.943386871421373563 ) ) ;
#8475 = DIRECTION ( 'NONE',  ( 0.000000000000000000, -0.000000000000000000, 1.000000000000000000 ) ) ;
#8476 = ORIENTED_EDGE ( 'NONE', *, *, #68395, .T. ) ;
#8477 = DIRECTION ( 'NONE',  ( -1.000000000000000000, 1.156482317317866302E-16, 0.000000000000000000 ) ) ;
#8478 = CARTESIAN_POINT ( 'NONE',  ( 10.01517768586949408, 136.8049999999999500, 1.839758294383810543E-15 ) ) ;
#8479 = LINE ( 'NONE', #13733, #68754 ) ;
#8480 = CARTESIAN_POINT ( 'NONE',  ( 0.000000000000000000, 115.4999999999999574, 0.000000000000000000 ) ) ;
#8481 = ORIENTED_EDGE ( 'NONE', *, *, #54574, .F. ) ;
#8482 = CARTESIAN_POINT ( 'NONE',  ( 4.716976649647096842, 112.7429263765338163, 6.492361379858953896 ) ) ;
#8483 = SURFACE_STYLE_FILL_AREA ( #40854 ) ;
#8484 = CARTESIAN_POINT ( 'NONE',  ( 21.75000000000001066, 21.74999999999998224, 4.000000000000000000 ) ) ;
#8485 =( LENGTH_UNIT ( ) NAMED_UNIT ( * ) SI_UNIT ( .MILLI., .METRE. ) );
#8486 = DIRECTION ( 'NONE',  ( 1.000000000000000000, 0.000000000000000000, -0.000000000000000000 ) ) ;
#8487 = ORIENTED_EDGE ( 'NONE', *, *, #33430, .T. ) ;
#8488 = CIRCLE ( 'NONE', #33179, 0.5000000000000004441 ) ;
#8489 = CARTESIAN_POINT ( 'NONE',  ( -145.9429263765337907, 0.000000000000000000, 9.524999999999991473 ) ) ;
#8490 = ORIENTED_EDGE ( 'NONE', *, *, #16704, .T. ) ;
#8491 = DIRECTION ( 'NONE',  ( -1.000000000000000000, 0.000000000000000000, 0.000000000000000000 ) ) ;
#8492 = DIRECTION ( 'NONE',  ( 1.000000000000000000, 0.000000000000000000, -0.000000000000000000 ) ) ;
#8493 = CARTESIAN_POINT ( 'NONE',  ( 21.25000000000001066, 24.74999999999998224, -3.750000000000000000 ) ) ;
#8494 = CARTESIAN_POINT ( 'NONE',  ( -160.4049999999999727, -2.607480562269069768, 8.024999999999991473 ) ) ;
#8495 = ORIENTED_EDGE ( 'NONE', *, *, #28312, .T. ) ;
#8496 = FILL_AREA_STYLE ('',( #52110 ) ) ;
#8497 = AXIS2_PLACEMENT_3D ( 'NONE', #34828, #8112, #47172 ) ;
#8498 = EDGE_CURVE ( 'NONE', #44728, #47926, #28711, .T. ) ;
#8499 = STYLED_ITEM ( 'NONE', ( #43174 ), #32251 ) ;
#8500 = CARTESIAN_POINT ( 'NONE',  ( -184.0000000000000000, 0.000000000000000000, 0.000000000000000000 ) ) ;
#8501 = CARTESIAN_POINT ( 'NONE',  ( 75.00000000000000000, 19.30628705663858113, 6.500000000000000888 ) ) ;
#8502 = ORIENTED_EDGE ( 'NONE', *, *, #51407, .T. ) ;
#8503 = DIRECTION ( 'NONE',  ( -0.000000000000000000, 1.000000000000000000, -0.000000000000000000 ) ) ;
#8504 = ORIENTED_EDGE ( 'NONE', *, *, #32354, .F. ) ;
#8505 = DIRECTION ( 'NONE',  ( 0.000000000000000000, 0.000000000000000000, 1.000000000000000000 ) ) ;
#8506 = CARTESIAN_POINT ( 'NONE',  ( -77.60499999999996135, 6.826472737025113702, -4.959722759717902107 ) ) ;
#8507 = ORIENTED_EDGE ( 'NONE', *, *, #53483, .F. ) ;
#8508 =( NAMED_UNIT ( * ) SI_UNIT ( $, .STERADIAN. ) SOLID_ANGLE_UNIT ( ) );
#8509 = PRESENTATION_LAYER_ASSIGNMENT (  '', '', ( #50041 ) ) ;
#8510 = SURFACE_STYLE_FILL_AREA ( #3885 ) ;
#8511 = VERTEX_POINT ( 'NONE', #50884 ) ;
#8512 = DIRECTION ( 'NONE',  ( -0.000000000000000000, -0.000000000000000000, 1.000000000000000000 ) ) ;
#8514 = CARTESIAN_POINT ( 'NONE',  ( 22.99999999999995026, 5.000000000000000000, -32.00402776293824303 ) ) ;
#8513 = CARTESIAN_POINT ( 'NONE',  ( 3.000000000000000444, 3.673940397442060361E-16, 32.50000000000000000 ) ) ;
#8515 = EDGE_CURVE ( 'NONE', #60522, #40281, #15262, .T. ) ;
#8516 = ADVANCED_FACE ( 'NONE', ( #17837 ), #12893, .T. ) ;
#8517 = CARTESIAN_POINT ( 'NONE',  ( 8.102448949553183510, 135.9950000000000045, -5.886773742842746238 ) ) ;
#8518 = CARTESIAN_POINT ( 'NONE',  ( -100.9449999999999932, -9.827790563157499189E-16, -8.024999999999991473 ) ) ;
#8519 = CARTESIAN_POINT ( 'NONE',  ( 3.999798566743339556, 8.867945265733707672, -2.000000000000000000 ) ) ;
#8520 = CIRCLE ( 'NONE', #68028, 0.7499999999999997780 ) ;
#8521 = PRESENTATION_STYLE_ASSIGNMENT (( #19031 ) ) ;
#8522 =( BOUNDED_CURVE ( )  B_SPLINE_CURVE ( 2, ( #29302, #29671, #51833, #2531, #19804, #30004, #35997, #2882, #14519, #45190, #18761 ),
 .UNSPECIFIED., .F., .F. ) 
 B_SPLINE_CURVE_WITH_KNOTS ( ( 3, 2, 2, 2, 2, 3 ),
 ( 0.7065217391304348116, 0.7086956521739130599, 0.7108695652173913082, 0.7130434782608695565, 0.7152173913043478048, 0.7173913043478260532 ),
 .UNSPECIFIED. ) 
 CURVE ( )  GEOMETRIC_REPRESENTATION_ITEM ( )  RATIONAL_B_SPLINE_CURVE ( ( 1.000000000000000000, 0.9510565162951535312, 1.000000000000000000, 0.9510565162951535312, 1.000000000000000000, 0.9510565162951535312, 1.000000000000000000, 0.9510565162951535312, 1.000000000000000000, 0.9510565162951535312, 1.000000000000000000 ) ) 
 REPRESENTATION_ITEM ( '' )  );
#8523 = ADVANCED_FACE ( 'NONE', ( #13578 ), #33250, .T. ) ;
#8525 = CARTESIAN_POINT ( 'NONE',  ( -70.94292637653380496, 0.000000000000000000, 9.524999999999991473 ) ) ;
#8524 = CARTESIAN_POINT ( 'NONE',  ( 15.48999599679679662, 117.4999999999999716, 10.00000000000000000 ) ) ;
#8526 = CARTESIAN_POINT ( 'NONE',  ( -140.6929263765338192, 10.01517768586948698, -1.839758294383808571E-15 ) ) ;
#8527 = FILL_AREA_STYLE ('',( #29962 ) ) ;
#8528 = FILL_AREA_STYLE ('',( #61961 ) ) ;
#8529 = CARTESIAN_POINT ( 'NONE',  ( -165.4450000000000216, 0.000000000000000000, 8.024999999999991473 ) ) ;
#8530 =( GEOMETRIC_REPRESENTATION_CONTEXT ( 3 ) GLOBAL_UNCERTAINTY_ASSIGNED_CONTEXT ( ( #63659 ) ) GLOBAL_UNIT_ASSIGNED_CONTEXT ( ( #52851, #47617, #15569 ) ) REPRESENTATION_CONTEXT ( 'NONE', 'WORKASPACE' ) );
#8531 = SURFACE_SIDE_STYLE ('',( #51783 ) ) ;
#8532 = AXIS2_PLACEMENT_3D ( 'NONE', #59396, #48216, #21434 ) ;
#8533 = EDGE_CURVE ( 'NONE', #30209, #27227, #55460, .T. ) ;
#8534 = PRESENTATION_LAYER_ASSIGNMENT (  '', '', ( #50117 ) ) ;
#8535 = ORIENTED_EDGE ( 'NONE', *, *, #64872, .F. ) ;
#8536 = CARTESIAN_POINT ( 'NONE',  ( -2.607480562269053781, 128.4070736234661467, 8.025000000000016342 ) ) ;
#8537 = ORIENTED_EDGE ( 'NONE', *, *, #47730, .F. ) ;
#8538 = CIRCLE ( 'NONE', #47911, 0.2500000000000002220 ) ;
#8539 = ADVANCED_FACE ( 'NONE', ( #68116 ), #19192, .F. ) ;
#8540 = CARTESIAN_POINT ( 'NONE',  ( -18.00000000000000711, 33.74999999999999289, 4.000000000000000000 ) ) ;
#8541 = FACE_OUTER_BOUND ( 'NONE', #6819, .T. ) ;
#8542 = DIRECTION ( 'NONE',  ( -1.000000000000000000, 0.000000000000000000, 0.000000000000000000 ) ) ;
#8543 = PRESENTATION_STYLE_ASSIGNMENT (( #39525 ) ) ;
#8544 = ORIENTED_EDGE ( 'NONE', *, *, #29228, .T. ) ;
#8545 = CARTESIAN_POINT ( 'NONE',  ( -164.3049999999999784, 8.437984349512086979, -1.550032578732815448E-15 ) ) ;
#8546 = VERTEX_POINT ( 'NONE', #47034 ) ;
#8547 =( LENGTH_UNIT ( ) NAMED_UNIT ( * ) SI_UNIT ( .MILLI., .METRE. ) );
#8548 = ORIENTED_EDGE ( 'NONE', *, *, #41407, .T. ) ;
#8549 = FILL_AREA_STYLE_COLOUR ( '', #25289 ) ;
#8550 = CARTESIAN_POINT ( 'NONE',  ( 8.102448949553181734, 114.3949999999999676, 5.886773742842750679 ) ) ;
#8551 =( GEOMETRIC_REPRESENTATION_CONTEXT ( 3 ) GLOBAL_UNCERTAINTY_ASSIGNED_CONTEXT ( ( #19365 ) ) GLOBAL_UNIT_ASSIGNED_CONTEXT ( ( #36821, #20247, #9017 ) ) REPRESENTATION_CONTEXT ( 'NONE', 'WORKASPACE' ) );
#8552 = ORIENTED_EDGE ( 'NONE', *, *, #50765, .F. ) ;
#8553 = PLANE ( 'NONE',  #13959 ) ;
#8554 = FACE_OUTER_BOUND ( 'NONE', #50185, .T. ) ;
#8555 = CARTESIAN_POINT ( 'NONE',  ( -76.55499999999997840, 0.000000000000000000, 8.024999999999991473 ) ) ;
#8556 = CARTESIAN_POINT ( 'NONE',  ( -79.70707362346615810, -3.094860106618431139, -9.524999999999991473 ) ) ;
#8557 = EDGE_LOOP ( 'NONE', ( #24973, #11217, #8707, #48937 ) ) ;
#8558 = CARTESIAN_POINT ( 'NONE',  ( 0.000000000000000000, 140.5549999999999784, -9.525000000000000355 ) ) ;
#8559 = DIRECTION ( 'NONE',  ( 1.000000000000000000, 0.000000000000000000, 0.000000000000000000 ) ) ;
#8560 = DIRECTION ( 'NONE',  ( -0.000000000000000000, 1.000000000000000000, -0.000000000000000000 ) ) ;
#8561 = AXIS2_PLACEMENT_3D ( 'NONE', #60118, #5949, #32683 ) ;
#8562 = FILL_AREA_STYLE_COLOUR ( '', #11819 ) ;
#8563 = AXIS2_PLACEMENT_3D ( 'NONE', #26449, #53210, #57432 ) ;
#8564 = CIRCLE ( 'NONE', #44554, 0.5000000000000004441 ) ;
#8565 = EDGE_LOOP ( 'NONE', ( #31997, #16219, #50175, #43650 ) ) ;
#8566 = PRESENTATION_LAYER_ASSIGNMENT (  '', '', ( #29892 ) ) ;
#8567 = FILL_AREA_STYLE ('',( #45183 ) ) ;
#8568 = CARTESIAN_POINT ( 'NONE',  ( -48.29499999999997328, -2.607480562269069768, 8.024999999999991473 ) ) ;
#8569 = ORIENTED_EDGE ( 'NONE', *, *, #32823, .F. ) ;
#8570 =( LENGTH_UNIT ( ) NAMED_UNIT ( * ) SI_UNIT ( .MILLI., .METRE. ) );
#8571 = ADVANCED_FACE ( 'NONE', ( #56858 ), #28703, .F. ) ;
#8572 = DIRECTION ( 'NONE',  ( 0.000000000000000000, 0.000000000000000000, 1.000000000000000000 ) ) ;
#8573 = DIRECTION ( 'NONE',  ( 0.000000000000000000, 0.000000000000000000, 1.000000000000000000 ) ) ;
#8574 = ORIENTED_EDGE ( 'NONE', *, *, #32823, .T. ) ;
#8575 = FACE_OUTER_BOUND ( 'NONE', #31739, .T. ) ;
#8576 = EDGE_LOOP ( 'NONE', ( #56182, #68047 ) ) ;
#8577 = CONICAL_SURFACE ( 'NONE', #27612, 7.000000000000000888, 0.7853981633974500554 ) ;
#8578 = FILL_AREA_STYLE_COLOUR ( '', #37104 ) ;
#8579 = CARTESIAN_POINT ( 'NONE',  ( -108.6549999999999869, -7.632228543268600340, -2.479861379858950166 ) ) ;
#8580 = ORIENTED_EDGE ( 'NONE', *, *, #45856, .T. ) ;
#8581 = DIRECTION ( 'NONE',  ( 2.312964634635740689E-15, -1.000000000000000000, 0.000000000000000000 ) ) ;
#8582 = CARTESIAN_POINT ( 'NONE',  ( -141.3570736234661638, 5.598654528085804216, 7.705886871421366635 ) ) ;
#8583 = CARTESIAN_POINT ( 'NONE',  ( -72.50000000000000000, 36.32520566882265456, 10.00000000000000000 ) ) ;
#8584 = CARTESIAN_POINT ( 'NONE',  ( 3.094860106618431583, 138.0949999999999989, 9.525000000000000355 ) ) ;
#8585 = COLOUR_RGB ( '', 0.66274510, 0.83137255, 0.94901961) ;
#8586 = CARTESIAN_POINT ( 'NONE',  ( -71.75707362346616947, -5.598654528085801552, 7.705886871421367523 ) ) ;
#8587 = EDGE_CURVE ( 'NONE', #50288, #37037, #7394, .T. ) ;
#8589 = EDGE_CURVE ( 'NONE', #65035, #11349, #41752, .T. ) ;
#8588 = CARTESIAN_POINT ( 'NONE',  ( -93.44292637653380496, -1.166476076187852838E-15, -9.524999999999991473 ) ) ;
#8590 = CARTESIAN_POINT ( 'NONE',  ( -16.30447726496212368, -10.98532143068888622, 4.829644968601866317 ) ) ;
#8591 = DIRECTION ( 'NONE',  ( -0.000000000000000000, 1.000000000000000000, -0.000000000000000000 ) ) ;
#8592 = EDGE_CURVE ( 'NONE', #20703, #16182, #586, .T. ) ;
#8593 = CARTESIAN_POINT ( 'NONE',  ( -118.4049999999999869, -2.607480562269069768, 8.024999999999991473 ) ) ;
#8594 = EDGE_CURVE ( 'NONE', #58540, #62495, #35515, .T. ) ;
#8595 = CARTESIAN_POINT ( 'NONE',  ( -158.6929263765338192, 10.01517768586948698, -1.839758294383808966E-15 ) ) ;
#8596 = CARTESIAN_POINT ( 'NONE',  ( 3.094860106618431583, 111.0949999999999704, 9.525000000000000355 ) ) ;
#8597 = CARTESIAN_POINT ( 'NONE',  ( -134.0949999999999420, -2.607480562269071545, -8.024999999999991473 ) ) ;
#8598 = CARTESIAN_POINT ( 'NONE',  ( -123.7449999999999903, 4.716976649647094177, 6.492361379858945902 ) ) ;
#8599 = FILL_AREA_STYLE ('',( #56785 ) ) ;
#8600 = VERTEX_POINT ( 'NONE', #68449 ) ;
#8601 = DIRECTION ( 'NONE',  ( 1.000000000000000000, 0.000000000000000000, 0.000000000000000000 ) ) ;
#8602 = EDGE_CURVE ( 'NONE', #41301, #14677, #16416, .T. ) ;
#8603 = CARTESIAN_POINT ( 'NONE',  ( 2.999999999999996447, 5.000000000000000000, -37.00402776293829277 ) ) ;
#8604 = CARTESIAN_POINT ( 'NONE',  ( -175.6429263765338078, -5.598654528085801552, 7.705886871421367523 ) ) ;
#8605 = CARTESIAN_POINT ( 'NONE',  ( -52.19499999999999318, 8.437984349512085203, -1.550032578732815448E-15 ) ) ;
#8606 = EDGE_CURVE ( 'NONE', #29207, #54497, #20625, .T. ) ;
#8607 = TOROIDAL_SURFACE ( 'NONE', #26556, 2.000000000000000000, 1.000000000000000000 ) ;
#8608 = VECTOR ( 'NONE', #33034, 1000.000000000000000 ) ;
#8609 = CARTESIAN_POINT ( 'NONE',  ( -4.716976649647097730, 124.3570736234661496, -6.492361379858953896 ) ) ;
#8610 = MECHANICAL_DESIGN_GEOMETRIC_PRESENTATION_REPRESENTATION (  '', ( #44597 ), #13068 ) ;
#8611 = CARTESIAN_POINT ( 'NONE',  ( 98.00000000000000000, 0.000000000000000000, -5.000000000000004441 ) ) ;
#8612 = CARTESIAN_POINT ( 'NONE',  ( -19.89974874213240597, 115.4999999999999574, 10.00000000000000000 ) ) ;
#8613 = VERTEX_POINT ( 'NONE', #37173 ) ;
#8614 = CARTESIAN_POINT ( 'NONE',  ( -88.19292637653379074, -10.01517768586948698, 6.132527647946031529E-16 ) ) ;
#8615 = CARTESIAN_POINT ( 'NONE',  ( -53.31913400974866590, -10.00145578784314715, -3.271963658655177021 ) ) ;
#8616 =( BOUNDED_CURVE ( )  B_SPLINE_CURVE ( 2, ( #39963, #50831, #37821, #57854, #68755, #20546, #41691, #25469, #64140, #69099, #52918 ),
 .UNSPECIFIED., .F., .F. ) 
 B_SPLINE_CURVE_WITH_KNOTS ( ( 3, 2, 2, 2, 2, 3 ),
 ( 0.7941176470588233727, 0.7999999999999999334, 0.8058823529411763831, 0.8117647058823528328, 0.8176470588235292825, 0.8235294117647057321 ),
 .UNSPECIFIED. ) 
 CURVE ( )  GEOMETRIC_REPRESENTATION_ITEM ( )  RATIONAL_B_SPLINE_CURVE ( ( 1.000000000000000888, 0.9510565162951526430, 1.000000000000000000, 0.9510565162951535312, 1.000000000000000000, 0.9510565162951535312, 1.000000000000000000, 0.9510565162951535312, 1.000000000000000000, 0.9510565162951544194, 0.9999999999999991118 ) ) 
 REPRESENTATION_ITEM ( '' )  );
#8617 = FILL_AREA_STYLE ('',( #51510 ) ) ;
#8618 = CARTESIAN_POINT ( 'NONE',  ( -5.249999999999997335, 0.000000000000000000, 0.000000000000000000 ) ) ;
#8619 = SURFACE_STYLE_FILL_AREA ( #30376 ) ;
#8620 = CIRCLE ( 'NONE', #13076, 5.000000000000004441 ) ;
#8621 = DIRECTION ( 'NONE',  ( -1.000000000000000000, 0.000000000000000000, 0.000000000000000000 ) ) ;
#8622 = ORIENTED_EDGE ( 'NONE', *, *, #36046, .F. ) ;
#8623 = DIRECTION ( 'NONE',  ( -1.000000000000000000, -0.000000000000000000, -0.000000000000000000 ) ) ;
#8624 = ORIENTED_EDGE ( 'NONE', *, *, #27852, .F. ) ;
#8625 = DIRECTION ( 'NONE',  ( -0.000000000000000000, -0.000000000000000000, 1.000000000000000000 ) ) ;
#8626 = EDGE_CURVE ( 'NONE', #5418, #17013, #5785, .T. ) ;
#8627 = FILL_AREA_STYLE_COLOUR ( '', #42126 ) ;
#8628 = CARTESIAN_POINT ( 'NONE',  ( 8.437984349512095861, 129.3070736234661524, 1.550032578732817026E-15 ) ) ;
#8629 = PRESENTATION_LAYER_ASSIGNMENT (  '', '', ( #61419 ) ) ;
#8630 = EDGE_LOOP ( 'NONE', ( #41716, #67374, #51357, #51942 ) ) ;
#8631 = SURFACE_STYLE_FILL_AREA ( #18493 ) ;
#8632 = CARTESIAN_POINT ( 'NONE',  ( -101.9049999999999869, 2.607480562269069324, -8.024999999999993250 ) ) ;
#8633 = CARTESIAN_POINT ( 'NONE',  ( 74.99999999999998579, 19.62820054891026444, -6.498343828034972347 ) ) ;
#8634 = CIRCLE ( 'NONE', #48007, 4.999999999999997335 ) ;
#8635 =( NAMED_UNIT ( * ) PLANE_ANGLE_UNIT ( ) SI_UNIT ( $, .RADIAN. ) );
#8636 = VERTEX_POINT ( 'NONE', #37880 ) ;
#8637 = CYLINDRICAL_SURFACE ( 'NONE', #56814, 3.499999999999999556 ) ;
#8638 = LINE ( 'NONE', #62074, #44013 ) ;
#8639 = CARTESIAN_POINT ( 'NONE',  ( -76.75000000000000000, 4.336808689942018722E-16, 20.00000000000000000 ) ) ;
#8640 =( NAMED_UNIT ( * ) SI_UNIT ( $, .STERADIAN. ) SOLID_ANGLE_UNIT ( ) );
#8641 = DIRECTION ( 'NONE',  ( -0.000000000000000000, 1.000000000000000000, -0.000000000000000000 ) ) ;
#8642 = CARTESIAN_POINT ( 'NONE',  ( -85.64499999999998181, 4.716976649647091513, -6.492361379858946790 ) ) ;
#8643 = ORIENTED_EDGE ( 'NONE', *, *, #32236, .F. ) ;
#8644 = DIRECTION ( 'NONE',  ( 0.000000000000000000, 0.000000000000000000, -1.000000000000000000 ) ) ;
#8645 = PRESENTATION_STYLE_ASSIGNMENT (( #3305 ) ) ;
#8646 = UNCERTAINTY_MEASURE_WITH_UNIT (LENGTH_MEASURE( 1.000000000000000082E-05 ), #26456, 'distance_accuracy_value', 'NONE');
#8647 = ORIENTED_EDGE ( 'NONE', *, *, #7661, .F. ) ;
#8648 = CARTESIAN_POINT ( 'NONE',  ( -24.00000000000000355, 36.75000000000000000, 3.750000000000000000 ) ) ;
#8649 = PRESENTATION_STYLE_ASSIGNMENT (( #18834 ) ) ;
#8650 =( GEOMETRIC_REPRESENTATION_CONTEXT ( 3 ) GLOBAL_UNCERTAINTY_ASSIGNED_CONTEXT ( ( #43932 ) ) GLOBAL_UNIT_ASSIGNED_CONTEXT ( ( #17754, #30261, #45806 ) ) REPRESENTATION_CONTEXT ( 'NONE', 'WORKASPACE' ) );
#8651 = CARTESIAN_POINT ( 'NONE',  ( 179.4361977533490631, 0.000000000000000000, -103.7004518695262192 ) ) ;
#8652 = ORIENTED_EDGE ( 'NONE', *, *, #17662, .T. ) ;
#8653 = DIRECTION ( 'NONE',  ( 0.000000000000000000, 0.000000000000000000, 1.000000000000000000 ) ) ;
#8654 = ORIENTED_EDGE ( 'NONE', *, *, #11928, .F. ) ;
#8655 = CIRCLE ( 'NONE', #65943, 5.000000000000004441 ) ;
#8656 = FILL_AREA_STYLE ('',( #63502 ) ) ;
#8657 = CARTESIAN_POINT ( 'NONE',  ( -136.5570736234661808, -1.166476076187852838E-15, -9.524999999999991473 ) ) ;
#8658 = CARTESIAN_POINT ( 'NONE',  ( -171.9570736234661865, 9.058813317711329915, -2.943386871421373119 ) ) ;
#8659 = FACE_OUTER_BOUND ( 'NONE', #43764, .T. ) ;
#8660 = CARTESIAN_POINT ( 'NONE',  ( -9.058813317711338797, 116.3449999999999847, 2.943386871421373563 ) ) ;
#8661 = CARTESIAN_POINT ( 'NONE',  ( -107.9070736234661894, -3.094860106618429807, 9.524999999999991473 ) ) ;
#8662 = ADVANCED_FACE ( 'NONE', ( #469 ), #59962, .T. ) ;
#8663 = FILL_AREA_STYLE_COLOUR ( '', #31794 ) ;
#8664 = CARTESIAN_POINT ( 'NONE',  ( -66.05707362346618083, 0.000000000000000000, 9.524999999999991473 ) ) ;
#8666 = ORIENTED_EDGE ( 'NONE', *, *, #30569, .F. ) ;
#8665 = B_SPLINE_CURVE_WITH_KNOTS ( 'NONE', 3,
 ( #45996, #67419, #14942, #60565, #64828, #1076, #43763, #38500 ),
 .UNSPECIFIED., .F., .F.,
 ( 4, 2, 2, 4 ),
 ( 2.544313220902908671E-07, 0.002693395767724538360, 0.004039966435925761504, 0.005386537104126985082 ),
 .UNSPECIFIED. ) ;
#8667 = CARTESIAN_POINT ( 'NONE',  ( -107.9929263765337879, 8.102448949553172852, -5.886773742842744461 ) ) ;
#8668 = CARTESIAN_POINT ( 'NONE',  ( -82.79292637653381348, -3.094860106618429807, 9.524999999999991473 ) ) ;
#8670 = CARTESIAN_POINT ( 'NONE',  ( 44.00000000000000000, 21.99999999999998579, 4.000000000000000000 ) ) ;
#8669 = CARTESIAN_POINT ( 'NONE',  ( 68.99999999999998579, 1.000000000000008438, 4.000000000000000000 ) ) ;
#8671 = PRESENTATION_STYLE_ASSIGNMENT (( #30796 ) ) ;
#8672 = AXIS2_PLACEMENT_3D ( 'NONE', #62766, #51901, #6036 ) ;
#8673 = EDGE_CURVE ( 'NONE', #40899, #41694, #36665, .T. ) ;
#8674 = CARTESIAN_POINT ( 'NONE',  ( -149.6050000000000182, 6.826472737025113702, -4.959722759717902107 ) ) ;
#8675 = CARTESIAN_POINT ( 'NONE',  ( -75.00000000000000000, 9.372904743120718862, 6.583929160757660881 ) ) ;
#8676 = CARTESIAN_POINT ( 'NONE',  ( -148.6429263765338078, -5.598654528085801552, 7.705886871421367523 ) ) ;
#8677 = CARTESIAN_POINT ( 'NONE',  ( -162.7450000000000045, 4.716976649647094177, 6.492361379858945902 ) ) ;
#8678 = CARTESIAN_POINT ( 'NONE',  ( -145.6450000000000102, 4.716976649647091513, -6.492361379858946790 ) ) ;
#8679 = VERTEX_POINT ( 'NONE', #43153 ) ;
#8680 = CARTESIAN_POINT ( 'NONE',  ( -8.021777294149474713, 4.105874159530735312, 1.233279971202261294E-15 ) ) ;
#8681 = DIRECTION ( 'NONE',  ( -0.5000000000000001110, -0.8660254037844385966, 0.000000000000000000 ) ) ;
#8682 = CARTESIAN_POINT ( 'NONE',  ( -61.70499999999997698, 2.607480562269073321, 8.024999999999991473 ) ) ;
#8683 = CARTESIAN_POINT ( 'NONE',  ( 2.786071468060228170E-15, 154.9999999999999716, 22.49999999999999645 ) ) ;
#8684 = EDGE_CURVE ( 'NONE', #57903, #37864, #6268, .T. ) ;
#8685 = CARTESIAN_POINT ( 'NONE',  ( -63.89499999999998181, 6.826472737025115478, 4.959722759717899443 ) ) ;
#8686 = CARTESIAN_POINT ( 'NONE',  ( 8.102448949553183510, 158.1049999999999898, -5.886773742842746238 ) ) ;
#8687 = CARTESIAN_POINT ( 'NONE',  ( -60.00000000000000000, -2.024042244987997205E-14, -6.500000000000000000 ) ) ;
#8688 = DIRECTION ( 'NONE',  ( 0.000000000000000000, 0.000000000000000000, 1.000000000000000000 ) ) ;
#8689 = UNCERTAINTY_MEASURE_WITH_UNIT (LENGTH_MEASURE( 1.000000000000000082E-05 ), #38219, 'distance_accuracy_value', 'NONE');
#8690 = CARTESIAN_POINT ( 'NONE',  ( -80.49999999999995737, 50.00000000000000000, -12.00000000000000000 ) ) ;
#8691 = DIRECTION ( 'NONE',  ( 1.000000000000000000, -0.000000000000000000, 0.000000000000000000 ) ) ;
#8692 = CARTESIAN_POINT ( 'NONE',  ( 23.71231517720798010, 117.4999999999999716, -7.000000000000000000 ) ) ;
#8693 = CIRCLE ( 'NONE', #65970, 5.000000000000000000 ) ;
#8694 = COLOUR_RGB ( '', 0.72549020, 0.75294118, 0.79215686) ;
#8695 = STYLED_ITEM ( 'NONE', ( #47551 ), #3795 ) ;
#8696 = EDGE_CURVE ( 'NONE', #6724, #16463, #43830, .T. ) ;
#8697 = FILL_AREA_STYLE_COLOUR ( '', #8345 ) ;
#8698 = DIRECTION ( 'NONE',  ( -1.000000000000000000, 0.000000000000000000, 0.000000000000000000 ) ) ;
#8699 = VERTEX_POINT ( 'NONE', #48078 ) ;
#8700 = ORIENTED_EDGE ( 'NONE', *, *, #5104, .T. ) ;
#8701 = CARTESIAN_POINT ( 'NONE',  ( -60.95707362346616520, 9.058813317711329915, -2.943386871421373119 ) ) ;
#8702 = EDGE_CURVE ( 'NONE', #7479, #65906, #1708, .T. ) ;
#8703 = CARTESIAN_POINT ( 'NONE',  ( 0.000000000000000000, 109.0570736234661524, -8.025000000000000355 ) ) ;
#8704 = DIRECTION ( 'NONE',  ( -0.7833176619561783571, -0.6216216216216310375, 0.000000000000000000 ) ) ;
#8705 = CIRCLE ( 'NONE', #45837, 0.5000000000000004441 ) ;
#8706 = CARTESIAN_POINT ( 'NONE',  ( 23.00000000000000000, 5.000000000000000000, -24.00402776293825013 ) ) ;
#8707 = ORIENTED_EDGE ( 'NONE', *, *, #13658, .F. ) ;
#8708 = ORIENTED_EDGE ( 'NONE', *, *, #29458, .T. ) ;
#8709 = VERTEX_POINT ( 'NONE', #37531 ) ;
#8710 = CARTESIAN_POINT ( 'NONE',  ( -3.094860106618432471, 110.7049999999999983, -9.525000000000000355 ) ) ;
#8711 = CARTESIAN_POINT ( 'NONE',  ( -145.9429263765337907, 0.000000000000000000, 9.524999999999991473 ) ) ;
#8712 = VERTEX_POINT ( 'NONE', #58936 ) ;
#8713 = CARTESIAN_POINT ( 'NONE',  ( -15.48999599679679662, 118.4999999999999716, -9.500000000000000000 ) ) ;
#8714 = SURFACE_SIDE_STYLE ('',( #19606 ) ) ;
#8715 = CARTESIAN_POINT ( 'NONE',  ( -108.1449999999999960, -4.716976649647092401, 6.492361379858946790 ) ) ;
#8716 = EDGE_LOOP ( 'NONE', ( #36734, #49457, #48984, #32874 ) ) ;
#8717 = DIRECTION ( 'NONE',  ( 0.000000000000000000, 1.000000000000000000, 0.000000000000000000 ) ) ;
#8718 = CARTESIAN_POINT ( 'NONE',  ( -72.49999999999998579, 119.9999999999997868, 9.500000000000000000 ) ) ;
#8719 = DIRECTION ( 'NONE',  ( 0.000000000000000000, 0.000000000000000000, 1.000000000000000000 ) ) ;
#8720 = VERTEX_POINT ( 'NONE', #17089 ) ;
#8721 = CARTESIAN_POINT ( 'NONE',  ( -8.437984349512095861, 141.6929263765338476, -5.166775262442723748E-16 ) ) ;
#8722 = CARTESIAN_POINT ( 'NONE',  ( -54.10982952226344622, -9.443833522991335272, -2.300020890959020736 ) ) ;
#8723 = PRESENTATION_STYLE_ASSIGNMENT (( #14004 ) ) ;
#8724 = FILL_AREA_STYLE ('',( #8027 ) ) ;
#8725 = ORIENTED_EDGE ( 'NONE', *, *, #67837, .F. ) ;
#8726 = EDGE_CURVE ( 'NONE', #8546, #45132, #53644, .T. ) ;
#8727 = DIRECTION ( 'NONE',  ( 0.000000000000000000, 1.000000000000000000, 0.000000000000000000 ) ) ;
#8728 = ORIENTED_EDGE ( 'NONE', *, *, #67682, .F. ) ;
#8729 = CARTESIAN_POINT ( 'NONE',  ( 0.000000000000000000, 128.9429263765338192, -8.025000000000000355 ) ) ;
#8730 = DIRECTION ( 'NONE',  ( -0.000000000000000000, 1.000000000000000000, -0.000000000000000000 ) ) ;
#8731 = CARTESIAN_POINT ( 'NONE',  ( 24.21231517720798010, 113.4999999999999858, 9.500000000000000000 ) ) ;
#8732 = DIRECTION ( 'NONE',  ( -0.8660254037844385966, 0.000000000000000000, -0.5000000000000003331 ) ) ;
#8733 = CARTESIAN_POINT ( 'NONE',  ( -126.9549999999999841, -7.632228543268599452, 2.479861379858951054 ) ) ;
#8734 = DIRECTION ( 'NONE',  ( 1.000000000000000000, -0.000000000000000000, 0.000000000000000000 ) ) ;
#8735 = DIRECTION ( 'NONE',  ( 0.000000000000000000, 0.000000000000000000, 1.000000000000000000 ) ) ;
#8736 = AXIS2_PLACEMENT_3D ( 'NONE', #46530, #68992, #4951 ) ;
#8737 = CARTESIAN_POINT ( 'NONE',  ( -47.71347897792733761, -13.42724224818812040, 0.9185643661977238583 ) ) ;
#8738 = LINE ( 'NONE', #40778, #40702 ) ;
#8739 = FILL_AREA_STYLE_COLOUR ( '', #39367 ) ;
#8740 = VERTEX_POINT ( 'NONE', #6154 ) ;
#8741 = VECTOR ( 'NONE', #27894, 1000.000000000000114 ) ;
#8742 = ORIENTED_EDGE ( 'NONE', *, *, #44817, .T. ) ;
#8743 = LINE ( 'NONE', #14022, #35051 ) ;
#8744 = CIRCLE ( 'NONE', #69450, 0.2500000000000002220 ) ;
#8745 = CARTESIAN_POINT ( 'NONE',  ( -32.17428486863278181, -8.821435577490872149, -1.966464606294938910 ) ) ;
#8746 = LINE ( 'NONE', #67138, #26643 ) ;
#8747 = FACE_OUTER_BOUND ( 'NONE', #26161, .T. ) ;
#8748 = ORIENTED_EDGE ( 'NONE', *, *, #101, .F. ) ;
#8749 = EDGE_CURVE ( 'NONE', #67943, #51712, #17549, .T. ) ;
#8750 = CARTESIAN_POINT ( 'NONE',  ( -181.8549999999999898, 4.716976649647094177, 6.492361379858945902 ) ) ;
#8751 = CARTESIAN_POINT ( 'NONE',  ( 6.000000000000017764, 26.00000000000000355, 20.49999999999999645 ) ) ;
#8752 = CARTESIAN_POINT ( 'NONE',  ( -60.35707362346616378, 5.598654528085804216, 7.705886871421366635 ) ) ;
#8753 = VECTOR ( 'NONE', #5450, 1000.000000000000000 ) ;
#8754 = ADVANCED_FACE ( 'NONE', ( #35231 ), #56691, .T. ) ;
#8755 = CARTESIAN_POINT ( 'NONE',  ( -172.6449999999999818, 4.716976649647091513, -6.492361379858946790 ) ) ;
#8756 = DIRECTION ( 'NONE',  ( 0.000000000000000000, 0.000000000000000000, 1.000000000000000000 ) ) ;
#8757 = ORIENTED_EDGE ( 'NONE', *, *, #7396, .F. ) ;
#8758 = FACE_OUTER_BOUND ( 'NONE', #35653, .T. ) ;
#8759 = ADVANCED_FACE ( 'NONE', ( #17436 ), #55380, .T. ) ;
#8760 = CARTESIAN_POINT ( 'NONE',  ( 21.02379604162863913, 109.9999999999999858, 9.500000000000000000 ) ) ;
#8761 = CARTESIAN_POINT ( 'NONE',  ( -75.00000000000000000, -2.215169945516535778E-14, 10.00000000000000000 ) ) ;
#8762 = CARTESIAN_POINT ( 'NONE',  ( -90.50499999999999545, -6.826472737025115478, -4.959722759717899443 ) ) ;
#8763 = PLANE ( 'NONE',  #13459 ) ;
#8764 = CARTESIAN_POINT ( 'NONE',  ( 0.000000000000000000, 0.000000000000000000, 0.000000000000000000 ) ) ;
#8766 = EDGE_CURVE ( 'NONE', #51395, #11136, #40051, .T. ) ;
#8765 = CIRCLE ( 'NONE', #14373, 4.000000000000000000 ) ;
#8767 = CARTESIAN_POINT ( 'NONE',  ( -94.34499999999998465, 7.632228543268599452, -2.479861379858951942 ) ) ;
#8768 = CARTESIAN_POINT ( 'NONE',  ( 5.598654528085805993, 130.3549999999999898, 7.705886871421374629 ) ) ;
#8769 = CARTESIAN_POINT ( 'NONE',  ( -66.14499999999998181, -4.716976649647092401, 6.492361379858946790 ) ) ;
#8770 = CARTESIAN_POINT ( 'NONE',  ( 20.46171737063437845, 114.7896496367841905, -10.31361660310133388 ) ) ;
#8771 = FILL_AREA_STYLE ('',( #52401 ) ) ;
#8772 = CARTESIAN_POINT ( 'NONE',  ( 17.15973193263811680, -3.000000000000000000, 12.50000000000000000 ) ) ;
#8773 = UNCERTAINTY_MEASURE_WITH_UNIT (LENGTH_MEASURE( 1.000000000000000082E-05 ), #41209, 'distance_accuracy_value', 'NONE');
#8774 =( NAMED_UNIT ( * ) SI_UNIT ( $, .STERADIAN. ) SOLID_ANGLE_UNIT ( ) );
#8775 = FILL_AREA_STYLE ('',( #25291 ) ) ;
#8776 = ORIENTED_EDGE ( 'NONE', *, *, #61250, .T. ) ;
#8777 = CARTESIAN_POINT ( 'NONE',  ( -110.3929263765337936, 8.102448949553176405, 5.886773742842740909 ) ) ;
#8778 = CARTESIAN_POINT ( 'NONE',  ( -133.0449999999999875, 7.632228543268600340, 2.479861379858949277 ) ) ;
#8779 = FILL_AREA_STYLE ('',( #57305 ) ) ;
#8780 = DIRECTION ( 'NONE',  ( 1.000000000000000000, 0.000000000000000000, 0.000000000000000000 ) ) ;
#8781 = FACE_OUTER_BOUND ( 'NONE', #51788, .T. ) ;
#8782 = ORIENTED_EDGE ( 'NONE', *, *, #59566, .F. ) ;
#8783 = ORIENTED_EDGE ( 'NONE', *, *, #53794, .T. ) ;
#8784 = CARTESIAN_POINT ( 'NONE',  ( 31.00000000000000000, 42.00000000000000000, -75.00000000000001421 ) ) ;
#8785 = CARTESIAN_POINT ( 'NONE',  ( -195.0000000000000000, 0.000000000000000000, 0.000000000000000000 ) ) ;
#8786 = TOROIDAL_SURFACE ( 'NONE', #26738, 1.000000000000000000, 0.5000000000000000000 ) ;
#8787 = LINE ( 'NONE', #30215, #54261 ) ;
#8789 = CARTESIAN_POINT ( 'NONE',  ( 4.750000000000002665, 24.99999999999998579, -3.750000000000000000 ) ) ;
#8788 = VECTOR ( 'NONE', #34274, 1000.000000000000000 ) ;
#8790 = EDGE_LOOP ( 'NONE', ( #24170, #2580, #11051, #14207 ) ) ;
#8791 = CARTESIAN_POINT ( 'NONE',  ( -133.7049999999999557, 2.607480562269072433, 8.024999999999991473 ) ) ;
#8792 = ORIENTED_EDGE ( 'NONE', *, *, #28967, .F. ) ;
#8793 = DIRECTION ( 'NONE',  ( -0.000000000000000000, 0.000000000000000000, -1.000000000000000000 ) ) ;
#8794 = CARTESIAN_POINT ( 'NONE',  ( -123.3570736234661780, 5.598654528085804216, 7.705886871421366635 ) ) ;
#8795 = ORIENTED_EDGE ( 'NONE', *, *, #23574, .T. ) ;
#8796 = LINE ( 'NONE', #46475, #51559 ) ;
#8797 = DIRECTION ( 'NONE',  ( 1.000000000000000000, -0.000000000000000000, 0.000000000000000000 ) ) ;
#8798 = EDGE_LOOP ( 'NONE', ( #58053, #18258, #28147, #23483 ) ) ;
#8799 = AXIS2_PLACEMENT_3D ( 'NONE', #33597, #55036, #1531 ) ;
#8800 = SURFACE_STYLE_FILL_AREA ( #57327 ) ;
#8801 = CARTESIAN_POINT ( 'NONE',  ( -8.102448949553181734, 137.4950000000000045, 5.886773742842747126 ) ) ;
#8802 = ORIENTED_EDGE ( 'NONE', *, *, #15538, .F. ) ;
#8803 = CARTESIAN_POINT ( 'NONE',  ( 3.094860106618435136, 140.4050000000000011, -9.525000000000000355 ) ) ;
#8804 = CARTESIAN_POINT ( 'NONE',  ( -48.50499999999998835, -6.826472737025113702, -4.959722759717900331 ) ) ;
#8805 =( NAMED_UNIT ( * ) SI_UNIT ( $, .STERADIAN. ) SOLID_ANGLE_UNIT ( ) );
#8806 = VERTEX_POINT ( 'NONE', #57029 ) ;
#8807 = CARTESIAN_POINT ( 'NONE',  ( 2.607480562269076430, 116.7929263765337851, -8.025000000000000355 ) ) ;
#8808 = CARTESIAN_POINT ( 'NONE',  ( -52.55707362346618083, -1.166476076187852838E-15, -9.524999999999991473 ) ) ;
#8809 = UNCERTAINTY_MEASURE_WITH_UNIT (LENGTH_MEASURE( 1.000000000000000082E-05 ), #68078, 'distance_accuracy_value', 'NONE');
#8810 = DIRECTION ( 'NONE',  ( 0.000000000000000000, -0.000000000000000000, 1.000000000000000000 ) ) ;
#8811 = SURFACE_STYLE_USAGE ( .BOTH. , #24617 ) ;
#8812 = ORIENTED_EDGE ( 'NONE', *, *, #18916, .F. ) ;
#8813 = EDGE_CURVE ( 'NONE', #40233, #47726, #8847, .T. ) ;
#8814 = CARTESIAN_POINT ( 'NONE',  ( 28.00000000000002132, 34.36176364315826248, 80.00402776293826435 ) ) ;
#8815 = ORIENTED_EDGE ( 'NONE', *, *, #8007, .F. ) ;
#8816 = DIRECTION ( 'NONE',  ( 0.000000000000000000, 0.000000000000000000, 1.000000000000000000 ) ) ;
#8817 = CARTESIAN_POINT ( 'NONE',  ( -44.50000000000000000, 10.49999999999998579, 3.000000000000000000 ) ) ;
#8818 = CARTESIAN_POINT ( 'NONE',  ( 30.75000000000001066, 16.24999999999997513, 4.000000000000000000 ) ) ;
#8819 = CARTESIAN_POINT ( 'NONE',  ( -150.0550000000000068, -9.827790563157499189E-16, -8.024999999999991473 ) ) ;
#8820 = ORIENTED_EDGE ( 'NONE', *, *, #28203, .T. ) ;
#8821 = B_SPLINE_CURVE_WITH_KNOTS ( 'NONE', 3,
 ( #4822, #47813, #42505, #37236, #25243, #58642, #10469, #46399 ),
 .UNSPECIFIED., .F., .F.,
 ( 4, 2, 2, 4 ),
 ( 2.544313220888523934E-07, 0.002693395767724531854, 0.004039966435925753697, 0.005386537104126975541 ),
 .UNSPECIFIED. ) ;
#8822 = CARTESIAN_POINT ( 'NONE',  ( 3.081487911019577365E-31, -7.500000000000000888, 0.000000000000000000 ) ) ;
#8823 = UNCERTAINTY_MEASURE_WITH_UNIT (LENGTH_MEASURE( 1.000000000000000082E-05 ), #25529, 'distance_accuracy_value', 'NONE');
#8824 = EDGE_CURVE ( 'NONE', #9835, #68674, #13058, .T. ) ;
#8825 = EDGE_CURVE ( 'NONE', #36852, #41467, #13353, .T. ) ;
#8826 = CARTESIAN_POINT ( 'NONE',  ( -9.827790563157511022E-16, 152.5570736234661524, 8.025000000000000355 ) ) ;
#8827 = CARTESIAN_POINT ( 'NONE',  ( 75.00000000000000000, 19.99999999996226663, 6.081205180447340375 ) ) ;
#8828 = DIRECTION ( 'NONE',  ( 0.000000000000000000, 0.000000000000000000, 1.000000000000000000 ) ) ;
#8829 = ORIENTED_EDGE ( 'NONE', *, *, #35683, .F. ) ;
#8830 = DIRECTION ( 'NONE',  ( -1.156482317317873451E-16, -1.000000000000000000, 0.000000000000000000 ) ) ;
#8831 = EDGE_CURVE ( 'NONE', #33741, #23152, #62831, .T. ) ;
#8832 = EDGE_LOOP ( 'NONE', ( #61920, #6710, #31880, #24021 ) ) ;
#8833 = AXIS2_PLACEMENT_3D ( 'NONE', #38472, #12027, #33483 ) ;
#8834 = CARTESIAN_POINT ( 'NONE',  ( -75.20499999999995566, -2.607480562269071545, -8.024999999999991473 ) ) ;
#8835 = ORIENTED_EDGE ( 'NONE', *, *, #49042, .F. ) ;
#8836 = EDGE_CURVE ( 'NONE', #35776, #18929, #7452, .T. ) ;
#8837 =( LENGTH_UNIT ( ) NAMED_UNIT ( * ) SI_UNIT ( .MILLI., .METRE. ) );
#8838 = EDGE_CURVE ( 'NONE', #20367, #19782, #68111, .T. ) ;
#8839 = TOROIDAL_SURFACE ( 'NONE', #33532, 27.49999999999999645, 0.5000000000000000000 ) ;
#8840 = EDGE_CURVE ( 'NONE', #14317, #13056, #47318, .T. ) ;
#8841 = DIRECTION ( 'NONE',  ( 0.000000000000000000, 0.000000000000000000, -1.000000000000000000 ) ) ;
#8842 = PLANE ( 'NONE',  #66808 ) ;
#8843 = AXIS2_PLACEMENT_3D ( 'NONE', #22397, #5491, #64263 ) ;
#8844 = ORIENTED_EDGE ( 'NONE', *, *, #21544, .F. ) ;
#8845 = EDGE_CURVE ( 'NONE', #21355, #38142, #55742, .T. ) ;
#8846 = CARTESIAN_POINT ( 'NONE',  ( -75.00000000000000000, 9.701644063436951626, -6.099264075924416773 ) ) ;
#8847 = LINE ( 'NONE', #7409, #16460 ) ;
#8848 = PRESENTATION_STYLE_ASSIGNMENT (( #57030 ) ) ;
#8849 = PRESENTATION_LAYER_ASSIGNMENT (  '', '', ( #67288 ) ) ;
#8850 = DIRECTION ( 'NONE',  ( -0.000000000000000000, -0.000000000000000000, -1.000000000000000000 ) ) ;
#8851 = AXIS2_PLACEMENT_3D ( 'NONE', #65235, #65584, #29690 ) ;
#8852 = CARTESIAN_POINT ( 'NONE',  ( -8.102448949553181734, 139.8950000000000102, -5.886773742842749790 ) ) ;
#8853 = CARTESIAN_POINT ( 'NONE',  ( -98.84499999999998465, -7.632228543268599452, 2.479861379858951054 ) ) ;
#8854 = DIRECTION ( 'NONE',  ( 0.000000000000000000, -1.712231188808094676E-15, -1.000000000000000000 ) ) ;
#8855 = UNCERTAINTY_MEASURE_WITH_UNIT (LENGTH_MEASURE( 1.000000000000000082E-05 ), #29747, 'distance_accuracy_value', 'NONE');
#8856 = CARTESIAN_POINT ( 'NONE',  ( -8.437984349512095861, 144.6929263765337623, -5.166775262442723748E-16 ) ) ;
#8857 = ORIENTED_EDGE ( 'NONE', *, *, #53226, .T. ) ;
#8858 = CARTESIAN_POINT ( 'NONE',  ( -141.2929263765338419, 3.094860106618428031, -9.524999999999993250 ) ) ;
#8859 = FILL_AREA_STYLE ('',( #7219 ) ) ;
#8860 = CARTESIAN_POINT ( 'NONE',  ( -152.5449999999999875, -7.632228543268600340, -2.479861379858950166 ) ) ;
#8861 = MECHANICAL_DESIGN_GEOMETRIC_PRESENTATION_REPRESENTATION (  '', ( #69505 ), #62761 ) ;
#8862 = CARTESIAN_POINT ( 'NONE',  ( 98.00000000000000000, 0.000000000000000000, 5.000000000000004441 ) ) ;
#8863 = DIRECTION ( 'NONE',  ( -0.000000000000000000, -1.000000000000000000, 0.000000000000000000 ) ) ;
#8864 = VERTEX_POINT ( 'NONE', #56265 ) ;
#8865 = CARTESIAN_POINT ( 'NONE',  ( -6.826472737025120807, 127.5070736234661695, -4.959722759717907437 ) ) ;
#8866 = ORIENTED_EDGE ( 'NONE', *, *, #32461, .T. ) ;
#8867 = DIRECTION ( 'NONE',  ( 1.156482317317873451E-16, 1.000000000000000000, -0.000000000000000000 ) ) ;
#8868 = EDGE_CURVE ( 'NONE', #10730, #47241, #66490, .T. ) ;
#8869 = AXIS2_PLACEMENT_3D ( 'NONE', #36914, #10836, #63265 ) ;
#8870 = CARTESIAN_POINT ( 'NONE',  ( 48.49999999999999289, 24.99999999999998579, 4.000000000000000000 ) ) ;
#8871 = CARTESIAN_POINT ( 'NONE',  ( 44.48136104367662114, 9.999999999999978684, 3.378068172219622856 ) ) ;
#8872 = PRESENTATION_LAYER_ASSIGNMENT (  '', '', ( #61662 ) ) ;
#8873 = ORIENTED_EDGE ( 'NONE', *, *, #49992, .F. ) ;
#8874 = CARTESIAN_POINT ( 'NONE',  ( -162.3549999999999898, -4.716976649647093289, -6.492361379858945902 ) ) ;
#8875 = VERTEX_POINT ( 'NONE', #29538 ) ;
#8876 = DIRECTION ( 'NONE',  ( 1.000000000000000000, 0.000000000000000000, 0.000000000000000000 ) ) ;
#8877 = CARTESIAN_POINT ( 'NONE',  ( -5.196152422706636465, 2.500000000000000000, -9.000000000000003553 ) ) ;
#8878 = ORIENTED_EDGE ( 'NONE', *, *, #37858, .F. ) ;
#8879 = FILL_AREA_STYLE ('',( #40570 ) ) ;
#8880 = PRESENTATION_STYLE_ASSIGNMENT (( #29982 ) ) ;
#8881 = CARTESIAN_POINT ( 'NONE',  ( 10.01517768586949231, 111.6949999999999932, 1.839758294383810543E-15 ) ) ;
#8882 = EDGE_LOOP ( 'NONE', ( #64853, #34799, #63560, #769 ) ) ;
#8883 = CARTESIAN_POINT ( 'NONE',  ( -58.04292637653379927, -9.058813317711329915, -2.943386871421370898 ) ) ;
#8884 = CARTESIAN_POINT ( 'NONE',  ( 9.058813317711337021, 112.6549999999999869, 2.943386871421375783 ) ) ;
#8885 = CARTESIAN_POINT ( 'NONE',  ( -73.25499999999998124, -4.716976649647092401, 6.492361379858946790 ) ) ;
#8886 = CARTESIAN_POINT ( 'NONE',  ( -79.55707362346616662, -1.166476076187852838E-15, -9.524999999999991473 ) ) ;
#8887 =( BOUNDED_CURVE ( )  B_SPLINE_CURVE ( 2, ( #32948, #38259, #27969, #33968, #65640, #60352, #43884, #516, #55429, #38611, #59296 ),
 .UNSPECIFIED., .F., .F. ) 
 B_SPLINE_CURVE_WITH_KNOTS ( ( 3, 2, 2, 2, 2, 3 ),
 ( 0.7352941176470590978, 0.7411764705882355475, 0.7470588235294121082, 0.7529411764705885579, 0.7588235294117651186, 0.7647058823529415683 ),
 .UNSPECIFIED. ) 
 CURVE ( )  GEOMETRIC_REPRESENTATION_ITEM ( )  RATIONAL_B_SPLINE_CURVE ( ( 0.9999999999999981126, 0.9510565162951554186, 1.000000000000000000, 0.9510565162951535312, 1.000000000000000000, 0.9510565162951535312, 1.000000000000000000, 0.9510565162951535312, 1.000000000000000000, 0.9510565162951498674, 1.000000000000003775 ) ) 
 REPRESENTATION_ITEM ( '' )  );
#8888 = ORIENTED_EDGE ( 'NONE', *, *, #40004, .T. ) ;
#8889 = CARTESIAN_POINT ( 'NONE',  ( -9.058813317711337021, 138.1550000000000011, -2.943386871421374895 ) ) ;
#8890 = UNCERTAINTY_MEASURE_WITH_UNIT (LENGTH_MEASURE( 1.000000000000000082E-05 ), #64027, 'distance_accuracy_value', 'NONE');
#8891 = FILL_AREA_STYLE ('',( #20118 ) ) ;
#8892 = AXIS2_PLACEMENT_3D ( 'NONE', #66550, #13414, #46168 ) ;
#8893 = FILL_AREA_STYLE ('',( #15252 ) ) ;
#8894 = CARTESIAN_POINT ( 'NONE',  ( 19.89974874213239886, 115.4999999999999574, 10.00000000000000000 ) ) ;
#8895 = EDGE_CURVE ( 'NONE', #59074, #32584, #9755, .T. ) ;
#8896 = FACE_OUTER_BOUND ( 'NONE', #54449, .T. ) ;
#8897 = DIRECTION ( 'NONE',  ( 0.000000000000000000, 0.000000000000000000, -1.000000000000000000 ) ) ;
#8898 = ORIENTED_EDGE ( 'NONE', *, *, #12514, .T. ) ;
#8899 = TOROIDAL_SURFACE ( 'NONE', #17884, 0.5000000000000000000, 0.2500000000000000000 ) ;
#8900 = DIRECTION ( 'NONE',  ( -1.000000000000000000, 0.000000000000000000, 0.000000000000000000 ) ) ;
#8901 = LINE ( 'NONE', #58141, #59761 ) ;
#8902 = CARTESIAN_POINT ( 'NONE',  ( -53.54499999999998039, -7.632228543268600340, -2.479861379858950166 ) ) ;
#8903 = VERTEX_POINT ( 'NONE', #51007 ) ;
#8904 = CARTESIAN_POINT ( 'NONE',  ( 3.648904307674076808, 111.0119688737778318, 8.259051035474742619 ) ) ;
#8905 = CIRCLE ( 'NONE', #30212, 7.749999999999993783 ) ;
#8906 = ADVANCED_FACE ( 'NONE', ( #4418 ), #56597, .F. ) ;
#8907 = DIRECTION ( 'NONE',  ( 0.7071067811865426878, 0.000000000000000000, -0.7071067811865524577 ) ) ;
#8908 = CARTESIAN_POINT ( 'NONE',  ( -45.00000000000000000, 7.768687147774684831, -7.000000000000003553 ) ) ;
#8909 = CARTESIAN_POINT ( 'NONE',  ( 10.00000000000002132, 50.00000000000000000, 55.00000000000000711 ) ) ;
#8910 = ORIENTED_EDGE ( 'NONE', *, *, #37585, .F. ) ;
#8911 = CARTESIAN_POINT ( 'NONE',  ( 8.750000000000001776, 24.99999999999998579, -4.000000000000000000 ) ) ;
#8912 = ORIENTED_EDGE ( 'NONE', *, *, #44992, .F. ) ;
#8913 = CIRCLE ( 'NONE', #65075, 0.5000000000000004441 ) ;
#8914 = CARTESIAN_POINT ( 'NONE',  ( -108.9549999999999983, -7.632228543268599452, 2.479861379858951054 ) ) ;
#8915 = EDGE_LOOP ( 'NONE', ( #67991, #22548, #48808, #21997 ) ) ;
#8916 = DIRECTION ( 'NONE',  ( 0.000000000000000000, 0.000000000000000000, -1.000000000000000000 ) ) ;
#8917 = EDGE_CURVE ( 'NONE', #3393, #61550, #26255, .T. ) ;
#8918 = DIRECTION ( 'NONE',  ( 1.000000000000000000, 9.570888143320315888E-16, 0.000000000000000000 ) ) ;
#8919 = CARTESIAN_POINT ( 'NONE',  ( -143.6070736234661354, -8.102448949553172852, 5.886773742842742685 ) ) ;
#8920 = CARTESIAN_POINT ( 'NONE',  ( 3.094860106618435136, 145.2949999999999875, -9.525000000000000355 ) ) ;
#8921 = CARTESIAN_POINT ( 'NONE',  ( -76.85707362346616378, -5.598654528085803328, -7.705886871421366635 ) ) ;
#8922 = VECTOR ( 'NONE', #61000, 1000.000000000000000 ) ;
#8923 = ADVANCED_FACE ( 'NONE', ( #18655 ), #16081, .T. ) ;
#8924 = DIRECTION ( 'NONE',  ( 0.000000000000000000, 0.000000000000000000, 1.000000000000000000 ) ) ;
#8925 = ORIENTED_EDGE ( 'NONE', *, *, #18364, .T. ) ;
#8926 = CARTESIAN_POINT ( 'NONE',  ( -71.99999999999998579, 63.67479433117734544, -7.500000000000000000 ) ) ;
#8927 = CARTESIAN_POINT ( 'NONE',  ( -17.22313415847698082, -11.12901830060570063, 4.490355093446679824 ) ) ;
#8929 = CARTESIAN_POINT ( 'NONE',  ( -6.767634268437465295, 2.367558512213881361, 2.278113600022078078 ) ) ;
#8928 = DIRECTION ( 'NONE',  ( 0.000000000000000000, 1.000000000000000000, 0.000000000000000000 ) ) ;
#8930 = CIRCLE ( 'NONE', #16834, 6.999999999999997335 ) ;
#8931 = CARTESIAN_POINT ( 'NONE',  ( -125.4549999999999841, 7.632228543268599452, -2.479861379858951942 ) ) ;
#8932 = FILL_AREA_STYLE_COLOUR ( '', #24650 ) ;
#8933 = CARTESIAN_POINT ( 'NONE',  ( -10.01517768586949231, 110.1949999999999648, -6.132527647946036459E-16 ) ) ;
#8934 = CARTESIAN_POINT ( 'NONE',  ( -121.3449999999999989, 7.632228543268599452, -2.479861379858951942 ) ) ;
#8935 = CIRCLE ( 'NONE', #48278, 1.000000000000000888 ) ;
#8936 = VECTOR ( 'NONE', #69131, 1000.000000000000000 ) ;
#8937 = CARTESIAN_POINT ( 'NONE',  ( -122.8449999999999847, -7.632228543268599452, 2.479861379858951054 ) ) ;
#8938 = AXIS2_PLACEMENT_3D ( 'NONE', #52245, #15316, #14238 ) ;
#8939 = ORIENTED_EDGE ( 'NONE', *, *, #1471, .T. ) ;
#8940 = MECHANICAL_DESIGN_GEOMETRIC_PRESENTATION_REPRESENTATION (  '', ( #11181 ), #25741 ) ;
#8941 = DIRECTION ( 'NONE',  ( -1.189524669241239115E-16, -1.000000000000000000, -0.000000000000000000 ) ) ;
#8942 = AXIS2_PLACEMENT_3D ( 'NONE', #37125, #55, #58189 ) ;
#8943 = FACE_OUTER_BOUND ( 'NONE', #35083, .T. ) ;
#8944 = CIRCLE ( 'NONE', #26873, 24.00000000000001421 ) ;
#8945 = CARTESIAN_POINT ( 'NONE',  ( -172.3429263765338249, -9.058813317711329915, 2.943386871421371787 ) ) ;
#8946 = SURFACE_STYLE_USAGE ( .BOTH. , #30040 ) ;
#8947 = CARTESIAN_POINT ( 'NONE',  ( -181.9449999999999932, -9.827790563157499189E-16, -8.024999999999991473 ) ) ;
#8948 = AXIS2_PLACEMENT_3D ( 'NONE', #43265, #10167, #31603 ) ;
#8949 = CARTESIAN_POINT ( 'NONE',  ( -45.00000000000000000, 9.708372675170618749, -3.611004237778681514 ) ) ;
#8950 = AXIS2_PLACEMENT_3D ( 'NONE', #43344, #32359, #47219 ) ;
#8951 = DIRECTION ( 'NONE',  ( -1.000000000000000000, 0.000000000000000000, 0.000000000000000000 ) ) ;
#8952 = CARTESIAN_POINT ( 'NONE',  ( 6.413663052920311358, 2.891209729714700138, -4.192813088908785199E-16 ) ) ;
#8953 = ORIENTED_EDGE ( 'NONE', *, *, #22185, .F. ) ;
#8954 = CARTESIAN_POINT ( 'NONE',  ( -82.94292637653380496, 0.000000000000000000, 9.524999999999991473 ) ) ;
#8955 = COLOUR_RGB ( '', 0.31764706, 0.68627451, 0.89019608) ;
#8956 = SURFACE_STYLE_FILL_AREA ( #67012 ) ;
#8957 = PRESENTATION_STYLE_ASSIGNMENT (( #24759 ) ) ;
#8958 = EDGE_CURVE ( 'NONE', #9871, #69641, #43147, .T. ) ;
#8959 = DIRECTION ( 'NONE',  ( -0.000000000000000000, -1.000000000000000000, -0.000000000000000000 ) ) ;
#8960 = DIRECTION ( 'NONE',  ( 0.000000000000000000, 1.000000000000000000, 0.000000000000000000 ) ) ;
#8961 = LINE ( 'NONE', #13887, #59473 ) ;
#8962 = EDGE_CURVE ( 'NONE', #26613, #36186, #37567, .T. ) ;
#8963 = LINE ( 'NONE', #40647, #35038 ) ;
#8964 = ORIENTED_EDGE ( 'NONE', *, *, #2997, .T. ) ;
#8965 = LINE ( 'NONE', #14241, #51609 ) ;
#8966 = DIRECTION ( 'NONE',  ( 1.000000000000000000, 0.000000000000000000, 0.000000000000000000 ) ) ;
#8967 = ORIENTED_EDGE ( 'NONE', *, *, #15768, .T. ) ;
#8968 = CARTESIAN_POINT ( 'NONE',  ( -184.0000000000000000, 0.000000000000000000, 0.000000000000000000 ) ) ;
#8969 = COLOUR_RGB ( '', 0.31764706, 0.68627451, 0.89019608) ;
#8970 = SPHERICAL_SURFACE ( 'NONE', #6109, 0.5000000000000000000 ) ;
#8971 = CARTESIAN_POINT ( 'NONE',  ( -2.607480562269073765, 130.2070736234661581, -8.025000000000000355 ) ) ;
#8972 = SURFACE_STYLE_FILL_AREA ( #35710 ) ;
#8973 = ORIENTED_EDGE ( 'NONE', *, *, #36353, .F. ) ;
#8974 = AXIS2_PLACEMENT_3D ( 'NONE', #68644, #63356, #61957 ) ;
#8975 = CARTESIAN_POINT ( 'NONE',  ( -103.4049999999999869, -2.607480562269069768, 8.024999999999991473 ) ) ;
#8976 = DIRECTION ( 'NONE',  ( 0.000000000000000000, 1.000000000000000000, 0.000000000000000000 ) ) ;
#8977 = EDGE_LOOP ( 'NONE', ( #38173, #64914, #27062, #23867 ) ) ;
#8978 = DIRECTION ( 'NONE',  ( -0.000000000000000000, 1.000000000000000000, -0.000000000000000000 ) ) ;
#8979 = EDGE_CURVE ( 'NONE', #60124, #56915, #37525, .T. ) ;
#8980 = CARTESIAN_POINT ( 'NONE',  ( -104.4570736234661723, -9.058813317711329915, 2.943386871421371787 ) ) ;
#8981 = EDGE_CURVE ( 'NONE', #69362, #44405, #31829, .T. ) ;
#8982 = CARTESIAN_POINT ( 'NONE',  ( 0.000000000000000000, -9.000000000000007105, 0.000000000000000000 ) ) ;
#8983 = AXIS2_PLACEMENT_3D ( 'NONE', #34805, #67517, #56259 ) ;
#8984 = AXIS2_PLACEMENT_3D ( 'NONE', #5640, #17297, #33434 ) ;
#8985 = ORIENTED_EDGE ( 'NONE', *, *, #58452, .T. ) ;
#8986 = DIRECTION ( 'NONE',  ( 0.000000000000000000, 0.000000000000000000, 1.000000000000000000 ) ) ;
#8987 = CARTESIAN_POINT ( 'NONE',  ( -82.64499999999998181, 4.716976649647091513, -6.492361379858946790 ) ) ;
#8989 = ORIENTED_EDGE ( 'NONE', *, *, #34142, .F. ) ;
#8988 = AXIS2_PLACEMENT_3D ( 'NONE', #36699, #56723, #8542 ) ;
#8990 = EDGE_CURVE ( 'NONE', #19860, #40912, #22900, .T. ) ;
#8991 = CARTESIAN_POINT ( 'NONE',  ( -34.23488332747668750, -9.007918291183415249, 5.430249810268243493 ) ) ;
#8992 = COLOUR_RGB ( '', 0.40784314, 0.44705882, 0.49803922) ;
#8993 = ORIENTED_EDGE ( 'NONE', *, *, #67361, .F. ) ;
#8994 = DIRECTION ( 'NONE',  ( 1.000000000000000000, -0.000000000000000000, 0.000000000000000000 ) ) ;
#8995 =( NAMED_UNIT ( * ) PLANE_ANGLE_UNIT ( ) SI_UNIT ( $, .RADIAN. ) );
#8996 = PRESENTATION_LAYER_ASSIGNMENT (  '', '', ( #65163 ) ) ;
#8997 = ADVANCED_FACE ( 'NONE', ( #63873 ), #53351, .F. ) ;
#8998 = DIRECTION ( 'NONE',  ( 1.000000000000000000, 0.000000000000000000, 0.000000000000000000 ) ) ;
#8999 = DIRECTION ( 'NONE',  ( 1.000000000000000000, 0.000000000000000000, 3.469446951953610639E-15 ) ) ;
#9000 = ORIENTED_EDGE ( 'NONE', *, *, #43442, .T. ) ;
#9001 =( NAMED_UNIT ( * ) PLANE_ANGLE_UNIT ( ) SI_UNIT ( $, .RADIAN. ) );
#9002 = ORIENTED_EDGE ( 'NONE', *, *, #6076, .T. ) ;
#9003 = EDGE_CURVE ( 'NONE', #35982, #21029, #49828, .T. ) ;
#9004 = PRESENTATION_STYLE_ASSIGNMENT (( #4041 ) ) ;
#9005 = LINE ( 'NONE', #68801, #42071 ) ;
#9006 = DIRECTION ( 'NONE',  ( 0.000000000000000000, 0.000000000000000000, 1.000000000000000000 ) ) ;
#9007 = CARTESIAN_POINT ( 'NONE',  ( -169.2570736234661695, 5.598654528085800663, -7.705886871421367523 ) ) ;
#9008 = CARTESIAN_POINT ( 'NONE',  ( 5.598654528085805993, 114.2449999999999903, 7.705886871421374629 ) ) ;
#9009 = CARTESIAN_POINT ( 'NONE',  ( -104.6070736234661922, -8.102448949553172852, 5.886773742842742685 ) ) ;
#9010 = CARTESIAN_POINT ( 'NONE',  ( 8.000000000000000000, 33.99999999999998579, 3.750000000000000000 ) ) ;
#9011 = ADVANCED_FACE ( 'NONE', ( #22027 ), #21667, .F. ) ;
#9012 = DIRECTION ( 'NONE',  ( 0.000000000000000000, 1.000000000000000000, 0.000000000000000000 ) ) ;
#9013 = ORIENTED_EDGE ( 'NONE', *, *, #17969, .F. ) ;
#9014 = DIRECTION ( 'NONE',  ( 0.000000000000000000, 0.000000000000000000, -1.000000000000000000 ) ) ;
#9015 = CARTESIAN_POINT ( 'NONE',  ( -81.59292637653378222, -3.094860106618431139, -9.524999999999991473 ) ) ;
#9016 = CARTESIAN_POINT ( 'NONE',  ( 48.25000000000000000, 21.74999999999998579, -4.000000000000000000 ) ) ;
#9017 =( NAMED_UNIT ( * ) SI_UNIT ( $, .STERADIAN. ) SOLID_ANGLE_UNIT ( ) );
#9018 = CARTESIAN_POINT ( 'NONE',  ( -150.9550000000000125, -7.632228543268599452, 2.479861379858951054 ) ) ;
#9019 = CARTESIAN_POINT ( 'NONE',  ( -6.611298881745738321, 111.1103466397262025, -5.993574246798706540 ) ) ;
#9020 = CARTESIAN_POINT ( 'NONE',  ( -151.6450000000000102, 4.716976649647091513, -6.492361379858946790 ) ) ;
#9021 = CARTESIAN_POINT ( 'NONE',  ( -143.3949999999999818, -6.826472737025113702, -4.959722759717900331 ) ) ;
#9022 = AXIS2_PLACEMENT_3D ( 'NONE', #46414, #56576, #35124 ) ;
#9023 = ORIENTED_EDGE ( 'NONE', *, *, #52605, .F. ) ;
#9024 =( BOUNDED_CURVE ( )  B_SPLINE_CURVE ( 2, ( #8588, #51849, #42028, #45886, #19820, #19468, #25784, #36401, #47296, #3972, #68724 ),
 .UNSPECIFIED., .F., .F. ) 
 B_SPLINE_CURVE_WITH_KNOTS ( ( 3, 2, 2, 2, 2, 3 ),
 ( 0.6630434782608538580, 0.6652173913043321063, 0.6673913043478103546, 0.6695652173912884919, 0.6717391304347667402, 0.6739130434782448775 ),
 .UNSPECIFIED. ) 
 CURVE ( )  GEOMETRIC_REPRESENTATION_ITEM ( )  RATIONAL_B_SPLINE_CURVE ( ( 1.000000000000352385, 0.9510565162948011464, 1.000000000000000000, 0.9510565162951535312, 1.000000000000000000, 0.9510565162951535312, 1.000000000000000000, 0.9510565162951535312, 1.000000000000000000, 0.9510565162955134655, 0.9999999999996400657 ) ) 
 REPRESENTATION_ITEM ( '' )  );
#9025 = CARTESIAN_POINT ( 'NONE',  ( -11.74999999999999645, -3.000000000000000000, 7.000000000000001776 ) ) ;
#9026 = SURFACE_SIDE_STYLE ('',( #9384 ) ) ;
#9027 = AXIS2_PLACEMENT_3D ( 'NONE', #62564, #30905, #46447 ) ;
#9028 = CARTESIAN_POINT ( 'NONE',  ( -1.953228634907021810, 72.00000000000001421, 12.50000000000000000 ) ) ;
#9029 = CARTESIAN_POINT ( 'NONE',  ( -60.35499999999998977, -4.716976649647093289, -6.492361379858945902 ) ) ;
#9030 = CARTESIAN_POINT ( 'NONE',  ( -40.20684803154669851, -11.80180942591514182, 3.296236230148514856 ) ) ;
#9031 = CARTESIAN_POINT ( 'NONE',  ( -167.2429263765338305, 5.598654528085804216, 7.705886871421366635 ) ) ;
#9032 = CARTESIAN_POINT ( 'NONE',  ( -61.34499999999998465, 7.632228543268599452, -2.479861379858951942 ) ) ;
#9033 = CARTESIAN_POINT ( 'NONE',  ( 8.102448949553183510, 161.1049999999999613, -5.886773742842746238 ) ) ;
#9034 = CARTESIAN_POINT ( 'NONE',  ( -143.9070736234666299, -3.094860106610496597, 9.525000000005753975 ) ) ;
#9035 = PRESENTATION_LAYER_ASSIGNMENT (  '', '', ( #14660 ) ) ;
#9036 = FILL_AREA_STYLE ('',( #35065 ) ) ;
#9037 =( GEOMETRIC_REPRESENTATION_CONTEXT ( 3 ) GLOBAL_UNCERTAINTY_ASSIGNED_CONTEXT ( ( #49654 ) ) GLOBAL_UNIT_ASSIGNED_CONTEXT ( ( #46465, #58034, #10528 ) ) REPRESENTATION_CONTEXT ( 'NONE', 'WORKASPACE' ) );
#9038 = DIRECTION ( 'NONE',  ( 1.000000000000000000, 0.000000000000000000, 0.000000000000000000 ) ) ;
#9039 = CARTESIAN_POINT ( 'NONE',  ( 68.99999999999998579, 8.450062914116736267E-15, -3.000000000000000000 ) ) ;
#9040 = EDGE_CURVE ( 'NONE', #68346, #39893, #43187, .T. ) ;
#9041 = VECTOR ( 'NONE', #36511, 1000.000000000000000 ) ;
#9042 = CARTESIAN_POINT ( 'NONE',  ( -2.879676287999554329, 110.7340786399931005, 8.840802594141578652 ) ) ;
#9043 = CARTESIAN_POINT ( 'NONE',  ( 8.000000000000000000, 33.74999999999998579, 4.000000000000000000 ) ) ;
#9044 = VECTOR ( 'NONE', #66664, 1000.000000000000000 ) ;
#9045 = MECHANICAL_DESIGN_GEOMETRIC_PRESENTATION_REPRESENTATION (  '', ( #57347 ), #15795 ) ;
#9046 =( NAMED_UNIT ( * ) SI_UNIT ( $, .STERADIAN. ) SOLID_ANGLE_UNIT ( ) );
#9047 = DIRECTION ( 'NONE',  ( -1.000000000000000000, 0.000000000000000000, 0.000000000000000000 ) ) ;
#9048 = ORIENTED_EDGE ( 'NONE', *, *, #40198, .T. ) ;
#9049 = AXIS2_PLACEMENT_3D ( 'NONE', #562, #44282, #23810 ) ;
#9050 = ORIENTED_EDGE ( 'NONE', *, *, #35592, .F. ) ;
#9051 = DIRECTION ( 'NONE',  ( -2.312964634635740689E-15, 1.000000000000000000, -0.000000000000000000 ) ) ;
#9052 = AXIS2_PLACEMENT_3D ( 'NONE', #37558, #69173, #43852 ) ;
#9053 = ADVANCED_FACE ( 'NONE', ( #54364 ), #49133, .F. ) ;
#9054 = SURFACE_STYLE_FILL_AREA ( #10446 ) ;
#9055 = CIRCLE ( 'NONE', #61788, 1.000000000000000000 ) ;
#9057 = ADVANCED_FACE ( 'NONE', ( #55764 ), #45244, .F. ) ;
#9056 = CARTESIAN_POINT ( 'NONE',  ( -78.05707362346616662, 0.000000000000000000, 9.524999999999991473 ) ) ;
#9058 = VERTEX_POINT ( 'NONE', #29358 ) ;
#9059 = ORIENTED_EDGE ( 'NONE', *, *, #9603, .T. ) ;
#9060 =( NAMED_UNIT ( * ) SI_UNIT ( $, .STERADIAN. ) SOLID_ANGLE_UNIT ( ) );
#9061 = SURFACE_STYLE_FILL_AREA ( #56181 ) ;
#9062 = EDGE_CURVE ( 'NONE', #23486, #60366, #17467, .T. ) ;
#9063 = ORIENTED_EDGE ( 'NONE', *, *, #62794, .F. ) ;
#9064 = EDGE_CURVE ( 'NONE', #47623, #62580, #66669, .T. ) ;
#9065 = CARTESIAN_POINT ( 'NONE',  ( 5.598654528085809545, 119.2549999999999812, -7.705886871421373741 ) ) ;
#9066 = CARTESIAN_POINT ( 'NONE',  ( 0.000000000000000000, 149.9999999999999716, 16.00000000000000000 ) ) ;
#9067 = ORIENTED_EDGE ( 'NONE', *, *, #12306, .T. ) ;
#9068 = ADVANCED_FACE ( 'NONE', ( #38596 ), #66307, .F. ) ;
#9069 = STYLED_ITEM ( 'NONE', ( #43262 ), #59678 ) ;
#9070 = DIRECTION ( 'NONE',  ( 1.000000000000000000, 0.000000000000000000, 0.000000000000000000 ) ) ;
#9071 = CARTESIAN_POINT ( 'NONE',  ( -113.0949999999999989, -2.607480562269071545, -8.024999999999991473 ) ) ;
#9072 = VERTEX_POINT ( 'NONE', #49458 ) ;
#9073 = DIRECTION ( 'NONE',  ( -0.000000000000000000, -0.000000000000000000, -1.000000000000000000 ) ) ;
#9074 = CARTESIAN_POINT ( 'NONE',  ( -165.0570736234661524, 0.000000000000000000, 9.524999999999991473 ) ) ;
#9075 = STYLED_ITEM ( 'NONE', ( #10621 ), #45224 ) ;
#9076 = STYLED_ITEM ( 'NONE', ( #8848 ), #12013 ) ;
#9077 = CARTESIAN_POINT ( 'NONE',  ( -179.4570736234661865, -9.058813317711329915, 2.943386871421371787 ) ) ;
#9078 = EDGE_LOOP ( 'NONE', ( #33049, #59682, #17408, #7260, #19323, #4634, #8133 ) ) ;
#9079 = CARTESIAN_POINT ( 'NONE',  ( 6.826472737025119919, 148.8929263765338078, 4.959722759717908325 ) ) ;
#9080 = DIRECTION ( 'NONE',  ( 1.000000000000000000, 0.000000000000000000, 0.000000000000000000 ) ) ;
#9081 = EDGE_CURVE ( 'NONE', #17236, #30128, #11653, .T. ) ;
#9082 = DIRECTION ( 'NONE',  ( 0.000000000000000000, -2.430666987507993885E-16, 1.000000000000000000 ) ) ;
#9083 = ORIENTED_EDGE ( 'NONE', *, *, #2507, .T. ) ;
#9084 = AXIS2_PLACEMENT_3D ( 'NONE', #5381, #53271, #5058 ) ;
#9085 = PRESENTATION_STYLE_ASSIGNMENT (( #57252 ) ) ;
#9086 = ORIENTED_EDGE ( 'NONE', *, *, #39046, .T. ) ;
#9087 = FILL_AREA_STYLE_COLOUR ( '', #23747 ) ;
#9088 = CARTESIAN_POINT ( 'NONE',  ( -45.90208486430518064, 9.410172310978721200, 3.203880287027108142 ) ) ;
#9089 = CARTESIAN_POINT ( 'NONE',  ( -140.6929263765337907, 10.01517768586948698, -1.839758294383808966E-15 ) ) ;
#9090 = CARTESIAN_POINT ( 'NONE',  ( -158.4570736234661581, -9.058813317711329915, 2.943386871421371787 ) ) ;
#9091 = CARTESIAN_POINT ( 'NONE',  ( -128.0049999999999670, 6.826472737025116366, 4.959722759717898555 ) ) ;
#9092 = CARTESIAN_POINT ( 'NONE',  ( -184.0000000000000568, -3.735988484587566827, 7.112865090842599436 ) ) ;
#9093 = COLOUR_RGB ( '', 0.08235294, 0.09019608, 0.10196078) ;
#9094 = DIRECTION ( 'NONE',  ( -0.000000000000000000, -0.000000000000000000, -1.000000000000000000 ) ) ;
#9095 = CARTESIAN_POINT ( 'NONE',  ( -72.00000000000000000, 35.92875272052971525, -7.500000000000000000 ) ) ;
#9096 =( GEOMETRIC_REPRESENTATION_CONTEXT ( 3 ) GLOBAL_UNCERTAINTY_ASSIGNED_CONTEXT ( ( #67245 ) ) GLOBAL_UNIT_ASSIGNED_CONTEXT ( ( #26996, #7993, #1266 ) ) REPRESENTATION_CONTEXT ( 'NONE', 'WORKASPACE' ) );
#9097 = CARTESIAN_POINT ( 'NONE',  ( -74.61075306680825747, 36.39434226735735223, 9.999999999999996447 ) ) ;
#9098 = ORIENTED_EDGE ( 'NONE', *, *, #66262, .F. ) ;
#9099 = PRESENTATION_LAYER_ASSIGNMENT (  '', '', ( #63009 ) ) ;
#9100 = ORIENTED_EDGE ( 'NONE', *, *, #37357, .F. ) ;
#9101 = DIRECTION ( 'NONE',  ( -1.000000000000000000, 0.000000000000000000, 0.000000000000000000 ) ) ;
#9102 = SURFACE_SIDE_STYLE ('',( #41135 ) ) ;
#9103 = LINE ( 'NONE', #40427, #9866 ) ;
#9104 = CARTESIAN_POINT ( 'NONE',  ( 7.632228543268608334, 114.4570736234661581, -2.479861379858951942 ) ) ;
#9105 = ORIENTED_EDGE ( 'NONE', *, *, #6051, .T. ) ;
#9106 = CARTESIAN_POINT ( 'NONE',  ( -183.0550000000000068, -9.827790563157499189E-16, -8.024999999999991473 ) ) ;
#9107 = DIRECTION ( 'NONE',  ( -1.000000000000000000, -0.000000000000000000, -0.000000000000000000 ) ) ;
#9108 = EDGE_CURVE ( 'NONE', #46872, #60023, #15051, .T. ) ;
#9109 = CONICAL_SURFACE ( 'NONE', #64124, 3.100000000000005418, 0.7853981633974445042 ) ;
#9110 = CARTESIAN_POINT ( 'NONE',  ( -47.90707362346616094, -3.094860106618429807, 9.524999999999991473 ) ) ;
#9111 = CARTESIAN_POINT ( 'NONE',  ( -178.3449999999999989, 7.632228543268599452, -2.479861379858951942 ) ) ;
#9112 = EDGE_CURVE ( 'NONE', #60430, #48506, #20645, .T. ) ;
#9113 = CARTESIAN_POINT ( 'NONE',  ( -18.25000000000000711, 31.24999999999999289, 3.750000000000000000 ) ) ;
#9114 = AXIS2_PLACEMENT_3D ( 'NONE', #67781, #51957, #45669 ) ;
#9115 = ORIENTED_EDGE ( 'NONE', *, *, #35707, .T. ) ;
#9116 = VECTOR ( 'NONE', #31916, 1000.000000000000000 ) ;
#9117 = FILL_AREA_STYLE_COLOUR ( '', #56055 ) ;
#9118 = CARTESIAN_POINT ( 'NONE',  ( -88.10499999999998977, -6.826472737025115478, 4.959722759717900331 ) ) ;
#9119 = DIRECTION ( 'NONE',  ( 0.000000000000000000, 0.000000000000000000, 1.000000000000000000 ) ) ;
#9120 = CARTESIAN_POINT ( 'NONE',  ( -169.5570736234661808, -1.166476076187852838E-15, -9.524999999999991473 ) ) ;
#9121 = FACE_OUTER_BOUND ( 'NONE', #54914, .T. ) ;
#9122 = CARTESIAN_POINT ( 'NONE',  ( -86.84499999999998465, -7.632228543268599452, 2.479861379858951054 ) ) ;
#9123 = CARTESIAN_POINT ( 'NONE',  ( -9.058813317711337021, 132.1550000000000011, -2.943386871421374895 ) ) ;
#9124 = CARTESIAN_POINT ( 'NONE',  ( -67.49499999999999034, 6.826472737025113702, -4.959722759717902107 ) ) ;
#9125 = LINE ( 'NONE', #41491, #7278 ) ;
#9126 = DIRECTION ( 'NONE',  ( 0.000000000000000000, 0.000000000000000000, 1.000000000000000000 ) ) ;
#9127 = AXIS2_PLACEMENT_3D ( 'NONE', #41686, #10346, #8354 ) ;
#9128 = DIRECTION ( 'NONE',  ( 0.000000000000000000, 0.000000000000000000, -1.000000000000000000 ) ) ;
#9129 = PRESENTATION_STYLE_ASSIGNMENT (( #20356 ) ) ;
#9131 = ORIENTED_EDGE ( 'NONE', *, *, #4618, .F. ) ;
#9130 = CIRCLE ( 'NONE', #21469, 1.000000000000000000 ) ;
#9132 = CARTESIAN_POINT ( 'NONE',  ( -101.3929263765337794, 8.102448949553176405, 5.886773742842740909 ) ) ;
#9133 = PRODUCT ( '4. Adjustment Screw', '4. Adjustment Screw', '', ( #1535 ) ) ;
#9134 = CARTESIAN_POINT ( 'NONE',  ( -125.5449999999999875, -7.632228543268600340, -2.479861379858950166 ) ) ;
#9135 = FILL_AREA_STYLE_COLOUR ( '', #44883 ) ;
#9136 = AXIS2_PLACEMENT_3D ( 'NONE', #52047, #41161, #46810 ) ;
#9137 = DIRECTION ( 'NONE',  ( 0.000000000000000000, -1.000000000000000000, 0.000000000000000000 ) ) ;
#9138 = EDGE_CURVE ( 'NONE', #32880, #13067, #36887, .T. ) ;
#9139 = CIRCLE ( 'NONE', #28171, 2.000000000000001776 ) ;
#9140 = CARTESIAN_POINT ( 'NONE',  ( -15.98999599679679839, 118.4999999999999716, 7.500000000000000000 ) ) ;
#9141 = CARTESIAN_POINT ( 'NONE',  ( 60.00000000000000000, -2.024042244987997205E-14, -7.500000000000000000 ) ) ;
#9142 = ORIENTED_EDGE ( 'NONE', *, *, #10702, .T. ) ;
#9143 = ORIENTED_EDGE ( 'NONE', *, *, #40417, .T. ) ;
#9144 =( GEOMETRIC_REPRESENTATION_CONTEXT ( 3 ) GLOBAL_UNCERTAINTY_ASSIGNED_CONTEXT ( ( #56657 ) ) GLOBAL_UNIT_ASSIGNED_CONTEXT ( ( #59207, #1812, #17726 ) ) REPRESENTATION_CONTEXT ( 'NONE', 'WORKASPACE' ) );
#9145 = FILL_AREA_STYLE ('',( #19679 ) ) ;
#9146 = CIRCLE ( 'NONE', #24829, 0.5000000000000004441 ) ;
#9147 = ADVANCED_FACE ( 'NONE', ( #61699 ), #25796, .T. ) ;
#9148 = CARTESIAN_POINT ( 'NONE',  ( 21.50000000000001066, 24.74999999999998224, 4.000000000000000000 ) ) ;
#9149 = CARTESIAN_POINT ( 'NONE',  ( -98.30707362346616662, -10.01517768586948698, 6.132527647946031529E-16 ) ) ;
#9150 = STYLED_ITEM ( 'NONE', ( #5927 ), #52916 ) ;
#9151 = DIRECTION ( 'NONE',  ( -0.5000000000000002220, 0.8660254037844385966, 0.000000000000000000 ) ) ;
#9152 = FACE_OUTER_BOUND ( 'NONE', #67030, .T. ) ;
#9153 = ORIENTED_EDGE ( 'NONE', *, *, #3402, .T. ) ;
#9154 = CARTESIAN_POINT ( 'NONE',  ( -124.7049999999999841, 2.607480562269072433, 8.024999999999991473 ) ) ;
#9155 = ORIENTED_EDGE ( 'NONE', *, *, #17893, .T. ) ;
#9156 = DIRECTION ( 'NONE',  ( 0.000000000000000000, 1.000000000000000000, 0.000000000000000000 ) ) ;
#9157 = CARTESIAN_POINT ( 'NONE',  ( -127.7070736234661581, -3.094860106618431139, -9.524999999999991473 ) ) ;
#9158 = EDGE_CURVE ( 'NONE', #26382, #12261, #26872, .T. ) ;
#9159 = ORIENTED_EDGE ( 'NONE', *, *, #26, .T. ) ;
#9160 = DIRECTION ( 'NONE',  ( 1.000000000000000000, -0.000000000000000000, -0.000000000000000000 ) ) ;
#9161 = LINE ( 'NONE', #51717, #29846 ) ;
#9162 = EDGE_LOOP ( 'NONE', ( #13971, #46859, #49685 ) ) ;
#9163 = MECHANICAL_DESIGN_GEOMETRIC_PRESENTATION_REPRESENTATION (  '', ( #60781 ), #9212 ) ;
#9164 =( NAMED_UNIT ( * ) PLANE_ANGLE_UNIT ( ) SI_UNIT ( $, .RADIAN. ) );
#9165 = CARTESIAN_POINT ( 'NONE',  ( 8.102448949553181734, 150.3949999999999818, 5.886773742842750679 ) ) ;
#9166 = VERTEX_POINT ( 'NONE', #24424 ) ;
#9167 = DIRECTION ( 'NONE',  ( -1.000000000000000000, -0.000000000000000000, -0.000000000000000000 ) ) ;
#9168 = CARTESIAN_POINT ( 'NONE',  ( -3.094860106618432471, 146.7049999999999841, -9.525000000000000355 ) ) ;
#9169 = FILL_AREA_STYLE_COLOUR ( '', #27134 ) ;
#9170 = VERTEX_POINT ( 'NONE', #51187 ) ;
#9171 = CARTESIAN_POINT ( 'NONE',  ( -2.607480562269073765, 114.0929263765338106, -8.025000000000000355 ) ) ;
#9172 = CARTESIAN_POINT ( 'NONE',  ( 25.75000000000001066, 19.24999999999997868, -4.000000000000000000 ) ) ;
#9173 = CARTESIAN_POINT ( 'NONE',  ( -5.249999999999991118, 0.000000000000000000, 0.000000000000000000 ) ) ;
#9174 =( GEOMETRIC_REPRESENTATION_CONTEXT ( 3 ) GLOBAL_UNCERTAINTY_ASSIGNED_CONTEXT ( ( #37054 ) ) GLOBAL_UNIT_ASSIGNED_CONTEXT ( ( #10221, #48930, #36985 ) ) REPRESENTATION_CONTEXT ( 'NONE', 'WORKASPACE' ) );
#9175 = CARTESIAN_POINT ( 'NONE',  ( 44.99999999999998579, 119.9999999999999716, 10.00000000000000000 ) ) ;
#9176 = EDGE_CURVE ( 'NONE', #22804, #57008, #30412, .T. ) ;
#9177 = CARTESIAN_POINT ( 'NONE',  ( -15.98999599679679839, 118.4999999999999716, 7.000000000000000000 ) ) ;
#9178 = ORIENTED_EDGE ( 'NONE', *, *, #44645, .F. ) ;
#9179 = CARTESIAN_POINT ( 'NONE',  ( -6.239160159721279797, 3.193457606803199678, 3.307663659028042824E-15 ) ) ;
#9180 = VERTEX_POINT ( 'NONE', #30381 ) ;
#9181 = CARTESIAN_POINT ( 'NONE',  ( -59.24292637653380211, 5.598654528085804216, 7.705886871421366635 ) ) ;
#9182 = DIRECTION ( 'NONE',  ( -0.000000000000000000, -0.000000000000000000, -1.000000000000000000 ) ) ;
#9183 = SURFACE_STYLE_FILL_AREA ( #46862 ) ;
#9185 = CARTESIAN_POINT ( 'NONE',  ( -147.9550000000000125, -7.632228543268599452, 2.479861379858951054 ) ) ;
#9184 = STYLED_ITEM ( 'NONE', ( #42323 ), #60270 ) ;
#9186 = ORIENTED_EDGE ( 'NONE', *, *, #5795, .F. ) ;
#9187 = AXIS2_PLACEMENT_3D ( 'NONE', #59923, #11739, #54646 ) ;
#9188 = CARTESIAN_POINT ( 'NONE',  ( -45.00000000000000000, -2.024041941016019177E-14, -6.999999999999999112 ) ) ;
#9189 = FACE_OUTER_BOUND ( 'NONE', #69551, .T. ) ;
#9190 = CARTESIAN_POINT ( 'NONE',  ( 74.57962914963242440, 19.59826060529047709, 6.436893197989940418 ) ) ;
#9191 = DIRECTION ( 'NONE',  ( 0.000000000000000000, -0.000000000000000000, -1.000000000000000000 ) ) ;
#9192 = ORIENTED_EDGE ( 'NONE', *, *, #34306, .T. ) ;
#9193 =( LENGTH_UNIT ( ) NAMED_UNIT ( * ) SI_UNIT ( .MILLI., .METRE. ) );
#9194 = ORIENTED_EDGE ( 'NONE', *, *, #25012, .T. ) ;
#9195 = CARTESIAN_POINT ( 'NONE',  ( 23.41056558150575029, 24.55989583710066526, 27.18999999999999417 ) ) ;
#9196 = CIRCLE ( 'NONE', #46271, 0.2500000000000002220 ) ;
#9197 = FILL_AREA_STYLE ('',( #3873 ) ) ;
#9198 = CARTESIAN_POINT ( 'NONE',  ( -65.75499999999998124, 4.716976649647091513, -6.492361379858946790 ) ) ;
#9199 = EDGE_LOOP ( 'NONE', ( #21905, #37331, #49742, #16027 ) ) ;
#9200 = CARTESIAN_POINT ( 'NONE',  ( -65.00000000000000000, -1.962809905030629631E-14, -12.00000000000000000 ) ) ;
#9201 = PRESENTATION_LAYER_ASSIGNMENT (  '', '', ( #39531 ) ) ;
#9202 = CYLINDRICAL_SURFACE ( 'NONE', #10452, 9.524999999999991473 ) ;
#9203 = ORIENTED_EDGE ( 'NONE', *, *, #19941, .F. ) ;
#9204 =( REPRESENTATION_RELATIONSHIP ('NONE','NONE', #5102, #21747 ) REPRESENTATION_RELATIONSHIP_WITH_TRANSFORMATION ( #63792 )SHAPE_REPRESENTATION_RELATIONSHIP( ) );
#9205 = SURFACE_STYLE_USAGE ( .BOTH. , #67588 ) ;
#9206 = STYLED_ITEM ( 'NONE', ( #47687 ), #53301 ) ;
#9208 = CARTESIAN_POINT ( 'NONE',  ( -10.39230484541326938, 2.500000000000000000, -1.734723475976807094E-15 ) ) ;
#9207 = DIRECTION ( 'NONE',  ( 1.000000000000000000, 0.000000000000000000, 0.000000000000000000 ) ) ;
#9209 = VECTOR ( 'NONE', #58309, 1000.000000000000000 ) ;
#9210 = CARTESIAN_POINT ( 'NONE',  ( 9.058813317711338797, 147.8449999999999989, -2.943386871421372675 ) ) ;
#9211 = CARTESIAN_POINT ( 'NONE',  ( -95.99499999999996191, -6.826472737025115478, 4.959722759717900331 ) ) ;
#9212 =( GEOMETRIC_REPRESENTATION_CONTEXT ( 3 ) GLOBAL_UNCERTAINTY_ASSIGNED_CONTEXT ( ( #25720 ) ) GLOBAL_UNIT_ASSIGNED_CONTEXT ( ( #7268, #23778, #12876 ) ) REPRESENTATION_CONTEXT ( 'NONE', 'WORKASPACE' ) );
#9213 = DIRECTION ( 'NONE',  ( -1.000000000000000000, 0.000000000000000000, 0.000000000000000000 ) ) ;
#9214 = CARTESIAN_POINT ( 'NONE',  ( -132.4429263765338192, -1.166476076187852838E-15, -9.524999999999991473 ) ) ;
#9215 = CIRCLE ( 'NONE', #66492, 1.000000000000000888 ) ;
#9216 = CARTESIAN_POINT ( 'NONE',  ( -4.716976649647097730, 144.2429263765338305, -6.492361379858953896 ) ) ;
#9217 = VERTEX_POINT ( 'NONE', #31092 ) ;
#9218 = CARTESIAN_POINT ( 'NONE',  ( -143.8429263765338249, 9.058813317711329915, -2.943386871421373119 ) ) ;
#9219 = DIRECTION ( 'NONE',  ( 1.000000000000000000, 1.554312234475218841E-14, 0.000000000000000000 ) ) ;
#9220 = CARTESIAN_POINT ( 'NONE',  ( -156.5949999999999704, 2.607480562269073321, 8.024999999999991473 ) ) ;
#9221 = AXIS2_PLACEMENT_3D ( 'NONE', #10718, #37505, #44164 ) ;
#9222 = EDGE_CURVE ( 'NONE', #63169, #16904, #54950, .T. ) ;
#9223 = DIRECTION ( 'NONE',  ( 0.000000000000000000, 0.000000000000000000, 1.000000000000000000 ) ) ;
#9224 = CARTESIAN_POINT ( 'NONE',  ( -132.5929263765344785, -3.094860106629523600, -9.524999999991933919 ) ) ;
#9225 = ORIENTED_EDGE ( 'NONE', *, *, #8845, .F. ) ;
#9226 = SURFACE_STYLE_USAGE ( .BOTH. , #27347 ) ;
#9227 = ORIENTED_EDGE ( 'NONE', *, *, #18809, .F. ) ;
#9228 = CARTESIAN_POINT ( 'NONE',  ( 0.000000000000000000, 2.500000000000000000, 0.000000000000000000 ) ) ;
#9229 = COLOUR_RGB ( '', 0.08235294, 0.09019608, 0.10196078) ;
#9230 = LINE ( 'NONE', #32058, #6871 ) ;
#9231 = PLANE ( 'NONE',  #28115 ) ;
#9232 = CARTESIAN_POINT ( 'NONE',  ( -9.250000000000003553, 27.74999999999998934, 3.750000000000000000 ) ) ;
#9233 = AXIS2_PLACEMENT_3D ( 'NONE', #52345, #4443, #63564 ) ;
#9234 = CARTESIAN_POINT ( 'NONE',  ( -60.17648784341465529, -8.499999999999994671, 0.03783916848062766208 ) ) ;
#9235 = ORIENTED_EDGE ( 'NONE', *, *, #27044, .T. ) ;
#9236 = CARTESIAN_POINT ( 'NONE',  ( -157.1049999999999898, -6.826472737025113702, 4.959722759717902107 ) ) ;
#9237 = EDGE_CURVE ( 'NONE', #4798, #67711, #30248, .T. ) ;
#9238 = ORIENTED_EDGE ( 'NONE', *, *, #58093, .T. ) ;
#9239 = DIRECTION ( 'NONE',  ( -0.000000000000000000, -0.000000000000000000, 1.000000000000000000 ) ) ;
#9240 = CARTESIAN_POINT ( 'NONE',  ( 8.082903768654761123, 2.500000000000000000, 9.511133375893962597E-16 ) ) ;
#9241 = STYLED_ITEM ( 'NONE', ( #65968 ), #22340 ) ;
#9243 = EDGE_CURVE ( 'NONE', #52329, #51279, #40292, .T. ) ;
#9242 = ORIENTED_EDGE ( 'NONE', *, *, #36972, .T. ) ;
#9244 = CARTESIAN_POINT ( 'NONE',  ( -195.0000000000000000, 1.166476076187852838E-15, -9.524999999999991473 ) ) ;
#9246 = EDGE_CURVE ( 'NONE', #68919, #10058, #24096, .T. ) ;
#9245 = AXIS2_PLACEMENT_3D ( 'NONE', #69532, #21335, #42858 ) ;
#9247 = DIRECTION ( 'NONE',  ( 0.000000000000000000, 0.000000000000000000, -1.000000000000000000 ) ) ;
#9248 = CARTESIAN_POINT ( 'NONE',  ( -3.094860106618434248, 110.7949999999999733, 9.525000000000000355 ) ) ;
#9249 = AXIS2_PLACEMENT_3D ( 'NONE', #3571, #68009, #19796 ) ;
#9250 = VERTEX_POINT ( 'NONE', #41695 ) ;
#9251 = SURFACE_STYLE_USAGE ( .BOTH. , #21161 ) ;
#9253 = EDGE_CURVE ( 'NONE', #417, #20026, #8965, .T. ) ;
#9252 = CARTESIAN_POINT ( 'NONE',  ( 5.598654528085805993, 124.3549999999999898, 7.705886871421374629 ) ) ;
#9254 = CARTESIAN_POINT ( 'NONE',  ( -74.75499999999998124, 4.716976649647091513, -6.492361379858946790 ) ) ;
#9255 = DIRECTION ( 'NONE',  ( 0.2413793103448194644, 0.9704308468600220117, 0.000000000000000000 ) ) ;
#9256 = ORIENTED_EDGE ( 'NONE', *, *, #57663, .F. ) ;
#9257 = CARTESIAN_POINT ( 'NONE',  ( 10.01517768586949231, 139.8050000000000068, 1.839758294383810543E-15 ) ) ;
#9258 = SPHERICAL_SURFACE ( 'NONE', #25119, 0.5000000000000000000 ) ;
#9259 = FACE_OUTER_BOUND ( 'NONE', #26650, .T. ) ;
#9260 = AXIS2_PLACEMENT_3D ( 'NONE', #43741, #65143, #64806 ) ;
#9261 = DIRECTION ( 'NONE',  ( 0.000000000000000000, 0.000000000000000000, 1.000000000000000000 ) ) ;
#9262 = AXIS2_PLACEMENT_3D ( 'NONE', #56930, #29842, #3054 ) ;
#9263 = PRESENTATION_STYLE_ASSIGNMENT (( #25075 ) ) ;
#9264 = EDGE_LOOP ( 'NONE', ( #6312, #55581, #43130, #32895, #69047 ) ) ;
#9265 =( NAMED_UNIT ( * ) SI_UNIT ( $, .STERADIAN. ) SOLID_ANGLE_UNIT ( ) );
#9266 = CARTESIAN_POINT ( 'NONE',  ( -13.75000000000000355, 28.24999999999998934, 4.000000000000000000 ) ) ;
#9267 = CARTESIAN_POINT ( 'NONE',  ( -179.7549999999999955, 4.716976649647091513, -6.492361379858946790 ) ) ;
#9268 = EDGE_LOOP ( 'NONE', ( #63884, #42354, #40070, #23487 ) ) ;
#9269 = CARTESIAN_POINT ( 'NONE',  ( 0.5396081309076795618, 110.8751430657346617, 9.149856934265335084 ) ) ;
#9270 = ORIENTED_EDGE ( 'NONE', *, *, #9407, .T. ) ;
#9271 = FILL_AREA_STYLE_COLOUR ( '', #53511 ) ;
#9272 = VERTEX_POINT ( 'NONE', #24767 ) ;
#9273 = SURFACE_STYLE_USAGE ( .BOTH. , #36003 ) ;
#9274 = CARTESIAN_POINT ( 'NONE',  ( -94.40500000000000114, -2.607480562269069768, 8.024999999999991473 ) ) ;
#9275 = VERTEX_POINT ( 'NONE', #63118 ) ;
#9276 = FACE_OUTER_BOUND ( 'NONE', #55975, .T. ) ;
#9277 = DIRECTION ( 'NONE',  ( -1.000000000000000000, 0.000000000000000000, 0.000000000000000000 ) ) ;
#9278 = CARTESIAN_POINT ( 'NONE',  ( -136.1070736234661922, 8.102448949553171076, -5.886773742842744461 ) ) ;
#9279 = STYLED_ITEM ( 'NONE', ( #7317 ), #60805 ) ;
#9280 = CARTESIAN_POINT ( 'NONE',  ( 3.094860106618431583, 153.0949999999999989, 9.525000000000000355 ) ) ;
#9281 = CARTESIAN_POINT ( 'NONE',  ( -79.70707362346614389, -3.094860106618431139, -9.524999999999991473 ) ) ;
#9282 = CIRCLE ( 'NONE', #3596, 4.999999999999997335 ) ;
#9283 = PLANE ( 'NONE',  #56106 ) ;
#9284 = VERTEX_POINT ( 'NONE', #46289 ) ;
#9285 = LINE ( 'NONE', #46957, #64195 ) ;
#9287 = CARTESIAN_POINT ( 'NONE',  ( 12.72792206135785698, 115.4999999999999574, -10.50000000000000000 ) ) ;
#9286 = AXIS2_PLACEMENT_3D ( 'NONE', #25840, #9342, #20574 ) ;
#9288 = FACE_OUTER_BOUND ( 'NONE', #19603, .T. ) ;
#9289 = CARTESIAN_POINT ( 'NONE',  ( -119.6049999999999756, 6.826472737025113702, -4.959722759717902107 ) ) ;
#9290 =( NAMED_UNIT ( * ) PLANE_ANGLE_UNIT ( ) SI_UNIT ( $, .RADIAN. ) );
#9291 = CARTESIAN_POINT ( 'NONE',  ( -3.094860106618432471, 115.5949999999999704, -9.525000000000000355 ) ) ;
#9292 = VECTOR ( 'NONE', #53530, 1000.000000000000000 ) ;
#9293 = CARTESIAN_POINT ( 'NONE',  ( -123.8949999999999676, 6.826472737025116366, 4.959722759717898555 ) ) ;
#9294 = ORIENTED_EDGE ( 'NONE', *, *, #20178, .T. ) ;
#9295 = COLOUR_RGB ( '', 0.66274510, 0.83137255, 0.94901961) ;
#9296 = FILL_AREA_STYLE ('',( #14932 ) ) ;
#9297 = FACE_OUTER_BOUND ( 'NONE', #59587, .T. ) ;
#9298 = EDGE_LOOP ( 'NONE', ( #8122, #9950, #16360, #45151, #21143, #17735, #40212 ) ) ;
#9299 = CARTESIAN_POINT ( 'NONE',  ( 62.24999999999998579, 33.74999999999999289, 4.000000000000000000 ) ) ;
#9300 = CARTESIAN_POINT ( 'NONE',  ( -176.6929263765338192, 10.01517768586948698, -1.839758294383808571E-15 ) ) ;
#9301 =( NAMED_UNIT ( * ) SI_UNIT ( $, .STERADIAN. ) SOLID_ANGLE_UNIT ( ) );
#9302 = CARTESIAN_POINT ( 'NONE',  ( -71.49999999999998579, 119.9999999999997868, -7.000000000000000000 ) ) ;
#9303 = CIRCLE ( 'NONE', #57589, 5.000000000000000888 ) ;
#9304 =( GEOMETRIC_REPRESENTATION_CONTEXT ( 3 ) GLOBAL_UNCERTAINTY_ASSIGNED_CONTEXT ( ( #8890 ) ) GLOBAL_UNIT_ASSIGNED_CONTEXT ( ( #64027, #27060, #21825 ) ) REPRESENTATION_CONTEXT ( 'NONE', 'WORKASPACE' ) );
#9305 = CARTESIAN_POINT ( 'NONE',  ( 0.000000000000000000, 0.000000000000000000, 0.000000000000000000 ) ) ;
#9306 = AXIS2_PLACEMENT_3D ( 'NONE', #48147, #59323, #32598 ) ;
#9307 = EDGE_CURVE ( 'NONE', #35954, #20328, #67708, .T. ) ;
#9308 = CARTESIAN_POINT ( 'NONE',  ( 23.50000000000001776, 42.00000000000000000, -29.68999999999999417 ) ) ;
#9309 = CARTESIAN_POINT ( 'NONE',  ( 3.999798566743339556, 8.867945265733707672, -2.000000000000000000 ) ) ;
#9310 = ORIENTED_EDGE ( 'NONE', *, *, #24946, .F. ) ;
#9311 = CARTESIAN_POINT ( 'NONE',  ( -83.54292637653381348, 9.058813317711329915, 2.943386871421369566 ) ) ;
#9312 = ITEM_DEFINED_TRANSFORMATION ( 'NONE', 'NONE', #62969,  #42840 ) ;
#9314 = EDGE_CURVE ( 'NONE', #56811, #52016, #22383, .T. ) ;
#9313 = CARTESIAN_POINT ( 'NONE',  ( -72.50000000000000000, 35.92875272052971525, 9.500000000000000000 ) ) ;
#9315 = CARTESIAN_POINT ( 'NONE',  ( -165.4429263765337907, -1.166476076187852838E-15, -9.524999999999991473 ) ) ;
#9316 = STYLED_ITEM ( 'NONE', ( #40527 ), #25881 ) ;
#9317 =( BOUNDED_CURVE ( )  B_SPLINE_CURVE ( 2, ( #44639, #50569, #18205, #49890, #40369, #13609, #7316, #28030, #1630, #39689, #45674 ),
 .UNSPECIFIED., .F., .F. ) 
 B_SPLINE_CURVE_WITH_KNOTS ( ( 3, 2, 2, 2, 2, 3 ),
 ( 0.4673913043478149509, 0.4695652173912931437, 0.4717391304347713366, 0.4739130434782495849, 0.4760869565217278332, 0.4782608695652060260 ),
 .UNSPECIFIED. ) 
 CURVE ( )  GEOMETRIC_REPRESENTATION_ITEM ( )  RATIONAL_B_SPLINE_CURVE ( ( 1.000000000000251132, 0.9510565162949022877, 1.000000000000000000, 0.9510565162951535312, 1.000000000000000000, 0.9510565162951535312, 1.000000000000000000, 0.9510565162951535312, 1.000000000000000000, 0.9510565162954097707, 0.9999999999997437605 ) ) 
 REPRESENTATION_ITEM ( '' )  );
#9318 = CARTESIAN_POINT ( 'NONE',  ( 0.000000000000000000, 87.30187232391182306, 0.000000000000000000 ) ) ;
#9319 = MECHANICAL_DESIGN_GEOMETRIC_PRESENTATION_REPRESENTATION (  '', ( #235 ), #29530 ) ;
#9320 = FILL_AREA_STYLE ('',( #67019 ) ) ;
#9321 = VERTEX_POINT ( 'NONE', #67021 ) ;
#9322 = DIRECTION ( 'NONE',  ( 0.000000000000000000, 0.000000000000000000, 1.000000000000000000 ) ) ;
#9323 = EDGE_CURVE ( 'NONE', #52417, #29181, #13395, .T. ) ;
#9324 = DIRECTION ( 'NONE',  ( 0.000000000000000000, -0.000000000000000000, 1.000000000000000000 ) ) ;
#9325 = VERTEX_POINT ( 'NONE', #45926 ) ;
#9326 = AXIS2_PLACEMENT_3D ( 'NONE', #38597, #59993, #60336 ) ;
#9327 = CARTESIAN_POINT ( 'NONE',  ( 4.716976649647099507, 135.7570736234661695, -6.492361379858953008 ) ) ;
#9328 = CIRCLE ( 'NONE', #39668, 12.50000000000001066 ) ;
#9329 = EDGE_LOOP ( 'NONE', ( #22080, #40183, #38140 ) ) ;
#9331 = ADVANCED_FACE ( 'NONE', ( #48033 ), #59200, .F. ) ;
#9330 = CARTESIAN_POINT ( 'NONE',  ( -101.0070736234661695, -8.102448949553174629, -5.886773742842741797 ) ) ;
#9332 = CARTESIAN_POINT ( 'NONE',  ( -107.1549999999999869, 7.632228543268600340, 2.479861379858949277 ) ) ;
#9333 = CARTESIAN_POINT ( 'NONE',  ( 71.74137931034479720, 63.10081643261027295, -10.00000000000000000 ) ) ;
#9334 = ORIENTED_EDGE ( 'NONE', *, *, #3521, .T. ) ;
#9335 = CARTESIAN_POINT ( 'NONE',  ( -35.63345864320083223, -11.41101942758246857, 1.735234313984338694 ) ) ;
#9336 = DIRECTION ( 'NONE',  ( -1.000000000000000000, 0.000000000000000000, 0.000000000000000000 ) ) ;
#9337 = SURFACE_STYLE_USAGE ( .BOTH. , #48297 ) ;
#9338 = DIRECTION ( 'NONE',  ( 1.000000000000000000, 0.000000000000000000, 0.000000000000000000 ) ) ;
#9339 = VECTOR ( 'NONE', #69288, 1000.000000000000000 ) ;
#9340 = EDGE_LOOP ( 'NONE', ( #28613, #41434, #21065, #15070 ) ) ;
#9341 = CIRCLE ( 'NONE', #55412, 1.000000000000000888 ) ;
#9342 = DIRECTION ( 'NONE',  ( 0.000000000000000000, 0.000000000000000000, 1.000000000000000000 ) ) ;
#9343 = CARTESIAN_POINT ( 'NONE',  ( -68.09499999999998465, -2.607480562269071545, -8.024999999999991473 ) ) ;
#9344 = ORIENTED_EDGE ( 'NONE', *, *, #60204, .T. ) ;
#9345 = DIRECTION ( 'NONE',  ( 0.000000000000000000, 0.000000000000000000, 1.000000000000000000 ) ) ;
#9346 = UNCERTAINTY_MEASURE_WITH_UNIT (LENGTH_MEASURE( 1.000000000000000082E-05 ), #18697, 'distance_accuracy_value', 'NONE');
#9347 = VERTEX_POINT ( 'NONE', #20550 ) ;
#9348 = LINE ( 'NONE', #52276, #61669 ) ;
#9349 = CARTESIAN_POINT ( 'NONE',  ( -22.75000000000000711, 36.75000000000000000, -4.000000000000000000 ) ) ;
#9350 =( GEOMETRIC_REPRESENTATION_CONTEXT ( 3 ) GLOBAL_UNCERTAINTY_ASSIGNED_CONTEXT ( ( #31113 ) ) GLOBAL_UNIT_ASSIGNED_CONTEXT ( ( #40578, #8208, #66594 ) ) REPRESENTATION_CONTEXT ( 'NONE', 'WORKASPACE' ) );
#9351 = COLOUR_RGB ( '', 0.66274510, 0.83137255, 0.94901961) ;
#9352 = SURFACE_STYLE_USAGE ( .BOTH. , #57526 ) ;
#9353 =( NAMED_UNIT ( * ) SI_UNIT ( $, .STERADIAN. ) SOLID_ANGLE_UNIT ( ) );
#9354 = EDGE_LOOP ( 'NONE', ( #69301, #33099, #48990, #68768 ) ) ;
#9355 = COLOUR_RGB ( '', 0.72549020, 0.75294118, 0.79215686) ;
#9356 = DIRECTION ( 'NONE',  ( -1.000000000000000000, -0.000000000000000000, -0.000000000000000000 ) ) ;
#9357 = EDGE_LOOP ( 'NONE', ( #3466, #14358, #9142, #33731, #59320, #166 ) ) ;
#9358 = FILL_AREA_STYLE ('',( #52283 ) ) ;
#9359 = CARTESIAN_POINT ( 'NONE',  ( -149.8429263765337964, 9.058813317711329915, -2.943386871421373119 ) ) ;
#9360 = CARTESIAN_POINT ( 'NONE',  ( 18.00000000000000711, 33.74999999999999289, 3.750000000000000000 ) ) ;
#9361 = CARTESIAN_POINT ( 'NONE',  ( -172.7070736234661581, -3.094860106618431139, -9.524999999999991473 ) ) ;
#9362 = UNCERTAINTY_MEASURE_WITH_UNIT (LENGTH_MEASURE( 1.000000000000000082E-05 ), #24393, 'distance_accuracy_value', 'NONE');
#9363 = CARTESIAN_POINT ( 'NONE',  ( 9.058813317711338797, 126.8449999999999847, -2.943386871421372675 ) ) ;
#9364 = CARTESIAN_POINT ( 'NONE',  ( -102.5070736234661837, 8.102448949553176405, 5.886773742842740909 ) ) ;
#9365 = EDGE_CURVE ( 'NONE', #60568, #63828, #32469, .T. ) ;
#9366 = STYLED_ITEM ( 'NONE', ( #11600 ), #26213 ) ;
#9367 = DIRECTION ( 'NONE',  ( 0.000000000000000000, 1.000000000000000000, 0.000000000000000000 ) ) ;
#9368 = ORIENTED_EDGE ( 'NONE', *, *, #2328, .F. ) ;
#9369 = DIRECTION ( 'NONE',  ( 1.000000000000000000, 0.000000000000000000, 0.000000000000000000 ) ) ;
#9370 = DIRECTION ( 'NONE',  ( -0.000000000000000000, 1.000000000000000000, -0.000000000000000000 ) ) ;
#9372 = CARTESIAN_POINT ( 'NONE',  ( 2.816687638038912352E-15, 154.9999999999999716, 23.00000000000000000 ) ) ;
#9371 = DIRECTION ( 'NONE',  ( -0.000000000000000000, -0.000000000000000000, -1.000000000000000000 ) ) ;
#9373 = CARTESIAN_POINT ( 'NONE',  ( 60.00000000000000000, 1.797044900979284448E-15, 6.999999999999988454 ) ) ;
#9374 = CARTESIAN_POINT ( 'NONE',  ( -152.9049999999999727, 2.607480562269068880, -8.024999999999993250 ) ) ;
#9375 = CARTESIAN_POINT ( 'NONE',  ( -75.00000000000000000, 9.519990751839809917, 6.451194676399506278 ) ) ;
#9376 = CARTESIAN_POINT ( 'NONE',  ( -8.255262359011400264, 111.6843284473704472, 1.256501419248624352 ) ) ;
#9377 = CARTESIAN_POINT ( 'NONE',  ( -152.6949999999999932, -8.437984349512085203, 5.166775262442717831E-16 ) ) ;
#9379 = VECTOR ( 'NONE', #8810, 1000.000000000000000 ) ;
#9378 = CONICAL_SURFACE ( 'NONE', #45347, 7.500000000000000000, 0.7853981633974518317 ) ;
#9380 = CARTESIAN_POINT ( 'NONE',  ( -152.2450000000000045, -4.716976649647093289, -6.492361379858945902 ) ) ;
#9381 = ORIENTED_EDGE ( 'NONE', *, *, #62291, .F. ) ;
#9382 = CARTESIAN_POINT ( 'NONE',  ( -180.2070736234662434, 3.094860106619025775, 9.524999999999563371 ) ) ;
#9383 = STYLED_ITEM ( 'NONE', ( #19805 ), #46912 ) ;
#9384 = SURFACE_STYLE_FILL_AREA ( #8339 ) ;
#9385 = CARTESIAN_POINT ( 'NONE',  ( 29.00000000000002842, 42.00000000000000000, 3.902931319921305165E-16 ) ) ;
#9386 = UNCERTAINTY_MEASURE_WITH_UNIT (LENGTH_MEASURE( 1.000000000000000082E-05 ), #69509, 'distance_accuracy_value', 'NONE');
#9387 = CARTESIAN_POINT ( 'NONE',  ( -67.70499999999998408, 2.607480562269073321, 8.024999999999991473 ) ) ;
#9388 = CARTESIAN_POINT ( 'NONE',  ( 8.000000000000035527, 5.000000000000000000, -77.00402776293825013 ) ) ;
#9389 = CARTESIAN_POINT ( 'NONE',  ( -153.0570736234661808, 0.000000000000000000, 9.524999999999991473 ) ) ;
#9390 = EDGE_CURVE ( 'NONE', #48634, #4737, #5540, .T. ) ;
#9391 = CARTESIAN_POINT ( 'NONE',  ( -60.59499999999997755, 2.607480562269072433, 8.024999999999991473 ) ) ;
#9392 = AXIS2_PLACEMENT_3D ( 'NONE', #15637, #43450, #26500 ) ;
#9393 = EDGE_CURVE ( 'NONE', #61842, #3021, #40378, .T. ) ;
#9394 = CARTESIAN_POINT ( 'NONE',  ( 9.058813317711337021, 160.6550000000000011, 2.943386871421375783 ) ) ;
#9395 =( LENGTH_UNIT ( ) NAMED_UNIT ( * ) SI_UNIT ( .MILLI., .METRE. ) );
#9396 = CARTESIAN_POINT ( 'NONE',  ( -112.9429263765338050, 0.000000000000000000, 9.524999999999991473 ) ) ;
#9397 = UNCERTAINTY_MEASURE_WITH_UNIT (LENGTH_MEASURE( 1.000000000000000082E-05 ), #40987, 'distance_accuracy_value', 'NONE');
#9398 = FILL_AREA_STYLE_COLOUR ( '', #33743 ) ;
#9399 = CIRCLE ( 'NONE', #13898, 1.000000000000000888 ) ;
#9400 =( NAMED_UNIT ( * ) PLANE_ANGLE_UNIT ( ) SI_UNIT ( $, .RADIAN. ) );
#9401 = EDGE_CURVE ( 'NONE', #29467, #48775, #69106, .T. ) ;
#9402 = MECHANICAL_DESIGN_GEOMETRIC_PRESENTATION_REPRESENTATION (  '', ( #18386 ), #13902 ) ;
#9403 = SURFACE_STYLE_USAGE ( .BOTH. , #24489 ) ;
#9404 = CARTESIAN_POINT ( 'NONE',  ( -178.1929263765338192, -10.01517768586948698, 6.132527647946031529E-16 ) ) ;
#9405 = AXIS2_PLACEMENT_3D ( 'NONE', #54888, #6715, #13376 ) ;
#9406 = CIRCLE ( 'NONE', #6017, 5.000000000000004441 ) ;
#9407 = EDGE_CURVE ( 'NONE', #34574, #4197, #15684, .T. ) ;
#9408 = FILL_AREA_STYLE ('',( #41425 ) ) ;
#9409 = ORIENTED_EDGE ( 'NONE', *, *, #35742, .T. ) ;
#9410 = ORIENTED_EDGE ( 'NONE', *, *, #18695, .F. ) ;
#9411 = DIRECTION ( 'NONE',  ( 1.189524669241239115E-16, 1.000000000000000000, 0.000000000000000000 ) ) ;
#9412 = PRESENTATION_LAYER_ASSIGNMENT (  '', '', ( #58808 ) ) ;
#9414 = EDGE_CURVE ( 'NONE', #64993, #10966, #10056, .T. ) ;
#9413 = CARTESIAN_POINT ( 'NONE',  ( -20.68718488045382742, 114.6829008731431543, 10.00000000000011724 ) ) ;
#9415 = CARTESIAN_POINT ( 'NONE',  ( 23.14573592869279750, 24.60297829105063983, -27.21022641015704835 ) ) ;
#9416 = EDGE_LOOP ( 'NONE', ( #63013, #21097, #69019 ) ) ;
#9417 = VERTEX_POINT ( 'NONE', #43461 ) ;
#9418 = DIRECTION ( 'NONE',  ( 0.000000000000000000, 0.000000000000000000, 1.000000000000000000 ) ) ;
#9419 = FILL_AREA_STYLE ('',( #57591 ) ) ;
#9420 = PRESENTATION_LAYER_ASSIGNMENT (  '', '', ( #65688 ) ) ;
#9421 = EDGE_LOOP ( 'NONE', ( #7352, #45612, #9063, #68113, #16032 ) ) ;
#9422 = CARTESIAN_POINT ( 'NONE',  ( -5.598654528085808657, 117.7549999999999812, 7.705886871421373741 ) ) ;
#9423 = CARTESIAN_POINT ( 'NONE',  ( -85.19292637653380496, -10.01517768586948698, 6.132527647946031529E-16 ) ) ;
#9424 = PRESENTATION_LAYER_ASSIGNMENT (  '', '', ( #46522 ) ) ;
#9425 =( NAMED_UNIT ( * ) SI_UNIT ( $, .STERADIAN. ) SOLID_ANGLE_UNIT ( ) );
#9426 = CARTESIAN_POINT ( 'NONE',  ( -103.6449999999999818, 4.716976649647091513, -6.492361379858946790 ) ) ;
#9427 = VERTEX_POINT ( 'NONE', #10696 ) ;
#9428 = CARTESIAN_POINT ( 'NONE',  ( 74.99999999999998579, 50.00000000000000000, 7.500000000000000000 ) ) ;
#9429 = AXIS2_PLACEMENT_3D ( 'NONE', #58071, #64366, #10566 ) ;
#9430 = ORIENTED_EDGE ( 'NONE', *, *, #64155, .F. ) ;
#9431 = CARTESIAN_POINT ( 'NONE',  ( 8.437984349512095861, 155.1929263765338192, 1.550032578732817026E-15 ) ) ;
#9432 = FACE_OUTER_BOUND ( 'NONE', #60566, .T. ) ;
#9433 = EDGE_LOOP ( 'NONE', ( #18884, #22184, #45088, #43483 ) ) ;
#9434 = CARTESIAN_POINT ( 'NONE',  ( 19.89974874213240241, 114.9999999999999574, -10.49999999999999822 ) ) ;
#9435 = ORIENTED_EDGE ( 'NONE', *, *, #68041, .T. ) ;
#9436 = SURFACE_SIDE_STYLE ('',( #14712 ) ) ;
#9437 = DIRECTION ( 'NONE',  ( 0.000000000000000000, 0.000000000000000000, 1.000000000000000000 ) ) ;
#9438 = CARTESIAN_POINT ( 'NONE',  ( -120.3549999999999898, -4.716976649647093289, -6.492361379858945902 ) ) ;
#9439 =( GEOMETRIC_REPRESENTATION_CONTEXT ( 3 ) GLOBAL_UNCERTAINTY_ASSIGNED_CONTEXT ( ( #44071 ) ) GLOBAL_UNIT_ASSIGNED_CONTEXT ( ( #62098, #29395, #13562 ) ) REPRESENTATION_CONTEXT ( 'NONE', 'WORKASPACE' ) );
#9440 = CARTESIAN_POINT ( 'NONE',  ( -8.921435019309294474E-16, -7.500000000000000888, 0.000000000000000000 ) ) ;
#9441 = CARTESIAN_POINT ( 'NONE',  ( -71.99999999999998579, 64.07124727947029896, -10.00000000000000000 ) ) ;
#9442 = DIRECTION ( 'NONE',  ( 0.000000000000000000, 0.000000000000000000, -1.000000000000000000 ) ) ;
#9443 =( BOUNDED_CURVE ( )  B_SPLINE_CURVE ( 2, ( #16941, #37743, #54544, #59827, #59124, #6356, #10612, #10946, #53521, #6695, #44402 ),
 .UNSPECIFIED., .F., .F. ) 
 B_SPLINE_CURVE_WITH_KNOTS ( ( 3, 2, 2, 2, 2, 3 ),
 ( 0.2391304347826030130, 0.2413043478260812058, 0.2434782608695594264, 0.2456521739130376469, 0.2478260869565158675, 0.2499999999999940603 ),
 .UNSPECIFIED. ) 
 CURVE ( )  GEOMETRIC_REPRESENTATION_ITEM ( )  RATIONAL_B_SPLINE_CURVE ( ( 1.000000000000128120, 0.9510565162950255225, 1.000000000000000000, 0.9510565162951535312, 1.000000000000000000, 0.9510565162951535312, 1.000000000000000000, 0.9510565162951535312, 1.000000000000000000, 0.9510565162952872020, 0.9999999999998663291 ) ) 
 REPRESENTATION_ITEM ( '' )  );
#9444 = ADVANCED_FACE ( 'NONE', ( #53934 ), #53601, .T. ) ;
#9445 = SURFACE_SIDE_STYLE ('',( #25585 ) ) ;
#9447 = DIRECTION ( 'NONE',  ( 0.000000000000000000, 0.000000000000000000, 1.000000000000000000 ) ) ;
#9446 = AXIS2_PLACEMENT_3D ( 'NONE', #10250, #57388, #30990 ) ;
#9448 = CARTESIAN_POINT ( 'NONE',  ( 21.25000000000001066, 24.99999999999998579, -3.750000000000000000 ) ) ;
#9449 = ORIENTED_EDGE ( 'NONE', *, *, #18282, .T. ) ;
#9450 = ORIENTED_EDGE ( 'NONE', *, *, #44371, .T. ) ;
#9451 = DIRECTION ( 'NONE',  ( -0.000000000000000000, -0.000000000000000000, -1.000000000000000000 ) ) ;
#9452 = AXIS2_PLACEMENT_3D ( 'NONE', #59388, #53457, #5935 ) ;
#9453 = CARTESIAN_POINT ( 'NONE',  ( 74.65811388300841145, 19.88603796100278487, 6.292893218813452094 ) ) ;
#9454 = ORIENTED_EDGE ( 'NONE', *, *, #62505, .T. ) ;
#9455 = CARTESIAN_POINT ( 'NONE',  ( 3.414213562373125121, 42.99999999999999289, 90.00000000000001421 ) ) ;
#9456 = CARTESIAN_POINT ( 'NONE',  ( -175.7049999999999557, 2.607480562269073321, 8.024999999999991473 ) ) ;
#9457 = LINE ( 'NONE', #43239, #50976 ) ;
#9458 =( NAMED_UNIT ( * ) PLANE_ANGLE_UNIT ( ) SI_UNIT ( $, .RADIAN. ) );
#9459 = CARTESIAN_POINT ( 'NONE',  ( -47.45707362346615810, -9.058813317711329915, 2.943386871421371787 ) ) ;
#9460 =( GEOMETRIC_REPRESENTATION_CONTEXT ( 3 ) GLOBAL_UNCERTAINTY_ASSIGNED_CONTEXT ( ( #52274 ) ) GLOBAL_UNIT_ASSIGNED_CONTEXT ( ( #4181, #14791, #9524 ) ) REPRESENTATION_CONTEXT ( 'NONE', 'WORKASPACE' ) );
#9461 = CARTESIAN_POINT ( 'NONE',  ( -180.5949999999999704, 2.607480562269072433, 8.024999999999991473 ) ) ;
#9462 = DIRECTION ( 'NONE',  ( -1.000000000000000000, 0.000000000000000000, 0.000000000000000000 ) ) ;
#9463 = EDGE_LOOP ( 'NONE', ( #28404, #48874, #54744, #17323 ) ) ;
#9464 = VECTOR ( 'NONE', #34003, 1000.000000000000000 ) ;
#9465 = VECTOR ( 'NONE', #41722, 1000.000000000000000 ) ;
#9466 = EDGE_CURVE ( 'NONE', #22579, #11830, #42066, .T. ) ;
#9467 =( LENGTH_UNIT ( ) NAMED_UNIT ( * ) SI_UNIT ( .MILLI., .METRE. ) );
#9468 = CARTESIAN_POINT ( 'NONE',  ( -11.23379897725272336, 11.53847739608159806, -3.304761116138219545 ) ) ;
#9469 = CARTESIAN_POINT ( 'NONE',  ( -96.65499999999998693, -7.632228543268600340, -2.479861379858950166 ) ) ;
#9470 =( LENGTH_UNIT ( ) NAMED_UNIT ( * ) SI_UNIT ( .MILLI., .METRE. ) );
#9471 = SURFACE_STYLE_USAGE ( .BOTH. , #40802 ) ;
#9472 = FILL_AREA_STYLE ('',( #14746 ) ) ;
#9473 = ADVANCED_FACE ( 'NONE', ( #20907 ), #32147, .T. ) ;
#9474 = AXIS2_PLACEMENT_3D ( 'NONE', #26283, #25583, #15766 ) ;
#9475 = CARTESIAN_POINT ( 'NONE',  ( -85.94499999999999318, -9.827790563157499189E-16, -8.024999999999991473 ) ) ;
#9476 = EDGE_CURVE ( 'NONE', #23152, #61204, #68490, .T. ) ;
#9477 = CARTESIAN_POINT ( 'NONE',  ( -3.094860106618434248, 129.9050000000000011, 9.525000000000000355 ) ) ;
#9478 = CARTESIAN_POINT ( 'NONE',  ( -64.19499999999999318, 8.437984349512085203, -1.550032578732815448E-15 ) ) ;
#9479 = CARTESIAN_POINT ( 'NONE',  ( 19.89974874213239886, 114.9999999999999574, -10.49999999999999645 ) ) ;
#9480 = CIRCLE ( 'NONE', #17371, 0.2500000000000002220 ) ;
#9481 = PRESENTATION_LAYER_ASSIGNMENT (  '', '', ( #44307 ) ) ;
#9482 = CARTESIAN_POINT ( 'NONE',  ( 24.00000000000000355, 37.00000000000000000, -3.750000000000000000 ) ) ;
#9483 = DIRECTION ( 'NONE',  ( -1.000000000000000000, 0.000000000000000000, 0.000000000000000000 ) ) ;
#9484 = UNCERTAINTY_MEASURE_WITH_UNIT (LENGTH_MEASURE( 1.000000000000000082E-05 ), #29945, 'distance_accuracy_value', 'NONE');
#9485 = SURFACE_SIDE_STYLE ('',( #3434 ) ) ;
#9486 = DIRECTION ( 'NONE',  ( 0.000000000000000000, 0.9396926207859082059, 0.3420201433256693790 ) ) ;
#9487 = ORIENTED_EDGE ( 'NONE', *, *, #52980, .T. ) ;
#9488 = EDGE_CURVE ( 'NONE', #8740, #3437, #11729, .T. ) ;
#9489 = CARTESIAN_POINT ( 'NONE',  ( -101.2429263765338021, 5.598654528085804216, 7.705886871421366635 ) ) ;
#9490 = CARTESIAN_POINT ( 'NONE',  ( -127.3449999999999847, 7.632228543268599452, -2.479861379858951942 ) ) ;
#9491 = EDGE_CURVE ( 'NONE', #29106, #65770, #1095, .T. ) ;
#9492 = STYLED_ITEM ( 'NONE', ( #23748 ), #38644 ) ;
#9493 = FILL_AREA_STYLE_COLOUR ( '', #5587 ) ;
#9495 = CARTESIAN_POINT ( 'NONE',  ( -4.250000000000001776, 22.24999999999998579, -4.000000000000000000 ) ) ;
#9494 = LINE ( 'NONE', #57664, #35200 ) ;
#9496 = SURFACE_STYLE_FILL_AREA ( #19321 ) ;
#9497 = ORIENTED_EDGE ( 'NONE', *, *, #50438, .T. ) ;
#9498 = EDGE_LOOP ( 'NONE', ( #45602, #26466, #13212, #57136 ) ) ;
#9499 = SURFACE_STYLE_USAGE ( .BOTH. , #58701 ) ;
#9500 = AXIS2_PLACEMENT_3D ( 'NONE', #49289, #28126, #999 ) ;
#9502 = UNCERTAINTY_MEASURE_WITH_UNIT (LENGTH_MEASURE( 1.000000000000000082E-05 ), #1539, 'distance_accuracy_value', 'NONE');
#9501 =( GEOMETRIC_REPRESENTATION_CONTEXT ( 3 ) GLOBAL_UNCERTAINTY_ASSIGNED_CONTEXT ( ( #65069 ) ) GLOBAL_UNIT_ASSIGNED_CONTEXT ( ( #67715, #52593, #3286 ) ) REPRESENTATION_CONTEXT ( 'NONE', 'WORKASPACE' ) );
#9503 = AXIS2_PLACEMENT_3D ( 'NONE', #40809, #34794, #45055 ) ;
#9504 = DIRECTION ( 'NONE',  ( 0.000000000000000000, 0.000000000000000000, 1.000000000000000000 ) ) ;
#9505 = CARTESIAN_POINT ( 'NONE',  ( 23.21231517720797655, 117.4999999999999716, -7.500000000000000000 ) ) ;
#9506 = CARTESIAN_POINT ( 'NONE',  ( 1.000000000000000000, 14.00000000000000000, -36.49999999999999289 ) ) ;
#9507 = ORIENTED_EDGE ( 'NONE', *, *, #62089, .T. ) ;
#9508 = CARTESIAN_POINT ( 'NONE',  ( -123.2049999999999699, -2.607480562269071545, -8.024999999999991473 ) ) ;
#9509 = VERTEX_POINT ( 'NONE', #44140 ) ;
#9510 = VECTOR ( 'NONE', #22905, 1000.000000000000000 ) ;
#9511 = PRESENTATION_STYLE_ASSIGNMENT (( #44488 ) ) ;
#9512 = CARTESIAN_POINT ( 'NONE',  ( -125.0070736234661979, -8.102448949553172852, -5.886773742842741797 ) ) ;
#9513 = VERTEX_POINT ( 'NONE', #17386 ) ;
#9514 = CARTESIAN_POINT ( 'NONE',  ( 44.99999999999977973, 146.4999999999999716, 7.000000000000000000 ) ) ;
#9515 = CARTESIAN_POINT ( 'NONE',  ( 6.062177826491067734, 2.500000000000000000, 3.500000000000000000 ) ) ;
#9516 = VERTEX_POINT ( 'NONE', #44815 ) ;
#9517 = EDGE_CURVE ( 'NONE', #56729, #61204, #39189, .T. ) ;
#9518 = FACE_OUTER_BOUND ( 'NONE', #61001, .T. ) ;
#9519 = CARTESIAN_POINT ( 'NONE',  ( -9.058813317711337021, 149.0449999999999875, -2.943386871421374895 ) ) ;
#9520 = SURFACE_STYLE_USAGE ( .BOTH. , #16536 ) ;
#9521 = TOROIDAL_SURFACE ( 'NONE', #66797, 0.5000000000000000000, 0.2500000000000000000 ) ;
#9522 = ORIENTED_EDGE ( 'NONE', *, *, #16085, .T. ) ;
#9523 = AXIS2_PLACEMENT_3D ( 'NONE', #63240, #36192, #9793 ) ;
#9524 =( NAMED_UNIT ( * ) SI_UNIT ( $, .STERADIAN. ) SOLID_ANGLE_UNIT ( ) );
#9525 = CARTESIAN_POINT ( 'NONE',  ( -3.094860106618434248, 147.9049999999999443, 9.525000000000000355 ) ) ;
#9526 = ORIENTED_EDGE ( 'NONE', *, *, #65403, .T. ) ;
#9527 = CARTESIAN_POINT ( 'NONE',  ( -6.826472737025120807, 123.3929263765337936, -4.959722759717907437 ) ) ;
#9528 = DIRECTION ( 'NONE',  ( 1.000000000000000000, 0.000000000000000000, 0.000000000000000000 ) ) ;
#9529 = UNCERTAINTY_MEASURE_WITH_UNIT (LENGTH_MEASURE( 1.000000000000000082E-05 ), #15602, 'distance_accuracy_value', 'NONE');
#9530 = SURFACE_SIDE_STYLE ('',( #31283 ) ) ;
#9531 = CIRCLE ( 'NONE', #39873, 1.000000000000000888 ) ;
#9532 = CARTESIAN_POINT ( 'NONE',  ( 22.75000000000000711, 36.75000000000000000, 4.000000000000000000 ) ) ;
#9533 = CARTESIAN_POINT ( 'NONE',  ( 66.24999999999998579, 34.24999999999999289, -4.000000000000000000 ) ) ;
#9534 = EDGE_LOOP ( 'NONE', ( #49471, #54439, #1183, #43572 ) ) ;
#9535 = CARTESIAN_POINT ( 'NONE',  ( 41.03386404901051776, 107.6974965691264856, 3.186685921634084817 ) ) ;
#9536 = VERTEX_POINT ( 'NONE', #23320 ) ;
#9537 = CARTESIAN_POINT ( 'NONE',  ( -60.59292637653378932, -3.094860106618431139, -9.524999999999991473 ) ) ;
#9538 =( GEOMETRIC_REPRESENTATION_CONTEXT ( 3 ) GLOBAL_UNCERTAINTY_ASSIGNED_CONTEXT ( ( #25530 ) ) GLOBAL_UNIT_ASSIGNED_CONTEXT ( ( #48368, #33531, #28214 ) ) REPRESENTATION_CONTEXT ( 'NONE', 'WORKASPACE' ) );
#9539 = MECHANICAL_DESIGN_GEOMETRIC_PRESENTATION_REPRESENTATION (  '', ( #60063 ), #17372 ) ;
#9540 = DIRECTION ( 'NONE',  ( -0.000000000000000000, -1.000000000000000000, -0.000000000000000000 ) ) ;
#9541 = CARTESIAN_POINT ( 'NONE',  ( -15.00000000000000000, 8.000000000000000000, -4.000000000000000000 ) ) ;
#9542 = CARTESIAN_POINT ( 'NONE',  ( -152.0050000000000239, 6.826472737025116366, 4.959722759717898555 ) ) ;
#9543 = ORIENTED_EDGE ( 'NONE', *, *, #39131, .F. ) ;
#9544 = SURFACE_STYLE_USAGE ( .BOTH. , #41917 ) ;
#9545 = UNCERTAINTY_MEASURE_WITH_UNIT (LENGTH_MEASURE( 1.000000000000000082E-05 ), #47755, 'distance_accuracy_value', 'NONE');
#9546 = FILL_AREA_STYLE_COLOUR ( '', #27251 ) ;
#9547 = CARTESIAN_POINT ( 'NONE',  ( -7.632228543268608334, 151.9570736234661581, 2.479861379858952830 ) ) ;
#9548 = CARTESIAN_POINT ( 'NONE',  ( -5.196152422706636465, 1.107695154586736175, -9.000000000000003553 ) ) ;
#9549 = CARTESIAN_POINT ( 'NONE',  ( 7.632228543268608334, 146.3429263765338249, -2.479861379858951942 ) ) ;
#9550 = ORIENTED_EDGE ( 'NONE', *, *, #12210, .F. ) ;
#9551 =( GEOMETRIC_REPRESENTATION_CONTEXT ( 3 ) GLOBAL_UNCERTAINTY_ASSIGNED_CONTEXT ( ( #2956 ) ) GLOBAL_UNIT_ASSIGNED_CONTEXT ( ( #69313, #37692, #48228 ) ) REPRESENTATION_CONTEXT ( 'NONE', 'WORKASPACE' ) );
#9552 = VERTEX_POINT ( 'NONE', #49063 ) ;
#9553 = FACE_OUTER_BOUND ( 'NONE', #43614, .T. ) ;
#9554 = CARTESIAN_POINT ( 'NONE',  ( -70.40499999999997272, -2.607480562269069768, 8.024999999999991473 ) ) ;
#9555 = EDGE_LOOP ( 'NONE', ( #319, #51133, #25862, #12313 ) ) ;
#9556 = DIRECTION ( 'NONE',  ( 0.000000000000000000, -1.000000000000000000, 0.000000000000000000 ) ) ;
#9557 = DIRECTION ( 'NONE',  ( 0.000000000000000000, 0.000000000000000000, -1.000000000000000000 ) ) ;
#9558 = EDGE_CURVE ( 'NONE', #29573, #56578, #49366, .T. ) ;
#9559 = AXIS2_PLACEMENT_3D ( 'NONE', #11017, #63461, #15311 ) ;
#9560 = CARTESIAN_POINT ( 'NONE',  ( -124.4929263765337879, -8.102448949553174629, 5.886773742842742685 ) ) ;
#9561 = CARTESIAN_POINT ( 'NONE',  ( 0.000000000000000000, 0.000000000000000000, 0.000000000000000000 ) ) ;
#9562 = ORIENTED_EDGE ( 'NONE', *, *, #11594, .F. ) ;
#9563 = EDGE_CURVE ( 'NONE', #13981, #63556, #58843, .T. ) ;
#9564 = LINE ( 'NONE', #61580, #3138 ) ;
#9565 = CIRCLE ( 'NONE', #45532, 0.2500000000000002220 ) ;
#9566 = DIRECTION ( 'NONE',  ( 0.000000000000000000, 0.000000000000000000, 1.000000000000000000 ) ) ;
#9567 = PLANE ( 'NONE',  #64536 ) ;
#9568 = DIRECTION ( 'NONE',  ( -2.168404344971007882E-16, 0.000000000000000000, -1.000000000000000000 ) ) ;
#9569 = ADVANCED_FACE ( 'NONE', ( #28576 ), #4384, .T. ) ;
#9570 = CARTESIAN_POINT ( 'NONE',  ( -8.102448949553181734, 148.8950000000000102, -5.886773742842749790 ) ) ;
#9571 = CARTESIAN_POINT ( 'NONE',  ( -98.69499999999999318, -8.437984349512085203, 5.166775262442717831E-16 ) ) ;
#9572 = DIRECTION ( 'NONE',  ( 0.000000000000000000, -0.9396926207859082059, 0.3420201433256693790 ) ) ;
#9573 = DIRECTION ( 'NONE',  ( -0.000000000000000000, -1.000000000000000000, -0.000000000000000000 ) ) ;
#9574 = UNCERTAINTY_MEASURE_WITH_UNIT (LENGTH_MEASURE( 1.000000000000000082E-05 ), #20454, 'distance_accuracy_value', 'NONE');
#9575 = AXIS2_PLACEMENT_3D ( 'NONE', #560, #53417, #21377 ) ;
#9576 = DIRECTION ( 'NONE',  ( 1.000000000000000000, -0.000000000000000000, -1.300977106640434891E-16 ) ) ;
#9577 = ORIENTED_EDGE ( 'NONE', *, *, #28226, .T. ) ;
#9578 = CARTESIAN_POINT ( 'NONE',  ( -133.1929263765337339, -10.01517768586948698, 6.132527647946031529E-16 ) ) ;
#9579 = CARTESIAN_POINT ( 'NONE',  ( 34.99999999999999289, 99.99999999999998579, -10.00000000000000000 ) ) ;
#9580 = CARTESIAN_POINT ( 'NONE',  ( -154.0449999999999875, 7.632228543268600340, 2.479861379858949277 ) ) ;
#9581 = PRESENTATION_STYLE_ASSIGNMENT (( #56085 ) ) ;
#9582 = ADVANCED_FACE ( 'NONE', ( #2128 ), #47038, .F. ) ;
#9583 = AXIS2_PLACEMENT_3D ( 'NONE', #48943, #38736, #7375 ) ;
#9584 = LINE ( 'NONE', #24333, #39340 ) ;
#9585 =( GEOMETRIC_REPRESENTATION_CONTEXT ( 3 ) GLOBAL_UNCERTAINTY_ASSIGNED_CONTEXT ( ( #54347 ) ) GLOBAL_UNIT_ASSIGNED_CONTEXT ( ( #13982, #41096, #29809 ) ) REPRESENTATION_CONTEXT ( 'NONE', 'WORKASPACE' ) );
#9586 = DIRECTION ( 'NONE',  ( 0.000000000000000000, 0.000000000000000000, 1.000000000000000000 ) ) ;
#9587 = ORIENTED_EDGE ( 'NONE', *, *, #5459, .F. ) ;
#9588 = EDGE_LOOP ( 'NONE', ( #23197, #17596, #12046 ) ) ;
#9589 =( GEOMETRIC_REPRESENTATION_CONTEXT ( 3 ) GLOBAL_UNCERTAINTY_ASSIGNED_CONTEXT ( ( #6731 ) ) GLOBAL_UNIT_ASSIGNED_CONTEXT ( ( #25907, #4436, #152 ) ) REPRESENTATION_CONTEXT ( 'NONE', 'WORKASPACE' ) );
#9590 = DIRECTION ( 'NONE',  ( 0.000000000000000000, 1.000000000000000000, 0.000000000000000000 ) ) ;
#9591 = UNCERTAINTY_MEASURE_WITH_UNIT (LENGTH_MEASURE( 1.000000000000000082E-05 ), #46047, 'distance_accuracy_value', 'NONE');
#9592 = CARTESIAN_POINT ( 'NONE',  ( -51.50000000000000000, -2.024042244987997205E-14, -10.49999999999999822 ) ) ;
#9593 = CARTESIAN_POINT ( 'NONE',  ( -45.00000000000000000, 9.581381838473474133, 6.370847823861928383 ) ) ;
#9594 = CARTESIAN_POINT ( 'NONE',  ( 109.0067032876572171, 0.9999999999999991118, 19.20378738324562917 ) ) ;
#9595 = FILL_AREA_STYLE_COLOUR ( '', #56696 ) ;
#9596 = ORIENTED_EDGE ( 'NONE', *, *, #64102, .F. ) ;
#9597 = CARTESIAN_POINT ( 'NONE',  ( -152.3050000000000068, 8.437984349512086979, -1.550032578732815448E-15 ) ) ;
#9598 = VECTOR ( 'NONE', #68325, 1000.000000000000000 ) ;
#9599 = ORIENTED_EDGE ( 'NONE', *, *, #21765, .F. ) ;
#9600 = CARTESIAN_POINT ( 'NONE',  ( 5.885195493260862776, 3.806542393196805651, -4.285986713106759716E-16 ) ) ;
#9601 = FILL_AREA_STYLE_COLOUR ( '', #67987 ) ;
#9602 = ORIENTED_EDGE ( 'NONE', *, *, #68459, .F. ) ;
#9603 = EDGE_CURVE ( 'NONE', #42377, #39893, #22987, .T. ) ;
#9604 = CARTESIAN_POINT ( 'NONE',  ( 74.89452121010485541, 13.00000000000000178, -66.39042820928574429 ) ) ;
#9605 = CARTESIAN_POINT ( 'NONE',  ( 0.000000000000000000, 118.4449999999999932, -9.525000000000000355 ) ) ;
#9606 = ORIENTED_EDGE ( 'NONE', *, *, #16783, .F. ) ;
#9607 = DIRECTION ( 'NONE',  ( -1.000000000000000000, 0.000000000000000000, 0.000000000000000000 ) ) ;
#9608 = CARTESIAN_POINT ( 'NONE',  ( -9.058813317711337021, 123.1549999999999869, -2.943386871421374895 ) ) ;
#9609 = CARTESIAN_POINT ( 'NONE',  ( -69.35499999999998977, -4.716976649647093289, -6.492361379858945902 ) ) ;
#9610 = AXIS2_PLACEMENT_3D ( 'NONE', #14228, #20177, #30728 ) ;
#9611 = ORIENTED_EDGE ( 'NONE', *, *, #35763, .T. ) ;
#9612 = CARTESIAN_POINT ( 'NONE',  ( 8.102448949553183510, 140.1049999999999898, -5.886773742842746238 ) ) ;
#9613 = UNCERTAINTY_MEASURE_WITH_UNIT (LENGTH_MEASURE( 1.000000000000000082E-05 ), #60216, 'distance_accuracy_value', 'NONE');
#9614 = CYLINDRICAL_SURFACE ( 'NONE', #29887, 9.524999999999991473 ) ;
#9615 =( LENGTH_UNIT ( ) NAMED_UNIT ( * ) SI_UNIT ( .MILLI., .METRE. ) );
#9616 =( NAMED_UNIT ( * ) PLANE_ANGLE_UNIT ( ) SI_UNIT ( $, .RADIAN. ) );
#9617 =( LENGTH_UNIT ( ) NAMED_UNIT ( * ) SI_UNIT ( .MILLI., .METRE. ) );
#9618 = ORIENTED_EDGE ( 'NONE', *, *, #42500, .F. ) ;
#9619 = CARTESIAN_POINT ( 'NONE',  ( -9.250000000000003553, 25.24999999999998934, 3.750000000000000000 ) ) ;
#9620 = CARTESIAN_POINT ( 'NONE',  ( 23.71231517720798010, 117.9999999999999716, -7.000000000000000000 ) ) ;
#9621 = CARTESIAN_POINT ( 'NONE',  ( -22.50000000000000711, 36.75000000000000000, 3.750000000000000000 ) ) ;
#9622 = CARTESIAN_POINT ( 'NONE',  ( -47.99499999999998323, -6.826472737025115478, 4.959722759717900331 ) ) ;
#9623 = VERTEX_POINT ( 'NONE', #20101 ) ;
#9624 = CARTESIAN_POINT ( 'NONE',  ( 7.239872073591122614, 111.2187526276816669, 5.042250455018136179 ) ) ;
#9625 = CARTESIAN_POINT ( 'NONE',  ( 26.00000000000001776, 15.00000000000000000, -34.49999999999999289 ) ) ;
#9626 = ORIENTED_EDGE ( 'NONE', *, *, #69129, .F. ) ;
#9627 = PLANE ( 'NONE',  #536 ) ;
#9628 = LINE ( 'NONE', #8911, #13032 ) ;
#9629 = VERTEX_POINT ( 'NONE', #34912 ) ;
#9630 = CARTESIAN_POINT ( 'NONE',  ( -2.755190520427473366, -7.000000000000002665, 0.4949495880430740402 ) ) ;
#9631 = PRESENTATION_LAYER_ASSIGNMENT (  '', '', ( #39966 ) ) ;
#9632 = CARTESIAN_POINT ( 'NONE',  ( -99.65499999999998693, -7.632228543268600340, -2.479861379858950166 ) ) ;
#9633 = ORIENTED_EDGE ( 'NONE', *, *, #18741, .F. ) ;
#9634 = CARTESIAN_POINT ( 'NONE',  ( 0.000000000000000000, 14.00000000000000000, -80.00402776293826435 ) ) ;
#9635 = EDGE_CURVE ( 'NONE', #49320, #64348, #53984, .T. ) ;
#9636 =( LENGTH_UNIT ( ) NAMED_UNIT ( * ) SI_UNIT ( .MILLI., .METRE. ) );
#9637 = VECTOR ( 'NONE', #18823, 1000.000000000000114 ) ;
#9638 = CARTESIAN_POINT ( 'NONE',  ( -129.6570736234661751, 9.058813317711329915, 2.943386871421369566 ) ) ;
#9639 = VECTOR ( 'NONE', #54742, 1000.000000000000114 ) ;
#9640 = SURFACE_SIDE_STYLE ('',( #25441 ) ) ;
#9641 = CARTESIAN_POINT ( 'NONE',  ( -73.70707362346615810, -3.094860106618431139, -9.524999999999991473 ) ) ;
#9642 = CARTESIAN_POINT ( 'NONE',  ( -160.5570736234661808, -1.166476076187852838E-15, -9.524999999999991473 ) ) ;
#9643 = VERTEX_POINT ( 'NONE', #66941 ) ;
#9644 = DIRECTION ( 'NONE',  ( 0.000000000000000000, -1.000000000000000000, 0.000000000000000000 ) ) ;
#9645 = CARTESIAN_POINT ( 'NONE',  ( -15.00000000000000000, -10.90871211463571200, 5.000000000000000000 ) ) ;
#9647 = CARTESIAN_POINT ( 'NONE',  ( -8.082903768654761123, 1.417096231345241097, -1.759977097422839922E-15 ) ) ;
#9646 = LINE ( 'NONE', #31062, #13346 ) ;
#9648 = CIRCLE ( 'NONE', #18621, 7.500000000000000000 ) ;
#9649 = CARTESIAN_POINT ( 'NONE',  ( -114.9549999999999841, -7.632228543268599452, 2.479861379858951054 ) ) ;
#9650 = EDGE_CURVE ( 'NONE', #6742, #34526, #14165, .T. ) ;
#9651 =( NAMED_UNIT ( * ) PLANE_ANGLE_UNIT ( ) SI_UNIT ( $, .RADIAN. ) );
#9652 = CARTESIAN_POINT ( 'NONE',  ( -5.598654528085808657, 119.6449999999999818, 7.705886871421373741 ) ) ;
#9653 = CARTESIAN_POINT ( 'NONE',  ( -123.7449999999999903, 4.716976649647094177, 6.492361379858945902 ) ) ;
#9654 = CIRCLE ( 'NONE', #41312, 13.00000000000000178 ) ;
#9655 = EDGE_CURVE ( 'NONE', #46540, #40174, #52167, .T. ) ;
#9656 = FACE_OUTER_BOUND ( 'NONE', #30338, .T. ) ;
#9657 = VECTOR ( 'NONE', #35548, 1000.000000000000000 ) ;
#9658 =( BOUNDED_CURVE ( )  B_SPLINE_CURVE ( 2, ( #59101, #1335, #44011, #33074, #11951, #43663, #22513, #33408, #27061, #26720, #58762 ),
 .UNSPECIFIED., .F., .F. ) 
 B_SPLINE_CURVE_WITH_KNOTS ( ( 3, 2, 2, 2, 2, 3 ),
 ( 0.4021739130434686116, 0.4043478260869468044, 0.4065217391304249972, 0.4086956521739032455, 0.4108695652173814383, 0.4130434782608596311 ),
 .UNSPECIFIED. ) 
 CURVE ( )  GEOMETRIC_REPRESENTATION_ITEM ( )  RATIONAL_B_SPLINE_CURVE ( ( 1.000000000000217382, 0.9510565162949360385, 1.000000000000000000, 0.9510565162951535312, 1.000000000000000000, 0.9510565162951535312, 1.000000000000000000, 0.9510565162951535312, 1.000000000000000000, 0.9510565162953772411, 0.9999999999997762901 ) ) 
 REPRESENTATION_ITEM ( '' )  );
#9659 = DIRECTION ( 'NONE',  ( 0.000000000000000000, 1.000000000000000000, 0.000000000000000000 ) ) ;
#9660 = DIRECTION ( 'NONE',  ( 0.000000000000000000, 0.000000000000000000, -1.000000000000000000 ) ) ;
#9661 = EDGE_CURVE ( 'NONE', #51304, #67697, #25396, .T. ) ;
#9662 = ORIENTED_EDGE ( 'NONE', *, *, #12925, .F. ) ;
#9663 = DIRECTION ( 'NONE',  ( 0.7833176619561879050, -0.6216216216216192691, 0.000000000000000000 ) ) ;
#9664 = VECTOR ( 'NONE', #28903, 1000.000000000000000 ) ;
#9665 = CARTESIAN_POINT ( 'NONE',  ( -161.5429263765338135, 9.058813317711329915, 2.943386871421369566 ) ) ;
#9666 = EDGE_CURVE ( 'NONE', #12229, #53118, #56012, .T. ) ;
#9667 = CARTESIAN_POINT ( 'NONE',  ( -4.716976649647098618, 125.2570736234661695, 6.492361379858953008 ) ) ;
#9668 = CARTESIAN_POINT ( 'NONE',  ( -20.06812647026248086, 114.9888238951376991, -10.44321692355803144 ) ) ;
#9669 = CARTESIAN_POINT ( 'NONE',  ( 2.000000000000009326, 50.00000000000000000, -54.99999999999998579 ) ) ;
#9670 = ORIENTED_EDGE ( 'NONE', *, *, #31348, .F. ) ;
#9671 = CARTESIAN_POINT ( 'NONE',  ( -87.44292637653380496, -1.166476076187852838E-15, -9.524999999999991473 ) ) ;
#9672 = CONTEXT_DEPENDENT_SHAPE_REPRESENTATION ( #36119, #52966 ) ;
#9673 =( NAMED_UNIT ( * ) SI_UNIT ( $, .STERADIAN. ) SOLID_ANGLE_UNIT ( ) );
#9674 = CARTESIAN_POINT ( 'NONE',  ( 10.42000000000000348, -1.224646799147353651E-15, 12.50000000000000000 ) ) ;
#9675 = AXIS2_PLACEMENT_3D ( 'NONE', #47382, #36108, #57545 ) ;
#9676 =( NAMED_UNIT ( * ) PLANE_ANGLE_UNIT ( ) SI_UNIT ( $, .RADIAN. ) );
#9677 = DIRECTION ( 'NONE',  ( 0.000000000000000000, 0.000000000000000000, 1.000000000000000000 ) ) ;
#9678 = PRESENTATION_LAYER_ASSIGNMENT (  '', '', ( #16423 ) ) ;
#9679 = CARTESIAN_POINT ( 'NONE',  ( -176.1550000000000011, 7.632228543268600340, 2.479861379858949277 ) ) ;
#9680 = ORIENTED_EDGE ( 'NONE', *, *, #7315, .T. ) ;
#9681 = CARTESIAN_POINT ( 'NONE',  ( 0.000000000000000000, -2.500000000000000000, 0.000000000000000000 ) ) ;
#9682 = FACE_OUTER_BOUND ( 'NONE', #28906, .T. ) ;
#9684 = ORIENTED_EDGE ( 'NONE', *, *, #22959, .T. ) ;
#9683 = AXIS2_PLACEMENT_3D ( 'NONE', #36066, #20566, #42083 ) ;
#9685 = CIRCLE ( 'NONE', #56863, 1.000000000000000888 ) ;
#9686 = CARTESIAN_POINT ( 'NONE',  ( 30.99999999999999289, 5.000000000000000000, 37.00402776293829277 ) ) ;
#9687 = AXIS2_PLACEMENT_3D ( 'NONE', #18530, #6922, #17835 ) ;
#9688 = DIRECTION ( 'NONE',  ( 0.000000000000000000, 1.000000000000000000, 0.000000000000000000 ) ) ;
#9689 = CARTESIAN_POINT ( 'NONE',  ( 8.437984349512095861, 144.3070736234661240, 1.550032578732817026E-15 ) ) ;
#9690 =( NAMED_UNIT ( * ) PLANE_ANGLE_UNIT ( ) SI_UNIT ( $, .RADIAN. ) );
#9691 = ORIENTED_EDGE ( 'NONE', *, *, #37719, .F. ) ;
#9692 = CARTESIAN_POINT ( 'NONE',  ( -98.90499999999998693, 2.607480562269069324, -8.024999999999993250 ) ) ;
#9693 = UNCERTAINTY_MEASURE_WITH_UNIT (LENGTH_MEASURE( 1.000000000000000082E-05 ), #15784, 'distance_accuracy_value', 'NONE');
#9694 = CARTESIAN_POINT ( 'NONE',  ( 33.00000000000000711, 15.00000000000000000, -36.50000000000000000 ) ) ;
#9695 = ORIENTED_EDGE ( 'NONE', *, *, #68419, .T. ) ;
#9696 = VECTOR ( 'NONE', #30846, 1000.000000000000000 ) ;
#9697 = CARTESIAN_POINT ( 'NONE',  ( 0.000000000000000000, 143.9429263765338192, -8.025000000000000355 ) ) ;
#9698 = CARTESIAN_POINT ( 'NONE',  ( -59.62249556327051891, -7.581530822753633991, -0.08527172969607607622 ) ) ;
#9699 = MECHANICAL_DESIGN_GEOMETRIC_PRESENTATION_REPRESENTATION (  '', ( #55720 ), #42160 ) ;
#9700 = ORIENTED_EDGE ( 'NONE', *, *, #52765, .T. ) ;
#9701 = CARTESIAN_POINT ( 'NONE',  ( -74.69499999999997897, -8.437984349512085203, 5.166775262442717831E-16 ) ) ;
#9702 = VERTEX_POINT ( 'NONE', #67623 ) ;
#9703 = FACE_BOUND ( 'NONE', #53458, .T. ) ;
#9704 = CARTESIAN_POINT ( 'NONE',  ( -120.2070736234669397, 3.094860106631407426, 9.524999999990566124 ) ) ;
#9705 = ORIENTED_EDGE ( 'NONE', *, *, #23823, .F. ) ;
#9706 = CARTESIAN_POINT ( 'NONE',  ( -4.250000000000001776, 21.99999999999998579, -3.750000000000000000 ) ) ;
#9707 = FILL_AREA_STYLE ('',( #31464 ) ) ;
#9708 = SURFACE_SIDE_STYLE ('',( #63498 ) ) ;
#9709 = SURFACE_STYLE_FILL_AREA ( #57527 ) ;
#9710 = ORIENTED_EDGE ( 'NONE', *, *, #33973, .F. ) ;
#9711 = DIRECTION ( 'NONE',  ( -1.000000000000000000, 0.000000000000000000, 0.000000000000000000 ) ) ;
#9713 = ORIENTED_EDGE ( 'NONE', *, *, #13027, .T. ) ;
#9712 = ADVANCED_FACE ( 'NONE', ( #19425 ), #8839, .T. ) ;
#9714 = CARTESIAN_POINT ( 'NONE',  ( 72.00000000000000000, 36.32520566882265456, 7.000000000000000000 ) ) ;
#9715 = DIRECTION ( 'NONE',  ( 0.000000000000000000, 0.000000000000000000, 1.000000000000000000 ) ) ;
#9716 = SURFACE_STYLE_USAGE ( .BOTH. , #68802 ) ;
#9717 = CARTESIAN_POINT ( 'NONE',  ( -164.7570736234661695, -5.598654528085801552, 7.705886871421367523 ) ) ;
#9718 = CARTESIAN_POINT ( 'NONE',  ( -5.598654528085806881, 121.7449999999999903, -7.705886871421374629 ) ) ;
#9719 = ADVANCED_FACE ( 'NONE', ( #41270 ), #35968, .T. ) ;
#9720 = CARTESIAN_POINT ( 'NONE',  ( -101.1570736234661609, -9.058813317711329915, -2.943386871421370898 ) ) ;
#9721 = AXIS2_PLACEMENT_3D ( 'NONE', #24647, #46165, #67589 ) ;
#9722 = EDGE_CURVE ( 'NONE', #51168, #5413, #31351, .T. ) ;
#9723 = PRESENTATION_STYLE_ASSIGNMENT (( #42113 ) ) ;
#9724 = CARTESIAN_POINT ( 'NONE',  ( -65.60707362346616378, -8.102448949553174629, 5.886773742842742685 ) ) ;
#9725 = PRODUCT_DEFINITION_SHAPE ( 'NONE', 'NONE',  #1190 ) ;
#9726 = ORIENTED_EDGE ( 'NONE', *, *, #55771, .T. ) ;
#9727 = FILL_AREA_STYLE ('',( #20954 ) ) ;
#9728 = EDGE_CURVE ( 'NONE', #24181, #39125, #53706, .T. ) ;
#9730 = CARTESIAN_POINT ( 'NONE',  ( -114.6570736234661751, 9.058813317711329915, 2.943386871421369566 ) ) ;
#9729 = CARTESIAN_POINT ( 'NONE',  ( 44.36184162591896296, 10.11502268137275351, 3.500000000000000000 ) ) ;
#9731 = CONICAL_SURFACE ( 'NONE', #23162, 4.999999999999997335, 0.7853981633974587151 ) ;
#9732 = CARTESIAN_POINT ( 'NONE',  ( -137.6049999999999329, 6.826472737025113702, -4.959722759717902107 ) ) ;
#9733 = EDGE_CURVE ( 'NONE', #17965, #32986, #4368, .T. ) ;
#9734 = PRESENTATION_STYLE_ASSIGNMENT (( #35049 ) ) ;
#9735 = PRESENTATION_LAYER_ASSIGNMENT (  '', '', ( #35584 ) ) ;
#9736 = DIRECTION ( 'NONE',  ( 0.000000000000000000, 0.000000000000000000, 1.000000000000000000 ) ) ;
#9737 = CARTESIAN_POINT ( 'NONE',  ( -150.7449999999999761, 4.716976649647094177, 6.492361379858945902 ) ) ;
#9738 = ADVANCED_FACE ( 'NONE', ( #53525 ), #57122, .T. ) ;
#9739 = AXIS2_PLACEMENT_3D ( 'NONE', #18992, #50014, #39470 ) ;
#9740 = CARTESIAN_POINT ( 'NONE',  ( -150.5949999999999704, 2.607480562269072433, 8.024999999999991473 ) ) ;
#9741 = EDGE_LOOP ( 'NONE', ( #34080, #61254 ) ) ;
#9742 = DIRECTION ( 'NONE',  ( -0.000000000000000000, -1.000000000000000000, -0.000000000000000000 ) ) ;
#9743 = DIRECTION ( 'NONE',  ( -0.000000000000000000, -0.000000000000000000, -1.000000000000000000 ) ) ;
#9744 = EDGE_CURVE ( 'NONE', #48456, #62990, #57774, .T. ) ;
#9745 = CARTESIAN_POINT ( 'NONE',  ( -62.90499999999997982, 2.607480562269068880, -8.024999999999993250 ) ) ;
#9746 = CARTESIAN_POINT ( 'NONE',  ( -1.166476076187854022E-15, 154.0550000000000068, 9.525000000000000355 ) ) ;
#9747 = CARTESIAN_POINT ( 'NONE',  ( -51.89292637653380069, -8.102448949553174629, -5.886773742842741797 ) ) ;
#9748 = LINE ( 'NONE', #54005, #63465 ) ;
#9749 = SURFACE_STYLE_USAGE ( .BOTH. , #57930 ) ;
#9750 = DIRECTION ( 'NONE',  ( -4.528264053928432009E-17, -2.220446049250312588E-16, -1.000000000000000000 ) ) ;
#9751 = SPHERICAL_SURFACE ( 'NONE', #30404, 0.5000000000000000000 ) ;
#9752 = CARTESIAN_POINT ( 'NONE',  ( -88.85707362346617799, -5.598654528085803328, -7.705886871421366635 ) ) ;
#9753 = CARTESIAN_POINT ( 'NONE',  ( 8.000000000000001776, 31.24999999999998579, -4.000000000000000000 ) ) ;
#9754 = DIRECTION ( 'NONE',  ( 0.9704308468600219006, -0.2413793103448194921, 0.000000000000000000 ) ) ;
#9755 = LINE ( 'NONE', #36141, #17318 ) ;
#9756 = CARTESIAN_POINT ( 'NONE',  ( 0.000000000000000000, 0.000000000000000000, 0.2500000000000011102 ) ) ;
#9757 = VERTEX_POINT ( 'NONE', #4255 ) ;
#9758 = ORIENTED_EDGE ( 'NONE', *, *, #23217, .T. ) ;
#9759 = SURFACE_STYLE_USAGE ( .BOTH. , #63206 ) ;
#9760 = EDGE_CURVE ( 'NONE', #13259, #65467, #20009, .T. ) ;
#9761 = DIRECTION ( 'NONE',  ( -1.000000000000000000, -0.000000000000000000, -0.000000000000000000 ) ) ;
#9762 = CARTESIAN_POINT ( 'NONE',  ( 62.24999999999998579, 33.74999999999999289, 3.750000000000000000 ) ) ;
#9763 = SURFACE_STYLE_FILL_AREA ( #31172 ) ;
#9764 = ORIENTED_EDGE ( 'NONE', *, *, #50203, .T. ) ;
#9765 = ORIENTED_EDGE ( 'NONE', *, *, #10519, .T. ) ;
#9766 = STYLED_ITEM ( 'NONE', ( #26865 ), #65246 ) ;
#9767 = CARTESIAN_POINT ( 'NONE',  ( -72.00000000000000000, 14.49137674618942562, -7.500000000000000000 ) ) ;
#9768 = DIRECTION ( 'NONE',  ( 1.445602896647337931E-16, -1.000000000000000000, -0.000000000000000000 ) ) ;
#9769 = ORIENTED_EDGE ( 'NONE', *, *, #12980, .F. ) ;
#9770 = CARTESIAN_POINT ( 'NONE',  ( 8.102448949553181734, 115.5049999999999812, 5.886773742842750679 ) ) ;
#9771 = CARTESIAN_POINT ( 'NONE',  ( 3.542752237027634976, 1.835478060177116566, -9.000000000000007105 ) ) ;
#9772 = STYLED_ITEM ( 'NONE', ( #12504 ), #3359 ) ;
#9773 = CARTESIAN_POINT ( 'NONE',  ( 34.99999999999992895, 113.4999999999999858, -7.500000000000000000 ) ) ;
#9774 = FILL_AREA_STYLE_COLOUR ( '', #53175 ) ;
#9775 = CARTESIAN_POINT ( 'NONE',  ( -96.29500000000000171, -2.607480562269069768, 8.024999999999991473 ) ) ;
#9776 = ORIENTED_EDGE ( 'NONE', *, *, #32031, .T. ) ;
#9777 = FACE_OUTER_BOUND ( 'NONE', #20860, .T. ) ;
#9778 = PRESENTATION_STYLE_ASSIGNMENT (( #36545 ) ) ;
#9779 = ORIENTED_EDGE ( 'NONE', *, *, #5425, .T. ) ;
#9780 = CARTESIAN_POINT ( 'NONE',  ( -2.607480562269073765, 153.0929263765338249, -8.025000000000000355 ) ) ;
#9781 = CYLINDRICAL_SURFACE ( 'NONE', #34645, 1.000000000000000888 ) ;
#9782 = FILL_AREA_STYLE_COLOUR ( '', #1424 ) ;
#9783 = AXIS2_PLACEMENT_3D ( 'NONE', #45455, #65827, #23594 ) ;
#9784 = DIRECTION ( 'NONE',  ( 0.000000000000000000, 0.000000000000000000, 1.000000000000000000 ) ) ;
#9785 = EDGE_CURVE ( 'NONE', #58314, #11393, #5652, .T. ) ;
#9786 = ORIENTED_EDGE ( 'NONE', *, *, #69206, .F. ) ;
#9787 = CARTESIAN_POINT ( 'NONE',  ( 20.56511377093078252, 115.3174848394179435, -10.00000000000000000 ) ) ;
#9788 = ORIENTED_EDGE ( 'NONE', *, *, #5312, .T. ) ;
#9789 = CARTESIAN_POINT ( 'NONE',  ( 20.56323889998346388, 115.3189275942976337, 10.00000000000000000 ) ) ;
#9790 = DIRECTION ( 'NONE',  ( -1.000000000000000000, 0.000000000000000000, 0.000000000000000000 ) ) ;
#9791 =( LENGTH_UNIT ( ) NAMED_UNIT ( * ) SI_UNIT ( .MILLI., .METRE. ) );
#9792 = DIRECTION ( 'NONE',  ( 0.000000000000000000, 0.000000000000000000, -1.000000000000000000 ) ) ;
#9793 = DIRECTION ( 'NONE',  ( 0.000000000000000000, 0.000000000000000000, 1.000000000000000000 ) ) ;
#9794 = CARTESIAN_POINT ( 'NONE',  ( 5.590169943749474513, 4.999999999999999112, 0.000000000000000000 ) ) ;
#9795 = EDGE_CURVE ( 'NONE', #8081, #23178, #41976, .T. ) ;
#9796 = CARTESIAN_POINT ( 'NONE',  ( 10.99999999999999645, 11.99999999999999289, 4.000000000000000000 ) ) ;
#9797 = CARTESIAN_POINT ( 'NONE',  ( 3.673940397442060361E-16, 2.000000000000000444, -3.000000000000000444 ) ) ;
#9798 = CARTESIAN_POINT ( 'NONE',  ( -5.196152422706634688, 9.000000000000008882, 1.392304845413263159 ) ) ;
#9799 = LINE ( 'NONE', #69226, #59353 ) ;
#9800 = ORIENTED_EDGE ( 'NONE', *, *, #24526, .T. ) ;
#9801 = ORIENTED_EDGE ( 'NONE', *, *, #1245, .T. ) ;
#9802 = CARTESIAN_POINT ( 'NONE',  ( -60.00000000000000000, -2.024042244987997205E-14, -12.00000000000000000 ) ) ;
#9803 = DIRECTION ( 'NONE',  ( 1.000000000000000000, 0.000000000000000000, 0.000000000000000000 ) ) ;
#9804 = CARTESIAN_POINT ( 'NONE',  ( -182.3929263765338078, 8.102448949553176405, 5.886773742842740909 ) ) ;
#9805 = CARTESIAN_POINT ( 'NONE',  ( 6.826472737025119919, 114.0070736234661553, 4.959722759717908325 ) ) ;
#9806 = ORIENTED_EDGE ( 'NONE', *, *, #41330, .T. ) ;
#9807 = PLANE ( 'NONE',  #49516 ) ;
#9808 = CARTESIAN_POINT ( 'NONE',  ( -181.5550000000000068, 0.000000000000000000, 8.024999999999991473 ) ) ;
#9809 = CARTESIAN_POINT ( 'NONE',  ( -8.252730563585672030, 2.464278740834326520, 3.705851362693083573 ) ) ;
#9810 = CYLINDRICAL_SURFACE ( 'NONE', #10024, 1.000000000000000888 ) ;
#9811 = CARTESIAN_POINT ( 'NONE',  ( -179.0949999999999704, -2.607480562269071545, -8.024999999999991473 ) ) ;
#9812 = EDGE_CURVE ( 'NONE', #14179, #13223, #52850, .T. ) ;
#9813 = CARTESIAN_POINT ( 'NONE',  ( -180.8949999999999818, 6.826472737025115478, 4.959722759717899443 ) ) ;
#9814 = ORIENTED_EDGE ( 'NONE', *, *, #48419, .F. ) ;
#9815 = SURFACE_STYLE_USAGE ( .BOTH. , #26974 ) ;
#9816 = EDGE_CURVE ( 'NONE', #64678, #66633, #47616, .T. ) ;
#9817 = DIRECTION ( 'NONE',  ( 0.000000000000000000, 0.000000000000000000, -1.000000000000000000 ) ) ;
#9818 = CARTESIAN_POINT ( 'NONE',  ( -95.15499999999998693, 7.632228543268600340, 2.479861379858949277 ) ) ;
#9819 = FACE_OUTER_BOUND ( 'NONE', #58061, .T. ) ;
#9820 = CYLINDRICAL_SURFACE ( 'NONE', #21447, 3.499999999999999556 ) ;
#9821 = SURFACE_STYLE_USAGE ( .BOTH. , #13328 ) ;
#9822 = CARTESIAN_POINT ( 'NONE',  ( -94.64499999999999602, 4.716976649647091513, -6.492361379858946790 ) ) ;
#9823 = CARTESIAN_POINT ( 'NONE',  ( 9.058813317711337021, 130.6550000000000011, 2.943386871421375783 ) ) ;
#9824 = AXIS2_PLACEMENT_3D ( 'NONE', #53131, #36286, #4917 ) ;
#9825 = CARTESIAN_POINT ( 'NONE',  ( -64.04499999999998749, 7.632228543268600340, 2.479861379858949277 ) ) ;
#9826 = CARTESIAN_POINT ( 'NONE',  ( -58.75000000000000000, -13.99999999999999822, 15.00000000000000178 ) ) ;
#9827 = CARTESIAN_POINT ( 'NONE',  ( 0.000000000000000000, -7.000000000000000888, 0.000000000000000000 ) ) ;
#9828 = FILL_AREA_STYLE ('',( #5204 ) ) ;
#9829 = FACE_OUTER_BOUND ( 'NONE', #59119, .T. ) ;
#9830 = ORIENTED_EDGE ( 'NONE', *, *, #1612, .F. ) ;
#9831 = CIRCLE ( 'NONE', #49152, 0.2500000000000002220 ) ;
#9832 = CARTESIAN_POINT ( 'NONE',  ( 107.0858988931383493, 0.000000000000000000, 16.89933289725615850 ) ) ;
#9833 = PRESENTATION_STYLE_ASSIGNMENT (( #21062 ) ) ;
#9834 = DIRECTION ( 'NONE',  ( 0.000000000000000000, 1.000000000000000000, -0.000000000000000000 ) ) ;
#9835 = VERTEX_POINT ( 'NONE', #26429 ) ;
#9836 = ORIENTED_EDGE ( 'NONE', *, *, #38638, .T. ) ;
#9837 = CARTESIAN_POINT ( 'NONE',  ( -45.91547277936962956, 9.430195807687216103, -6.000000000000000000 ) ) ;
#9838 = CARTESIAN_POINT ( 'NONE',  ( -15.98999599679679839, 117.4999999999999716, 10.00000000000000000 ) ) ;
#9839 = ADVANCED_FACE ( 'NONE', ( #15918 ), #43702, .T. ) ;
#9840 = CARTESIAN_POINT ( 'NONE',  ( -2.607480562268991608, 148.2929263765338703, 8.025000000000060751 ) ) ;
#9841 = CARTESIAN_POINT ( 'NONE',  ( -74.99999999999998579, 146.4999999999999716, 7.500000000000000000 ) ) ;
#9842 = FACE_OUTER_BOUND ( 'NONE', #14780, .T. ) ;
#9843 = CARTESIAN_POINT ( 'NONE',  ( -8.920833891111501046, -2.231456886122025640, 2.548662454712524283 ) ) ;
#9844 = ORIENTED_EDGE ( 'NONE', *, *, #36154, .F. ) ;
#9845 = CARTESIAN_POINT ( 'NONE',  ( -118.8549999999999898, 4.716976649647094177, 6.492361379858945902 ) ) ;
#9846 = ORIENTED_EDGE ( 'NONE', *, *, #24499, .T. ) ;
#9847 = DIRECTION ( 'NONE',  ( 0.000000000000000000, 0.7071067811865517916, 0.7071067811865431318 ) ) ;
#9848 = CARTESIAN_POINT ( 'NONE',  ( 21.02379604162863913, 114.4999999999999574, -10.00000000000000000 ) ) ;
#9849 = ORIENTED_EDGE ( 'NONE', *, *, #65370, .T. ) ;
#9850 = FILL_AREA_STYLE ('',( #10537 ) ) ;
#9851 = EDGE_LOOP ( 'NONE', ( #4970, #67115, #30222, #46798 ) ) ;
#9852 = CARTESIAN_POINT ( 'NONE',  ( 8.690363669209105524, 2.361802048420730493, 2.947848588679143234 ) ) ;
#9853 = CARTESIAN_POINT ( 'NONE',  ( -5.598654528085806881, 148.7449999999999761, -7.705886871421374629 ) ) ;
#9854 =( NAMED_UNIT ( * ) PLANE_ANGLE_UNIT ( ) SI_UNIT ( $, .RADIAN. ) );
#9855 = VERTEX_POINT ( 'NONE', #42660 ) ;
#9856 = EDGE_CURVE ( 'NONE', #41276, #28244, #38072, .T. ) ;
#9857 =( NAMED_UNIT ( * ) SI_UNIT ( $, .STERADIAN. ) SOLID_ANGLE_UNIT ( ) );
#9858 = CARTESIAN_POINT ( 'NONE',  ( -1.166476076187854022E-15, 151.0550000000000068, 9.525000000000000355 ) ) ;
#9859 = CARTESIAN_POINT ( 'NONE',  ( 30.25000000000000711, 18.74999999999997868, -4.000000000000000000 ) ) ;
#9860 = ORIENTED_EDGE ( 'NONE', *, *, #17277, .T. ) ;
#9861 = CARTESIAN_POINT ( 'NONE',  ( 4.716976649647096842, 124.7429263765338163, 6.492361379858953896 ) ) ;
#9862 = CARTESIAN_POINT ( 'NONE',  ( 3.000000000000002665, 34.36176364315826248, -80.00402776293826435 ) ) ;
#9863 = CARTESIAN_POINT ( 'NONE',  ( -46.70707362346617941, -3.094860106618431139, -9.524999999999991473 ) ) ;
#9865 = CARTESIAN_POINT ( 'NONE',  ( -195.0000000000000000, 1.166476076187852838E-15, -9.524999999999991473 ) ) ;
#9864 = AXIS2_PLACEMENT_3D ( 'NONE', #69212, #42184, #25923 ) ;
#9866 = VECTOR ( 'NONE', #13309, 1000.000000000000000 ) ;
#9867 = EDGE_CURVE ( 'NONE', #9629, #45776, #42562, .T. ) ;
#9868 =( LENGTH_UNIT ( ) NAMED_UNIT ( * ) SI_UNIT ( .MILLI., .METRE. ) );
#9869 = FILL_AREA_STYLE_COLOUR ( '', #17534 ) ;
#9870 = EDGE_CURVE ( 'NONE', #17642, #61023, #32752, .T. ) ;
#9871 = VERTEX_POINT ( 'NONE', #39455 ) ;
#9872 = CYLINDRICAL_SURFACE ( 'NONE', #7121, 8.025000000000000355 ) ;
#9873 = ORIENTED_EDGE ( 'NONE', *, *, #37497, .T. ) ;
#9874 = CARTESIAN_POINT ( 'NONE',  ( -54.59292637653378222, -3.094860106618431139, -9.524999999999991473 ) ) ;
#9875 = SURFACE_STYLE_FILL_AREA ( #57005 ) ;
#9876 = CARTESIAN_POINT ( 'NONE',  ( 23.21231517720797655, 117.9999999999999716, -7.500000000000000000 ) ) ;
#9877 = CARTESIAN_POINT ( 'NONE',  ( -155.9049999999999443, 2.607480562269068880, -8.024999999999993250 ) ) ;
#9878 = ORIENTED_EDGE ( 'NONE', *, *, #57912, .T. ) ;
#9879 = ADVANCED_FACE ( 'NONE', ( #6019 ), #55597, .F. ) ;
#9880 = CARTESIAN_POINT ( 'NONE',  ( -74.99999999999998579, 50.00000000000000000, -6.500000000000000000 ) ) ;
#9881 = ADVANCED_FACE ( 'NONE', ( #7422 ), #33448, .T. ) ;
#9882 = CARTESIAN_POINT ( 'NONE',  ( -5.185928986913077132, -5.017707510222358280, 0.2088670156639313991 ) ) ;
#9883 = CARTESIAN_POINT ( 'NONE',  ( -7.731910350068054619E-16, -6.500000000000000888, 3.000000000000000000 ) ) ;
#9884 = CARTESIAN_POINT ( 'NONE',  ( 2.311115933264683462E-31, -6.500000000000000888, 3.000000000000002665 ) ) ;
#9885 = SURFACE_STYLE_USAGE ( .BOTH. , #31301 ) ;
#9886 = ORIENTED_EDGE ( 'NONE', *, *, #16377, .F. ) ;
#9887 = PRESENTATION_LAYER_ASSIGNMENT (  '', '', ( #53642 ) ) ;
#9889 = EDGE_CURVE ( 'NONE', #42152, #6348, #34191, .T. ) ;
#9888 = ORIENTED_EDGE ( 'NONE', *, *, #44930, .T. ) ;
#9890 = CARTESIAN_POINT ( 'NONE',  ( 53.00000000000000000, 24.99999999999998579, 4.000000000000000000 ) ) ;
#9891 = DIRECTION ( 'NONE',  ( 0.000000000000000000, 0.000000000000000000, 1.000000000000000000 ) ) ;
#9892 = CARTESIAN_POINT ( 'NONE',  ( -67.70499999999998408, 2.607480562269073321, 8.024999999999991473 ) ) ;
#9893 = EDGE_LOOP ( 'NONE', ( #21773, #5562, #21619, #15783 ) ) ;
#9894 = FACE_OUTER_BOUND ( 'NONE', #60295, .T. ) ;
#9895 = DIRECTION ( 'NONE',  ( 1.000000000000000000, 0.000000000000000000, 0.000000000000000000 ) ) ;
#9896 = B_SPLINE_CURVE_WITH_KNOTS ( 'NONE', 3,
 ( #23863, #55876, #2342, #18246, #45713, #8036 ),
 .UNSPECIFIED., .F., .F.,
 ( 4, 2, 4 ),
 ( 0.005386537104126978143, 0.008060814333094822037, 0.01073509156206266593 ),
 .UNSPECIFIED. ) ;
#9897 = EDGE_CURVE ( 'NONE', #44738, #31646, #38435, .T. ) ;
#9898 = CARTESIAN_POINT ( 'NONE',  ( 71.49999999999998579, 119.9999999999997868, -7.500000000000000000 ) ) ;
#9899 = CARTESIAN_POINT ( 'NONE',  ( 0.000000000000000000, 14.00000000000000000, 36.50000000000000000 ) ) ;
#9900 = ORIENTED_EDGE ( 'NONE', *, *, #1556, .T. ) ;
#9901 = FACE_OUTER_BOUND ( 'NONE', #22838, .T. ) ;
#9902 = EDGE_CURVE ( 'NONE', #34864, #34213, #36934, .T. ) ;
#9903 = LINE ( 'NONE', #20797, #44073 ) ;
#9904 =( LENGTH_UNIT ( ) NAMED_UNIT ( * ) SI_UNIT ( .MILLI., .METRE. ) );
#9905 = CARTESIAN_POINT ( 'NONE',  ( -13.23915246117191025, 52.65078610323165265, -2.000000000000000000 ) ) ;
#9906 = CARTESIAN_POINT ( 'NONE',  ( -5.598654528085806881, 145.7449999999999761, -7.705886871421374629 ) ) ;
#9907 = CARTESIAN_POINT ( 'NONE',  ( -97.79500000000000171, 2.607480562269068880, -8.024999999999993250 ) ) ;
#9908 = DIRECTION ( 'NONE',  ( -1.000000000000000000, 0.000000000000000000, 0.000000000000000000 ) ) ;
#9909 = LINE ( 'NONE', #41580, #68524 ) ;
#9910 =( NAMED_UNIT ( * ) SI_UNIT ( $, .STERADIAN. ) SOLID_ANGLE_UNIT ( ) );
#9911 = EDGE_LOOP ( 'NONE', ( #26834, #53017, #28155, #10091 ) ) ;
#9912 = VECTOR ( 'NONE', #3515, 1000.000000000000000 ) ;
#9913 = CARTESIAN_POINT ( 'NONE',  ( -133.6429263765338078, -5.598654528085801552, 7.705886871421367523 ) ) ;
#9914 = FACE_OUTER_BOUND ( 'NONE', #14594, .T. ) ;
#9915 = CARTESIAN_POINT ( 'NONE',  ( -154.7950000000000159, 2.607480562269068880, -8.024999999999993250 ) ) ;
#9916 = CARTESIAN_POINT ( 'NONE',  ( 71.49999999999998579, 64.07124727947029896, 9.500000000000000000 ) ) ;
#9917 = CIRCLE ( 'NONE', #3099, 1.000000000000000888 ) ;
#9918 = SURFACE_STYLE_FILL_AREA ( #58107 ) ;
#9919 = CARTESIAN_POINT ( 'NONE',  ( 8.250000000000001776, 30.74999999999998579, 3.750000000000000000 ) ) ;
#9920 = CARTESIAN_POINT ( 'NONE',  ( 0.000000000000000000, 0.000000000000000000, 0.000000000000000000 ) ) ;
#9921 = ORIENTED_EDGE ( 'NONE', *, *, #13332, .F. ) ;
#9922 = MECHANICAL_DESIGN_GEOMETRIC_PRESENTATION_REPRESENTATION (  '', ( #18865 ), #7631 ) ;
#9923 = ORIENTED_EDGE ( 'NONE', *, *, #68041, .F. ) ;
#9924 = DIRECTION ( 'NONE',  ( -1.000000000000000000, 0.000000000000000000, 0.000000000000000000 ) ) ;
#9925 = CARTESIAN_POINT ( 'NONE',  ( 0.000000000000000000, -3.500000000000000000, 24.00000000000000000 ) ) ;
#9926 = CARTESIAN_POINT ( 'NONE',  ( 0.9999999999999991118, 50.00000000000000000, -60.00000000000000000 ) ) ;
#9927 = STYLED_ITEM ( 'NONE', ( #20170 ), #67540 ) ;
#9928 = SURFACE_SIDE_STYLE ('',( #4623 ) ) ;
#9929 = VERTEX_POINT ( 'NONE', #28131 ) ;
#9930 = CARTESIAN_POINT ( 'NONE',  ( -155.0049999999999955, 6.826472737025115478, 4.959722759717899443 ) ) ;
#9931 = ORIENTED_EDGE ( 'NONE', *, *, #7326, .T. ) ;
#9932 = DIRECTION ( 'NONE',  ( -0.000000000000000000, -1.000000000000000000, -0.000000000000000000 ) ) ;
#9933 = ORIENTED_EDGE ( 'NONE', *, *, #31239, .T. ) ;
#9934 =( NAMED_UNIT ( * ) PLANE_ANGLE_UNIT ( ) SI_UNIT ( $, .RADIAN. ) );
#9935 = CARTESIAN_POINT ( 'NONE',  ( 8.102448949553183510, 120.9949999999999761, -5.886773742842746238 ) ) ;
#9936 = PLANE ( 'NONE',  #1330 ) ;
#9937 = ORIENTED_EDGE ( 'NONE', *, *, #38412, .T. ) ;
#9938 = EDGE_CURVE ( 'NONE', #60418, #36018, #61577, .T. ) ;
#9939 = CARTESIAN_POINT ( 'NONE',  ( 5.598654528085809545, 116.2549999999999812, -7.705886871421373741 ) ) ;
#9940 = CARTESIAN_POINT ( 'NONE',  ( -64.70499999999998408, 2.607480562269072433, 8.024999999999991473 ) ) ;
#9941 = STYLED_ITEM ( 'NONE', ( #65426 ), #43504 ) ;
#9942 = ORIENTED_EDGE ( 'NONE', *, *, #32512, .F. ) ;
#9943 = CARTESIAN_POINT ( 'NONE',  ( -8.102448949553181734, 144.6049999999999613, 5.886773742842747126 ) ) ;
#9944 = EDGE_CURVE ( 'NONE', #66425, #59410, #49294, .T. ) ;
#9945 = DIRECTION ( 'NONE',  ( 0.000000000000000000, 0.000000000000000000, 1.000000000000000000 ) ) ;
#9946 = EDGE_CURVE ( 'NONE', #69681, #23161, #856, .T. ) ;
#9947 = CARTESIAN_POINT ( 'NONE',  ( 20.71462257909523075, 114.5925267038606563, 10.00000000000000000 ) ) ;
#9948 =( NAMED_UNIT ( * ) SI_UNIT ( $, .STERADIAN. ) SOLID_ANGLE_UNIT ( ) );
#9949 = SURFACE_STYLE_USAGE ( .BOTH. , #21530 ) ;
#9950 = ORIENTED_EDGE ( 'NONE', *, *, #30726, .T. ) ;
#9951 = PRESENTATION_STYLE_ASSIGNMENT (( #63409 ) ) ;
#9952 = CARTESIAN_POINT ( 'NONE',  ( 0.000000000000000000, 0.000000000000000000, 0.000000000000000000 ) ) ;
#9953 = CARTESIAN_POINT ( 'NONE',  ( 0.000000000000000000, 1.999999999999998668, 0.000000000000000000 ) ) ;
#9954 = CARTESIAN_POINT ( 'NONE',  ( -183.5049999999999955, -6.826472737025115478, -4.959722759717899443 ) ) ;
#9955 = ORIENTED_EDGE ( 'NONE', *, *, #24307, .F. ) ;
#9956 =( BOUNDED_CURVE ( )  B_SPLINE_CURVE ( 2, ( #193, #17509, #10821, #38288, #17165, #26955, #11153, #16484, #64636, #60376, #43233 ),
 .UNSPECIFIED., .F., .F. ) 
 B_SPLINE_CURVE_WITH_KNOTS ( ( 3, 2, 2, 2, 2, 3 ),
 ( 0.9673913043478260532, 0.9695652173913043015, 0.9717391304347826608, 0.9739130434782609091, 0.9760869565217391575, 0.9782608695652174058 ),
 .UNSPECIFIED. ) 
 CURVE ( )  GEOMETRIC_REPRESENTATION_ITEM ( )  RATIONAL_B_SPLINE_CURVE ( ( 1.000000000000000000, 0.9510565162951535312, 1.000000000000000000, 0.9510565162951535312, 1.000000000000000000, 0.9510565162951535312, 1.000000000000000000, 0.9510565162951535312, 1.000000000000000000, 0.9510565162951535312, 1.000000000000000000 ) ) 
 REPRESENTATION_ITEM ( '' )  );
#9957 = CARTESIAN_POINT ( 'NONE',  ( -2.451748578458123784E-13, 110.8535625161535592, 9.171437483846442973 ) ) ;
#9958 = STYLED_ITEM ( 'NONE', ( #10473 ), #4196 ) ;
#9959 = CARTESIAN_POINT ( 'NONE',  ( 0.000000000000000000, 0.000000000000000000, 10.99999999999995381 ) ) ;
#9960 = CARTESIAN_POINT ( 'NONE',  ( -1.502314598737159031E-15, 2.500000000000000000, -9.000000000000000000 ) ) ;
#9961 = ORIENTED_EDGE ( 'NONE', *, *, #8813, .F. ) ;
#9962 = DIRECTION ( 'NONE',  ( -1.000000000000000000, 0.000000000000000000, 0.000000000000000000 ) ) ;
#9963 = ORIENTED_EDGE ( 'NONE', *, *, #30898, .T. ) ;
#9964 = VECTOR ( 'NONE', #23363, 1000.000000000000000 ) ;
#9965 = EDGE_CURVE ( 'NONE', #22579, #54909, #22550, .T. ) ;
#9966 = CARTESIAN_POINT ( 'NONE',  ( -1.403516486455608892, -7.000000000000002665, 0.1310752030855618366 ) ) ;
#9967 =( NAMED_UNIT ( * ) SI_UNIT ( $, .STERADIAN. ) SOLID_ANGLE_UNIT ( ) );
#9968 = CARTESIAN_POINT ( 'NONE',  ( -95.00499999999998124, 6.826472737025116366, 4.959722759717898555 ) ) ;
#9969 = VERTEX_POINT ( 'NONE', #65461 ) ;
#9970 = DIRECTION ( 'NONE',  ( 0.000000000000000000, -1.000000000000000000, 0.000000000000000000 ) ) ;
#9971 = DIRECTION ( 'NONE',  ( 0.000000000000000000, 0.000000000000000000, 1.000000000000000000 ) ) ;
#9972 = CIRCLE ( 'NONE', #23396, 0.5000000000000004441 ) ;
#9973 = CARTESIAN_POINT ( 'NONE',  ( -131.1570736234661751, -9.058813317711329915, -2.943386871421370898 ) ) ;
#9974 =( LENGTH_UNIT ( ) NAMED_UNIT ( * ) SI_UNIT ( .MILLI., .METRE. ) );
#9975 = CARTESIAN_POINT ( 'NONE',  ( -8.102448949553179958, 152.4949999999999761, 5.886773742842747126 ) ) ;
#9976 = CARTESIAN_POINT ( 'NONE',  ( -77.15707362346617515, -9.058813317711329915, -2.943386871421370898 ) ) ;
#9977 = VERTEX_POINT ( 'NONE', #7060 ) ;
#9978 = CARTESIAN_POINT ( 'NONE',  ( 30.25000000000000711, 18.74999999999997868, 3.750000000000000000 ) ) ;
#9979 = CARTESIAN_POINT ( 'NONE',  ( -16.62496282464071840, -11.02508589828193131, -4.739834931414112162 ) ) ;
#9980 = AXIS2_PLACEMENT_3D ( 'NONE', #17602, #55550, #7698 ) ;
#9981 = LINE ( 'NONE', #49031, #31372 ) ;
#9982 = CARTESIAN_POINT ( 'NONE',  ( -113.3049999999999784, 8.437984349512085203, -1.550032578732815448E-15 ) ) ;
#9984 = ADVANCED_FACE ( 'NONE', ( #24965 ), #35877, .F. ) ;
#9983 = CARTESIAN_POINT ( 'NONE',  ( -195.0000000000000000, 0.000000000000000000, 9.524999999999991473 ) ) ;
#9985 = CARTESIAN_POINT ( 'NONE',  ( 5.598654528085805993, 117.2449999999999903, 7.705886871421374629 ) ) ;
#9986 = CARTESIAN_POINT ( 'NONE',  ( -129.1449999999999818, -4.716976649647092401, 6.492361379858946790 ) ) ;
#9987 = EDGE_CURVE ( 'NONE', #51568, #39729, #6588, .T. ) ;
#9988 = CARTESIAN_POINT ( 'NONE',  ( -118.9429263765338050, 0.000000000000000000, 9.524999999999991473 ) ) ;
#9989 = ORIENTED_EDGE ( 'NONE', *, *, #5247, .F. ) ;
#9990 = AXIS2_PLACEMENT_3D ( 'NONE', #56422, #51167, #2912 ) ;
#9991 = CARTESIAN_POINT ( 'NONE',  ( -159.2929263765337851, 3.094860106618428031, -9.524999999999993250 ) ) ;
#9992 = FILL_AREA_STYLE ('',( #4315 ) ) ;
#9993 =( NAMED_UNIT ( * ) PLANE_ANGLE_UNIT ( ) SI_UNIT ( $, .RADIAN. ) );
#9994 = AXIS2_PLACEMENT_3D ( 'NONE', #34680, #44943, #33995 ) ;
#9995 =( GEOMETRIC_REPRESENTATION_CONTEXT ( 3 ) GLOBAL_UNCERTAINTY_ASSIGNED_CONTEXT ( ( #9693 ) ) GLOBAL_UNIT_ASSIGNED_CONTEXT ( ( #15784, #52032, #42215 ) ) REPRESENTATION_CONTEXT ( 'NONE', 'WORKASPACE' ) );
#9996 = AXIS2_PLACEMENT_3D ( 'NONE', #25997, #68243, #20384 ) ;
#9997 = CARTESIAN_POINT ( 'NONE',  ( -48.81081081081080697, 14.09971791521132900, 9.500000000000000000 ) ) ;
#9998 = CARTESIAN_POINT ( 'NONE',  ( -71.99999999999998579, 119.9999999999997868, -7.000000000000000000 ) ) ;
#9999 = LINE ( 'NONE', #58877, #59683 ) ;
#10000 = ORIENTED_EDGE ( 'NONE', *, *, #66561, .T. ) ;
#10001 = CARTESIAN_POINT ( 'NONE',  ( -73.19292637653380496, -10.01517768586948698, 6.132527647946031529E-16 ) ) ;
#10002 = ITEM_DEFINED_TRANSFORMATION ( 'NONE', 'NONE', #56236,  #42840 ) ;
#10003 = DIRECTION ( 'NONE',  ( -1.189524669241239115E-16, -1.000000000000000000, 0.000000000000000000 ) ) ;
#10004 = DIRECTION ( 'NONE',  ( -1.000000000000000000, 4.336808689941999001E-16, 0.000000000000000000 ) ) ;
#10005 = PRESENTATION_STYLE_ASSIGNMENT (( #30050 ) ) ;
#10006 = MECHANICAL_DESIGN_GEOMETRIC_PRESENTATION_REPRESENTATION (  '', ( #67288 ), #12178 ) ;
#10007 = CIRCLE ( 'NONE', #5444, 8.500000000000000000 ) ;
#10008 = CARTESIAN_POINT ( 'NONE',  ( -175.4049999999999727, -2.607480562269069768, 8.024999999999991473 ) ) ;
#10009 = VERTEX_POINT ( 'NONE', #56642 ) ;
#10010 =( NAMED_UNIT ( * ) SI_UNIT ( $, .STERADIAN. ) SOLID_ANGLE_UNIT ( ) );
#10012 = EDGE_CURVE ( 'NONE', #58922, #25661, #17009, .T. ) ;
#10011 = PRESENTATION_STYLE_ASSIGNMENT (( #42753 ) ) ;
#10013 = CARTESIAN_POINT ( 'NONE',  ( 24.00000000000000000, 1.000000000000000888, 3.000000000000000000 ) ) ;
#10014 = VERTEX_POINT ( 'NONE', #14081 ) ;
#10015 = CARTESIAN_POINT ( 'NONE',  ( -103.4929263765337879, -8.102448949553174629, 5.886773742842742685 ) ) ;
#10016 = PRESENTATION_LAYER_ASSIGNMENT (  '', '', ( #42578 ) ) ;
#10017 = CARTESIAN_POINT ( 'NONE',  ( 31.00000000000000000, 42.00000000000000000, -79.00402776293826435 ) ) ;
#10018 = CARTESIAN_POINT ( 'NONE',  ( 7.632228543268608334, 141.4570736234661581, -2.479861379858951942 ) ) ;
#10019 = CYLINDRICAL_SURFACE ( 'NONE', #57390, 0.2500000000000002220 ) ;
#10020 = CIRCLE ( 'NONE', #50480, 16.00000000000000711 ) ;
#10021 = ORIENTED_EDGE ( 'NONE', *, *, #13254, .T. ) ;
#10022 = DIRECTION ( 'NONE',  ( 0.000000000000000000, 0.000000000000000000, -1.000000000000000000 ) ) ;
#10023 = CARTESIAN_POINT ( 'NONE',  ( -94.40500000000000114, -2.607480562269069768, 8.024999999999991473 ) ) ;
#10024 = AXIS2_PLACEMENT_3D ( 'NONE', #36578, #67144, #30885 ) ;
#10025 = DIRECTION ( 'NONE',  ( 0.000000000000000000, 0.000000000000000000, 1.000000000000000000 ) ) ;
#10026 = VERTEX_POINT ( 'NONE', #40145 ) ;
#10027 = EDGE_CURVE ( 'NONE', #49213, #40311, #53504, .T. ) ;
#10028 = DIRECTION ( 'NONE',  ( 0.000000000000000000, 0.000000000000000000, 1.000000000000000000 ) ) ;
#10029 = DIRECTION ( 'NONE',  ( 0.000000000000000000, 0.000000000000000000, 1.000000000000000000 ) ) ;
#10030 = ORIENTED_EDGE ( 'NONE', *, *, #13048, .F. ) ;
#10031 = DIRECTION ( 'NONE',  ( -0.000000000000000000, 1.000000000000000000, -0.000000000000000000 ) ) ;
#10032 = CARTESIAN_POINT ( 'NONE',  ( -76.64499999999999602, 4.716976649647091513, -6.492361379858946790 ) ) ;
#10033 = ORIENTED_EDGE ( 'NONE', *, *, #26187, .T. ) ;
#10034 =( LENGTH_UNIT ( ) NAMED_UNIT ( * ) SI_UNIT ( .MILLI., .METRE. ) );
#10035 = CARTESIAN_POINT ( 'NONE',  ( -120.3570736234661780, 5.598654528085804216, 7.705886871421366635 ) ) ;
#10036 = PRESENTATION_STYLE_ASSIGNMENT (( #31112 ) ) ;
#10037 = MECHANICAL_DESIGN_GEOMETRIC_PRESENTATION_REPRESENTATION (  '', ( #40364 ), #41532 ) ;
#10038 = VERTEX_POINT ( 'NONE', #18665 ) ;
#10039 = FACE_OUTER_BOUND ( 'NONE', #31821, .T. ) ;
#10040 = DIRECTION ( 'NONE',  ( 0.000000000000000000, 0.000000000000000000, 1.000000000000000000 ) ) ;
#10041 = AXIS2_PLACEMENT_3D ( 'NONE', #31482, #15360, #67751 ) ;
#10042 = EDGE_CURVE ( 'NONE', #19928, #44275, #34672, .T. ) ;
#10043 = EDGE_LOOP ( 'NONE', ( #42400, #54838, #30829, #39184, #25089 ) ) ;
#10044 = DIRECTION ( 'NONE',  ( 1.000000000000000000, -0.000000000000000000, 0.000000000000000000 ) ) ;
#10045 = ORIENTED_EDGE ( 'NONE', *, *, #26039, .T. ) ;
#10046 = CIRCLE ( 'NONE', #35898, 18.00000000000000355 ) ;
#10047 =( NAMED_UNIT ( * ) SI_UNIT ( $, .STERADIAN. ) SOLID_ANGLE_UNIT ( ) );
#10048 = CARTESIAN_POINT ( 'NONE',  ( -148.9429263765338192, 0.000000000000000000, 9.524999999999991473 ) ) ;
#10049 = CONICAL_SURFACE ( 'NONE', #30241, 6.999999999999997335, 0.7853981633974500554 ) ;
#10050 = CARTESIAN_POINT ( 'NONE',  ( -158.1570736234661751, -9.058813317711329915, -2.943386871421370898 ) ) ;
#10051 = AXIS2_PLACEMENT_3D ( 'NONE', #48362, #17027, #21585 ) ;
#10052 = CARTESIAN_POINT ( 'NONE',  ( 8.102448949553179958, 120.3949999999999818, 5.886773742842750679 ) ) ;
#10053 = VECTOR ( 'NONE', #13847, 1000.000000000000000 ) ;
#10054 = SHAPE_REPRESENTATION ( '10. Bolt M10x25', ( #42840 ), #29323 ) ;
#10055 = CARTESIAN_POINT ( 'NONE',  ( -105.6570736234661751, 9.058813317711329915, 2.943386871421369566 ) ) ;
#10056 = CIRCLE ( 'NONE', #63955, 0.2500000000000002220 ) ;
#10057 = DIRECTION ( 'NONE',  ( 0.000000000000000000, 0.000000000000000000, 1.000000000000000000 ) ) ;
#10058 = VERTEX_POINT ( 'NONE', #61537 ) ;
#10059 = AXIS2_PLACEMENT_3D ( 'NONE', #660, #31695, #4965 ) ;
#10060 = CYLINDRICAL_SURFACE ( 'NONE', #64380, 0.5000000000000004441 ) ;
#10062 = CARTESIAN_POINT ( 'NONE',  ( -115.1070736234661638, 8.102448949553172852, -5.886773742842744461 ) ) ;
#10061 = CYLINDRICAL_SURFACE ( 'NONE', #45875, 10.00000000000000000 ) ;
#10063 = CARTESIAN_POINT ( 'NONE',  ( -142.4049999999999443, -2.607480562269069768, 8.024999999999991473 ) ) ;
#10064 = DIRECTION ( 'NONE',  ( 0.000000000000000000, 0.000000000000000000, 1.000000000000000000 ) ) ;
#10065 = CARTESIAN_POINT ( 'NONE',  ( -159.4449999999999932, 0.000000000000000000, 8.024999999999991473 ) ) ;
#10066 = CIRCLE ( 'NONE', #34727, 0.2500000000000002220 ) ;
#10067 = CARTESIAN_POINT ( 'NONE',  ( -138.7450000000000045, 4.716976649647094177, 6.492361379858945902 ) ) ;
#10068 = ORIENTED_EDGE ( 'NONE', *, *, #62505, .F. ) ;
#10069 = AXIS2_PLACEMENT_3D ( 'NONE', #35243, #10255, #58779 ) ;
#10070 = B_SPLINE_CURVE_WITH_KNOTS ( 'NONE', 3,
 ( #28298, #39271, #24098, #50493, #44900, #23393, #28664, #13183 ),
 .UNSPECIFIED., .F., .F.,
 ( 4, 2, 2, 4 ),
 ( 0.000000000000000000, 0.001660002979567827509, 0.002490004469351742022, 0.003320005959135656319 ),
 .UNSPECIFIED. ) ;
#10071 = DIRECTION ( 'NONE',  ( -1.000000000000000000, 0.000000000000000000, 0.000000000000000000 ) ) ;
#10072 = CARTESIAN_POINT ( 'NONE',  ( 20.71938756518089875, 149.6378529145318907, -9.985383568374002650 ) ) ;
#10073 = UNCERTAINTY_MEASURE_WITH_UNIT (LENGTH_MEASURE( 1.000000000000000082E-05 ), #1753, 'distance_accuracy_value', 'NONE');
#10074 = CARTESIAN_POINT ( 'NONE',  ( -52.10499999999998266, -6.826472737025115478, 4.959722759717900331 ) ) ;
#10075 = CARTESIAN_POINT ( 'NONE',  ( 3.094860106618431583, 154.2049999999999272, 9.525000000000000355 ) ) ;
#10076 = CARTESIAN_POINT ( 'NONE',  ( -144.0570736234661808, 0.000000000000000000, 9.524999999999991473 ) ) ;
#10077 = CARTESIAN_POINT ( 'NONE',  ( -71.50000000000000000, 14.49137674618942562, 7.500000000000000000 ) ) ;
#10078 = AXIS2_PLACEMENT_3D ( 'NONE', #58918, #4034, #41374 ) ;
#10079 = CIRCLE ( 'NONE', #31393, 113.0000000000000284 ) ;
#10080 = UNCERTAINTY_MEASURE_WITH_UNIT (LENGTH_MEASURE( 1.000000000000000082E-05 ), #7202, 'distance_accuracy_value', 'NONE');
#10081 =( LENGTH_UNIT ( ) NAMED_UNIT ( * ) SI_UNIT ( .MILLI., .METRE. ) );
#10082 = MECHANICAL_DESIGN_GEOMETRIC_PRESENTATION_REPRESENTATION (  '', ( #39326 ), #23567 ) ;
#10083 = CARTESIAN_POINT ( 'NONE',  ( -81.50707362346616947, 8.102448949553176405, 5.886773742842740909 ) ) ;
#10084 = CIRCLE ( 'NONE', #34765, 18.00000000000000355 ) ;
#10085 = CARTESIAN_POINT ( 'NONE',  ( 82.09357085539566867, 0.000000000000000000, -32.00402776293823592 ) ) ;
#10086 = DIRECTION ( 'NONE',  ( 0.000000000000000000, 0.000000000000000000, 1.000000000000000000 ) ) ;
#10087 = EDGE_CURVE ( 'NONE', #24854, #7947, #18321, .T. ) ;
#10088 = STYLED_ITEM ( 'NONE', ( #67561 ), #20668 ) ;
#10089 = CARTESIAN_POINT ( 'NONE',  ( 26.25000000000001066, 18.99999999999997868, -3.750000000000000000 ) ) ;
#10090 = ORIENTED_EDGE ( 'NONE', *, *, #17209, .F. ) ;
#10091 = ORIENTED_EDGE ( 'NONE', *, *, #39186, .F. ) ;
#10092 = FILL_AREA_STYLE ('',( #20282 ) ) ;
#10093 = CIRCLE ( 'NONE', #25843, 0.2500000000000002220 ) ;
#10094 = CARTESIAN_POINT ( 'NONE',  ( 6.826472737025121695, 117.6070736234661638, -4.959722759717905660 ) ) ;
#10095 = EDGE_CURVE ( 'NONE', #20493, #59308, #23926, .T. ) ;
#10096 = EDGE_CURVE ( 'NONE', #41120, #56763, #22341, .T. ) ;
#10098 = SURFACE_STYLE_USAGE ( .BOTH. , #36856 ) ;
#10097 = CIRCLE ( 'NONE', #64012, 13.49999999999999822 ) ;
#10099 = COLOUR_RGB ( '', 0.66274510, 0.83137255, 0.94901961) ;
#10100 =( LENGTH_UNIT ( ) NAMED_UNIT ( * ) SI_UNIT ( .MILLI., .METRE. ) );
#10101 = ORIENTED_EDGE ( 'NONE', *, *, #57431, .T. ) ;
#10102 = ORIENTED_EDGE ( 'NONE', *, *, #49426, .T. ) ;
#10103 = DIRECTION ( 'NONE',  ( -3.717264591378879477E-17, 0.000000000000000000, 1.000000000000000000 ) ) ;
#10104 = EDGE_CURVE ( 'NONE', #42659, #55156, #64994, .T. ) ;
#10105 = FACE_OUTER_BOUND ( 'NONE', #36903, .T. ) ;
#10106 = ORIENTED_EDGE ( 'NONE', *, *, #47963, .F. ) ;
#10107 = CARTESIAN_POINT ( 'NONE',  ( 3.094860106618435136, 122.4049999999999727, -9.525000000000000355 ) ) ;
#10108 = CARTESIAN_POINT ( 'NONE',  ( -84.44292637653380496, -1.166476076187852838E-15, -9.524999999999991473 ) ) ;
#10109 = FILL_AREA_STYLE_COLOUR ( '', #32219 ) ;
#10110 = ADVANCED_FACE ( 'NONE', ( #13365 ), #35544, .F. ) ;
#10111 = MECHANICAL_DESIGN_GEOMETRIC_PRESENTATION_REPRESENTATION (  '', ( #66224 ), #60586 ) ;
#10112 = EDGE_CURVE ( 'NONE', #9929, #58002, #56278, .T. ) ;
#10113 = DIRECTION ( 'NONE',  ( 0.000000000000000000, 0.000000000000000000, -1.000000000000000000 ) ) ;
#10114 = CARTESIAN_POINT ( 'NONE',  ( -98.84499999999998465, -7.632228543268599452, 2.479861379858951054 ) ) ;
#10115 = EDGE_LOOP ( 'NONE', ( #27710, #11208, #59055, #2986 ) ) ;
#10116 =( REPRESENTATION_RELATIONSHIP ('NONE','NONE', #5102, #12274 ) REPRESENTATION_RELATIONSHIP_WITH_TRANSFORMATION ( #64834 )SHAPE_REPRESENTATION_RELATIONSHIP( ) );
#10117 = CARTESIAN_POINT ( 'NONE',  ( 5.203376869638292490, 154.0320170787420579, -7.424028789300809450 ) ) ;
#10118 = CARTESIAN_POINT ( 'NONE',  ( -164.6070736234661922, -8.102448949553174629, 5.886773742842742685 ) ) ;
#10119 = EDGE_CURVE ( 'NONE', #22278, #38572, #8796, .T. ) ;
#10120 = ORIENTED_EDGE ( 'NONE', *, *, #55610, .T. ) ;
#10121 = CARTESIAN_POINT ( 'NONE',  ( 4.716976649647096842, 157.7429263765338021, 6.492361379858953896 ) ) ;
#10122 = CARTESIAN_POINT ( 'NONE',  ( 45.50000000000000000, -1.414600137340999687E-14, 9.500000000000000000 ) ) ;
#10123 = MECHANICAL_DESIGN_GEOMETRIC_PRESENTATION_REPRESENTATION (  '', ( #17947 ), #67397 ) ;
#10124 = DIRECTION ( 'NONE',  ( 0.000000000000000000, 1.000000000000000000, -0.000000000000000000 ) ) ;
#10125 = ORIENTED_EDGE ( 'NONE', *, *, #51267, .T. ) ;
#10126 = CARTESIAN_POINT ( 'NONE',  ( 25.75000000000001066, 21.74999999999998224, -4.000000000000000000 ) ) ;
#10127 = DIRECTION ( 'NONE',  ( -1.000000000000000000, 0.000000000000000000, 0.000000000000000000 ) ) ;
#10128 = COLOUR_RGB ( '', 0.09019608, 0.27058824, 0.51372549) ;
#10129 = CYLINDRICAL_SURFACE ( 'NONE', #9474, 5.000000000000000000 ) ;
#10130 = CIRCLE ( 'NONE', #14653, 1.000000000000000888 ) ;
#10131 = CARTESIAN_POINT ( 'NONE',  ( -74.42860156060436339, 8.073466093857248893, 6.500000000000083489 ) ) ;
#10132 = DIRECTION ( 'NONE',  ( -0.000000000000000000, -0.000000000000000000, 1.000000000000000000 ) ) ;
#10133 = DIRECTION ( 'NONE',  ( 0.000000000000000000, 0.000000000000000000, -1.000000000000000000 ) ) ;
#10134 = ORIENTED_EDGE ( 'NONE', *, *, #14692, .T. ) ;
#10135 = EDGE_LOOP ( 'NONE', ( #69350, #29921 ) ) ;
#10136 = DIRECTION ( 'NONE',  ( 1.000000000000000000, 0.000000000000000000, -0.000000000000000000 ) ) ;
#10137 = DIRECTION ( 'NONE',  ( -0.000000000000000000, 0.000000000000000000, -1.000000000000000000 ) ) ;
#10138 = DIRECTION ( 'NONE',  ( -0.8660254037844385966, 0.000000000000000000, 0.5000000000000003331 ) ) ;
#10139 = VERTEX_POINT ( 'NONE', #14406 ) ;
#10140 = CARTESIAN_POINT ( 'NONE',  ( -165.0550000000000068, -9.827790563157499189E-16, -8.024999999999991473 ) ) ;
#10141 = DIRECTION ( 'NONE',  ( -0.000000000000000000, -0.000000000000000000, -1.000000000000000000 ) ) ;
#10142 = FACE_OUTER_BOUND ( 'NONE', #56761, .T. ) ;
#10143 =( GEOMETRIC_REPRESENTATION_CONTEXT ( 3 ) GLOBAL_UNCERTAINTY_ASSIGNED_CONTEXT ( ( #42080 ) ) GLOBAL_UNIT_ASSIGNED_CONTEXT ( ( #15470, #58343, #52058 ) ) REPRESENTATION_CONTEXT ( 'NONE', 'WORKASPACE' ) );
#10144 = CARTESIAN_POINT ( 'NONE',  ( -48.65707362346616094, 9.058813317711329915, 2.943386871421369566 ) ) ;
#10145 = VECTOR ( 'NONE', #22158, 1000.000000000000000 ) ;
#10146 = CARTESIAN_POINT ( 'NONE',  ( -163.7949999999999875, 2.607480562269069324, -8.024999999999993250 ) ) ;
#10147 = MECHANICAL_DESIGN_GEOMETRIC_PRESENTATION_REPRESENTATION (  '', ( #55055 ), #42777 ) ;
#10148 = ORIENTED_EDGE ( 'NONE', *, *, #1145, .F. ) ;
#10149 = DIRECTION ( 'NONE',  ( -1.000000000000000000, -0.000000000000000000, -0.000000000000000000 ) ) ;
#10150 = LINE ( 'NONE', #68545, #23463 ) ;
#10151 = AXIS2_PLACEMENT_3D ( 'NONE', #22099, #33345, #54769 ) ;
#10152 = CARTESIAN_POINT ( 'NONE',  ( -13.68927517661561133, 10.98243962888954428, -4.836436941715524185 ) ) ;
#10153 = CARTESIAN_POINT ( 'NONE',  ( -82.10499999999998977, -6.826472737025115478, 4.959722759717900331 ) ) ;
#10154 =( NAMED_UNIT ( * ) SI_UNIT ( $, .STERADIAN. ) SOLID_ANGLE_UNIT ( ) );
#10155 = MECHANICAL_DESIGN_GEOMETRIC_PRESENTATION_REPRESENTATION (  '', ( #65163 ), #34842 ) ;
#10156 = CARTESIAN_POINT ( 'NONE',  ( -75.43856457103669300, 36.03011512829429819, -9.655596932504062480 ) ) ;
#10157 = CARTESIAN_POINT ( 'NONE',  ( -94.79499999999997328, 2.607480562269069324, -8.024999999999993250 ) ) ;
#10158 = CARTESIAN_POINT ( 'NONE',  ( -8.102448949553181734, 129.6049999999999613, 5.886773742842747126 ) ) ;
#10159 = CARTESIAN_POINT ( 'NONE',  ( -87.50000000000000000, -8.499999999999989342, 23.00000000000000000 ) ) ;
#10160 = DIRECTION ( 'NONE',  ( -0.000000000000000000, 1.000000000000000000, -0.000000000000000000 ) ) ;
#10161 = PRESENTATION_STYLE_ASSIGNMENT (( #43258 ) ) ;
#10162 = UNCERTAINTY_MEASURE_WITH_UNIT (LENGTH_MEASURE( 1.000000000000000082E-05 ), #41249, 'distance_accuracy_value', 'NONE');
#10163 = CIRCLE ( 'NONE', #6774, 0.5000000000000004441 ) ;
#10164 = CARTESIAN_POINT ( 'NONE',  ( -0.7087670488506471189, -2.466410156631502648, -7.000000000000002665 ) ) ;
#10165 = SURFACE_STYLE_USAGE ( .BOTH. , #11531 ) ;
#10166 = ORIENTED_EDGE ( 'NONE', *, *, #33064, .F. ) ;
#10167 = DIRECTION ( 'NONE',  ( 0.000000000000000000, 0.000000000000000000, -1.000000000000000000 ) ) ;
#10168 = VECTOR ( 'NONE', #48862, 1000.000000000000000 ) ;
#10169 = ADVANCED_FACE ( 'NONE', ( #56982 ), #35182, .T. ) ;
#10171 = FILL_AREA_STYLE ('',( #48184 ) ) ;
#10170 = CARTESIAN_POINT ( 'NONE',  ( -131.8429263765337964, 9.058813317711329915, -2.943386871421373119 ) ) ;
#10172 = FACE_OUTER_BOUND ( 'NONE', #37114, .T. ) ;
#10173 = ORIENTED_EDGE ( 'NONE', *, *, #5445, .T. ) ;
#10174 = VERTEX_POINT ( 'NONE', #34484 ) ;
#10175 = VECTOR ( 'NONE', #42880, 1000.000000000000000 ) ;
#10176 =( LENGTH_UNIT ( ) NAMED_UNIT ( * ) SI_UNIT ( .MILLI., .METRE. ) );
#10177 = ADVANCED_FACE ( 'NONE', ( #29183 ), #59056, .T. ) ;
#10178 = CIRCLE ( 'NONE', #30373, 5.000000000000004441 ) ;
#10179 = FILL_AREA_STYLE_COLOUR ( '', #13628 ) ;
#10180 = LINE ( 'NONE', #20376, #23939 ) ;
#10181 = VERTEX_POINT ( 'NONE', #50671 ) ;
#10182 = CARTESIAN_POINT ( 'NONE',  ( -123.9549999999999841, -7.632228543268599452, 2.479861379858951054 ) ) ;
#10183 = ORIENTED_EDGE ( 'NONE', *, *, #58138, .T. ) ;
#10184 = CARTESIAN_POINT ( 'NONE',  ( -137.3070736234661808, -10.01517768586948698, 6.132527647946031529E-16 ) ) ;
#10185 = CARTESIAN_POINT ( 'NONE',  ( -9.827790563157511022E-16, 128.5570736234661524, 8.025000000000000355 ) ) ;
#10186 = EDGE_LOOP ( 'NONE', ( #69136, #53449, #46753, #58357 ) ) ;
#10187 = CARTESIAN_POINT ( 'NONE',  ( 7.440601873764704166, 2.005109422339667269, 1.112499515747340073 ) ) ;
#10188 = ORIENTED_EDGE ( 'NONE', *, *, #2589, .T. ) ;
#10189 = CIRCLE ( 'NONE', #34883, 0.2500000000000002220 ) ;
#10190 = ADVANCED_FACE ( 'NONE', ( #52762 ), #31975, .F. ) ;
#10191 = PRESENTATION_LAYER_ASSIGNMENT (  '', '', ( #4541 ) ) ;
#10192 = PRESENTATION_LAYER_ASSIGNMENT (  '', '', ( #61824 ) ) ;
#10193 = CARTESIAN_POINT ( 'NONE',  ( 0.000000000000000000, 154.4449999999999932, -9.525000000000000355 ) ) ;
#10194 = DIRECTION ( 'NONE',  ( 1.000000000000000000, 0.000000000000000000, -0.000000000000000000 ) ) ;
#10195 = AXIS2_PLACEMENT_3D ( 'NONE', #54944, #1079, #59542 ) ;
#10196 = ORIENTED_EDGE ( 'NONE', *, *, #55376, .T. ) ;
#10197 = SURFACE_SIDE_STYLE ('',( #52089 ) ) ;
#10198 = CARTESIAN_POINT ( 'NONE',  ( 3.094860106618435136, 146.4050000000000011, -9.525000000000000355 ) ) ;
#10199 = DIRECTION ( 'NONE',  ( -1.000000000000000000, 0.000000000000000000, 0.000000000000000000 ) ) ;
#10200 = ADVANCED_FACE ( 'NONE', ( #15828 ), #14781, .F. ) ;
#10201 = DIRECTION ( 'NONE',  ( -0.000000000000000000, -1.000000000000000000, -0.000000000000000000 ) ) ;
#10202 = ORIENTED_EDGE ( 'NONE', *, *, #10279, .F. ) ;
#10203 = CARTESIAN_POINT ( 'NONE',  ( 2.607480562269076430, 125.7929263765338277, -8.025000000000000355 ) ) ;
#10204 = FACE_OUTER_BOUND ( 'NONE', #3501, .T. ) ;
#10205 = UNCERTAINTY_MEASURE_WITH_UNIT (LENGTH_MEASURE( 1.000000000000000082E-05 ), #8244, 'distance_accuracy_value', 'NONE');
#10206 = CARTESIAN_POINT ( 'NONE',  ( -30.38025804288030329, -7.499999999999996447, 0.06931351858050209536 ) ) ;
#10207 = CARTESIAN_POINT ( 'NONE',  ( -99.14292637653380780, 5.598654528085800663, -7.705886871421367523 ) ) ;
#10208 =( NAMED_UNIT ( * ) SI_UNIT ( $, .STERADIAN. ) SOLID_ANGLE_UNIT ( ) );
#10209 = ORIENTED_EDGE ( 'NONE', *, *, #1038, .F. ) ;
#10210 = AXIS2_PLACEMENT_3D ( 'NONE', #33069, #69322, #44006 ) ;
#10211 = DIRECTION ( 'NONE',  ( 0.000000000000000000, 0.000000000000000000, 1.000000000000000000 ) ) ;
#10212 = VERTEX_POINT ( 'NONE', #9514 ) ;
#10213 = CARTESIAN_POINT ( 'NONE',  ( -54.14292637653381490, 5.598654528085800663, -7.705886871421367523 ) ) ;
#10214 = DIRECTION ( 'NONE',  ( -1.000000000000000000, 0.000000000000000000, 0.000000000000000000 ) ) ;
#10215 = CARTESIAN_POINT ( 'NONE',  ( -150.3549999999999898, -4.716976649647093289, -6.492361379858945902 ) ) ;
#10216 = FILL_AREA_STYLE ('',( #6301 ) ) ;
#10217 =( LENGTH_UNIT ( ) NAMED_UNIT ( * ) SI_UNIT ( .MILLI., .METRE. ) );
#10218 = UNCERTAINTY_MEASURE_WITH_UNIT (LENGTH_MEASURE( 1.000000000000000082E-05 ), #37828, 'distance_accuracy_value', 'NONE');
#10219 = MECHANICAL_DESIGN_GEOMETRIC_PRESENTATION_REPRESENTATION (  '', ( #60740 ), #61851 ) ;
#10220 = DIRECTION ( 'NONE',  ( 1.000000000000000000, 0.000000000000000000, 0.000000000000000000 ) ) ;
#10221 =( LENGTH_UNIT ( ) NAMED_UNIT ( * ) SI_UNIT ( .MILLI., .METRE. ) );
#10222 = FILL_AREA_STYLE ('',( #58398 ) ) ;
#10223 = FACE_OUTER_BOUND ( 'NONE', #35482, .T. ) ;
#10224 = VERTEX_POINT ( 'NONE', #36625 ) ;
#10225 = COLOUR_RGB ( '', 0.31764706, 0.68627451, 0.89019608) ;
#10226 = ORIENTED_EDGE ( 'NONE', *, *, #41727, .F. ) ;
#10227 = CARTESIAN_POINT ( 'NONE',  ( 23.14150002214069701, 27.39558012762189065, 27.21086609277890034 ) ) ;
#10228 = DIRECTION ( 'NONE',  ( 1.000000000000000000, 0.000000000000000000, 0.000000000000000000 ) ) ;
#10229 = CARTESIAN_POINT ( 'NONE',  ( -67.10499999999997556, -6.826472737025115478, 4.959722759717900331 ) ) ;
#10230 = ORIENTED_EDGE ( 'NONE', *, *, #54926, .T. ) ;
#10231 = CARTESIAN_POINT ( 'NONE',  ( -37.74999999999999289, 4.336808689942018722E-16, 16.97056274847714974 ) ) ;
#10232 = CYLINDRICAL_SURFACE ( 'NONE', #39408, 3.100000000000000533 ) ;
#10233 = DIRECTION ( 'NONE',  ( 0.000000000000000000, 0.000000000000000000, -1.000000000000000000 ) ) ;
#10234 = AXIS2_PLACEMENT_3D ( 'NONE', #64135, #69426, #42738 ) ;
#10235 = CARTESIAN_POINT ( 'NONE',  ( -124.6429263765338078, -5.598654528085801552, 7.705886871421367523 ) ) ;
#10236 = CARTESIAN_POINT ( 'NONE',  ( -87.50000000000000000, -6.499999999999990230, 3.000000000000000000 ) ) ;
#10237 = ORIENTED_EDGE ( 'NONE', *, *, #36356, .T. ) ;
#10238 = EDGE_CURVE ( 'NONE', #31166, #12387, #30932, .T. ) ;
#10239 = AXIS2_PLACEMENT_3D ( 'NONE', #60938, #12756, #56362 ) ;
#10240 = DIRECTION ( 'NONE',  ( 1.000000000000000000, 0.000000000000000000, 0.000000000000000000 ) ) ;
#10241 = CARTESIAN_POINT ( 'NONE',  ( -44.50000000000000000, 10.49999999999998579, 3.500000000000000000 ) ) ;
#10242 = CARTESIAN_POINT ( 'NONE',  ( -195.0000000000000000, 0.000000000000000000, 0.000000000000000000 ) ) ;
#10244 = DIRECTION ( 'NONE',  ( -0.000000000000000000, 1.000000000000000000, -0.000000000000000000 ) ) ;
#10243 = LINE ( 'NONE', #30626, #48099 ) ;
#10245 = AXIS2_PLACEMENT_3D ( 'NONE', #2756, #18640, #19307 ) ;
#10246 = CARTESIAN_POINT ( 'NONE',  ( -122.5449999999999875, -7.632228543268600340, -2.479861379858950166 ) ) ;
#10247 = CARTESIAN_POINT ( 'NONE',  ( 10.01517768586949231, 150.6949999999999648, 1.839758294383810543E-15 ) ) ;
#10248 = CARTESIAN_POINT ( 'NONE',  ( -84.29499999999998749, -2.607480562269069768, 8.024999999999991473 ) ) ;
#10249 = VECTOR ( 'NONE', #19326, 1000.000000000000000 ) ;
#10250 = CARTESIAN_POINT ( 'NONE',  ( 60.00000000000000000, 1.797044900979284448E-15, -11.50000000000000000 ) ) ;
#10251 = CARTESIAN_POINT ( 'NONE',  ( 36.00000000000002842, 0.000000000000000000, -29.00402776293825724 ) ) ;
#10252 =( GEOMETRIC_REPRESENTATION_CONTEXT ( 3 ) GLOBAL_UNCERTAINTY_ASSIGNED_CONTEXT ( ( #60199 ) ) GLOBAL_UNIT_ASSIGNED_CONTEXT ( ( #57140, #9690, #36785 ) ) REPRESENTATION_CONTEXT ( 'NONE', 'WORKASPACE' ) );
#10253 = UNCERTAINTY_MEASURE_WITH_UNIT (LENGTH_MEASURE( 1.000000000000000082E-05 ), #65487, 'distance_accuracy_value', 'NONE');
#10254 = VECTOR ( 'NONE', #18873, 1000.000000000000000 ) ;
#10255 = DIRECTION ( 'NONE',  ( -0.000000000000000000, 1.000000000000000000, 0.000000000000000000 ) ) ;
#10256 = ORIENTED_EDGE ( 'NONE', *, *, #19415, .F. ) ;
#10257 = CARTESIAN_POINT ( 'NONE',  ( -130.3429263765337964, -9.058813317711329915, 2.943386871421371787 ) ) ;
#10258 = SURFACE_STYLE_USAGE ( .BOTH. , #20084 ) ;
#10259 = CARTESIAN_POINT ( 'NONE',  ( -153.4449999999999932, 0.000000000000000000, 8.024999999999991473 ) ) ;
#10260 = DIRECTION ( 'NONE',  ( 0.000000000000000000, 1.350863103983176297E-16, 1.000000000000000000 ) ) ;
#10261 = EDGE_CURVE ( 'NONE', #15159, #15321, #69526, .T. ) ;
#10262 = EDGE_CURVE ( 'NONE', #67533, #33857, #5232, .T. ) ;
#10263 = STYLED_ITEM ( 'NONE', ( #64262 ), #18116 ) ;
#10264 = ORIENTED_EDGE ( 'NONE', *, *, #50830, .T. ) ;
#10265 = ORIENTED_EDGE ( 'NONE', *, *, #67353, .F. ) ;
#10266 = AXIS2_PLACEMENT_3D ( 'NONE', #22271, #49710, #33851 ) ;
#10267 = CARTESIAN_POINT ( 'NONE',  ( 45.50000000000000000, 1.797044900979284448E-15, 6.500000000000000000 ) ) ;
#10268 = CARTESIAN_POINT ( 'NONE',  ( -33.10370830234652573, -9.126466545927527818, -3.681448577161279712 ) ) ;
#10269 = EDGE_CURVE ( 'NONE', #68002, #55126, #4176, .T. ) ;
#10270 = CARTESIAN_POINT ( 'NONE',  ( -45.00000000000000000, -2.024042244987997205E-14, 6.999999999999999112 ) ) ;
#10271 = CARTESIAN_POINT ( 'NONE',  ( 0.000000000000000000, 0.000000000000000000, 0.000000000000000000 ) ) ;
#10272 = SURFACE_SIDE_STYLE ('',( #47249 ) ) ;
#10273 = ORIENTED_EDGE ( 'NONE', *, *, #42909, .T. ) ;
#10274 = CARTESIAN_POINT ( 'NONE',  ( -153.0550000000000068, -9.827790563157499189E-16, -8.024999999999991473 ) ) ;
#10275 = ORIENTED_EDGE ( 'NONE', *, *, #31275, .F. ) ;
#10276 = DIRECTION ( 'NONE',  ( -0.000000000000000000, -1.000000000000000000, -0.000000000000000000 ) ) ;
#10277 = DIRECTION ( 'NONE',  ( 0.000000000000000000, 1.000000000000000000, -0.000000000000000000 ) ) ;
#10278 = ORIENTED_EDGE ( 'NONE', *, *, #4204, .T. ) ;
#10279 = EDGE_CURVE ( 'NONE', #31185, #14977, #67272, .T. ) ;
#10280 = STYLED_ITEM ( 'NONE', ( #18390 ), #60190 ) ;
#10281 = DIRECTION ( 'NONE',  ( -0.000000000000000000, -1.000000000000000000, -0.000000000000000000 ) ) ;
#10282 = CARTESIAN_POINT ( 'NONE',  ( 3.249999999999999112, 34.24999999999998579, -4.000000000000000000 ) ) ;
#10283 = CARTESIAN_POINT ( 'NONE',  ( 9.058813317711337021, 117.5449999999999875, 2.943386871421375783 ) ) ;
#10284 = CARTESIAN_POINT ( 'NONE',  ( 34.99999999999992895, 113.4999999999999858, 7.500000000000000000 ) ) ;
#10285 = ORIENTED_EDGE ( 'NONE', *, *, #52459, .F. ) ;
#10286 =( NAMED_UNIT ( * ) PLANE_ANGLE_UNIT ( ) SI_UNIT ( $, .RADIAN. ) );
#10287 = CARTESIAN_POINT ( 'NONE',  ( -3.094860106618434248, 123.9049999999999727, 9.525000000000000355 ) ) ;
#10288 = CARTESIAN_POINT ( 'NONE',  ( -66.20499999999996987, -2.607480562269071545, -8.024999999999991473 ) ) ;
#10289 = EDGE_CURVE ( 'NONE', #53965, #25042, #27708, .T. ) ;
#10290 = DIRECTION ( 'NONE',  ( 0.000000000000000000, 0.000000000000000000, -1.000000000000000000 ) ) ;
#10291 = PRODUCT ( '8. Upper Jaw Support', '8. Upper Jaw Support', '', ( #44206 ) ) ;
#10292 = EDGE_LOOP ( 'NONE', ( #53621, #42125, #47000 ) ) ;
#10293 = CARTESIAN_POINT ( 'NONE',  ( 5.598654528085809545, 146.2549999999999955, -7.705886871421373741 ) ) ;
#10294 = UNCERTAINTY_MEASURE_WITH_UNIT (LENGTH_MEASURE( 1.000000000000000082E-05 ), #34192, 'distance_accuracy_value', 'NONE');
#10295 = TOROIDAL_SURFACE ( 'NONE', #49608, 0.5000000000000000000, 0.2500000000000000000 ) ;
#10296 =( NAMED_UNIT ( * ) SI_UNIT ( $, .STERADIAN. ) SOLID_ANGLE_UNIT ( ) );
#10297 = SURFACE_STYLE_FILL_AREA ( #357 ) ;
#10298 = CIRCLE ( 'NONE', #29392, 3.000000000000000444 ) ;
#10299 = DIRECTION ( 'NONE',  ( 1.000000000000000000, 0.000000000000000000, 0.000000000000000000 ) ) ;
#10300 = ORIENTED_EDGE ( 'NONE', *, *, #2888, .F. ) ;
#10301 = DIRECTION ( 'NONE',  ( 0.000000000000000000, 0.000000000000000000, -1.000000000000000000 ) ) ;
#10302 = DIRECTION ( 'NONE',  ( -1.000000000000000000, 0.000000000000000000, 0.000000000000000000 ) ) ;
#10303 = CARTESIAN_POINT ( 'NONE',  ( -183.9550000000000125, -7.632228543268599452, 2.479861379858951054 ) ) ;
#10304 = ORIENTED_EDGE ( 'NONE', *, *, #63722, .F. ) ;
#10305 = CARTESIAN_POINT ( 'NONE',  ( 39.24999999999999289, 16.24999999999997513, -3.750000000000000000 ) ) ;
#10306 = AXIS2_PLACEMENT_3D ( 'NONE', #37905, #42831, #64223 ) ;
#10307 = LINE ( 'NONE', #37070, #36943 ) ;
#10308 = VERTEX_POINT ( 'NONE', #65008 ) ;
#10309 = SURFACE_SIDE_STYLE ('',( #5012 ) ) ;
#10310 = LINE ( 'NONE', #31738, #65814 ) ;
#10311 = CIRCLE ( 'NONE', #37299, 4.499999999999976019 ) ;
#10312 = VERTEX_POINT ( 'NONE', #33024 ) ;
#10313 = CARTESIAN_POINT ( 'NONE',  ( -127.7070736234668260, -3.094860106629993890, -9.524999999991592858 ) ) ;
#10314 = CARTESIAN_POINT ( 'NONE',  ( 3.249999999999998668, 36.99999999999999289, -3.750000000000000000 ) ) ;
#10315 = CARTESIAN_POINT ( 'NONE',  ( -91.40500000000000114, -2.607480562269069768, 8.024999999999991473 ) ) ;
#10316 = ORIENTED_EDGE ( 'NONE', *, *, #44817, .F. ) ;
#10317 = CARTESIAN_POINT ( 'NONE',  ( 0.000000000000000000, 2.500000000000000000, 0.000000000000000000 ) ) ;
#10318 = CIRCLE ( 'NONE', #54117, 7.000000000000001776 ) ;
#10319 = DIRECTION ( 'NONE',  ( 0.000000000000000000, -0.000000000000000000, 1.000000000000000000 ) ) ;
#10320 = CARTESIAN_POINT ( 'NONE',  ( -130.8570736234661922, -5.598654528085803328, -7.705886871421366635 ) ) ;
#10321 = CARTESIAN_POINT ( 'NONE',  ( -3.094860106618434248, 152.7949999999999591, 9.525000000000000355 ) ) ;
#10322 = CARTESIAN_POINT ( 'NONE',  ( -61.70707362346615810, -3.094860106618431139, -9.524999999999991473 ) ) ;
#10323 = EDGE_CURVE ( 'NONE', #18337, #62258, #27777, .T. ) ;
#10324 = VECTOR ( 'NONE', #27215, 1000.000000000000000 ) ;
#10325 = SURFACE_STYLE_USAGE ( .BOTH. , #384 ) ;
#10326 = ORIENTED_EDGE ( 'NONE', *, *, #7315, .F. ) ;
#10327 = FACE_OUTER_BOUND ( 'NONE', #40065, .T. ) ;
#10328 = FACE_OUTER_BOUND ( 'NONE', #49921, .T. ) ;
#10329 = CARTESIAN_POINT ( 'NONE',  ( -110.4549999999999841, 7.632228543268599452, -2.479861379858951942 ) ) ;
#10330 = CARTESIAN_POINT ( 'NONE',  ( -3.094860106618432471, 118.5949999999999847, -9.525000000000000355 ) ) ;
#10331 = CARTESIAN_POINT ( 'NONE',  ( -113.6949999999999790, -8.437984349512085203, 5.166775262442717831E-16 ) ) ;
#10332 = AXIS2_PLACEMENT_3D ( 'NONE', #52416, #9834, #63630 ) ;
#10333 = DIRECTION ( 'NONE',  ( 0.000000000000000000, 0.000000000000000000, -1.000000000000000000 ) ) ;
#10334 = CARTESIAN_POINT ( 'NONE',  ( -117.8929263765337794, -8.102448949553174629, -5.886773742842741797 ) ) ;
#10335 = AXIS2_PLACEMENT_3D ( 'NONE', #58902, #64525, #5074 ) ;
#10336 = EDGE_CURVE ( 'NONE', #39701, #60504, #597, .T. ) ;
#10337 = ORIENTED_EDGE ( 'NONE', *, *, #7612, .T. ) ;
#10338 = CIRCLE ( 'NONE', #49649, 1.000000000000000888 ) ;
#10339 = CARTESIAN_POINT ( 'NONE',  ( -160.4929263765338305, -8.102448949553172852, 5.886773742842742685 ) ) ;
#10340 =( LENGTH_UNIT ( ) NAMED_UNIT ( * ) SI_UNIT ( .MILLI., .METRE. ) );
#10341 = CARTESIAN_POINT ( 'NONE',  ( 21.75000000000001066, 22.24999999999998224, -4.000000000000000000 ) ) ;
#10342 = TOROIDAL_SURFACE ( 'NONE', #61807, 0.5000000000000000000, 0.2500000000000000000 ) ;
#10343 = EDGE_CURVE ( 'NONE', #49504, #23750, #11077, .T. ) ;
#10344 = ADVANCED_FACE ( 'NONE', ( #28396 ), #21778, .T. ) ;
#10345 = DIRECTION ( 'NONE',  ( 0.000000000000000000, 0.000000000000000000, 1.000000000000000000 ) ) ;
#10346 = DIRECTION ( 'NONE',  ( 0.000000000000000000, 0.000000000000000000, 1.000000000000000000 ) ) ;
#10347 =( NAMED_UNIT ( * ) SI_UNIT ( $, .STERADIAN. ) SOLID_ANGLE_UNIT ( ) );
#10348 = FILL_AREA_STYLE ('',( #4323 ) ) ;
#10349 = ORIENTED_EDGE ( 'NONE', *, *, #568, .F. ) ;
#10350 = CIRCLE ( 'NONE', #67627, 0.5000000000000004441 ) ;
#10351 = CARTESIAN_POINT ( 'NONE',  ( -71.54292637653379927, 9.058813317711329915, 2.943386871421369566 ) ) ;
#10352 = CONTEXT_DEPENDENT_SHAPE_REPRESENTATION ( #59917, #1382 ) ;
#10353 = FACE_OUTER_BOUND ( 'NONE', #50755, .T. ) ;
#10354 = CIRCLE ( 'NONE', #5797, 0.2500000000000002220 ) ;
#10355 = EDGE_CURVE ( 'NONE', #24259, #63980, #24573, .T. ) ;
#10356 = SURFACE_STYLE_FILL_AREA ( #10691 ) ;
#10357 = CARTESIAN_POINT ( 'NONE',  ( 2.607480562268988500, 146.7070736234661581, 8.025000000000062528 ) ) ;
#10358 = DIRECTION ( 'NONE',  ( -1.000000000000000000, -0.000000000000000000, -0.000000000000000000 ) ) ;
#10359 = CIRCLE ( 'NONE', #10195, 0.5000000000000004441 ) ;
#10360 = EDGE_CURVE ( 'NONE', #15634, #20172, #33582, .T. ) ;
#10361 = CARTESIAN_POINT ( 'NONE',  ( -182.0049999999999670, 6.826472737025115478, 4.959722759717899443 ) ) ;
#10362 =( GEOMETRIC_REPRESENTATION_CONTEXT ( 3 ) GLOBAL_UNCERTAINTY_ASSIGNED_CONTEXT ( ( #19439 ) ) GLOBAL_UNIT_ASSIGNED_CONTEXT ( ( #37249, #49763, #23029 ) ) REPRESENTATION_CONTEXT ( 'NONE', 'WORKASPACE' ) );
#10363 = VERTEX_POINT ( 'NONE', #27366 ) ;
#10364 = VECTOR ( 'NONE', #6638, 1000.000000000000000 ) ;
#10366 = SURFACE_STYLE_FILL_AREA ( #68761 ) ;
#10365 = B_SPLINE_CURVE_WITH_KNOTS ( 'NONE', 3,
 ( #66991, #61664, #35326, #18784, #62720, #19110, #29329, #40262, #14549, #61341 ),
 .UNSPECIFIED., .F., .F.,
 ( 4, 2, 2, 2, 4 ),
 ( 0.002117352549236312977, 0.002645155315643570038, 0.003172958082050826665, 0.003700760848458083292, 0.004228563614865340353 ),
 .UNSPECIFIED. ) ;
#10367 = LINE ( 'NONE', #37486, #37488 ) ;
#10368 = DIRECTION ( 'NONE',  ( -0.000000000000000000, -0.000000000000000000, -1.000000000000000000 ) ) ;
#10369 =( BOUNDED_CURVE ( )  B_SPLINE_CURVE ( 2, ( #57906, #41750, #51934, #10062, #47033, #36483, #9730, #31137, #2981, #62466, #67400 ),
 .UNSPECIFIED., .F., .F. ) 
 B_SPLINE_CURVE_WITH_KNOTS ( ( 3, 2, 2, 2, 2, 3 ),
 ( 0.4891304347825972121, 0.4913043478260754049, 0.4934782608695535977, 0.4956521739130318460, 0.4978260869565100388, 0.4999999999999882316 ),
 .UNSPECIFIED. ) 
 CURVE ( )  GEOMETRIC_REPRESENTATION_ITEM ( )  RATIONAL_B_SPLINE_CURVE ( ( 1.000000000000258682, 0.9510565162948948492, 1.000000000000000000, 0.9510565162951535312, 1.000000000000000000, 0.9510565162951535312, 1.000000000000000000, 0.9510565162951535312, 1.000000000000000000, 0.9510565162954184304, 0.9999999999997351008 ) ) 
 REPRESENTATION_ITEM ( '' )  );
#10370 = CARTESIAN_POINT ( 'NONE',  ( -181.8570736234661638, -5.598654528085803328, -7.705886871421366635 ) ) ;
#10371 = CARTESIAN_POINT ( 'NONE',  ( -6.826472737025120807, 142.5070736234661410, -4.959722759717907437 ) ) ;
#10372 = VECTOR ( 'NONE', #23701, 1000.000000000000114 ) ;
#10373 = ORIENTED_EDGE ( 'NONE', *, *, #807, .T. ) ;
#10374 = CARTESIAN_POINT ( 'NONE',  ( 11.00000000000000000, 8.000000000000000000, -3.500000000000017764 ) ) ;
#10375 = CARTESIAN_POINT ( 'NONE',  ( -95.90499999999998693, 2.607480562269069324, -8.024999999999993250 ) ) ;
#10376 = UNCERTAINTY_MEASURE_WITH_UNIT (LENGTH_MEASURE( 1.000000000000000082E-05 ), #14979, 'distance_accuracy_value', 'NONE');
#10377 = AXIS2_PLACEMENT_3D ( 'NONE', #48308, #21178, #31734 ) ;
#10378 = CARTESIAN_POINT ( 'NONE',  ( 6.826472737025119919, 132.0070736234661695, 4.959722759717908325 ) ) ;
#10379 = EDGE_LOOP ( 'NONE', ( #1366, #21730, #54317, #47809 ) ) ;
#10380 = CARTESIAN_POINT ( 'NONE',  ( 0.000000000000000000, -3.500000000000000000, 24.00000000000000000 ) ) ;
#10381 = CARTESIAN_POINT ( 'NONE',  ( -103.5570736234661808, -1.166476076187852838E-15, -9.524999999999991473 ) ) ;
#10382 = ADVANCED_FACE ( 'NONE', ( #22820, #59376 ), #11212, .T. ) ;
#10383 = SURFACE_STYLE_USAGE ( .BOTH. , #41711 ) ;
#10384 = ORIENTED_EDGE ( 'NONE', *, *, #9563, .F. ) ;
#10385 = DIRECTION ( 'NONE',  ( 0.000000000000000000, 0.000000000000000000, 1.000000000000000000 ) ) ;
#10386 = EDGE_CURVE ( 'NONE', #11113, #22147, #68438, .T. ) ;
#10387 = CARTESIAN_POINT ( 'NONE',  ( -73.94499999999997897, -9.827790563157499189E-16, -8.024999999999991473 ) ) ;
#10388 = ORIENTED_EDGE ( 'NONE', *, *, #55881, .T. ) ;
#10389 = DIRECTION ( 'NONE',  ( -1.000000000000000000, 0.000000000000000000, 0.000000000000000000 ) ) ;
#10390 = DIRECTION ( 'NONE',  ( 1.000000000000000000, 0.000000000000000000, 0.000000000000000000 ) ) ;
#10391 = ORIENTED_EDGE ( 'NONE', *, *, #21060, .T. ) ;
#10392 = PLANE ( 'NONE',  #13388 ) ;
#10393 = DIRECTION ( 'NONE',  ( -0.000000000000000000, -0.000000000000000000, 1.000000000000000000 ) ) ;
#10394 = AXIS2_PLACEMENT_3D ( 'NONE', #47724, #15339, #69457 ) ;
#10395 = DIRECTION ( 'NONE',  ( -9.376883653928687363E-17, 1.000000000000000000, 0.000000000000000000 ) ) ;
#10396 = CARTESIAN_POINT ( 'NONE',  ( 4.286263797015740046E-16, 2.500000000000000000, -3.500000000000003553 ) ) ;
#10397 = EDGE_LOOP ( 'NONE', ( #35111, #15687, #19596, #69541 ) ) ;
#10398 = CIRCLE ( 'NONE', #33966, 0.5000000000000004441 ) ;
#10399 = ORIENTED_EDGE ( 'NONE', *, *, #39600, .F. ) ;
#10400 = LINE ( 'NONE', #21624, #15138 ) ;
#10401 = CARTESIAN_POINT ( 'NONE',  ( -74.49999999999998579, 64.49137674618943095, -10.00000000000000000 ) ) ;
#10402 = CARTESIAN_POINT ( 'NONE',  ( -159.3570736234661922, 5.598654528085804216, 7.705886871421366635 ) ) ;
#10403 = MECHANICAL_DESIGN_GEOMETRIC_PRESENTATION_REPRESENTATION (  '', ( #17138 ), #35078 ) ;
#10404 = CARTESIAN_POINT ( 'NONE',  ( -8.102448949553179958, 118.8949999999999676, -5.886773742842749790 ) ) ;
#10405 = CARTESIAN_POINT ( 'NONE',  ( -91.70707362346614389, -3.094860106618431139, -9.524999999999991473 ) ) ;
#10406 = CARTESIAN_POINT ( 'NONE',  ( 53.24999999999999289, 27.99999999999998579, 3.750000000000000000 ) ) ;
#10407 = VERTEX_POINT ( 'NONE', #67804 ) ;
#10408 = CARTESIAN_POINT ( 'NONE',  ( -44.99999999999977973, 146.9999999999999716, -7.000000000000000000 ) ) ;
#10409 =( NAMED_UNIT ( * ) SI_UNIT ( $, .STERADIAN. ) SOLID_ANGLE_UNIT ( ) );
#10410 = AXIS2_PLACEMENT_3D ( 'NONE', #61944, #2461, #28883 ) ;
#10411 = CARTESIAN_POINT ( 'NONE',  ( -138.3550000000000182, -4.716976649647093289, -6.492361379858945902 ) ) ;
#10412 = SURFACE_SIDE_STYLE ('',( #58583 ) ) ;
#10413 = CARTESIAN_POINT ( 'NONE',  ( 0.000000000000000000, 24.74999999999998579, 3.750000000000000000 ) ) ;
#10414 = VECTOR ( 'NONE', #44610, 1000.000000000000000 ) ;
#10415 = EDGE_CURVE ( 'NONE', #51275, #20383, #35003, .T. ) ;
#10416 = CARTESIAN_POINT ( 'NONE',  ( -156.4449999999999932, 0.000000000000000000, 8.024999999999991473 ) ) ;
#10417 = CARTESIAN_POINT ( 'NONE',  ( -139.7950000000000159, 2.607480562269069324, -8.024999999999993250 ) ) ;
#10418 = ORIENTED_EDGE ( 'NONE', *, *, #20652, .T. ) ;
#10419 = DIRECTION ( 'NONE',  ( -0.000000000000000000, -0.000000000000000000, 1.000000000000000000 ) ) ;
#10420 = VECTOR ( 'NONE', #60544, 1000.000000000000000 ) ;
#10421 = CYLINDRICAL_SURFACE ( 'NONE', #65989, 0.5000000000000004441 ) ;
#10422 = EDGE_CURVE ( 'NONE', #66072, #46073, #19000, .T. ) ;
#10423 = SURFACE_STYLE_FILL_AREA ( #58593 ) ;
#10424 = CARTESIAN_POINT ( 'NONE',  ( -56.45499999999997698, 7.632228543268599452, -2.479861379858951942 ) ) ;
#10425 = COLOUR_RGB ( '', 0.09019608, 0.27058824, 0.51372549) ;
#10426 = ADVANCED_FACE ( 'NONE', ( #55507 ), #17955, .T. ) ;
#10427 = DIRECTION ( 'NONE',  ( 0.000000000000000000, -0.000000000000000000, 1.000000000000000000 ) ) ;
#10428 = DIRECTION ( 'NONE',  ( 0.7833176619561877940, -0.6216216216216191581, -4.313366480807175060E-15 ) ) ;
#10429 = VECTOR ( 'NONE', #1319, 1000.000000000000000 ) ;
#10430 = AXIS2_PLACEMENT_3D ( 'NONE', #55050, #23071, #17796 ) ;
#10431 = CARTESIAN_POINT ( 'NONE',  ( 41.49999999999998579, 99.99999999999998579, 3.500000000000000000 ) ) ;
#10432 =( GEOMETRIC_REPRESENTATION_CONTEXT ( 3 ) GLOBAL_UNCERTAINTY_ASSIGNED_CONTEXT ( ( #69162 ) ) GLOBAL_UNIT_ASSIGNED_CONTEXT ( ( #47899, #21093, #52100 ) ) REPRESENTATION_CONTEXT ( 'NONE', 'WORKASPACE' ) );
#10433 = CARTESIAN_POINT ( 'NONE',  ( 4.041451884327377897, 2.500000000000000000, 7.000000000000000888 ) ) ;
#10434 = SURFACE_STYLE_USAGE ( .BOTH. , #492 ) ;
#10435 = AXIS2_PLACEMENT_3D ( 'NONE', #9953, #41290, #42357 ) ;
#10436 = EDGE_CURVE ( 'NONE', #41309, #60166, #33634, .T. ) ;
#10437 = FACE_OUTER_BOUND ( 'NONE', #50232, .T. ) ;
#10438 = CIRCLE ( 'NONE', #49757, 0.2500000000000002220 ) ;
#10439 = DIRECTION ( 'NONE',  ( 0.000000000000000000, 1.000000000000000000, -0.000000000000000000 ) ) ;
#10440 = FACE_OUTER_BOUND ( 'NONE', #45474, .T. ) ;
#10441 = ORIENTED_EDGE ( 'NONE', *, *, #9488, .F. ) ;
#10442 = STYLED_ITEM ( 'NONE', ( #42692 ), #35833 ) ;
#10443 = CARTESIAN_POINT ( 'NONE',  ( -6.826472737025120807, 110.1070736234661496, 4.959722759717906548 ) ) ;
#10444 = AXIS2_PLACEMENT_3D ( 'NONE', #34167, #39134, #44078 ) ;
#10445 = LINE ( 'NONE', #36523, #39443 ) ;
#10446 = FILL_AREA_STYLE ('',( #36525 ) ) ;
#10447 = SURFACE_STYLE_FILL_AREA ( #48112 ) ;
#10448 = EDGE_LOOP ( 'NONE', ( #60854, #18106, #12544, #30309 ) ) ;
#10449 = ORIENTED_EDGE ( 'NONE', *, *, #13993, .T. ) ;
#10450 = CARTESIAN_POINT ( 'NONE',  ( -109.2570736234661837, 5.598654528085800663, -7.705886871421367523 ) ) ;
#10451 = SURFACE_STYLE_FILL_AREA ( #68852 ) ;
#10452 = AXIS2_PLACEMENT_3D ( 'NONE', #15198, #36662, #58087 ) ;
#10453 = ORIENTED_EDGE ( 'NONE', *, *, #12062, .F. ) ;
#10454 = CARTESIAN_POINT ( 'NONE',  ( -5.598654528085806881, 122.8549999999999898, -7.705886871421374629 ) ) ;
#10455 = DIRECTION ( 'NONE',  ( 0.000000000000000000, 0.000000000000000000, -1.000000000000000000 ) ) ;
#10456 =( NAMED_UNIT ( * ) PLANE_ANGLE_UNIT ( ) SI_UNIT ( $, .RADIAN. ) );
#10457 = AXIS2_PLACEMENT_3D ( 'NONE', #1149, #53980, #21272 ) ;
#10458 = CARTESIAN_POINT ( 'NONE',  ( 10.00000000000001954, 43.00000000000000000, 45.61250543006183733 ) ) ;
#10459 = ADVANCED_FACE ( 'NONE', ( #17491 ), #10049, .T. ) ;
#10460 = CARTESIAN_POINT ( 'NONE',  ( -102.5949999999999704, 2.607480562269073321, 8.024999999999991473 ) ) ;
#10461 = VERTEX_POINT ( 'NONE', #27978 ) ;
#10462 =( BOUNDED_CURVE ( )  B_SPLINE_CURVE ( 3, ( #40941, #20121, #67293, #35641 ),
 .UNSPECIFIED., .F., .F. ) 
 B_SPLINE_CURVE_WITH_KNOTS ( ( 4, 4 ),
 ( 1.570796326794896558, 3.141592653589793116 ),
 .UNSPECIFIED. ) 
 CURVE ( )  GEOMETRIC_REPRESENTATION_ITEM ( )  RATIONAL_B_SPLINE_CURVE ( ( 1.000000000000000000, 0.8047378541243649375, 0.8047378541243649375, 1.000000000000000000 ) ) 
 REPRESENTATION_ITEM ( '' )  );
#10463 = PRESENTATION_STYLE_ASSIGNMENT (( #59299 ) ) ;
#10464 = CARTESIAN_POINT ( 'NONE',  ( -140.0070736234661695, -8.102448949553174629, -5.886773742842741797 ) ) ;
#10465 = CARTESIAN_POINT ( 'NONE',  ( -48.00000000000000000, 14.49137674618942562, 9.500000000000000000 ) ) ;
#10466 = ORIENTED_EDGE ( 'NONE', *, *, #28648, .T. ) ;
#10467 = CARTESIAN_POINT ( 'NONE',  ( -4.716976649647098618, 151.1429263765338078, 6.492361379858953008 ) ) ;
#10468 = LINE ( 'NONE', #69209, #7682 ) ;
#10469 = CARTESIAN_POINT ( 'NONE',  ( 7.566679973970428463, 2.499999999999998224, 4.894125840469273570 ) ) ;
#10470 = DIRECTION ( 'NONE',  ( 1.000000000000000000, 0.000000000000000000, 0.000000000000000000 ) ) ;
#10471 = CARTESIAN_POINT ( 'NONE',  ( 20.06856914206998610, 114.9886858359306814, -10.44306996520268527 ) ) ;
#10472 = ORIENTED_EDGE ( 'NONE', *, *, #43855, .F. ) ;
#10473 = PRESENTATION_STYLE_ASSIGNMENT (( #30866 ) ) ;
#10474 = AXIS2_PLACEMENT_3D ( 'NONE', #42243, #59046, #25983 ) ;
#10475 = SURFACE_STYLE_USAGE ( .BOTH. , #42513 ) ;
#10476 = SURFACE_SIDE_STYLE ('',( #63584 ) ) ;
#10477 = COLOUR_RGB ( '', 0.08235294, 0.09019608, 0.10196078) ;
#10478 = SURFACE_STYLE_USAGE ( .BOTH. , #9445 ) ;
#10479 = DIRECTION ( 'NONE',  ( 0.000000000000000000, 0.000000000000000000, 1.000000000000000000 ) ) ;
#10480 = DIRECTION ( 'NONE',  ( -0.000000000000000000, -1.000000000000000000, -0.000000000000000000 ) ) ;
#10481 = CARTESIAN_POINT ( 'NONE',  ( -114.4429263765338050, -1.166476076187852838E-15, -9.524999999999991473 ) ) ;
#10482 = ORIENTED_EDGE ( 'NONE', *, *, #8962, .F. ) ;
#10483 = ORIENTED_EDGE ( 'NONE', *, *, #20972, .T. ) ;
#10484 = DIRECTION ( 'NONE',  ( 0.000000000000000000, -1.000000000000000000, 0.000000000000000000 ) ) ;
#10485 = LINE ( 'NONE', #17510, #8472 ) ;
#10486 = CARTESIAN_POINT ( 'NONE',  ( -100.5570736234661808, -1.166476076187852838E-15, -9.524999999999991473 ) ) ;
#10487 = PRESENTATION_STYLE_ASSIGNMENT (( #53719 ) ) ;
#10488 = ORIENTED_EDGE ( 'NONE', *, *, #42742, .T. ) ;
#10489 = CARTESIAN_POINT ( 'NONE',  ( -170.0049999999999955, 6.826472737025116366, 4.959722759717898555 ) ) ;
#10490 = CARTESIAN_POINT ( 'NONE',  ( -11.74999999999999645, -3.000000000000000000, 6.000000000000001776 ) ) ;
#10491 = LINE ( 'NONE', #53408, #12196 ) ;
#10492 = EDGE_CURVE ( 'NONE', #37645, #15154, #12510, .T. ) ;
#10493 = CARTESIAN_POINT ( 'NONE',  ( -181.1949999999999648, 8.437984349512085203, -1.550032578732815448E-15 ) ) ;
#10494 = STYLED_ITEM ( 'NONE', ( #21803 ), #36477 ) ;
#10495 = CARTESIAN_POINT ( 'NONE',  ( -166.0449999999999875, 7.632228543268600340, 2.479861379858949277 ) ) ;
#10496 = ORIENTED_EDGE ( 'NONE', *, *, #65603, .F. ) ;
#10497 = AXIS2_PLACEMENT_3D ( 'NONE', #16204, #5250, #69626 ) ;
#10498 = PRESENTATION_STYLE_ASSIGNMENT (( #69567 ) ) ;
#10499 = CARTESIAN_POINT ( 'NONE',  ( 2.816687638038913141E-15, 149.9999999999999716, 23.00000000000000355 ) ) ;
#10500 = CARTESIAN_POINT ( 'NONE',  ( -54.93556801395976663, -8.762778093175660032, -2.499999999999992895 ) ) ;
#10501 = CARTESIAN_POINT ( 'NONE',  ( -86.30499999999997840, 8.437984349512085203, -1.550032578732815448E-15 ) ) ;
#10502 = CARTESIAN_POINT ( 'NONE',  ( -15.00000000000000000, 8.000000000000000000, -4.000000000000000000 ) ) ;
#10503 = CARTESIAN_POINT ( 'NONE',  ( -74.96321444755994889, 35.57983959226599779, -9.691745531186823470 ) ) ;
#10504 = CIRCLE ( 'NONE', #29569, 29.50000000000000000 ) ;
#10505 = ADVANCED_FACE ( 'NONE', ( #44245 ), #16797, .T. ) ;
#10506 = CARTESIAN_POINT ( 'NONE',  ( -84.14499999999998181, -4.716976649647092401, 6.492361379858946790 ) ) ;
#10507 = CARTESIAN_POINT ( 'NONE',  ( -1.166476076187854022E-15, 139.0549999999999784, 9.525000000000000355 ) ) ;
#10508 = EDGE_CURVE ( 'NONE', #19236, #823, #65648, .T. ) ;
#10509 = CARTESIAN_POINT ( 'NONE',  ( -6.826472737025120807, 126.9929263765338163, 4.959722759717906548 ) ) ;
#10510 = CARTESIAN_POINT ( 'NONE',  ( -170.6929263765337623, 10.01517768586948698, -1.839758294383808966E-15 ) ) ;
#10511 = EDGE_CURVE ( 'NONE', #51968, #35469, #37929, .T. ) ;
#10512 = DIRECTION ( 'NONE',  ( 0.000000000000000000, 0.000000000000000000, 1.000000000000000000 ) ) ;
#10513 = VECTOR ( 'NONE', #47115, 1000.000000000000000 ) ;
#10514 = CARTESIAN_POINT ( 'NONE',  ( 7.511572993685799101E-16, -2.500000000000000000, -6.999999999999997335 ) ) ;
#10515 =( GEOMETRIC_REPRESENTATION_CONTEXT ( 3 ) GLOBAL_UNCERTAINTY_ASSIGNED_CONTEXT ( ( #13754 ) ) GLOBAL_UNIT_ASSIGNED_CONTEXT ( ( #5820, #54018, #69507 ) ) REPRESENTATION_CONTEXT ( 'NONE', 'WORKASPACE' ) );
#10516 = ORIENTED_EDGE ( 'NONE', *, *, #62562, .T. ) ;
#10517 = EDGE_CURVE ( 'NONE', #16804, #53241, #54941, .T. ) ;
#10518 = CARTESIAN_POINT ( 'NONE',  ( 8.082903768654761123, -1.417096231345241097, 9.294316082458970795E-16 ) ) ;
#10519 = EDGE_CURVE ( 'NONE', #15573, #20378, #20105, .T. ) ;
#10520 = MECHANICAL_DESIGN_GEOMETRIC_PRESENTATION_REPRESENTATION (  '', ( #65688 ), #50000 ) ;
#10521 =( NAMED_UNIT ( * ) PLANE_ANGLE_UNIT ( ) SI_UNIT ( $, .RADIAN. ) );
#10522 = DIRECTION ( 'NONE',  ( -1.000000000000000000, 0.000000000000000000, 0.000000000000000000 ) ) ;
#10523 = CARTESIAN_POINT ( 'NONE',  ( -6.826472737025120807, 137.1070736234661638, 4.959722759717906548 ) ) ;
#10524 = ORIENTED_EDGE ( 'NONE', *, *, #8118, .T. ) ;
#10526 = ORIENTED_EDGE ( 'NONE', *, *, #62572, .F. ) ;
#10525 =( GEOMETRIC_REPRESENTATION_CONTEXT ( 3 ) GLOBAL_UNCERTAINTY_ASSIGNED_CONTEXT ( ( #9386 ) ) GLOBAL_UNIT_ASSIGNED_CONTEXT ( ( #69509, #57578, #15395 ) ) REPRESENTATION_CONTEXT ( 'NONE', 'WORKASPACE' ) );
#10527 = AXIS2_PLACEMENT_3D ( 'NONE', #7645, #6966, #2306 ) ;
#10528 =( NAMED_UNIT ( * ) SI_UNIT ( $, .STERADIAN. ) SOLID_ANGLE_UNIT ( ) );
#10529 =( LENGTH_UNIT ( ) NAMED_UNIT ( * ) SI_UNIT ( .MILLI., .METRE. ) );
#10530 = DIRECTION ( 'NONE',  ( 0.000000000000000000, 0.000000000000000000, -1.000000000000000000 ) ) ;
#10531 = ORIENTED_EDGE ( 'NONE', *, *, #29644, .T. ) ;
#10532 = CARTESIAN_POINT ( 'NONE',  ( -120.0549999999999926, -9.827790563157499189E-16, -8.024999999999991473 ) ) ;
#10533 = ORIENTED_EDGE ( 'NONE', *, *, #8702, .T. ) ;
#10534 = PLANE ( 'NONE',  #18554 ) ;
#10535 = PRESENTATION_LAYER_ASSIGNMENT (  '', '', ( #61079 ) ) ;
#10536 = ORIENTED_EDGE ( 'NONE', *, *, #67587, .F. ) ;
#10537 = FILL_AREA_STYLE_COLOUR ( '', #41441 ) ;
#10538 = CARTESIAN_POINT ( 'NONE',  ( 21.25000000000001066, 24.99999999999998579, 4.000000000000000000 ) ) ;
#10539 = ORIENTED_EDGE ( 'NONE', *, *, #29145, .T. ) ;
#10540 = AXIS2_PLACEMENT_3D ( 'NONE', #65311, #37597, #53704 ) ;
#10541 = CARTESIAN_POINT ( 'NONE',  ( 3.129636159629258261E-31, -7.500000000000000888, 23.00000000000000000 ) ) ;
#10542 = CARTESIAN_POINT ( 'NONE',  ( -9.058813317711338797, 149.3449999999999989, 2.943386871421373563 ) ) ;
#10543 =( GEOMETRIC_REPRESENTATION_CONTEXT ( 3 ) GLOBAL_UNCERTAINTY_ASSIGNED_CONTEXT ( ( #2383 ) ) GLOBAL_UNIT_ASSIGNED_CONTEXT ( ( #3755, #31195, #14710 ) ) REPRESENTATION_CONTEXT ( 'NONE', 'WORKASPACE' ) );
#10544 = ORIENTED_EDGE ( 'NONE', *, *, #35592, .T. ) ;
#10545 = CARTESIAN_POINT ( 'NONE',  ( -4.390521455347703217, 1.510510638266201910, 9.000000000000001776 ) ) ;
#10546 = SURFACE_SIDE_STYLE ('',( #37319 ) ) ;
#10547 = DIRECTION ( 'NONE',  ( 1.000000000000000000, 0.000000000000000000, 0.000000000000000000 ) ) ;
#10548 = ORIENTED_EDGE ( 'NONE', *, *, #19704, .F. ) ;
#10549 = CARTESIAN_POINT ( 'NONE',  ( 4.716976649647096842, 127.7429263765338163, 6.492361379858953896 ) ) ;
#10550 = DIRECTION ( 'NONE',  ( 1.000000000000000000, -0.000000000000000000, -0.000000000000000000 ) ) ;
#10551 = DIRECTION ( 'NONE',  ( -0.4834014344020922671, 0.000000000000000000, 0.8753987966738359106 ) ) ;
#10552 =( GEOMETRIC_REPRESENTATION_CONTEXT ( 3 ) GLOBAL_UNCERTAINTY_ASSIGNED_CONTEXT ( ( #49671 ) ) GLOBAL_UNIT_ASSIGNED_CONTEXT ( ( #14794, #46487, #8805 ) ) REPRESENTATION_CONTEXT ( 'NONE', 'WORKASPACE' ) );
#10553 = PRESENTATION_LAYER_ASSIGNMENT (  '', '', ( #7185 ) ) ;
#10554 = FACE_OUTER_BOUND ( 'NONE', #55788, .T. ) ;
#10555 = ORIENTED_EDGE ( 'NONE', *, *, #22876, .F. ) ;
#10556 = LINE ( 'NONE', #59398, #68903 ) ;
#10557 = ORIENTED_EDGE ( 'NONE', *, *, #31768, .F. ) ;
#10558 = CARTESIAN_POINT ( 'NONE',  ( -59.99292637653379501, 8.102448949553171076, -5.886773742842744461 ) ) ;
#10559 = PLANE ( 'NONE',  #59231 ) ;
#10560 = DIRECTION ( 'NONE',  ( 0.000000000000000000, 0.000000000000000000, -1.000000000000000000 ) ) ;
#10561 = CARTESIAN_POINT ( 'NONE',  ( -145.1049999999999898, -6.826472737025115478, 4.959722759717900331 ) ) ;
#10562 = DIRECTION ( 'NONE',  ( 1.000000000000000000, 0.000000000000000000, 0.000000000000000000 ) ) ;
#10563 = CARTESIAN_POINT ( 'NONE',  ( 27.00000000000001776, 15.00000000000000000, -34.49999999999999289 ) ) ;
#10564 = CIRCLE ( 'NONE', #49878, 0.2500000000000002220 ) ;
#10565 =( GEOMETRIC_REPRESENTATION_CONTEXT ( 3 ) GLOBAL_UNCERTAINTY_ASSIGNED_CONTEXT ( ( #68616 ) ) GLOBAL_UNIT_ASSIGNED_CONTEXT ( ( #51543, #45948, #41030 ) ) REPRESENTATION_CONTEXT ( 'NONE', 'WORKASPACE' ) );
#10566 = DIRECTION ( 'NONE',  ( 0.000000000000000000, 0.000000000000000000, 1.000000000000000000 ) ) ;
#10567 =( NAMED_UNIT ( * ) SI_UNIT ( $, .STERADIAN. ) SOLID_ANGLE_UNIT ( ) );
#10568 =( LENGTH_UNIT ( ) NAMED_UNIT ( * ) SI_UNIT ( .MILLI., .METRE. ) );
#10569 = EDGE_LOOP ( 'NONE', ( #57356, #13841, #15267, #15570 ) ) ;
#10570 = EDGE_LOOP ( 'NONE', ( #34245, #56523, #58816, #37845 ) ) ;
#10571 = DIRECTION ( 'NONE',  ( 0.000000000000000000, -0.000000000000000000, 1.000000000000000000 ) ) ;
#10572 = CARTESIAN_POINT ( 'NONE',  ( -5.365183871890740974, 2.392512705203733159, 4.707228941936125288 ) ) ;
#10574 = CARTESIAN_POINT ( 'NONE',  ( -63.20499999999998408, -2.607480562269071545, -8.024999999999991473 ) ) ;
#10573 = VECTOR ( 'NONE', #44603, 1000.000000000000114 ) ;
#10575 = ORIENTED_EDGE ( 'NONE', *, *, #55164, .F. ) ;
#10576 = CARTESIAN_POINT ( 'NONE',  ( -74.99999999999998579, 50.00000000000000000, 11.50000000000003730 ) ) ;
#10577 = FACE_OUTER_BOUND ( 'NONE', #49099, .T. ) ;
#10578 = LINE ( 'NONE', #639, #14422 ) ;
#10579 = EDGE_CURVE ( 'NONE', #67895, #63907, #24623, .T. ) ;
#10580 = STYLED_ITEM ( 'NONE', ( #54962 ), #48654 ) ;
#10582 = EDGE_CURVE ( 'NONE', #1270, #57659, #5391, .T. ) ;
#10581 = ORIENTED_EDGE ( 'NONE', *, *, #38505, .F. ) ;
#10583 = SURFACE_STYLE_USAGE ( .BOTH. , #4949 ) ;
#10584 = CARTESIAN_POINT ( 'NONE',  ( -48.50000000000000000, 14.49137674618942562, -7.500000000000000000 ) ) ;
#10585 = EDGE_CURVE ( 'NONE', #64274, #46287, #33623, .T. ) ;
#10586 = VECTOR ( 'NONE', #66127, 1000.000000000000000 ) ;
#10587 = CARTESIAN_POINT ( 'NONE',  ( -112.0449999999999875, 7.632228543268600340, 2.479861379858949277 ) ) ;
#10588 = CARTESIAN_POINT ( 'NONE',  ( 5.598654528085805993, 153.2450000000000045, 7.705886871421374629 ) ) ;
#10589 = CARTESIAN_POINT ( 'NONE',  ( -85.49499999999999034, 6.826472737025113702, -4.959722759717902107 ) ) ;
#10590 = ADVANCED_FACE ( 'NONE', ( #22747 ), #2077, .T. ) ;
#10591 = DIRECTION ( 'NONE',  ( 0.000000000000000000, 1.000000000000000000, 0.000000000000000000 ) ) ;
#10592 = MECHANICAL_DESIGN_GEOMETRIC_PRESENTATION_REPRESENTATION (  '', ( #39791 ), #9439 ) ;
#10593 = DIRECTION ( 'NONE',  ( 0.000000000000000000, 0.000000000000000000, -1.000000000000000000 ) ) ;
#10594 = AXIS2_PLACEMENT_3D ( 'NONE', #65572, #59592, #38887 ) ;
#10595 = DIRECTION ( 'NONE',  ( 0.6402681315062906942, 0.000000000000000000, -0.7681514953298230752 ) ) ;
#10596 = PRESENTATION_LAYER_ASSIGNMENT (  '', '', ( #25195 ) ) ;
#10597 = EDGE_LOOP ( 'NONE', ( #54410, #11323, #43655 ) ) ;
#10598 = ADVANCED_FACE ( 'NONE', ( #28328 ), #7592, .T. ) ;
#10599 = CARTESIAN_POINT ( 'NONE',  ( -138.4429263765337907, -1.166476076187852838E-15, -9.524999999999991473 ) ) ;
#10600 =( GEOMETRIC_REPRESENTATION_CONTEXT ( 3 ) GLOBAL_UNCERTAINTY_ASSIGNED_CONTEXT ( ( #13823 ) ) GLOBAL_UNIT_ASSIGNED_CONTEXT ( ( #52497, #47602, #36691 ) ) REPRESENTATION_CONTEXT ( 'NONE', 'WORKASPACE' ) );
#10601 = CARTESIAN_POINT ( 'NONE',  ( -143.8449999999999989, -7.632228543268599452, 2.479861379858951054 ) ) ;
#10602 = AXIS2_PLACEMENT_3D ( 'NONE', #31518, #58610, #52999 ) ;
#10603 = CARTESIAN_POINT ( 'NONE',  ( -47.69499999999998607, -8.437984349512086979, 5.166775262442717831E-16 ) ) ;
#10604 = LINE ( 'NONE', #5636, #11362 ) ;
#10605 = ORIENTED_EDGE ( 'NONE', *, *, #13243, .T. ) ;
#10607 = ORIENTED_EDGE ( 'NONE', *, *, #16237, .T. ) ;
#10606 = COLOUR_RGB ( '', 0.66274510, 0.83137255, 0.94901961) ;
#10608 = DIRECTION ( 'NONE',  ( 0.000000000000000000, 0.000000000000000000, -1.000000000000000000 ) ) ;
#10609 = CARTESIAN_POINT ( 'NONE',  ( 0.000000000000000000, 116.9429263765338192, -8.025000000000000355 ) ) ;
#10610 = CARTESIAN_POINT ( 'NONE',  ( -45.91400648542629170, 9.424643574460597861, 6.049632038801588507 ) ) ;
#10611 = B_SPLINE_CURVE_WITH_KNOTS ( 'NONE', 3,
 ( #10514, #47499, #59350, #10164, #4507, #31598, #48521, #32292, #53081 ),
 .UNSPECIFIED., .F., .F.,
 ( 4, 2, 1, 2, 4 ),
 ( 0.008420575619166661974, 0.008943833652465347367, 0.009467091685764034495, 0.01051360775236140702, 0.01260663988555615379 ),
 .UNSPECIFIED. ) ;
#10612 = CARTESIAN_POINT ( 'NONE',  ( -151.0429263765337851, -9.058813317711329915, -2.943386871421370898 ) ) ;
#10613 = VERTEX_POINT ( 'NONE', #13206 ) ;
#10614 = CARTESIAN_POINT ( 'NONE',  ( -148.2549999999999955, -4.716976649647092401, 6.492361379858946790 ) ) ;
#10615 = VECTOR ( 'NONE', #57732, 1000.000000000000000 ) ;
#10616 = VERTEX_POINT ( 'NONE', #40675 ) ;
#10617 = SURFACE_STYLE_FILL_AREA ( #58802 ) ;
#10618 = LINE ( 'NONE', #41977, #51202 ) ;
#10619 = EDGE_LOOP ( 'NONE', ( #26445, #7362, #50589, #66174 ) ) ;
#10620 = COLOUR_RGB ( '', 0.08235294, 0.09019608, 0.10196078) ;
#10621 = PRESENTATION_STYLE_ASSIGNMENT (( #26759 ) ) ;
#10622 = CARTESIAN_POINT ( 'NONE',  ( 8.102448949553183510, 117.9949999999999761, -5.886773742842746238 ) ) ;
#10623 = DIRECTION ( 'NONE',  ( -0.000000000000000000, -0.000000000000000000, -1.000000000000000000 ) ) ;
#10624 = EDGE_CURVE ( 'NONE', #54061, #1147, #49022, .T. ) ;
#10625 = EDGE_LOOP ( 'NONE', ( #51374, #60549, #30181, #14162 ) ) ;
#10626 =( NAMED_UNIT ( * ) SI_UNIT ( $, .STERADIAN. ) SOLID_ANGLE_UNIT ( ) );
#10627 = CARTESIAN_POINT ( 'NONE',  ( -3.094860106618434248, 117.9049999999999727, 9.525000000000000355 ) ) ;
#10628 = CARTESIAN_POINT ( 'NONE',  ( -67.25499999999998124, -4.716976649647092401, 6.492361379858946790 ) ) ;
#10629 = CARTESIAN_POINT ( 'NONE',  ( -122.3949999999999818, -6.826472737025115478, -4.959722759717899443 ) ) ;
#10630 = CARTESIAN_POINT ( 'NONE',  ( -41.68184459379065032, 107.4432011401341640, -3.569690802414609010 ) ) ;
#10631 = ORIENTED_EDGE ( 'NONE', *, *, #2008, .T. ) ;
#10632 = CARTESIAN_POINT ( 'NONE',  ( 5.598654528085809545, 149.2549999999999955, -7.705886871421373741 ) ) ;
#10633 = DIRECTION ( 'NONE',  ( 1.000000000000000000, 0.000000000000000000, 0.000000000000000000 ) ) ;
#10634 = CARTESIAN_POINT ( 'NONE',  ( 45.00000000000000000, 99.99999999999992895, 4.000000000000000000 ) ) ;
#10635 = AXIS2_PLACEMENT_3D ( 'NONE', #8455, #67525, #3453 ) ;
#10636 =( LENGTH_UNIT ( ) NAMED_UNIT ( * ) SI_UNIT ( .MILLI., .METRE. ) );
#10637 = CARTESIAN_POINT ( 'NONE',  ( -15.98999599679679839, 146.4999999999999716, -7.500000000000000000 ) ) ;
#10638 = VERTEX_POINT ( 'NONE', #8310 ) ;
#10639 = CARTESIAN_POINT ( 'NONE',  ( -70.75000000000000000, -0.9999999999999995559, 20.00000000000000000 ) ) ;
#10641 =( NAMED_UNIT ( * ) SI_UNIT ( $, .STERADIAN. ) SOLID_ANGLE_UNIT ( ) );
#10640 = CIRCLE ( 'NONE', #29709, 0.2500000000000002220 ) ;
#10642 = CARTESIAN_POINT ( 'NONE',  ( -175.4049999999999727, -2.607480562269069768, 8.024999999999991473 ) ) ;
#10643 = ORIENTED_EDGE ( 'NONE', *, *, #47065, .F. ) ;
#10644 = DIRECTION ( 'NONE',  ( -1.000000000000000000, 0.000000000000000000, 0.000000000000000000 ) ) ;
#10645 = AXIS2_PLACEMENT_3D ( 'NONE', #15325, #41008, #36783 ) ;
#10646 = CARTESIAN_POINT ( 'NONE',  ( -48.50000000000000000, 14.49137674618942562, -9.500000000000000000 ) ) ;
#10647 = VECTOR ( 'NONE', #18290, 1000.000000000000000 ) ;
#10648 = FACE_OUTER_BOUND ( 'NONE', #53815, .T. ) ;
#10649 = EDGE_LOOP ( 'NONE', ( #6091, #42013, #57786, #61439 ) ) ;
#10650 = EDGE_CURVE ( 'NONE', #19696, #35085, #32507, .T. ) ;
#10651 = CARTESIAN_POINT ( 'NONE',  ( -96.35499999999997556, -4.716976649647093289, -6.492361379858945902 ) ) ;
#10652 = ORIENTED_EDGE ( 'NONE', *, *, #9040, .T. ) ;
#10653 = EDGE_CURVE ( 'NONE', #34825, #40596, #45953, .T. ) ;
#10654 =( NAMED_UNIT ( * ) SI_UNIT ( $, .STERADIAN. ) SOLID_ANGLE_UNIT ( ) );
#10655 = CARTESIAN_POINT ( 'NONE',  ( 60.00000000000000000, 1.797044900979284448E-15, 12.00000000000000000 ) ) ;
#10656 = CARTESIAN_POINT ( 'NONE',  ( -131.3070736234661524, -10.01517768586948698, 6.132527647946031529E-16 ) ) ;
#10657 = DIRECTION ( 'NONE',  ( 1.000000000000000000, 0.000000000000000000, 0.000000000000000000 ) ) ;
#10658 = SURFACE_STYLE_USAGE ( .BOTH. , #9640 ) ;
#10659 = CARTESIAN_POINT ( 'NONE',  ( -67.70707362346617231, -3.094860106618431139, -9.524999999999991473 ) ) ;
#10660 = EDGE_CURVE ( 'NONE', #25577, #26262, #26192, .T. ) ;
#10661 = AXIS2_PLACEMENT_3D ( 'NONE', #58328, #9119, #19295 ) ;
#10662 = COLOUR_RGB ( '', 0.31764706, 0.68627451, 0.89019608) ;
#10663 = CARTESIAN_POINT ( 'NONE',  ( -55.78467112892083435, -8.499999999999994671, 5.997393757699851058 ) ) ;
#10664 = ORIENTED_EDGE ( 'NONE', *, *, #39558, .T. ) ;
#10665 = CARTESIAN_POINT ( 'NONE',  ( 7.000000000000017764, 17.78868675966041835, -4.077457891279206668E-16 ) ) ;
#10666 = CARTESIAN_POINT ( 'NONE',  ( -115.4049999999999727, -2.607480562269069768, 8.024999999999991473 ) ) ;
#10667 = CARTESIAN_POINT ( 'NONE',  ( 10.01517768586949231, 123.6949999999999932, 1.839758294383810543E-15 ) ) ;
#10668 = CARTESIAN_POINT ( 'NONE',  ( -114.8949999999999818, 6.826472737025116366, 4.959722759717898555 ) ) ;
#10669 = EDGE_CURVE ( 'NONE', #33379, #35954, #25163, .T. ) ;
#10670 = AXIS2_PLACEMENT_3D ( 'NONE', #43464, #27185, #49376 ) ;
#10671 = AXIS2_PLACEMENT_3D ( 'NONE', #47431, #53015, #53364 ) ;
#10672 = CARTESIAN_POINT ( 'NONE',  ( 24.00000000000000355, 37.00000000000000000, -3.000000000000000000 ) ) ;
#10673 = FACE_OUTER_BOUND ( 'NONE', #38150, .T. ) ;
#10674 = VERTEX_POINT ( 'NONE', #47733 ) ;
#10675 = ADVANCED_FACE ( 'NONE', ( #14989 ), #10392, .T. ) ;
#10676 = CARTESIAN_POINT ( 'NONE',  ( -167.0929263765338249, 3.094860106618433360, 9.524999999999991473 ) ) ;
#10677 = SURFACE_STYLE_USAGE ( .BOTH. , #20889 ) ;
#10678 = CARTESIAN_POINT ( 'NONE',  ( -174.8950000000000102, 6.826472737025116366, 4.959722759717898555 ) ) ;
#10679 = AXIS2_PLACEMENT_3D ( 'NONE', #43279, #18486, #64681 ) ;
#10680 = CARTESIAN_POINT ( 'NONE',  ( -109.5570736234661666, -1.166476076187852838E-15, -9.524999999999991473 ) ) ;
#10681 = CIRCLE ( 'NONE', #17482, 0.5000000000000004441 ) ;
#10682 = CARTESIAN_POINT ( 'NONE',  ( -20.51914007124930706, 114.9043000146497207, -10.00000000000000000 ) ) ;
#10683 = LINE ( 'NONE', #27521, #47096 ) ;
#10684 = ORIENTED_EDGE ( 'NONE', *, *, #9889, .F. ) ;
#10685 = CARTESIAN_POINT ( 'NONE',  ( -76.49292637653381632, -8.102448949553172852, 5.886773742842742685 ) ) ;
#10686 = CONTEXT_DEPENDENT_SHAPE_REPRESENTATION ( #46940, #39115 ) ;
#10687 = MECHANICAL_DESIGN_GEOMETRIC_PRESENTATION_REPRESENTATION (  '', ( #61249 ), #56737 ) ;
#10688 = DIRECTION ( 'NONE',  ( 0.000000000000000000, 1.000000000000000000, 0.000000000000000000 ) ) ;
#10689 = SURFACE_SIDE_STYLE ('',( #14578 ) ) ;
#10690 = AXIS2_PLACEMENT_3D ( 'NONE', #64982, #69578, #16837 ) ;
#10691 = FILL_AREA_STYLE ('',( #5057 ) ) ;
#10692 = FACE_OUTER_BOUND ( 'NONE', #57781, .T. ) ;
#10693 = DIRECTION ( 'NONE',  ( 0.000000000000000000, 0.000000000000000000, -1.000000000000000000 ) ) ;
#10694 = CARTESIAN_POINT ( 'NONE',  ( -180.2049999999999841, -2.607480562269071545, -8.024999999999991473 ) ) ;
#10695 = VERTEX_POINT ( 'NONE', #68098 ) ;
#10696 = CARTESIAN_POINT ( 'NONE',  ( 12.25000000000000355, 30.74999999999998579, 4.000000000000000000 ) ) ;
#10697 = DIRECTION ( 'NONE',  ( 0.000000000000000000, -1.000000000000000000, 0.000000000000000000 ) ) ;
#10698 = FILL_AREA_STYLE ('',( #64150 ) ) ;
#10699 = CARTESIAN_POINT ( 'NONE',  ( 0.000000000000000000, 139.0570736234661808, -8.025000000000000355 ) ) ;
#10700 = B_SPLINE_CURVE_WITH_KNOTS ( 'NONE', 3,
 ( #58005, #31936, #63606, #59339, #31226, #31582, #64291, #16498, #53065, #25954 ),
 .UNSPECIFIED., .F., .F.,
 ( 4, 2, 2, 2, 4 ),
 ( 0.009262909725840906203, 0.01194559479670475113, 0.01328693733213667447, 0.01395760859985263613, 0.01462827986756859780 ),
 .UNSPECIFIED. ) ;
#10701 = CIRCLE ( 'NONE', #42245, 0.5000000000000000000 ) ;
#10702 = EDGE_CURVE ( 'NONE', #51757, #47479, #16033, .T. ) ;
#10703 = ORIENTED_EDGE ( 'NONE', *, *, #3718, .T. ) ;
#10704 = CARTESIAN_POINT ( 'NONE',  ( 40.99999999999997868, 9.999999999999978684, -3.000000000000000444 ) ) ;
#10705 = CARTESIAN_POINT ( 'NONE',  ( -94.70499999999998408, 2.607480562269072433, 8.024999999999991473 ) ) ;
#10706 = EDGE_LOOP ( 'NONE', ( #67577, #7101, #48727, #13233 ) ) ;
#10707 = CARTESIAN_POINT ( 'NONE',  ( 75.00000000000000000, 19.30628705663858113, -6.999999999999999112 ) ) ;
#10708 = CIRCLE ( 'NONE', #2779, 1.000000000000000888 ) ;
#10709 = CARTESIAN_POINT ( 'NONE',  ( 7.632228543268608334, 143.3429263765338249, -2.479861379858951942 ) ) ;
#10710 = LINE ( 'NONE', #32164, #6304 ) ;
#10711 = SURFACE_STYLE_USAGE ( .BOTH. , #32487 ) ;
#10712 = SURFACE_SIDE_STYLE ('',( #5078 ) ) ;
#10713 = CIRCLE ( 'NONE', #69122, 2.000000000000001776 ) ;
#10714 = ORIENTED_EDGE ( 'NONE', *, *, #16715, .T. ) ;
#10715 = FILL_AREA_STYLE ('',( #23008 ) ) ;
#10716 = CARTESIAN_POINT ( 'NONE',  ( -68.99499999999999034, -6.826472737025115478, 4.959722759717900331 ) ) ;
#10717 = ORIENTED_EDGE ( 'NONE', *, *, #8032, .F. ) ;
#10718 = CARTESIAN_POINT ( 'NONE',  ( 4.750000000000002665, 24.74999999999998579, -3.750000000000000000 ) ) ;
#10719 = ADVANCED_FACE ( 'NONE', ( #10039 ), #48279, .F. ) ;
#10720 = FACE_OUTER_BOUND ( 'NONE', #4124, .T. ) ;
#10721 = CARTESIAN_POINT ( 'NONE',  ( -125.9070736234668715, -3.094860106606598382, 9.525000000008585488 ) ) ;
#10722 = EDGE_CURVE ( 'NONE', #62143, #15151, #56071, .T. ) ;
#10723 = ORIENTED_EDGE ( 'NONE', *, *, #26813, .F. ) ;
#10724 = SURFACE_SIDE_STYLE ('',( #48747 ) ) ;
#10725 = EDGE_CURVE ( 'NONE', #13821, #34386, #53303, .T. ) ;
#10726 = DIRECTION ( 'NONE',  ( -0.000000000000000000, -0.000000000000000000, -1.000000000000000000 ) ) ;
#10727 = STYLED_ITEM ( 'NONE', ( #56358 ), #39122 ) ;
#10728 = PRESENTATION_STYLE_ASSIGNMENT (( #42436 ) ) ;
#10729 = CARTESIAN_POINT ( 'NONE',  ( -119.3049999999999926, 8.437984349512085203, -1.550032578732815448E-15 ) ) ;
#10730 = VERTEX_POINT ( 'NONE', #63149 ) ;
#10731 = EDGE_CURVE ( 'NONE', #66069, #59058, #40373, .T. ) ;
#10732 = CARTESIAN_POINT ( 'NONE',  ( -9.985360875542991010, 1.514639124457108244, -0.7048476316491002480 ) ) ;
#10733 = AXIS2_PLACEMENT_3D ( 'NONE', #15582, #49314, #10975 ) ;
#10734 = VERTEX_POINT ( 'NONE', #36463 ) ;
#10735 = CARTESIAN_POINT ( 'NONE',  ( -44.99999999999977973, 149.4999999999999716, 10.00000000000000000 ) ) ;
#10736 =( NAMED_UNIT ( * ) PLANE_ANGLE_UNIT ( ) SI_UNIT ( $, .RADIAN. ) );
#10737 =( NAMED_UNIT ( * ) SI_UNIT ( $, .STERADIAN. ) SOLID_ANGLE_UNIT ( ) );
#10738 = CARTESIAN_POINT ( 'NONE',  ( -161.0070736234661410, -8.102448949553172852, -5.886773742842741797 ) ) ;
#10739 = CARTESIAN_POINT ( 'NONE',  ( 3.094860106618435136, 124.2949999999999733, -9.525000000000000355 ) ) ;
#10740 = AXIS2_PLACEMENT_3D ( 'NONE', #28850, #2418, #17648 ) ;
#10741 = CARTESIAN_POINT ( 'NONE',  ( -95.00707362346616947, -8.102448949553172852, -5.886773742842741797 ) ) ;
#10742 = EDGE_CURVE ( 'NONE', #69397, #2052, #9348, .T. ) ;
#10743 = AXIS2_PLACEMENT_3D ( 'NONE', #23381, #61686, #66655 ) ;
#10744 = DIRECTION ( 'NONE',  ( 0.000000000000000000, 0.000000000000000000, 1.000000000000000000 ) ) ;
#10745 = ORIENTED_EDGE ( 'NONE', *, *, #52216, .F. ) ;
#10746 = CYLINDRICAL_SURFACE ( 'NONE', #39688, 0.9999999999999998890 ) ;
#10747 = ADVANCED_FACE ( 'NONE', ( #68427 ), #20938, .F. ) ;
#10749 = CARTESIAN_POINT ( 'NONE',  ( 18.99979856674334044, 49.77026365512251971, 12.50000000000000000 ) ) ;
#10748 = CARTESIAN_POINT ( 'NONE',  ( -18.25000000000000711, 31.24999999999999289, -4.000000000000000000 ) ) ;
#10750 = CARTESIAN_POINT ( 'NONE',  ( -4.716976649647097730, 130.3570736234661638, -6.492361379858953896 ) ) ;
#10751 = CARTESIAN_POINT ( 'NONE',  ( -139.2549999999999955, -4.716976649647092401, 6.492361379858946790 ) ) ;
#10752 = CARTESIAN_POINT ( 'NONE',  ( -85.55707362346618083, -1.166476076187852838E-15, -9.524999999999991473 ) ) ;
#10753 = CARTESIAN_POINT ( 'NONE',  ( 1.000000000000000000, 0.000000000000000000, 3.000000000000000000 ) ) ;
#10754 = CARTESIAN_POINT ( 'NONE',  ( 41.06069799967658440, 107.9552192246431730, 3.682425535826294727 ) ) ;
#10755 = CARTESIAN_POINT ( 'NONE',  ( -144.7449999999999761, 4.716976649647094177, 6.492361379858945902 ) ) ;
#10756 = CARTESIAN_POINT ( 'NONE',  ( -138.1449999999999818, -4.716976649647092401, 6.492361379858946790 ) ) ;
#10757 = ORIENTED_EDGE ( 'NONE', *, *, #68917, .T. ) ;
#10758 = FILL_AREA_STYLE_COLOUR ( '', #15676 ) ;
#10759 = CARTESIAN_POINT ( 'NONE',  ( -74.99999999999998579, 50.00000000000000000, 7.000000000000000000 ) ) ;
#10760 = UNCERTAINTY_MEASURE_WITH_UNIT (LENGTH_MEASURE( 1.000000000000000082E-05 ), #45869, 'distance_accuracy_value', 'NONE');
#10761 = CARTESIAN_POINT ( 'NONE',  ( -55.85499999999998977, 4.716976649647094177, 6.492361379858945902 ) ) ;
#10762 = CARTESIAN_POINT ( 'NONE',  ( -138.8929263765338078, -8.102448949553174629, -5.886773742842741797 ) ) ;
#10763 =( LENGTH_UNIT ( ) NAMED_UNIT ( * ) SI_UNIT ( .MILLI., .METRE. ) );
#10764 = DIRECTION ( 'NONE',  ( 0.000000000000000000, 0.000000000000000000, 1.000000000000000000 ) ) ;
#10765 = AXIS2_PLACEMENT_3D ( 'NONE', #4806, #42844, #42491 ) ;
#10766 = CIRCLE ( 'NONE', #50096, 1.000000000000000888 ) ;
#10767 = CARTESIAN_POINT ( 'NONE',  ( -190.0000000000000000, 0.000000000000000000, 7.499999999999985789 ) ) ;
#10768 = EDGE_CURVE ( 'NONE', #51977, #19151, #20223, .T. ) ;
#10770 =( BOUNDED_CURVE ( )  B_SPLINE_CURVE ( 2, ( #23213, #44707, #17927, #39416, #52035, #7706, #62551, #34445, #30184, #24236, #51325 ),
 .UNSPECIFIED., .F., .F. ) 
 B_SPLINE_CURVE_WITH_KNOTS ( ( 3, 2, 2, 2, 2, 3 ),
 ( 0.1470588235294118806, 0.1529411764705883026, 0.1588235294117646967, 0.1647058823529411464, 0.1705882352941175684, 0.1764705882352939903 ),
 .UNSPECIFIED. ) 
 CURVE ( )  GEOMETRIC_REPRESENTATION_ITEM ( )  RATIONAL_B_SPLINE_CURVE ( ( 0.9999999999999991118, 0.9510565162951544194, 1.000000000000000000, 0.9510565162951535312, 1.000000000000000000, 0.9510565162951535312, 1.000000000000000000, 0.9510565162951535312, 1.000000000000000000, 0.9510565162951546414, 0.9999999999999988898 ) ) 
 REPRESENTATION_ITEM ( '' )  );
#10769 = CARTESIAN_POINT ( 'NONE',  ( -107.8429263765338106, 9.058813317711329915, -2.943386871421373119 ) ) ;
#10771 = DIRECTION ( 'NONE',  ( 8.326672684688674053E-17, -0.1585527532634884440, 0.9873505073845698643 ) ) ;
#10772 =( NAMED_UNIT ( * ) SI_UNIT ( $, .STERADIAN. ) SOLID_ANGLE_UNIT ( ) );
#10773 = CARTESIAN_POINT ( 'NONE',  ( 3.999798566743338668, 8.867945265733711224, -11.56480034751363917 ) ) ;
#10774 = DIRECTION ( 'NONE',  ( 0.000000000000000000, 1.000000000000000000, 0.000000000000000000 ) ) ;
#10775 = MECHANICAL_DESIGN_GEOMETRIC_PRESENTATION_REPRESENTATION (  '', ( #1732 ), #17530 ) ;
#10776 = DIRECTION ( 'NONE',  ( 0.000000000000000000, 0.000000000000000000, -1.000000000000000000 ) ) ;
#10777 = CARTESIAN_POINT ( 'NONE',  ( -74.99999999999998579, 50.00000000000000000, 10.50000000000000000 ) ) ;
#10778 = FACE_OUTER_BOUND ( 'NONE', #22050, .T. ) ;
#10779 = VECTOR ( 'NONE', #30254, 1000.000000000000000 ) ;
#10780 = EDGE_LOOP ( 'NONE', ( #28332, #4960, #53302 ) ) ;
#10781 = CARTESIAN_POINT ( 'NONE',  ( -24.00000000000000000, 1.000000000000000000, 3.000000000000000000 ) ) ;
#10783 = CARTESIAN_POINT ( 'NONE',  ( -6.826472737025120807, 112.5070736234661410, -4.959722759717907437 ) ) ;
#10782 =( GEOMETRIC_REPRESENTATION_CONTEXT ( 3 ) GLOBAL_UNCERTAINTY_ASSIGNED_CONTEXT ( ( #33422 ) ) GLOBAL_UNIT_ASSIGNED_CONTEXT ( ( #49212, #7655, #17227 ) ) REPRESENTATION_CONTEXT ( 'NONE', 'WORKASPACE' ) );
#10784 = B_SPLINE_CURVE_WITH_KNOTS ( 'NONE', 3,
 ( #28768, #1657, #44664, #29094, #65726, #54801, #7339, #39371, #18587, #33706, #55860, #34407 ),
 .UNSPECIFIED., .F., .F.,
 ( 4, 2, 2, 2, 2, 4 ),
 ( 0.000000000000000000, 0.0009366607938385700409, 0.001404991190757859994, 0.001639156389217507953, 0.001756238988447332908, 0.001873321587677158296 ),
 .UNSPECIFIED. ) ;
#10785 = DIRECTION ( 'NONE',  ( 0.000000000000000000, -1.000000000000000000, 0.000000000000000000 ) ) ;
#10786 = SURFACE_STYLE_USAGE ( .BOTH. , #22371 ) ;
#10787 = ORIENTED_EDGE ( 'NONE', *, *, #53929, .F. ) ;
#10788 = ORIENTED_EDGE ( 'NONE', *, *, #23196, .T. ) ;
#10789 = LINE ( 'NONE', #20994, #12959 ) ;
#10790 = FILL_AREA_STYLE ('',( #4809 ) ) ;
#10791 = ORIENTED_EDGE ( 'NONE', *, *, #39502, .T. ) ;
#10792 = CARTESIAN_POINT ( 'NONE',  ( 9.058813317711338797, 130.9549999999999841, -2.943386871421372675 ) ) ;
#10793 = PLANE ( 'NONE',  #25433 ) ;
#10794 = DIRECTION ( 'NONE',  ( 0.000000000000000000, 0.000000000000000000, -1.000000000000000000 ) ) ;
#10795 = DIRECTION ( 'NONE',  ( 0.000000000000000000, 0.000000000000000000, 1.000000000000000000 ) ) ;
#10796 = CARTESIAN_POINT ( 'NONE',  ( -104.3949999999999960, -6.826472737025115478, -4.959722759717899443 ) ) ;
#10797 = EDGE_LOOP ( 'NONE', ( #67933, #3816, #21896, #45681 ) ) ;
#10798 = AXIS2_PLACEMENT_3D ( 'NONE', #40134, #66848, #12661 ) ;
#10799 = CARTESIAN_POINT ( 'NONE',  ( 8.459058532691745569, 153.5028685191038562, -1.153563530786663405 ) ) ;
#10800 = ADVANCED_FACE ( 'NONE', ( #69463 ), #11178, .T. ) ;
#10801 = ORIENTED_EDGE ( 'NONE', *, *, #52222, .F. ) ;
#10802 = CARTESIAN_POINT ( 'NONE',  ( 6.826472737025121695, 152.4929263765338590, -4.959722759717905660 ) ) ;
#10803 = FACE_OUTER_BOUND ( 'NONE', #59369, .T. ) ;
#10804 = DIRECTION ( 'NONE',  ( 0.000000000000000000, 0.000000000000000000, 1.000000000000000000 ) ) ;
#10805 = ADVANCED_FACE ( 'NONE', ( #58216 ), #2172, .T. ) ;
#10806 = CARTESIAN_POINT ( 'NONE',  ( -20.74185979783655043, 149.7721295005298714, -9.939118314201632387 ) ) ;
#10807 = DIRECTION ( 'NONE',  ( 1.000000000000000000, -1.445602896647339656E-16, -0.000000000000000000 ) ) ;
#10808 = VERTEX_POINT ( 'NONE', #41373 ) ;
#10809 = DIRECTION ( 'NONE',  ( 1.000000000000000000, 0.000000000000000000, 0.000000000000000000 ) ) ;
#10810 = STYLED_ITEM ( 'NONE', ( #13118 ), #49883 ) ;
#10811 = CARTESIAN_POINT ( 'NONE',  ( 5.196152422706631135, 1.107695154586740394, 9.000000000000001776 ) ) ;
#10812 = CARTESIAN_POINT ( 'NONE',  ( 1.189524669241243060E-16, -7.500000000000000888, 24.00000000000000000 ) ) ;
#10813 = CARTESIAN_POINT ( 'NONE',  ( -23.21231517720797655, 117.9999999999999716, -7.500000000000000000 ) ) ;
#10814 = FILL_AREA_STYLE_COLOUR ( '', #37579 ) ;
#10815 = FILL_AREA_STYLE_COLOUR ( '', #22878 ) ;
#10816 = CARTESIAN_POINT ( 'NONE',  ( 23.21231517720797655, 112.9999999999999858, 9.500000000000000000 ) ) ;
#10817 = CARTESIAN_POINT ( 'NONE',  ( 22.00000000000000711, 43.00000000000000000, -45.61250543006183733 ) ) ;
#10818 = CARTESIAN_POINT ( 'NONE',  ( -7.239872073591128832, 153.7812473723182904, 5.042250455018151278 ) ) ;
#10819 = EDGE_LOOP ( 'NONE', ( #51073, #63855, #44445, #30515 ) ) ;
#10820 = ORIENTED_EDGE ( 'NONE', *, *, #42468, .T. ) ;
#10821 = CARTESIAN_POINT ( 'NONE',  ( -49.25707362346617657, 5.598654528085800663, -7.705886871421367523 ) ) ;
#10822 = DIRECTION ( 'NONE',  ( -1.000000000000000000, 0.000000000000000000, 0.000000000000000000 ) ) ;
#10823 = EDGE_CURVE ( 'NONE', #68013, #66131, #37099, .T. ) ;
#10824 = DIRECTION ( 'NONE',  ( 1.000000000000000000, 0.000000000000000000, 0.000000000000000000 ) ) ;
#10826 = VERTEX_POINT ( 'NONE', #52950 ) ;
#10825 = STYLED_ITEM ( 'NONE', ( #20385 ), #39675 ) ;
#10827 = FILL_AREA_STYLE ('',( #50803 ) ) ;
#10828 = CARTESIAN_POINT ( 'NONE',  ( -168.0550000000000068, -9.827790563157499189E-16, -8.024999999999991473 ) ) ;
#10829 = CARTESIAN_POINT ( 'NONE',  ( -195.0000000000000000, 0.000000000000000000, 0.000000000000000000 ) ) ;
#10830 = DIRECTION ( 'NONE',  ( 0.000000000000000000, 0.000000000000000000, 1.000000000000000000 ) ) ;
#10831 = CARTESIAN_POINT ( 'NONE',  ( -176.3949999999999818, -6.826472737025115478, -4.959722759717899443 ) ) ;
#10832 = VECTOR ( 'NONE', #3956, 1000.000000000000000 ) ;
#10833 = CARTESIAN_POINT ( 'NONE',  ( -163.9449999999999932, -9.827790563157499189E-16, -8.024999999999991473 ) ) ;
#10834 = VERTEX_POINT ( 'NONE', #31463 ) ;
#10835 = CARTESIAN_POINT ( 'NONE',  ( -23.21231517720797655, 117.4999999999999716, 9.500000000000000000 ) ) ;
#10836 = DIRECTION ( 'NONE',  ( 0.000000000000000000, 1.224646799147353207E-16, -1.000000000000000000 ) ) ;
#10837 =( NAMED_UNIT ( * ) SI_UNIT ( $, .STERADIAN. ) SOLID_ANGLE_UNIT ( ) );
#10838 = CARTESIAN_POINT ( 'NONE',  ( -83.45499999999998408, 7.632228543268599452, -2.479861379858951942 ) ) ;
#10839 = CARTESIAN_POINT ( 'NONE',  ( -195.0000000000000000, 0.000000000000000000, 0.000000000000000000 ) ) ;
#10840 = CARTESIAN_POINT ( 'NONE',  ( 17.15973193263811680, -3.000000000000000000, 2.000000000000000000 ) ) ;
#10841 = CARTESIAN_POINT ( 'NONE',  ( -74.99506141310581597, 35.51815782338716332, -9.580134848897966293 ) ) ;
#10842 = CARTESIAN_POINT ( 'NONE',  ( -81.29499999999997328, -2.607480562269069768, 8.024999999999991473 ) ) ;
#10843 = CARTESIAN_POINT ( 'NONE',  ( -8.102448949553181734, 135.0050000000000239, -5.886773742842749790 ) ) ;
#10844 = ADVANCED_FACE ( 'NONE', ( #4738 ), #22308, .T. ) ;
#10845 = CARTESIAN_POINT ( 'NONE',  ( -4.716976649647098618, 127.1429263765338220, 6.492361379858953008 ) ) ;
#10846 = CARTESIAN_POINT ( 'NONE',  ( 4.041451884327379673, -7.000000000000002665, 1.082903768654758903 ) ) ;
#10847 = CARTESIAN_POINT ( 'NONE',  ( 48.50000000000000000, 22.24999999999998579, 3.750000000000000000 ) ) ;
#10848 = ADVANCED_FACE ( 'NONE', ( #15667 ), #6133, .T. ) ;
#10849 = UNCERTAINTY_MEASURE_WITH_UNIT (LENGTH_MEASURE( 1.000000000000000082E-05 ), #35251, 'distance_accuracy_value', 'NONE');
#10850 = CARTESIAN_POINT ( 'NONE',  ( -74.24292637653380211, 5.598654528085804216, 7.705886871421366635 ) ) ;
#10851 = DIRECTION ( 'NONE',  ( 0.000000000000000000, 0.000000000000000000, 1.000000000000000000 ) ) ;
#10852 = ORIENTED_EDGE ( 'NONE', *, *, #65124, .F. ) ;
#10853 = MECHANICAL_DESIGN_GEOMETRIC_PRESENTATION_REPRESENTATION (  '', ( #36762 ), #69260 ) ;
#10854 = FILL_AREA_STYLE_COLOUR ( '', #50661 ) ;
#10855 = CARTESIAN_POINT ( 'NONE',  ( 18.25000000000000711, 33.74999999999999289, 4.000000000000000000 ) ) ;
#10856 =( GEOMETRIC_REPRESENTATION_CONTEXT ( 3 ) GLOBAL_UNCERTAINTY_ASSIGNED_CONTEXT ( ( #48309 ) ) GLOBAL_UNIT_ASSIGNED_CONTEXT ( ( #47805, #31894, #16107 ) ) REPRESENTATION_CONTEXT ( 'NONE', 'WORKASPACE' ) );
#10858 = DIRECTION ( 'NONE',  ( 0.000000000000000000, 0.000000000000000000, -1.000000000000000000 ) ) ;
#10857 =( NAMED_UNIT ( * ) PLANE_ANGLE_UNIT ( ) SI_UNIT ( $, .RADIAN. ) );
#10859 =( NAMED_UNIT ( * ) PLANE_ANGLE_UNIT ( ) SI_UNIT ( $, .RADIAN. ) );
#10860 = VERTEX_POINT ( 'NONE', #54988 ) ;
#10861 = ORIENTED_EDGE ( 'NONE', *, *, #4694, .T. ) ;
#10862 = CYLINDRICAL_SURFACE ( 'NONE', #34053, 0.5000000000000004441 ) ;
#10863 = CARTESIAN_POINT ( 'NONE',  ( 7.632228543268608334, 131.3429263765338249, -2.479861379858951942 ) ) ;
#10864 =( BOUNDED_CURVE ( )  B_SPLINE_CURVE ( 2, ( #52702, #4469, #25936, #67132, #46058, #19268, #62194, #56927, #63918, #64272, #188 ),
 .UNSPECIFIED., .F., .F. ) 
 B_SPLINE_CURVE_WITH_KNOTS ( ( 3, 2, 2, 2, 2, 3 ),
 ( 0.1764705882352939903, 0.1823529411764704400, 0.1882352941176469174, 0.1941176470588234226, 0.1999999999999999001, 0.2058823529411763498 ),
 .UNSPECIFIED. ) 
 CURVE ( )  GEOMETRIC_REPRESENTATION_ITEM ( )  RATIONAL_B_SPLINE_CURVE ( ( 1.000000000000001110, 0.9510565162951523099, 1.000000000000000000, 0.9510565162951535312, 1.000000000000000000, 0.9510565162951535312, 1.000000000000000000, 0.9510565162951535312, 1.000000000000000000, 0.9510565162951544194, 0.9999999999999991118 ) ) 
 REPRESENTATION_ITEM ( '' )  );
#10865 = CARTESIAN_POINT ( 'NONE',  ( 0.000000000000000000, 87.30187232391182306, 0.000000000000000000 ) ) ;
#10866 = LINE ( 'NONE', #22812, #62159 ) ;
#10867 = ORIENTED_EDGE ( 'NONE', *, *, #33921, .F. ) ;
#10868 = CARTESIAN_POINT ( 'NONE',  ( -115.2549999999999955, -4.716976649647092401, 6.492361379858946790 ) ) ;
#10869 = EDGE_LOOP ( 'NONE', ( #60774, #46709, #57154, #29097 ) ) ;
#10870 = CARTESIAN_POINT ( 'NONE',  ( -138.0570736234661808, 0.000000000000000000, 9.524999999999991473 ) ) ;
#10871 = PRESENTATION_LAYER_ASSIGNMENT (  '', '', ( #4067 ) ) ;
#10872 = DIRECTION ( 'NONE',  ( 0.000000000000000000, 0.000000000000000000, 1.000000000000000000 ) ) ;
#10873 = ORIENTED_EDGE ( 'NONE', *, *, #27339, .T. ) ;
#10874 = FILL_AREA_STYLE_COLOUR ( '', #35850 ) ;
#10875 = DIRECTION ( 'NONE',  ( 0.000000000000000000, 0.000000000000000000, -1.000000000000000000 ) ) ;
#10876 = EDGE_LOOP ( 'NONE', ( #28210, #6737, #22634, #42000 ) ) ;
#10877 = EDGE_CURVE ( 'NONE', #32066, #69681, #47191, .T. ) ;
#10878 = CARTESIAN_POINT ( 'NONE',  ( 61.74999999999998579, 30.74999999999999289, 4.000000000000000000 ) ) ;
#10879 = CARTESIAN_POINT ( 'NONE',  ( 8.102448949553181734, 159.3949999999999534, 5.886773742842750679 ) ) ;
#10880 = CARTESIAN_POINT ( 'NONE',  ( 24.21231517720798010, 113.4999999999999858, -7.000000000000000000 ) ) ;
#10881 = ORIENTED_EDGE ( 'NONE', *, *, #61431, .T. ) ;
#10882 = DIRECTION ( 'NONE',  ( 0.000000000000000000, 0.000000000000000000, 1.000000000000000000 ) ) ;
#10883 = PRESENTATION_STYLE_ASSIGNMENT (( #31985 ) ) ;
#10884 = FILL_AREA_STYLE ('',( #63989 ) ) ;
#10885 = CARTESIAN_POINT ( 'NONE',  ( -181.7929263765338135, -3.094860106617829398, 9.525000000000428457 ) ) ;
#10886 = ORIENTED_EDGE ( 'NONE', *, *, #55288, .T. ) ;
#10887 = CARTESIAN_POINT ( 'NONE',  ( -4.716976649647097730, 123.2429263765338163, -6.492361379858953896 ) ) ;
#10888 = DIRECTION ( 'NONE',  ( 0.000000000000000000, 1.000000000000000000, 0.000000000000000000 ) ) ;
#10889 = CARTESIAN_POINT ( 'NONE',  ( -1.224646799147353207E-16, 1.000000000000000000, 3.000000000000000000 ) ) ;
#10890 = CARTESIAN_POINT ( 'NONE',  ( 3.108481029118200567, -9.000000000000003553, 0.5125184569636065390 ) ) ;
#10891 = ADVANCED_FACE ( 'NONE', ( #38543 ), #38193, .T. ) ;
#10892 = SURFACE_STYLE_FILL_AREA ( #15846 ) ;
#10893 = EDGE_LOOP ( 'NONE', ( #61757, #37618, #2702 ) ) ;
#10894 = CARTESIAN_POINT ( 'NONE',  ( 4.683753779217433078, -5.887500484252664812, 0.4948905776603311213 ) ) ;
#10895 = ORIENTED_EDGE ( 'NONE', *, *, #20439, .F. ) ;
#10896 =( NAMED_UNIT ( * ) PLANE_ANGLE_UNIT ( ) SI_UNIT ( $, .RADIAN. ) );
#10897 =( NAMED_UNIT ( * ) PLANE_ANGLE_UNIT ( ) SI_UNIT ( $, .RADIAN. ) );
#10898 = SURFACE_STYLE_FILL_AREA ( #38013 ) ;
#10899 = CARTESIAN_POINT ( 'NONE',  ( -140.6050000000000182, 6.826472737025113702, -4.959722759717902107 ) ) ;
#10900 = ADVANCED_FACE ( 'NONE', ( #49084 ), #7518, .F. ) ;
#10901 = DIRECTION ( 'NONE',  ( 1.000000000000000000, 0.000000000000000000, -0.000000000000000000 ) ) ;
#10902 = UNCERTAINTY_MEASURE_WITH_UNIT (LENGTH_MEASURE( 1.000000000000000082E-05 ), #66272, 'distance_accuracy_value', 'NONE');
#10903 = ADVANCED_FACE ( 'NONE', ( #24044 ), #12586, .T. ) ;
#10904 = CARTESIAN_POINT ( 'NONE',  ( -65.00000000000000000, -1.962809905030629631E-14, 11.50000000000003020 ) ) ;
#10905 = SURFACE_STYLE_FILL_AREA ( #53797 ) ;
#10906 = ORIENTED_EDGE ( 'NONE', *, *, #42864, .T. ) ;
#10907 = EDGE_LOOP ( 'NONE', ( #46102, #24266, #4649 ) ) ;
#10908 = LINE ( 'NONE', #33729, #10364 ) ;
#10909 = AXIS2_PLACEMENT_3D ( 'NONE', #52118, #8151, #46515 ) ;
#10910 = ADVANCED_FACE ( 'NONE', ( #39444 ), #53844, .F. ) ;
#10911 = FACE_OUTER_BOUND ( 'NONE', #58437, .T. ) ;
#10912 = CARTESIAN_POINT ( 'NONE',  ( -56.60499999999998266, 6.826472737025113702, -4.959722759717902107 ) ) ;
#10913 = EDGE_LOOP ( 'NONE', ( #68514, #53354, #47068, #36354 ) ) ;
#10914 = SURFACE_STYLE_USAGE ( .BOTH. , #46878 ) ;
#10915 = CARTESIAN_POINT ( 'NONE',  ( 0.000000000000000000, 0.000000000000000000, 0.7500000000000000000 ) ) ;
#10916 = PRESENTATION_LAYER_ASSIGNMENT (  '', '', ( #34452 ) ) ;
#10917 = DIRECTION ( 'NONE',  ( 1.000000000000000000, 0.000000000000000000, -0.000000000000000000 ) ) ;
#10918 = CARTESIAN_POINT ( 'NONE',  ( -60.00000000000000000, -2.024042244987997205E-14, 6.000000000000000888 ) ) ;
#10919 = CARTESIAN_POINT ( 'NONE',  ( 1.000000000000000000, 1.000000000000000222, -3.000000000000000000 ) ) ;
#10920 = ORIENTED_EDGE ( 'NONE', *, *, #9785, .T. ) ;
#10921 = SPHERICAL_SURFACE ( 'NONE', #23415, 0.5000000000000000000 ) ;
#10922 = DIRECTION ( 'NONE',  ( 0.000000000000000000, 1.000000000000000000, 0.000000000000000000 ) ) ;
#10923 = PLANE ( 'NONE',  #8950 ) ;
#10924 = MECHANICAL_DESIGN_GEOMETRIC_PRESENTATION_REPRESENTATION (  '', ( #52485 ), #28877 ) ;
#10925 = CARTESIAN_POINT ( 'NONE',  ( -104.9949999999999761, -6.826472737025113702, 4.959722759717902107 ) ) ;
#10926 = CARTESIAN_POINT ( 'NONE',  ( -1.166476076187854022E-15, 155.9449999999999932, 9.525000000000000355 ) ) ;
#10927 = CARTESIAN_POINT ( 'NONE',  ( -84.74499999999999034, 4.716976649647094177, 6.492361379858945902 ) ) ;
#10928 = CARTESIAN_POINT ( 'NONE',  ( -4.716976649647097730, 112.3570736234661496, -6.492361379858953896 ) ) ;
#10929 = LINE ( 'NONE', #53826, #24659 ) ;
#10930 = DIRECTION ( 'NONE',  ( 0.000000000000000000, 0.000000000000000000, 1.000000000000000000 ) ) ;
#10931 = UNCERTAINTY_MEASURE_WITH_UNIT (LENGTH_MEASURE( 1.000000000000000082E-05 ), #6528, 'distance_accuracy_value', 'NONE');
#10932 = CARTESIAN_POINT ( 'NONE',  ( -153.0570736234661808, 0.000000000000000000, 9.524999999999991473 ) ) ;
#10933 = ORIENTED_EDGE ( 'NONE', *, *, #21200, .F. ) ;
#10934 = CARTESIAN_POINT ( 'NONE',  ( -133.7929263765338135, -3.094860106618429807, 9.524999999999991473 ) ) ;
#10935 = CARTESIAN_POINT ( 'NONE',  ( -151.4949999999999761, 6.826472737025113702, -4.959722759717902107 ) ) ;
#10936 = CARTESIAN_POINT ( 'NONE',  ( -71.50000000000000000, 36.32520566882265456, -7.500000000000000000 ) ) ;
#10937 = CARTESIAN_POINT ( 'NONE',  ( -66.80707362346618083, 10.01517768586948698, -1.839758294383808966E-15 ) ) ;
#10938 = DIRECTION ( 'NONE',  ( -0.5000000000000001110, -0.8660254037844384856, 0.000000000000000000 ) ) ;
#10939 = VERTEX_POINT ( 'NONE', #993 ) ;
#10940 = ORIENTED_EDGE ( 'NONE', *, *, #2822, .F. ) ;
#10941 = FACE_OUTER_BOUND ( 'NONE', #22499, .T. ) ;
#10942 = CARTESIAN_POINT ( 'NONE',  ( -133.1070736234661922, 8.102448949553172852, -5.886773742842744461 ) ) ;
#10943 = CARTESIAN_POINT ( 'NONE',  ( -45.00000000000000000, 8.092291901770513718, 5.807866024088225387 ) ) ;
#10944 = PRESENTATION_STYLE_ASSIGNMENT (( #31343 ) ) ;
#10945 = STYLED_ITEM ( 'NONE', ( #55545 ), #65596 ) ;
#10946 = CARTESIAN_POINT ( 'NONE',  ( -150.8929263765337794, -8.102448949553174629, -5.886773742842741797 ) ) ;
#10947 = ORIENTED_EDGE ( 'NONE', *, *, #34966, .T. ) ;
#10948 = CARTESIAN_POINT ( 'NONE',  ( -151.8549999999999898, 4.716976649647094177, 6.492361379858945902 ) ) ;
#10949 = CIRCLE ( 'NONE', #50285, 17.00000000000000000 ) ;
#10950 = ORIENTED_EDGE ( 'NONE', *, *, #62566, .T. ) ;
#10951 = CARTESIAN_POINT ( 'NONE',  ( 31.00000000000000711, 42.00000000000000000, -36.50000000000000000 ) ) ;
#10952 = VERTEX_POINT ( 'NONE', #22901 ) ;
#10953 = EDGE_CURVE ( 'NONE', #26431, #8149, #7809, .T. ) ;
#10954 = CARTESIAN_POINT ( 'NONE',  ( -45.00000000000000000, -2.024042244987997205E-14, 10.00000000000000000 ) ) ;
#10955 = CARTESIAN_POINT ( 'NONE',  ( 21.02379604162863913, 114.4999999999999574, -10.50000000000000000 ) ) ;
#10956 = CARTESIAN_POINT ( 'NONE',  ( 3.094860106618431583, 123.0949999999999704, 9.525000000000000355 ) ) ;
#10957 = FILL_AREA_STYLE ('',( #31356 ) ) ;
#10958 = ADVANCED_FACE ( 'NONE', ( #12304 ), #52789, .F. ) ;
#10959 = EDGE_LOOP ( 'NONE', ( #50162, #9684, #35282, #35946 ) ) ;
#10960 = ADVANCED_FACE ( 'NONE', ( #27441 ), #21855, .T. ) ;
#10961 = LINE ( 'NONE', #38780, #49876 ) ;
#10962 = CARTESIAN_POINT ( 'NONE',  ( -10.01517768586949408, 129.3050000000000068, -6.132527647946036459E-16 ) ) ;
#10963 = CARTESIAN_POINT ( 'NONE',  ( -64.55499999999999261, 0.000000000000000000, 8.024999999999991473 ) ) ;
#10964 = CARTESIAN_POINT ( 'NONE',  ( -120.4449999999999932, 0.000000000000000000, 8.024999999999991473 ) ) ;
#10965 = CARTESIAN_POINT ( 'NONE',  ( -71.62068965517239860, 36.41396814395972115, 9.500000000000000000 ) ) ;
#10966 = VERTEX_POINT ( 'NONE', #16936 ) ;
#10967 = CARTESIAN_POINT ( 'NONE',  ( -10.01517768586949231, 144.3049999999999784, -6.132527647946036459E-16 ) ) ;
#10968 =( NAMED_UNIT ( * ) SI_UNIT ( $, .STERADIAN. ) SOLID_ANGLE_UNIT ( ) );
#10969 = UNCERTAINTY_MEASURE_WITH_UNIT (LENGTH_MEASURE( 1.000000000000000082E-05 ), #60412, 'distance_accuracy_value', 'NONE');
#10970 = ADVANCED_FACE ( 'NONE', ( #32376 ), #30283, .F. ) ;
#10971 = DIRECTION ( 'NONE',  ( 5.782411586589351722E-16, -1.000000000000000000, 0.000000000000000000 ) ) ;
#10972 = CIRCLE ( 'NONE', #19940, 1.000000000000000888 ) ;
#10973 = DIRECTION ( 'NONE',  ( 1.000000000000000000, 0.000000000000000000, 0.000000000000000000 ) ) ;
#10974 = ADVANCED_FACE ( 'NONE', ( #11635 ), #1008, .T. ) ;
#10975 = DIRECTION ( 'NONE',  ( 1.000000000000000000, 0.000000000000000000, 0.000000000000000000 ) ) ;
#10976 = EDGE_CURVE ( 'NONE', #10695, #67841, #17970, .T. ) ;
#10977 = CARTESIAN_POINT ( 'NONE',  ( -34.99999999999999289, 99.99999999999998579, 9.500000000000000000 ) ) ;
#10978 = ORIENTED_EDGE ( 'NONE', *, *, #42803, .F. ) ;
#10979 =( LENGTH_UNIT ( ) NAMED_UNIT ( * ) SI_UNIT ( .MILLI., .METRE. ) );
#10980 = CARTESIAN_POINT ( 'NONE',  ( -174.0549999999999784, -9.827790563157499189E-16, -8.024999999999991473 ) ) ;
#10982 = EDGE_LOOP ( 'NONE', ( #48835, #37610, #52512, #14906 ) ) ;
#10981 = EDGE_CURVE ( 'NONE', #67106, #3926, #14605, .T. ) ;
#10983 = DIRECTION ( 'NONE',  ( 0.000000000000000000, 0.000000000000000000, -1.000000000000000000 ) ) ;
#10984 = UNCERTAINTY_MEASURE_WITH_UNIT (LENGTH_MEASURE( 1.000000000000000082E-05 ), #41811, 'distance_accuracy_value', 'NONE');
#10985 = EDGE_CURVE ( 'NONE', #51461, #44668, #11284, .T. ) ;
#10986 = SURFACE_SIDE_STYLE ('',( #47281 ) ) ;
#10987 = DIRECTION ( 'NONE',  ( 0.000000000000000000, -1.000000000000000000, 0.000000000000000000 ) ) ;
#10988 = CARTESIAN_POINT ( 'NONE',  ( -65.99999999999998579, 50.00000000000000000, 12.00000000000000000 ) ) ;
#10989 = ORIENTED_EDGE ( 'NONE', *, *, #30740, .T. ) ;
#10990 = CARTESIAN_POINT ( 'NONE',  ( -128.3070736234661524, -10.01517768586948698, 6.132527647946031529E-16 ) ) ;
#10991 = DIRECTION ( 'NONE',  ( 0.000000000000000000, 0.000000000000000000, -1.000000000000000000 ) ) ;
#10992 = CARTESIAN_POINT ( 'NONE',  ( -87.35499999999998977, -4.716976649647093289, -6.492361379858945902 ) ) ;
#10993 = EDGE_LOOP ( 'NONE', ( #22972, #60205, #5155, #48683 ) ) ;
#10994 = CARTESIAN_POINT ( 'NONE',  ( -62.30707362346616662, -10.01517768586948698, 6.132527647946031529E-16 ) ) ;
#10995 = MECHANICAL_DESIGN_GEOMETRIC_PRESENTATION_REPRESENTATION (  '', ( #1932 ), #61501 ) ;
#10996 = VERTEX_POINT ( 'NONE', #1367 ) ;
#10997 = DIRECTION ( 'NONE',  ( -0.000000000000000000, 0.000000000000000000, -1.000000000000000000 ) ) ;
#10998 = FACE_OUTER_BOUND ( 'NONE', #27896, .T. ) ;
#10999 =( GEOMETRIC_REPRESENTATION_CONTEXT ( 3 ) GLOBAL_UNCERTAINTY_ASSIGNED_CONTEXT ( ( #46892 ) ) GLOBAL_UNIT_ASSIGNED_CONTEXT ( ( #57520, #36461, #15665 ) ) REPRESENTATION_CONTEXT ( 'NONE', 'WORKASPACE' ) );
#11001 = FILL_AREA_STYLE ('',( #26133 ) ) ;
#11000 = FACE_OUTER_BOUND ( 'NONE', #38211, .T. ) ;
#11002 = CARTESIAN_POINT ( 'NONE',  ( -109.8549999999999898, 4.716976649647094177, 6.492361379858945902 ) ) ;
#11003 = CARTESIAN_POINT ( 'NONE',  ( 5.598654528085809545, 130.1449999999999818, -7.705886871421373741 ) ) ;
#11004 = CARTESIAN_POINT ( 'NONE',  ( -116.9949999999999761, -6.826472737025115478, 4.959722759717900331 ) ) ;
#11005 = CARTESIAN_POINT ( 'NONE',  ( -25.00000000000000000, 1.000000000000000888, 4.000000000000000000 ) ) ;
#11006 = EDGE_CURVE ( 'NONE', #10674, #26634, #6003, .T. ) ;
#11007 = SURFACE_STYLE_USAGE ( .BOTH. , #30814 ) ;
#11008 = CARTESIAN_POINT ( 'NONE',  ( -165.5929263765337964, -3.094860106618431139, -9.524999999999991473 ) ) ;
#11009 = CARTESIAN_POINT ( 'NONE',  ( -178.4949999999999477, 6.826472737025113702, -4.959722759717902107 ) ) ;
#11010 = AXIS2_PLACEMENT_3D ( 'NONE', #57164, #8999, #30414 ) ;
#11011 = LINE ( 'NONE', #16337, #36650 ) ;
#11012 = DIRECTION ( 'NONE',  ( -0.000000000000000000, -0.000000000000000000, -1.000000000000000000 ) ) ;
#11013 = DIRECTION ( 'NONE',  ( -0.000000000000000000, 1.000000000000000000, -0.000000000000000000 ) ) ;
#11014 = VERTEX_POINT ( 'NONE', #48972 ) ;
#11015 = CARTESIAN_POINT ( 'NONE',  ( -76.19292637653380496, -10.01517768586948698, 6.132527647946031529E-16 ) ) ;
#11016 = ITEM_DEFINED_TRANSFORMATION ( 'NONE', 'NONE', #48410,  #42840 ) ;
#11017 = CARTESIAN_POINT ( 'NONE',  ( 30.25000000000002842, 3.498359009886561184E-14, 3.750000000000000000 ) ) ;
#11018 = FACE_OUTER_BOUND ( 'NONE', #3769, .T. ) ;
#11019 = CARTESIAN_POINT ( 'NONE',  ( -45.99999999999999289, 1.166476076187854022E-15, -9.525000000000000355 ) ) ;
#11020 = PRESENTATION_STYLE_ASSIGNMENT (( #15640 ) ) ;
#11021 = CARTESIAN_POINT ( 'NONE',  ( -13.23915246117191025, 52.65078610323165265, -12.50000000000000000 ) ) ;
#11022 = CARTESIAN_POINT ( 'NONE',  ( -179.7549999999999955, 4.716976649647091513, -6.492361379858946790 ) ) ;
#11023 = EDGE_CURVE ( 'NONE', #25558, #29227, #666, .T. ) ;
#11024 = ORIENTED_EDGE ( 'NONE', *, *, #2394, .T. ) ;
#11025 = DIRECTION ( 'NONE',  ( -0.000000000000000000, -0.000000000000000000, -1.000000000000000000 ) ) ;
#11026 = MECHANICAL_DESIGN_GEOMETRIC_PRESENTATION_REPRESENTATION (  '', ( #24514 ), #63852 ) ;
#11027 = CARTESIAN_POINT ( 'NONE',  ( 28.00000000000002842, 0.000000000000000000, 89.00000000000000000 ) ) ;
#11028 = CARTESIAN_POINT ( 'NONE',  ( -9.827790563157511022E-16, 143.5570736234661524, 8.025000000000000355 ) ) ;
#11029 = EDGE_CURVE ( 'NONE', #10461, #50919, #22192, .T. ) ;
#11030 = ORIENTED_EDGE ( 'NONE', *, *, #45504, .T. ) ;
#11031 = CARTESIAN_POINT ( 'NONE',  ( 2.607480562269155921, 136.5929263765337964, 8.024999999999941735 ) ) ;
#11032 = CARTESIAN_POINT ( 'NONE',  ( -92.75499999999999545, 4.716976649647091513, -6.492361379858946790 ) ) ;
#11033 = UNCERTAINTY_MEASURE_WITH_UNIT (LENGTH_MEASURE( 1.000000000000000082E-05 ), #49299, 'distance_accuracy_value', 'NONE');
#11034 = LINE ( 'NONE', #21963, #51094 ) ;
#11035 = CIRCLE ( 'NONE', #35761, 0.5000000000000004441 ) ;
#11036 = ORIENTED_EDGE ( 'NONE', *, *, #56069, .T. ) ;
#11037 = VECTOR ( 'NONE', #47379, 1000.000000000000000 ) ;
#11038 = SURFACE_STYLE_USAGE ( .BOTH. , #33206 ) ;
#11039 = CARTESIAN_POINT ( 'NONE',  ( -127.9429263765338192, 0.000000000000000000, 9.524999999999991473 ) ) ;
#11040 = SURFACE_SIDE_STYLE ('',( #26842 ) ) ;
#11041 = CARTESIAN_POINT ( 'NONE',  ( 68.99999999999998579, 0.000000000000000000, 4.000000000000000000 ) ) ;
#11042 = EDGE_CURVE ( 'NONE', #23699, #6580, #6349, .T. ) ;
#11043 = ORIENTED_EDGE ( 'NONE', *, *, #59959, .T. ) ;
#11044 = VECTOR ( 'NONE', #63789, 1000.000000000000000 ) ;
#11045 = CARTESIAN_POINT ( 'NONE',  ( -62.54499999999998749, -7.632228543268600340, -2.479861379858950166 ) ) ;
#11046 = ORIENTED_EDGE ( 'NONE', *, *, #18068, .F. ) ;
#11047 = SURFACE_STYLE_USAGE ( .BOTH. , #21610 ) ;
#11048 = MECHANICAL_DESIGN_GEOMETRIC_PRESENTATION_REPRESENTATION (  '', ( #18921 ), #36959 ) ;
#11049 = FILL_AREA_STYLE ('',( #58557 ) ) ;
#11050 = EDGE_CURVE ( 'NONE', #47241, #19502, #22540, .T. ) ;
#11051 = ORIENTED_EDGE ( 'NONE', *, *, #17200, .T. ) ;
#11052 = DIRECTION ( 'NONE',  ( 2.312964634635740689E-15, -1.000000000000000000, 0.000000000000000000 ) ) ;
#11053 = ORIENTED_EDGE ( 'NONE', *, *, #12286, .T. ) ;
#11054 = COLOUR_RGB ( '', 0.08235294, 0.09019608, 0.10196078) ;
#11055 = FILL_AREA_STYLE ('',( #47361 ) ) ;
#11056 = CARTESIAN_POINT ( 'NONE',  ( 22.00000000000000355, 42.47058823529412308, -74.11764705882353610 ) ) ;
#11057 = CARTESIAN_POINT ( 'NONE',  ( -121.8549999999999898, 4.716976649647094177, 6.492361379858945902 ) ) ;
#11058 = VERTEX_POINT ( 'NONE', #49629 ) ;
#11059 = ORIENTED_EDGE ( 'NONE', *, *, #53376, .T. ) ;
#11060 = CARTESIAN_POINT ( 'NONE',  ( -159.7429263765338021, -5.598654528085803328, -7.705886871421366635 ) ) ;
#11061 = CARTESIAN_POINT ( 'NONE',  ( 45.50000000000000000, 99.99999999999992895, -9.500000000000000000 ) ) ;
#11062 = CARTESIAN_POINT ( 'NONE',  ( -163.8570736234661922, -5.598654528085803328, -7.705886871421366635 ) ) ;
#11063 = CARTESIAN_POINT ( 'NONE',  ( -5.598654528085808657, 128.6449999999999818, 7.705886871421373741 ) ) ;
#11064 = CARTESIAN_POINT ( 'NONE',  ( -98.00707362346618368, -8.102448949553172852, -5.886773742842741797 ) ) ;
#11065 = CIRCLE ( 'NONE', #34658, 8.500000000000000000 ) ;
#11066 = LINE ( 'NONE', #43498, #26810 ) ;
#11067 = ORIENTED_EDGE ( 'NONE', *, *, #68710, .T. ) ;
#11068 =( LENGTH_UNIT ( ) NAMED_UNIT ( * ) SI_UNIT ( .MILLI., .METRE. ) );
#11069 = CARTESIAN_POINT ( 'NONE',  ( 40.99999999999998579, 107.7459666924148252, 3.000000000000000000 ) ) ;
#11070 = CIRCLE ( 'NONE', #40320, 0.2500000000000002220 ) ;
#11071 = CARTESIAN_POINT ( 'NONE',  ( -140.9050000000000011, 2.607480562269068880, -8.024999999999993250 ) ) ;
#11072 = CARTESIAN_POINT ( 'NONE',  ( -7.731910350068054619E-16, -6.500000000000000888, 3.000000000000000000 ) ) ;
#11073 = PRESENTATION_STYLE_ASSIGNMENT (( #62470 ) ) ;
#11075 = FILL_AREA_STYLE_COLOUR ( '', #35423 ) ;
#11074 = ADVANCED_BREP_SHAPE_REPRESENTATION ( '', ( #50379, #42840 ), #47260 ) ;
#11076 = CARTESIAN_POINT ( 'NONE',  ( -142.9449999999999932, -9.827790563157499189E-16, -8.024999999999991473 ) ) ;
#11077 = CIRCLE ( 'NONE', #62789, 2.499999999999998668 ) ;
#11078 = CARTESIAN_POINT ( 'NONE',  ( -139.0450000000000159, 7.632228543268600340, 2.479861379858949277 ) ) ;
#11079 = ORIENTED_EDGE ( 'NONE', *, *, #5978, .F. ) ;
#11080 =( GEOMETRIC_REPRESENTATION_CONTEXT ( 3 ) GLOBAL_UNCERTAINTY_ASSIGNED_CONTEXT ( ( #33478 ) ) GLOBAL_UNIT_ASSIGNED_CONTEXT ( ( #68518, #53038, #31199 ) ) REPRESENTATION_CONTEXT ( 'NONE', 'WORKASPACE' ) );
#11081 = EDGE_CURVE ( 'NONE', #23924, #58314, #65800, .T. ) ;
#11082 = CARTESIAN_POINT ( 'NONE',  ( 26.25000000000001066, 19.24999999999997868, 4.000000000000000000 ) ) ;
#11083 = DIRECTION ( 'NONE',  ( -1.000000000000000000, 0.000000000000000000, 0.000000000000000000 ) ) ;
#11084 = CARTESIAN_POINT ( 'NONE',  ( -57.50499999999997414, -6.826472737025115478, -4.959722759717899443 ) ) ;
#11085 = SURFACE_STYLE_FILL_AREA ( #32916 ) ;
#11086 = EDGE_CURVE ( 'NONE', #17986, #42973, #55051, .T. ) ;
#11087 = CARTESIAN_POINT ( 'NONE',  ( -55.19499999999998607, 8.437984349512085203, -1.550032578732815448E-15 ) ) ;
#11088 =( GEOMETRIC_REPRESENTATION_CONTEXT ( 3 ) GLOBAL_UNCERTAINTY_ASSIGNED_CONTEXT ( ( #12124 ) ) GLOBAL_UNIT_ASSIGNED_CONTEXT ( ( #30999, #61685, #18470 ) ) REPRESENTATION_CONTEXT ( 'NONE', 'WORKASPACE' ) );
#11089 = MECHANICAL_DESIGN_GEOMETRIC_PRESENTATION_REPRESENTATION (  '', ( #58161 ), #50320 ) ;
#11090 = CARTESIAN_POINT ( 'NONE',  ( -124.9429263765338192, 0.000000000000000000, 9.524999999999991473 ) ) ;
#11091 = LINE ( 'NONE', #68467, #61636 ) ;
#11092 = STYLED_ITEM ( 'NONE', ( #16051 ), #14785 ) ;
#11093 =( NAMED_UNIT ( * ) SI_UNIT ( $, .STERADIAN. ) SOLID_ANGLE_UNIT ( ) );
#11094 = CARTESIAN_POINT ( 'NONE',  ( -109.0429263765337993, -9.058813317711329915, -2.943386871421370898 ) ) ;
#11095 = DIRECTION ( 'NONE',  ( 1.665334536937734811E-16, -0.2829836251474255882, 0.9591247405308765961 ) ) ;
#11096 = DIRECTION ( 'NONE',  ( 0.000000000000000000, 0.000000000000000000, -1.000000000000000000 ) ) ;
#11097 = DIRECTION ( 'NONE',  ( 1.000000000000000000, 0.000000000000000000, 0.000000000000000000 ) ) ;
#11098 = EDGE_CURVE ( 'NONE', #62495, #58540, #39386, .T. ) ;
#11099 = CARTESIAN_POINT ( 'NONE',  ( 1.709458476932651091E-14, -60.04052944165106709, -35.50000000000000000 ) ) ;
#11100 = EDGE_CURVE ( 'NONE', #47666, #6055, #20212, .T. ) ;
#11101 = ORIENTED_EDGE ( 'NONE', *, *, #55186, .T. ) ;
#11102 = CARTESIAN_POINT ( 'NONE',  ( -4.716976649647097730, 138.2429263765338305, -6.492361379858953896 ) ) ;
#11103 = ORIENTED_EDGE ( 'NONE', *, *, #35177, .F. ) ;
#11104 = PRESENTATION_STYLE_ASSIGNMENT (( #55053 ) ) ;
#11105 = B_SPLINE_CURVE_WITH_KNOTS ( 'NONE', 3,
 ( #61859, #13686, #7708, #18279, #51327, #35145, #60816, #45050, #7382, #23214, #17928, #39417, #12637, #29148, #50634, #2372, #14744, #35503, #57644, #42219, #4861, #46077, #25281, #63609, #19657, #36588, #62553, #41153, #36917, #67495, #36220, #14371 ),
 .UNSPECIFIED., .F., .F.,
 ( 4, 2, 2, 2, 2, 2, 2, 2, 2, 2, 2, 2, 2, 2, 2, 4 ),
 ( 0.001113530544794672211, 0.002431556489591745265, 0.003749582434388818754, 0.005067608379185892242, 0.006385634323982964863, 0.007703660268780037484, 0.009021686213577111840, 0.01165773810317125535, 0.01297576404796832797, 0.01429378999276540059, 0.01561181593756247668, 0.01692984188235954757, 0.01824786782715661845, 0.01956589377195369281, 0.02088391971675076370, 0.02220194566154783458 ),
 .UNSPECIFIED. ) ;
#11106 = CARTESIAN_POINT ( 'NONE',  ( -6.826472737025120807, 115.5070736234661553, -4.959722759717907437 ) ) ;
#11107 = ADVANCED_FACE ( 'NONE', ( #36660 ), #26716, .T. ) ;
#11108 = VECTOR ( 'NONE', #2192, 1000.000000000000000 ) ;
#11109 = DIRECTION ( 'NONE',  ( -1.000000000000000000, -0.000000000000000000, -0.000000000000000000 ) ) ;
#11110 = CARTESIAN_POINT ( 'NONE',  ( -9.827790563157511022E-16, 137.5570736234661808, 8.025000000000000355 ) ) ;
#11111 = DIRECTION ( 'NONE',  ( 0.000000000000000000, 0.3420201433256693790, 0.9396926207859082059 ) ) ;
#11112 = EDGE_CURVE ( 'NONE', #69269, #37989, #14661, .T. ) ;
#11113 = VERTEX_POINT ( 'NONE', #52807 ) ;
#11115 = VERTEX_POINT ( 'NONE', #26390 ) ;
#11114 = AXIS2_PLACEMENT_3D ( 'NONE', #66711, #18527, #13572 ) ;
#11116 = CYLINDRICAL_SURFACE ( 'NONE', #42259, 9.524999999999991473 ) ;
#11117 = CYLINDRICAL_SURFACE ( 'NONE', #27510, 9.524999999999991473 ) ;
#11118 = ORIENTED_EDGE ( 'NONE', *, *, #22651, .F. ) ;
#11119 = CARTESIAN_POINT ( 'NONE',  ( -3.094860106618432471, 128.7049999999999841, -9.525000000000000355 ) ) ;
#11120 = CARTESIAN_POINT ( 'NONE',  ( 43.75000000000000000, 19.24999999999998224, 4.000000000000000000 ) ) ;
#11121 = LINE ( 'NONE', #5476, #58705 ) ;
#11122 = EDGE_CURVE ( 'NONE', #64166, #68610, #59094, .T. ) ;
#11123 = VECTOR ( 'NONE', #57524, 1000.000000000000000 ) ;
#11124 = DIRECTION ( 'NONE',  ( 0.000000000000000000, 0.000000000000000000, -1.000000000000000000 ) ) ;
#11125 = CARTESIAN_POINT ( 'NONE',  ( -89.84499999999999886, -7.632228543268599452, 2.479861379858951054 ) ) ;
#11126 = ORIENTED_EDGE ( 'NONE', *, *, #20724, .F. ) ;
#11127 = VECTOR ( 'NONE', #18160, 1000.000000000000000 ) ;
#11128 = DIRECTION ( 'NONE',  ( -1.000000000000000000, 0.000000000000000000, 0.000000000000000000 ) ) ;
#11129 = EDGE_CURVE ( 'NONE', #20689, #43029, #16226, .T. ) ;
#11130 = EDGE_LOOP ( 'NONE', ( #63148, #40572, #44306, #21979 ) ) ;
#11131 = CARTESIAN_POINT ( 'NONE',  ( -175.6429263765338078, -5.598654528085801552, 7.705886871421367523 ) ) ;
#11132 =( BOUNDED_CURVE ( )  B_SPLINE_CURVE ( 2, ( #62619, #14436, #46149, #67937, #67572, #40873, #9547, #41922, #57011, #3496, #8826 ),
 .UNSPECIFIED., .F., .T. ) 
 B_SPLINE_CURVE_WITH_KNOTS ( ( 3, 2, 2, 2, 2, 3 ),
 ( 0.8235294117647057321, 0.8294117647058822929, 0.8352941176470587425, 0.8411764705882351922, 0.8470588235294116419, 0.8529411764705880916 ),
 .UNSPECIFIED. ) 
 CURVE ( )  GEOMETRIC_REPRESENTATION_ITEM ( )  RATIONAL_B_SPLINE_CURVE ( ( 1.000000000000000888, 0.9510565162951526430, 1.000000000000000000, 0.9510565162951535312, 1.000000000000000000, 0.9510565162951535312, 1.000000000000000000, 0.9510565162951535312, 1.000000000000000000, 0.9510565162951544194, 0.9999999999999991118 ) ) 
 REPRESENTATION_ITEM ( '' )  );
#11133 = CARTESIAN_POINT ( 'NONE',  ( 45.50000000000000000, -1.469576158976824618E-14, 6.500000000000000000 ) ) ;
#11134 = COLOUR_RGB ( '', 0.72549020, 0.75294118, 0.79215686) ;
#11135 = CARTESIAN_POINT ( 'NONE',  ( 8.082903768654762899, -1.269775441351268174E-15, 1.082903768654759125 ) ) ;
#11136 = VERTEX_POINT ( 'NONE', #48235 ) ;
#11137 = CARTESIAN_POINT ( 'NONE',  ( -60.00000000000000000, -2.024042244987997205E-14, 10.50000000000000000 ) ) ;
#11138 = VERTEX_POINT ( 'NONE', #42296 ) ;
#11139 = DIRECTION ( 'NONE',  ( 1.000000000000000000, 0.000000000000000000, -1.300977106640434891E-16 ) ) ;
#11140 = DIRECTION ( 'NONE',  ( 0.000000000000000000, -1.000000000000000000, -0.000000000000000000 ) ) ;
#11141 = DIRECTION ( 'NONE',  ( -0.000000000000000000, -1.000000000000000000, 0.000000000000000000 ) ) ;
#11143 = COLOUR_RGB ( '', 0.66274510, 0.83137255, 0.94901961) ;
#11142 = SURFACE_STYLE_FILL_AREA ( #64952 ) ;
#11144 = SURFACE_STYLE_FILL_AREA ( #5860 ) ;
#11145 = AXIS2_PLACEMENT_3D ( 'NONE', #17606, #12276, #5030 ) ;
#11146 = DIRECTION ( 'NONE',  ( -0.8660254037844384856, 0.5000000000000003331, 0.000000000000000000 ) ) ;
#11147 = CARTESIAN_POINT ( 'NONE',  ( -69.44292637653380496, -1.166476076187852838E-15, -9.524999999999991473 ) ) ;
#11148 = CARTESIAN_POINT ( 'NONE',  ( 30.99999999999998579, 5.000000000000000000, 72.00402776293822171 ) ) ;
#11149 = CARTESIAN_POINT ( 'NONE',  ( -3.607123150363804154, 153.1289957264864938, -7.332553890433554322 ) ) ;
#11150 = ORIENTED_EDGE ( 'NONE', *, *, #1842, .T. ) ;
#11151 = MECHANICAL_DESIGN_GEOMETRIC_PRESENTATION_REPRESENTATION (  '', ( #56096 ), #62814 ) ;
#11152 = ORIENTED_EDGE ( 'NONE', *, *, #13182, .T. ) ;
#11153 = CARTESIAN_POINT ( 'NONE',  ( -48.65707362346616094, 9.058813317711329915, 2.943386871421369566 ) ) ;
#11154 = LINE ( 'NONE', #53400, #9639 ) ;
#11155 =( NAMED_UNIT ( * ) PLANE_ANGLE_UNIT ( ) SI_UNIT ( $, .RADIAN. ) );
#11156 = DIRECTION ( 'NONE',  ( -0.7833176619561877940, -0.6216216216216191581, 4.313366480807175060E-15 ) ) ;
#11157 = ORIENTED_EDGE ( 'NONE', *, *, #33102, .T. ) ;
#11158 = CARTESIAN_POINT ( 'NONE',  ( -164.6049999999999898, 6.826472737025113702, -4.959722759717902107 ) ) ;
#11159 = DIRECTION ( 'NONE',  ( -0.000000000000000000, -1.000000000000000000, -0.000000000000000000 ) ) ;
#11160 = DIRECTION ( 'NONE',  ( 0.000000000000000000, 0.000000000000000000, 1.000000000000000000 ) ) ;
#11161 = CARTESIAN_POINT ( 'NONE',  ( -173.3950000000000102, -6.826472737025115478, -4.959722759717899443 ) ) ;
#11162 = CARTESIAN_POINT ( 'NONE',  ( -165.8949999999999818, 6.826472737025115478, 4.959722759717899443 ) ) ;
#11163 =( GEOMETRIC_REPRESENTATION_CONTEXT ( 3 ) GLOBAL_UNCERTAINTY_ASSIGNED_CONTEXT ( ( #47445 ) ) GLOBAL_UNIT_ASSIGNED_CONTEXT ( ( #46314, #8995, #61394 ) ) REPRESENTATION_CONTEXT ( 'NONE', 'WORKASPACE' ) );
#11164 = AXIS2_PLACEMENT_3D ( 'NONE', #41728, #20226, #37513 ) ;
#11165 =( BOUNDED_CURVE ( )  B_SPLINE_CURVE ( 2, ( #66885, #45466, #29213, #34850, #17989, #35208, #61244, #23607, #39477, #34172, #60882 ),
 .UNSPECIFIED., .F., .F. ) 
 B_SPLINE_CURVE_WITH_KNOTS ( ( 3, 2, 2, 2, 2, 3 ),
 ( 0.4347826086956419478, 0.4369565217391201406, 0.4391304347825983889, 0.4413043478260766372, 0.4434782608695548300, 0.4456521739130330229 ),
 .UNSPECIFIED. ) 
 CURVE ( )  GEOMETRIC_REPRESENTATION_ITEM ( )  RATIONAL_B_SPLINE_CURVE ( ( 1.000000000000230038, 0.9510565162949236040, 1.000000000000000000, 0.9510565162951535312, 1.000000000000000000, 0.9510565162951535312, 1.000000000000000000, 0.9510565162951535312, 1.000000000000000000, 0.9510565162953884544, 0.9999999999997650768 ) ) 
 REPRESENTATION_ITEM ( '' )  );
#11166 = EDGE_LOOP ( 'NONE', ( #44484, #55461, #5510, #22985, #33559, #41610 ) ) ;
#11167 = EDGE_CURVE ( 'NONE', #6975, #61023, #36305, .T. ) ;
#11168 = FACE_OUTER_BOUND ( 'NONE', #33698, .T. ) ;
#11170 = CARTESIAN_POINT ( 'NONE',  ( -71.50000000000000000, 35.92875272052971525, 9.500000000000000000 ) ) ;
#11169 = CIRCLE ( 'NONE', #67315, 0.5000000000000004441 ) ;
#11171 = CARTESIAN_POINT ( 'NONE',  ( 0.000000000000000000, 114.9999999999999574, 0.000000000000000000 ) ) ;
#11172 = CARTESIAN_POINT ( 'NONE',  ( -82.55499999999999261, 0.000000000000000000, 8.024999999999991473 ) ) ;
#11173 = CARTESIAN_POINT ( 'NONE',  ( -75.00000000000000000, 9.708372675170620525, 10.00000000000000000 ) ) ;
#11174 = VECTOR ( 'NONE', #32434, 1000.000000000000000 ) ;
#11175 = CARTESIAN_POINT ( 'NONE',  ( -76.19499999999997897, 8.437984349512086979, -1.550032578732815448E-15 ) ) ;
#11176 = CARTESIAN_POINT ( 'NONE',  ( -5.598654528085808657, 138.7549999999999955, 7.705886871421373741 ) ) ;
#11177 = CARTESIAN_POINT ( 'NONE',  ( -133.7070736234668118, -3.094860106628716245, -9.524999999992518340 ) ) ;
#11178 = TOROIDAL_SURFACE ( 'NONE', #16839, 0.5000000000000000000, 0.2500000000000000000 ) ;
#11179 = FACE_OUTER_BOUND ( 'NONE', #10619, .T. ) ;
#11180 = CIRCLE ( 'NONE', #50510, 0.2500000000000002220 ) ;
#11181 = STYLED_ITEM ( 'NONE', ( #44174 ), #4754 ) ;
#11182 = CARTESIAN_POINT ( 'NONE',  ( -75.29292637653379927, 3.094860106618428031, -9.524999999999993250 ) ) ;
#11183 = VECTOR ( 'NONE', #8623, 1000.000000000000000 ) ;
#11184 = DIRECTION ( 'NONE',  ( -0.000000000000000000, 0.000000000000000000, 1.000000000000000000 ) ) ;
#11185 = VERTEX_POINT ( 'NONE', #30974 ) ;
#11186 = ADVANCED_FACE ( 'NONE', ( #9894 ), #64378, .F. ) ;
#11187 = DIRECTION ( 'NONE',  ( 0.000000000000000000, 0.000000000000000000, 1.000000000000000000 ) ) ;
#11188 =( NAMED_UNIT ( * ) PLANE_ANGLE_UNIT ( ) SI_UNIT ( $, .RADIAN. ) );
#11189 = PRESENTATION_LAYER_ASSIGNMENT (  '', '', ( #41559 ) ) ;
#11190 = ADVANCED_FACE ( 'NONE', ( #62982 ), #67417, .T. ) ;
#11191 = ADVANCED_FACE ( 'NONE', ( #53487 ), #68628, .F. ) ;
#11192 = EDGE_CURVE ( 'NONE', #2160, #32455, #20266, .T. ) ;
#11194 = DIRECTION ( 'NONE',  ( 0.7071067811865543451, 0.000000000000000000, 0.7071067811865408004 ) ) ;
#11193 = CARTESIAN_POINT ( 'NONE',  ( -195.0000000000000000, 0.000000000000000000, 0.000000000000000000 ) ) ;
#11195 = DIRECTION ( 'NONE',  ( 0.000000000000000000, 0.000000000000000000, -1.000000000000000000 ) ) ;
#11196 = ORIENTED_EDGE ( 'NONE', *, *, #49273, .T. ) ;
#11197 = COLOUR_RGB ( '', 0.66274510, 0.83137255, 0.94901961) ;
#11198 = ORIENTED_EDGE ( 'NONE', *, *, #1464, .F. ) ;
#11199 = SURFACE_STYLE_USAGE ( .BOTH. , #45245 ) ;
#11200 = EDGE_CURVE ( 'NONE', #52429, #45842, #34091, .T. ) ;
#11201 = DIRECTION ( 'NONE',  ( 0.000000000000000000, 0.000000000000000000, 1.000000000000000000 ) ) ;
#11202 = SURFACE_STYLE_FILL_AREA ( #31252 ) ;
#11203 = CIRCLE ( 'NONE', #55030, 0.5000000000000004441 ) ;
#11204 = DIRECTION ( 'NONE',  ( 0.000000000000000000, 0.000000000000000000, -1.000000000000000000 ) ) ;
#11205 = ADVANCED_FACE ( 'NONE', ( #6313, #38030 ), #55182, .F. ) ;
#11206 = ORIENTED_EDGE ( 'NONE', *, *, #39836, .F. ) ;
#11207 = CARTESIAN_POINT ( 'NONE',  ( -109.5549999999999926, 0.000000000000000000, 8.024999999999991473 ) ) ;
#11208 = ORIENTED_EDGE ( 'NONE', *, *, #63233, .T. ) ;
#11209 =( NAMED_UNIT ( * ) SI_UNIT ( $, .STERADIAN. ) SOLID_ANGLE_UNIT ( ) );
#11210 = LINE ( 'NONE', #37659, #23129 ) ;
#11211 = EDGE_LOOP ( 'NONE', ( #8182, #41378 ) ) ;
#11212 = PLANE ( 'NONE',  #34713 ) ;
#11213 = ORIENTED_EDGE ( 'NONE', *, *, #36591, .T. ) ;
#11214 = COLOUR_RGB ( '', 0.66274510, 0.83137255, 0.94901961) ;
#11215 = CARTESIAN_POINT ( 'NONE',  ( -9.058813317711337021, 155.0449999999999875, -2.943386871421374895 ) ) ;
#11216 = VERTEX_POINT ( 'NONE', #66091 ) ;
#11217 = ORIENTED_EDGE ( 'NONE', *, *, #23412, .T. ) ;
#11218 = FACE_OUTER_BOUND ( 'NONE', #41533, .T. ) ;
#11219 = CARTESIAN_POINT ( 'NONE',  ( -151.5570736234661808, -1.166476076187852838E-15, -9.524999999999991473 ) ) ;
#11220 = CIRCLE ( 'NONE', #4466, 0.5000000000000004441 ) ;
#11221 = DIRECTION ( 'NONE',  ( 0.000000000000000000, 1.000000000000000000, 0.000000000000000000 ) ) ;
#11222 = ORIENTED_EDGE ( 'NONE', *, *, #41087, .T. ) ;
#11223 = CARTESIAN_POINT ( 'NONE',  ( -7.632228543268607446, 132.5429263765338135, -2.479861379858953718 ) ) ;
#11224 = CARTESIAN_POINT ( 'NONE',  ( -45.50000000000000000, -2.024042244987997205E-14, -6.500000000000000000 ) ) ;
#11225 = CARTESIAN_POINT ( 'NONE',  ( -75.16423876665271564, 36.16671995880537338, -9.876590145901744222 ) ) ;
#11226 = CARTESIAN_POINT ( 'NONE',  ( 2.607480562269075985, 125.7929263765338277, -8.025000000000000355 ) ) ;
#11227 = CARTESIAN_POINT ( 'NONE',  ( -41.49999999999998579, 106.9282032302754999, -4.000000000000000000 ) ) ;
#11228 = EDGE_CURVE ( 'NONE', #66508, #35623, #54832, .T. ) ;
#11229 = EDGE_LOOP ( 'NONE', ( #10188, #20783, #67897, #41258 ) ) ;
#11230 = STYLED_ITEM ( 'NONE', ( #57831 ), #20656 ) ;
#11231 = CYLINDRICAL_SURFACE ( 'NONE', #53181, 1.999999999999998224 ) ;
#11232 = ORIENTED_EDGE ( 'NONE', *, *, #10112, .F. ) ;
#11233 = FACE_OUTER_BOUND ( 'NONE', #14390, .T. ) ;
#11234 = DIRECTION ( 'NONE',  ( 0.000000000000000000, 0.000000000000000000, 1.000000000000000000 ) ) ;
#11235 = CARTESIAN_POINT ( 'NONE',  ( -195.0000000000000000, 0.000000000000000000, 0.000000000000000000 ) ) ;
#11236 = FILL_AREA_STYLE_COLOUR ( '', #54625 ) ;
#11237 = CARTESIAN_POINT ( 'NONE',  ( -146.3049999999999784, 8.437984349512085203, -1.550032578732815448E-15 ) ) ;
#11238 = EDGE_CURVE ( 'NONE', #15151, #36166, #22507, .T. ) ;
#11239 = AXIS2_PLACEMENT_3D ( 'NONE', #38762, #2405, #28837 ) ;
#11240 = CARTESIAN_POINT ( 'NONE',  ( -9.827790563157511022E-16, 116.5570736234661666, 8.025000000000000355 ) ) ;
#11241 =( GEOMETRIC_REPRESENTATION_CONTEXT ( 3 ) GLOBAL_UNCERTAINTY_ASSIGNED_CONTEXT ( ( #27805 ) ) GLOBAL_UNIT_ASSIGNED_CONTEXT ( ( #222, #49193, #59720 ) ) REPRESENTATION_CONTEXT ( 'NONE', 'WORKASPACE' ) );
#11242 = CARTESIAN_POINT ( 'NONE',  ( 41.36494435661962399, 107.7173713599237601, 3.929015280518105335 ) ) ;
#11243 = ORIENTED_EDGE ( 'NONE', *, *, #64252, .F. ) ;
#11244 = AXIS2_PLACEMENT_3D ( 'NONE', #26905, #52993, #52650 ) ;
#11245 = ORIENTED_EDGE ( 'NONE', *, *, #52862, .T. ) ;
#11246 = DIRECTION ( 'NONE',  ( 0.000000000000000000, 0.000000000000000000, -1.000000000000000000 ) ) ;
#11247 = DIRECTION ( 'NONE',  ( -1.000000000000000000, 0.000000000000000000, 0.000000000000000000 ) ) ;
#11248 = CARTESIAN_POINT ( 'NONE',  ( -56.15499999999997982, 7.632228543268600340, 2.479861379858949277 ) ) ;
#11249 = EDGE_LOOP ( 'NONE', ( #64684, #40739, #13548, #26623 ) ) ;
#11250 = FACE_OUTER_BOUND ( 'NONE', #66139, .T. ) ;
#11251 = CARTESIAN_POINT ( 'NONE',  ( 10.99999999999999645, 11.99999999999999289, 4.000000000000000000 ) ) ;
#11252 = LINE ( 'NONE', #955, #22807 ) ;
#11253 = DIRECTION ( 'NONE',  ( 1.000000000000000000, 0.000000000000000000, -0.000000000000000000 ) ) ;
#11254 = AXIS2_PLACEMENT_3D ( 'NONE', #41173, #31959, #53433 ) ;
#11255 = CIRCLE ( 'NONE', #45041, 0.2500000000000002220 ) ;
#11256 = DIRECTION ( 'NONE',  ( -1.000000000000000000, 0.000000000000000000, 0.000000000000000000 ) ) ;
#11257 = CARTESIAN_POINT ( 'NONE',  ( -83.49999999999997158, 50.00000000000000000, -11.50000000000000000 ) ) ;
#11258 = AXIS2_PLACEMENT_3D ( 'NONE', #42314, #37020, #4959 ) ;
#11259 = VERTEX_POINT ( 'NONE', #21819 ) ;
#11260 = FACE_OUTER_BOUND ( 'NONE', #3025, .T. ) ;
#11261 = PLANE ( 'NONE',  #24103 ) ;
#11262 = CARTESIAN_POINT ( 'NONE',  ( -111.4449999999999932, 0.000000000000000000, 8.024999999999991473 ) ) ;
#11263 = CARTESIAN_POINT ( 'NONE',  ( -5.598654528085806881, 154.7450000000000045, -7.705886871421374629 ) ) ;
#11264 = CARTESIAN_POINT ( 'NONE',  ( -92.24499999999999034, -4.716976649647093289, -6.492361379858945902 ) ) ;
#11265 = ADVANCED_FACE ( 'NONE', ( #11250 ), #65762, .T. ) ;
#11266 = CARTESIAN_POINT ( 'NONE',  ( 2.999999999999993339, 5.000000000000000000, 24.00402776293822882 ) ) ;
#11267 = CARTESIAN_POINT ( 'NONE',  ( 74.89452121010485541, 1.000000000000000000, -66.39042820928574429 ) ) ;
#11268 = CARTESIAN_POINT ( 'NONE',  ( -57.11974195712093660, -13.49999999999999112, -2.000000000000000000 ) ) ;
#11269 = CARTESIAN_POINT ( 'NONE',  ( -71.49999999999998579, 119.9999999999997868, -7.000000000000000000 ) ) ;
#11270 =( BOUNDED_CURVE ( )  B_SPLINE_CURVE ( 2, ( #36557, #35812, #57256, #36884, #20678, #9089, #3759, #30505, #57974, #4113, #52003 ),
 .UNSPECIFIED., .F., .F. ) 
 B_SPLINE_CURVE_WITH_KNOTS ( ( 3, 2, 2, 2, 2, 3 ),
 ( 0.3152173913043403997, 0.3173913043478185925, 0.3195652173912967853, 0.3217391304347749781, 0.3239130434782532264, 0.3260869565217314192 ),
 .UNSPECIFIED. ) 
 CURVE ( )  GEOMETRIC_REPRESENTATION_ITEM ( )  RATIONAL_B_SPLINE_CURVE ( ( 1.000000000000167422, 0.9510565162949861095, 1.000000000000000000, 0.9510565162951535312, 1.000000000000000000, 0.9510565162951535312, 1.000000000000000000, 0.9510565162951535312, 1.000000000000000000, 0.9510565162953272811, 0.9999999999998262501 ) ) 
 REPRESENTATION_ITEM ( '' )  );
#11271 = DIRECTION ( 'NONE',  ( -1.000000000000000000, 0.000000000000000000, 0.000000000000000000 ) ) ;
#11273 = ORIENTED_EDGE ( 'NONE', *, *, #6847, .T. ) ;
#11272 = VECTOR ( 'NONE', #44026, 1000.000000000000000 ) ;
#11274 = EDGE_CURVE ( 'NONE', #29573, #65886, #6642, .T. ) ;
#11275 = CARTESIAN_POINT ( 'NONE',  ( -122.0929263765338106, 3.094860106618433360, 9.524999999999991473 ) ) ;
#11276 = CARTESIAN_POINT ( 'NONE',  ( -143.5449999999999875, -7.632228543268600340, -2.479861379858950166 ) ) ;
#11277 = LINE ( 'NONE', #5632, #59429 ) ;
#11278 = EDGE_CURVE ( 'NONE', #54731, #23185, #19100, .T. ) ;
#11279 = DIRECTION ( 'NONE',  ( -1.000000000000000000, 0.000000000000000000, 0.000000000000000000 ) ) ;
#11280 = VECTOR ( 'NONE', #20789, 1000.000000000000000 ) ;
#11281 = SURFACE_STYLE_FILL_AREA ( #44038 ) ;
#11282 = ORIENTED_EDGE ( 'NONE', *, *, #66005, .T. ) ;
#11283 = ORIENTED_EDGE ( 'NONE', *, *, #6435, .F. ) ;
#11284 = LINE ( 'NONE', #33100, #24667 ) ;
#11285 = DIRECTION ( 'NONE',  ( 0.000000000000000000, 1.000000000000000000, 0.000000000000000000 ) ) ;
#11286 = STYLED_ITEM ( 'NONE', ( #12483 ), #33509 ) ;
#11287 = CARTESIAN_POINT ( 'NONE',  ( -155.5429263765338135, 9.058813317711329915, 2.943386871421369566 ) ) ;
#11288 = SURFACE_STYLE_FILL_AREA ( #34130 ) ;
#11289 =( NAMED_UNIT ( * ) SI_UNIT ( $, .STERADIAN. ) SOLID_ANGLE_UNIT ( ) );
#11290 = CARTESIAN_POINT ( 'NONE',  ( -116.2429263765338021, 5.598654528085804216, 7.705886871421366635 ) ) ;
#11292 = EDGE_CURVE ( 'NONE', #2410, #58564, #65418, .T. ) ;
#11291 = FACE_OUTER_BOUND ( 'NONE', #54414, .T. ) ;
#11293 = ORIENTED_EDGE ( 'NONE', *, *, #27044, .F. ) ;
#11294 = CARTESIAN_POINT ( 'NONE',  ( -137.4549999999999841, 7.632228543268599452, -2.479861379858951942 ) ) ;
#11295 = VERTEX_POINT ( 'NONE', #54503 ) ;
#11296 = ORIENTED_EDGE ( 'NONE', *, *, #2974, .F. ) ;
#11297 =( NAMED_UNIT ( * ) SI_UNIT ( $, .STERADIAN. ) SOLID_ANGLE_UNIT ( ) );
#11298 = CARTESIAN_POINT ( 'NONE',  ( 0.000000000000000000, 87.30187232391182306, 0.000000000000000000 ) ) ;
#11299 = VERTEX_POINT ( 'NONE', #27744 ) ;
#11300 = CONICAL_SURFACE ( 'NONE', #66372, 9.000000000000007105, 0.7853981633974500554 ) ;
#11301 = DIRECTION ( 'NONE',  ( 1.000000000000000000, -6.162975822039156098E-33, -1.300977106640435384E-16 ) ) ;
#11302 = FILL_AREA_STYLE_COLOUR ( '', #33145 ) ;
#11303 = CARTESIAN_POINT ( 'NONE',  ( 3.094860106618435136, 133.2950000000000159, -9.525000000000000355 ) ) ;
#11304 = PRESENTATION_LAYER_ASSIGNMENT (  '', '', ( #45044 ) ) ;
#11305 = PRODUCT_DEFINITION_FORMATION_WITH_SPECIFIED_SOURCE ( 'ANY', '', #10291, .NOT_KNOWN. ) ;
#11306 = ORIENTED_EDGE ( 'NONE', *, *, #69031, .T. ) ;
#11307 = DIRECTION ( 'NONE',  ( -1.000000000000000000, -0.000000000000000000, -0.000000000000000000 ) ) ;
#11308 = CARTESIAN_POINT ( 'NONE',  ( -3.094860106618432471, 131.7049999999999557, -9.525000000000000355 ) ) ;
#11309 = CARTESIAN_POINT ( 'NONE',  ( -56.90499999999998693, 2.607480562269069324, -8.024999999999993250 ) ) ;
#11310 = CARTESIAN_POINT ( 'NONE',  ( -119.9949999999999903, -6.826472737025115478, 4.959722759717900331 ) ) ;
#11311 = CARTESIAN_POINT ( 'NONE',  ( 71.50000000000000000, 35.92875272052971525, 7.500000000000000000 ) ) ;
#11312 = EDGE_LOOP ( 'NONE', ( #27949, #56843, #14730, #30559 ) ) ;
#11313 = CARTESIAN_POINT ( 'NONE',  ( 8.102448949553183510, 149.1049999999999898, -5.886773742842746238 ) ) ;
#11314 =( NAMED_UNIT ( * ) PLANE_ANGLE_UNIT ( ) SI_UNIT ( $, .RADIAN. ) );
#11315 = STYLED_ITEM ( 'NONE', ( #13161 ), #14448 ) ;
#11316 = CARTESIAN_POINT ( 'NONE',  ( 8.000000000000001776, 30.99999999999998579, 4.000000000000000000 ) ) ;
#11317 = CARTESIAN_POINT ( 'NONE',  ( -48.50000000000000000, 14.49137674618942562, -9.500000000000000000 ) ) ;
#11318 = CYLINDRICAL_SURFACE ( 'NONE', #21630, 1.000000000000000888 ) ;
#11319 = VERTEX_POINT ( 'NONE', #28437 ) ;
#11320 = CARTESIAN_POINT ( 'NONE',  ( -33.58491031241940306, -9.466447511860014430, -3.170070218111009197 ) ) ;
#11321 =( LENGTH_UNIT ( ) NAMED_UNIT ( * ) SI_UNIT ( .MILLI., .METRE. ) );
#11322 = CARTESIAN_POINT ( 'NONE',  ( -172.5549999999999784, 0.000000000000000000, 8.024999999999991473 ) ) ;
#11323 = ORIENTED_EDGE ( 'NONE', *, *, #46868, .T. ) ;
#11324 = MECHANICAL_DESIGN_GEOMETRIC_PRESENTATION_REPRESENTATION (  '', ( #48469 ), #42860 ) ;
#11325 = CARTESIAN_POINT ( 'NONE',  ( -183.9999999999999147, -7.795498455245760461, 2.554623800884867624 ) ) ;
#11326 = DIRECTION ( 'NONE',  ( 1.000000000000000000, 0.000000000000000000, 0.000000000000000000 ) ) ;
#11327 = CARTESIAN_POINT ( 'NONE',  ( 54.49999999999999289, 1.797044900979284448E-15, 6.500000000000000000 ) ) ;
#11328 = ORIENTED_EDGE ( 'NONE', *, *, #33071, .T. ) ;
#11329 = CARTESIAN_POINT ( 'NONE',  ( -44.99742019440035534, 9.654572671137946926, -3.431488482060549128 ) ) ;
#11330 = CARTESIAN_POINT ( 'NONE',  ( -86.45499999999998408, 7.632228543268599452, -2.479861379858951942 ) ) ;
#11331 = VERTEX_POINT ( 'NONE', #17266 ) ;
#11332 = AXIS2_PLACEMENT_3D ( 'NONE', #31789, #48713, #32835 ) ;
#11333 = CARTESIAN_POINT ( 'NONE',  ( 28.00000000000002842, 42.00000000000000000, 3.902931319921305165E-16 ) ) ;
#11334 = MECHANICAL_DESIGN_GEOMETRIC_PRESENTATION_REPRESENTATION (  '', ( #45075 ), #10252 ) ;
#11335 = CARTESIAN_POINT ( 'NONE',  ( 4.716976649647099507, 144.7570736234661410, -6.492361379858953008 ) ) ;
#11336 = LINE ( 'NONE', #50039, #18497 ) ;
#11337 = CARTESIAN_POINT ( 'NONE',  ( -69.35707362346617799, 5.598654528085804216, 7.705886871421366635 ) ) ;
#11338 = AXIS2_PLACEMENT_3D ( 'NONE', #66380, #56165, #61434 ) ;
#11339 = ORIENTED_EDGE ( 'NONE', *, *, #20275, .F. ) ;
#11340 = DIRECTION ( 'NONE',  ( -1.000000000000000000, -0.000000000000000000, -0.000000000000000000 ) ) ;
#11342 =( NAMED_UNIT ( * ) PLANE_ANGLE_UNIT ( ) SI_UNIT ( $, .RADIAN. ) );
#11341 = FILL_AREA_STYLE_COLOUR ( '', #45972 ) ;
#11343 = CARTESIAN_POINT ( 'NONE',  ( -106.2549999999999955, -4.716976649647092401, 6.492361379858946790 ) ) ;
#11344 = CARTESIAN_POINT ( 'NONE',  ( -10.01517768586949231, 134.1949999999999932, -6.132527647946036459E-16 ) ) ;
#11345 = CARTESIAN_POINT ( 'NONE',  ( -118.6449999999999818, 4.716976649647091513, -6.492361379858946790 ) ) ;
#11346 = VECTOR ( 'NONE', #11139, 1000.000000000000000 ) ;
#11347 = ADVANCED_FACE ( 'NONE', ( #38730 ), #64725, .F. ) ;
#11348 = STYLED_ITEM ( 'NONE', ( #55043 ), #17033 ) ;
#11349 = VERTEX_POINT ( 'NONE', #54001 ) ;
#11351 = CARTESIAN_POINT ( 'NONE',  ( -7.731910350068054619E-16, -6.500000000000000888, 3.000000000000000000 ) ) ;
#11350 = CARTESIAN_POINT ( 'NONE',  ( 45.65811388300841855, 10.21937129433613478, 3.598410089384283417 ) ) ;
#11352 = CARTESIAN_POINT ( 'NONE',  ( -156.7429263765338021, -5.598654528085803328, -7.705886871421366635 ) ) ;
#11353 = CARTESIAN_POINT ( 'NONE',  ( -176.8449999999999989, -7.632228543268599452, 2.479861379858951054 ) ) ;
#11354 = EDGE_CURVE ( 'NONE', #56002, #45281, #62204, .T. ) ;
#11355 = ADVANCED_FACE ( 'NONE', ( #3060 ), #2004, .F. ) ;
#11356 =( NAMED_UNIT ( * ) PLANE_ANGLE_UNIT ( ) SI_UNIT ( $, .RADIAN. ) );
#11357 = EDGE_CURVE ( 'NONE', #3674, #4136, #62939, .T. ) ;
#11358 = VERTEX_POINT ( 'NONE', #23878 ) ;
#11359 = DIRECTION ( 'NONE',  ( 0.000000000000000000, -1.000000000000000000, 0.000000000000000000 ) ) ;
#11360 = FACE_OUTER_BOUND ( 'NONE', #65371, .T. ) ;
#11361 = VERTEX_POINT ( 'NONE', #50969 ) ;
#11362 = VECTOR ( 'NONE', #37734, 1000.000000000000000 ) ;
#11363 = EDGE_CURVE ( 'NONE', #54295, #55506, #66016, .T. ) ;
#11364 = CARTESIAN_POINT ( 'NONE',  ( -77.84292637653379643, 9.058813317711329915, -2.943386871421373119 ) ) ;
#11365 = ITEM_DEFINED_TRANSFORMATION ( 'NONE', 'NONE', #55070,  #42840 ) ;
#11366 = DIRECTION ( 'NONE',  ( 0.000000000000000000, 0.000000000000000000, 1.000000000000000000 ) ) ;
#11367 = DIRECTION ( 'NONE',  ( 1.000000000000000000, 0.000000000000000000, 0.000000000000000000 ) ) ;
#11368 = VECTOR ( 'NONE', #16781, 1000.000000000000000 ) ;
#11369 = ADVANCED_FACE ( 'NONE', ( #2730 ), #50621, .T. ) ;
#11370 = MECHANICAL_DESIGN_GEOMETRIC_PRESENTATION_REPRESENTATION (  '', ( #41744 ), #17024 ) ;
#11371 =( LENGTH_UNIT ( ) NAMED_UNIT ( * ) SI_UNIT ( .MILLI., .METRE. ) );
#11372 = DIRECTION ( 'NONE',  ( 0.000000000000000000, 0.000000000000000000, 1.000000000000000000 ) ) ;
#11373 = DIRECTION ( 'NONE',  ( 1.000000000000000000, -0.000000000000000000, 0.000000000000000000 ) ) ;
#11374 = CARTESIAN_POINT ( 'NONE',  ( -78.74292637653380211, -5.598654528085803328, -7.705886871421366635 ) ) ;
#11375 = ORIENTED_EDGE ( 'NONE', *, *, #63113, .T. ) ;
#11376 = CARTESIAN_POINT ( 'NONE',  ( -166.8549999999999898, 4.716976649647094177, 6.492361379858945902 ) ) ;
#11377 = ORIENTED_EDGE ( 'NONE', *, *, #58298, .F. ) ;
#11378 = CARTESIAN_POINT ( 'NONE',  ( 7.999999999999992895, 0.000000000000000000, -24.00402776293826079 ) ) ;
#11379 = FACE_OUTER_BOUND ( 'NONE', #7343, .T. ) ;
#11380 = PRESENTATION_LAYER_ASSIGNMENT (  '', '', ( #2317 ) ) ;
#11381 = DIRECTION ( 'NONE',  ( 0.000000000000000000, 0.000000000000000000, -1.000000000000000000 ) ) ;
#11382 = SURFACE_SIDE_STYLE ('',( #58890 ) ) ;
#11383 = CARTESIAN_POINT ( 'NONE',  ( 7.632228543268607446, 153.1570736234661751, 2.479861379858954606 ) ) ;
#11384 = VERTEX_POINT ( 'NONE', #62543 ) ;
#11385 = CARTESIAN_POINT ( 'NONE',  ( 7.632228543268608334, 137.3429263765337964, -2.479861379858951942 ) ) ;
#11386 = CARTESIAN_POINT ( 'NONE',  ( -93.65499999999998693, -7.632228543268600340, -2.479861379858950166 ) ) ;
#11387 = MECHANICAL_DESIGN_GEOMETRIC_PRESENTATION_REPRESENTATION (  '', ( #42925 ), #25988 ) ;
#11388 = DIRECTION ( 'NONE',  ( -1.000000000000000000, 0.000000000000000000, 0.000000000000000000 ) ) ;
#11389 = ORIENTED_EDGE ( 'NONE', *, *, #63688, .T. ) ;
#11390 = CARTESIAN_POINT ( 'NONE',  ( 57.00000000000000000, 5.000000000000000000, -60.00402776293825724 ) ) ;
#11391 = MECHANICAL_DESIGN_GEOMETRIC_PRESENTATION_REPRESENTATION (  '', ( #58598 ), #6929 ) ;
#11392 = CARTESIAN_POINT ( 'NONE',  ( 5.196152422706631135, -1.107695154586740394, 9.000000000000001776 ) ) ;
#11393 = VERTEX_POINT ( 'NONE', #52711 ) ;
#11394 = FACE_OUTER_BOUND ( 'NONE', #33617, .T. ) ;
#11395 = CARTESIAN_POINT ( 'NONE',  ( -62.09499999999998465, -2.607480562269071545, -8.024999999999991473 ) ) ;
#11396 = ORIENTED_EDGE ( 'NONE', *, *, #22695, .F. ) ;
#11397 = CIRCLE ( 'NONE', #2347, 0.5000000000000004441 ) ;
#11398 = FILL_AREA_STYLE ('',( #27561 ) ) ;
#11399 = AXIS2_PLACEMENT_3D ( 'NONE', #41128, #62533, #14348 ) ;
#11400 = DIRECTION ( 'NONE',  ( -1.000000000000000000, 0.000000000000000000, 0.000000000000000000 ) ) ;
#11401 = FACE_OUTER_BOUND ( 'NONE', #59850, .T. ) ;
#11402 = ORIENTED_EDGE ( 'NONE', *, *, #50599, .T. ) ;
#11403 =( LENGTH_UNIT ( ) NAMED_UNIT ( * ) SI_UNIT ( .MILLI., .METRE. ) );
#11404 = CARTESIAN_POINT ( 'NONE',  ( 3.000000000000030198, 42.00000000000000000, 89.00000000000000000 ) ) ;
#11405 = ORIENTED_EDGE ( 'NONE', *, *, #6903, .F. ) ;
#11406 = CARTESIAN_POINT ( 'NONE',  ( 0.2500000000000000000, 36.99999999999999289, 4.000000000000000000 ) ) ;
#11407 = DIRECTION ( 'NONE',  ( 0.000000000000000000, 1.000000000000000000, 0.000000000000000000 ) ) ;
#11408 = CARTESIAN_POINT ( 'NONE',  ( -111.2049999999999983, -2.607480562269071545, -8.024999999999991473 ) ) ;
#11409 = ORIENTED_EDGE ( 'NONE', *, *, #16967, .T. ) ;
#11410 = DIRECTION ( 'NONE',  ( 0.000000000000000000, -0.000000000000000000, 1.000000000000000000 ) ) ;
#11411 = DIRECTION ( 'NONE',  ( -0.000000000000000000, -0.000000000000000000, -1.000000000000000000 ) ) ;
#11412 = CARTESIAN_POINT ( 'NONE',  ( 13.50000000000000533, 30.99999999999999289, 4.000000000000000000 ) ) ;
#11413 = FILL_AREA_STYLE ('',( #27218 ) ) ;
#11414 = CARTESIAN_POINT ( 'NONE',  ( -152.9070736234662036, -3.094860106618429807, 9.524999999999991473 ) ) ;
#11415 = TOROIDAL_SURFACE ( 'NONE', #18193, 22.50000000000000000, 0.5000000000000000000 ) ;
#11416 = CARTESIAN_POINT ( 'NONE',  ( -8.102448949553179958, 136.8949999999999534, -5.886773742842749790 ) ) ;
#11417 = CARTESIAN_POINT ( 'NONE',  ( -90.50707362346618368, 8.102448949553176405, 5.886773742842740909 ) ) ;
#11418 = CONICAL_SURFACE ( 'NONE', #145, 7.000000000000000888, 0.7853981633974500554 ) ;
#11419 = SURFACE_STYLE_FILL_AREA ( #43148 ) ;
#11420 = ORIENTED_EDGE ( 'NONE', *, *, #35925, .F. ) ;
#11421 =( GEOMETRIC_REPRESENTATION_CONTEXT ( 3 ) GLOBAL_UNCERTAINTY_ASSIGNED_CONTEXT ( ( #37134 ) ) GLOBAL_UNIT_ASSIGNED_CONTEXT ( ( #37584, #20296, #9425 ) ) REPRESENTATION_CONTEXT ( 'NONE', 'WORKASPACE' ) );
#11423 = MECHANICAL_DESIGN_GEOMETRIC_PRESENTATION_REPRESENTATION (  '', ( #40631 ), #39526 ) ;
#11422 = DIRECTION ( 'NONE',  ( -0.000000000000000000, -0.000000000000000000, -1.000000000000000000 ) ) ;
#11424 = SURFACE_STYLE_FILL_AREA ( #42451 ) ;
#11425 = CARTESIAN_POINT ( 'NONE',  ( -129.8050000000000068, -8.437984349512085203, 5.166775262442717831E-16 ) ) ;
#11426 = DIRECTION ( 'NONE',  ( 0.000000000000000000, -1.000000000000000000, -0.000000000000000000 ) ) ;
#11427 = LINE ( 'NONE', #27589, #2102 ) ;
#11428 = DIRECTION ( 'NONE',  ( 0.000000000000000000, -0.000000000000000000, 1.000000000000000000 ) ) ;
#11429 = AXIS2_PLACEMENT_3D ( 'NONE', #63635, #53096, #25987 ) ;
#11430 = CARTESIAN_POINT ( 'NONE',  ( -148.1950000000000216, 8.437984349512085203, -1.550032578732815448E-15 ) ) ;
#11431 = EDGE_CURVE ( 'NONE', #1416, #65761, #3524, .T. ) ;
#11432 = CARTESIAN_POINT ( 'NONE',  ( -138.2949999999999875, -2.607480562269069768, 8.024999999999991473 ) ) ;
#11433 = ORIENTED_EDGE ( 'NONE', *, *, #40790, .F. ) ;
#11434 = EDGE_CURVE ( 'NONE', #30747, #49901, #16133, .T. ) ;
#11435 = STYLED_ITEM ( 'NONE', ( #15163 ), #54541 ) ;
#11436 = UNCERTAINTY_MEASURE_WITH_UNIT (LENGTH_MEASURE( 1.000000000000000082E-05 ), #1647, 'distance_accuracy_value', 'NONE');
#11437 = CARTESIAN_POINT ( 'NONE',  ( -51.05499999999999261, -9.827790563157499189E-16, -8.024999999999991473 ) ) ;
#11438 = FILL_AREA_STYLE ('',( #53658 ) ) ;
#11439 = CIRCLE ( 'NONE', #14835, 17.50000000000000000 ) ;
#11440 = CARTESIAN_POINT ( 'NONE',  ( -57.44499999999999318, 0.000000000000000000, 8.024999999999991473 ) ) ;
#11441 = AXIS2_PLACEMENT_3D ( 'NONE', #29316, #19464, #18775 ) ;
#11442 = CYLINDRICAL_SURFACE ( 'NONE', #32049, 0.5000000000000004441 ) ;
#11443 = SURFACE_SIDE_STYLE ('',( #49789 ) ) ;
#11444 = CYLINDRICAL_SURFACE ( 'NONE', #51172, 8.025000000000000355 ) ;
#11445 = CIRCLE ( 'NONE', #41819, 16.00000000000000000 ) ;
#11446 = EDGE_CURVE ( 'NONE', #55926, #11014, #19802, .T. ) ;
#11447 = LINE ( 'NONE', #60656, #23354 ) ;
#11448 = DIRECTION ( 'NONE',  ( -0.000000000000000000, -0.000000000000000000, -1.000000000000000000 ) ) ;
#11449 = CARTESIAN_POINT ( 'NONE',  ( -107.5429263765337993, 9.058813317711329915, 2.943386871421369566 ) ) ;
#11450 = DIRECTION ( 'NONE',  ( -3.102125002257859534E-16, -1.067062355321543450E-15, 1.000000000000000000 ) ) ;
#11451 = CARTESIAN_POINT ( 'NONE',  ( 24.00000000000000000, 1.000000000000000000, -3.000000000000000000 ) ) ;
#11452 = CIRCLE ( 'NONE', #66547, 0.2500000000000002220 ) ;
#11453 = ADVANCED_FACE ( 'NONE', ( #25597 ), #9807, .T. ) ;
#11454 = FACE_OUTER_BOUND ( 'NONE', #26589, .T. ) ;
#11455 = DIRECTION ( 'NONE',  ( -1.000000000000000000, 0.000000000000000000, 0.000000000000000000 ) ) ;
#11456 = STYLED_ITEM ( 'NONE', ( #57155 ), #24240 ) ;
#11457 = PLANE ( 'NONE',  #20372 ) ;
#11458 = ORIENTED_EDGE ( 'NONE', *, *, #21858, .T. ) ;
#11459 = DIRECTION ( 'NONE',  ( 1.000000000000000000, 0.000000000000000000, 0.000000000000000000 ) ) ;
#11460 = DIRECTION ( 'NONE',  ( -1.000000000000000000, 0.000000000000000000, 0.000000000000000000 ) ) ;
#11461 = VERTEX_POINT ( 'NONE', #57633 ) ;
#11462 = CARTESIAN_POINT ( 'NONE',  ( 4.716976649647096842, 113.8570736234661638, 6.492361379858953896 ) ) ;
#11463 = AXIS2_PLACEMENT_3D ( 'NONE', #67556, #18994, #18343 ) ;
#11464 = AXIS2_PLACEMENT_3D ( 'NONE', #7391, #60479, #65436 ) ;
#11465 = CARTESIAN_POINT ( 'NONE',  ( -45.50000000000000000, 99.99999999999992895, 9.500000000000000000 ) ) ;
#11466 = CARTESIAN_POINT ( 'NONE',  ( 75.00000000000000000, 20.36037961002804408, -6.000000000000000000 ) ) ;
#11467 = PRESENTATION_LAYER_ASSIGNMENT (  '', '', ( #21615 ) ) ;
#11468 = ADVANCED_FACE ( 'NONE', ( #63253 ), #34271, .F. ) ;
#11469 = ORIENTED_EDGE ( 'NONE', *, *, #10012, .T. ) ;
#11470 = EDGE_LOOP ( 'NONE', ( #67175, #55646, #36392 ) ) ;
#11471 = FACE_OUTER_BOUND ( 'NONE', #22310, .T. ) ;
#11472 = SURFACE_SIDE_STYLE ('',( #23083 ) ) ;
#11473 = VERTEX_POINT ( 'NONE', #20694 ) ;
#11474 =( NAMED_UNIT ( * ) SI_UNIT ( $, .STERADIAN. ) SOLID_ANGLE_UNIT ( ) );
#11475 =( NAMED_UNIT ( * ) SI_UNIT ( $, .STERADIAN. ) SOLID_ANGLE_UNIT ( ) );
#11476 = MECHANICAL_DESIGN_GEOMETRIC_PRESENTATION_REPRESENTATION (  '', ( #56418 ), #31671 ) ;
#11477 = DIRECTION ( 'NONE',  ( 0.000000000000000000, 0.000000000000000000, -1.000000000000000000 ) ) ;
#11478 = CARTESIAN_POINT ( 'NONE',  ( -88.34499999999999886, 7.632228543268599452, -2.479861379858951942 ) ) ;
#11479 = ORIENTED_EDGE ( 'NONE', *, *, #15533, .F. ) ;
#11480 = EDGE_CURVE ( 'NONE', #20740, #17716, #28209, .T. ) ;
#11481 = VECTOR ( 'NONE', #17892, 1000.000000000000000 ) ;
#11482 = FILL_AREA_STYLE ('',( #50177 ) ) ;
#11483 =( NAMED_UNIT ( * ) SI_UNIT ( $, .STERADIAN. ) SOLID_ANGLE_UNIT ( ) );
#11484 = UNCERTAINTY_MEASURE_WITH_UNIT (LENGTH_MEASURE( 1.000000000000000082E-05 ), #19867, 'distance_accuracy_value', 'NONE');
#11485 = EDGE_LOOP ( 'NONE', ( #65846, #1381, #38070, #1761 ) ) ;
#11486 = CARTESIAN_POINT ( 'NONE',  ( -174.8929263765337794, -8.102448949553174629, -5.886773742842741797 ) ) ;
#11487 = DIRECTION ( 'NONE',  ( 1.000000000000000000, -7.080503983578803083E-17, 0.000000000000000000 ) ) ;
#11488 = DIRECTION ( 'NONE',  ( -1.000000000000000000, 1.189524669241239115E-16, 0.000000000000000000 ) ) ;
#11489 = MECHANICAL_DESIGN_GEOMETRIC_PRESENTATION_REPRESENTATION (  '', ( #55280 ), #51935 ) ;
#11490 = DIRECTION ( 'NONE',  ( -1.000000000000000000, 0.000000000000000000, 1.300977106640435137E-16 ) ) ;
#11491 = ORIENTED_EDGE ( 'NONE', *, *, #62437, .F. ) ;
#11492 = AXIS2_PLACEMENT_3D ( 'NONE', #59784, #28432, #12262 ) ;
#11493 = CARTESIAN_POINT ( 'NONE',  ( -71.99999999999998579, 64.07124727947029896, -9.500000000000000000 ) ) ;
#11494 = ORIENTED_EDGE ( 'NONE', *, *, #64178, .F. ) ;
#11495 = CARTESIAN_POINT ( 'NONE',  ( 28.58578643762692550, 42.99999999999999289, 79.58981420056515788 ) ) ;
#11496 = LINE ( 'NONE', #11841, #6544 ) ;
#11497 = CARTESIAN_POINT ( 'NONE',  ( 45.07697505292422591, 10.02565835097472480, 3.091949714863343246 ) ) ;
#11498 = PLANE ( 'NONE',  #39822 ) ;
#11499 = MECHANICAL_DESIGN_GEOMETRIC_PRESENTATION_REPRESENTATION (  '', ( #48667 ), #58703 ) ;
#11500 = CARTESIAN_POINT ( 'NONE',  ( -8.601545703395441222, 153.5693124935650360, 0.4166762051479260820 ) ) ;
#11501 = EDGE_LOOP ( 'NONE', ( #52432, #11213, #4097, #7421, #22501, #44492, #24691, #1755 ) ) ;
#11502 = VECTOR ( 'NONE', #42360, 1000.000000000000000 ) ;
#11503 = PRESENTATION_STYLE_ASSIGNMENT (( #27311 ) ) ;
#11504 = CARTESIAN_POINT ( 'NONE',  ( 60.00000000000000000, 1.797044900979284448E-15, 11.50000000000003730 ) ) ;
#11505 = EDGE_CURVE ( 'NONE', #6607, #20333, #9196, .T. ) ;
#11506 = VERTEX_POINT ( 'NONE', #23711 ) ;
#11507 = PRESENTATION_STYLE_ASSIGNMENT (( #22073 ) ) ;
#11508 = CARTESIAN_POINT ( 'NONE',  ( -166.8549999999999898, 4.716976649647094177, 6.492361379858945902 ) ) ;
#11509 = ADVANCED_FACE ( 'NONE', ( #7532 ), #38641, .T. ) ;
#11510 = LINE ( 'NONE', #200, #29630 ) ;
#11511 = CARTESIAN_POINT ( 'NONE',  ( 32.00000000000001421, -60.04052944165106709, 35.50000000000000000 ) ) ;
#11512 = CARTESIAN_POINT ( 'NONE',  ( -170.9950000000000330, -6.826472737025115478, 4.959722759717900331 ) ) ;
#11513 = MECHANICAL_DESIGN_GEOMETRIC_PRESENTATION_REPRESENTATION (  '', ( #18408 ), #57734 ) ;
#11514 = CARTESIAN_POINT ( 'NONE',  ( -169.3449999999999989, 7.632228543268599452, -2.479861379858951942 ) ) ;
#11515 = ORIENTED_EDGE ( 'NONE', *, *, #37637, .T. ) ;
#11516 = PRESENTATION_LAYER_ASSIGNMENT (  '', '', ( #7050 ) ) ;
#11517 = EDGE_CURVE ( 'NONE', #67683, #68764, #32774, .T. ) ;
#11518 = CARTESIAN_POINT ( 'NONE',  ( 45.30708737912571848, 10.10236245970856750, 3.219298532130914658 ) ) ;
#11519 = CARTESIAN_POINT ( 'NONE',  ( -82.85499999999998977, 4.716976649647094177, 6.492361379858945902 ) ) ;
#11520 = CARTESIAN_POINT ( 'NONE',  ( 24.68215826162192528, 25.64799036762169848, 27.48644429636420128 ) ) ;
#11521 = DIRECTION ( 'NONE',  ( 0.000000000000000000, -1.000000000000000000, 0.000000000000000000 ) ) ;
#11522 = CARTESIAN_POINT ( 'NONE',  ( -82.04499999999998749, 7.632228543268600340, 2.479861379858949277 ) ) ;
#11523 = CLOSED_SHELL ( 'NONE', ( #21668, #23996, #783, #17496, #62733, #57184 ) ) ;
#11524 = CARTESIAN_POINT ( 'NONE',  ( 5.598654528085809545, 140.2549999999999955, -7.705886871421373741 ) ) ;
#11525 = AXIS2_PLACEMENT_3D ( 'NONE', #18672, #40842, #25321 ) ;
#11526 = FACE_BOUND ( 'NONE', #61628, .T. ) ;
#11527 = EDGE_CURVE ( 'NONE', #47282, #35271, #57478, .T. ) ;
#11528 = PRODUCT_DEFINITION_SHAPE ( 'NONE', 'NONE',  #69709 ) ;
#11529 = SURFACE_STYLE_FILL_AREA ( #569 ) ;
#11530 = UNCERTAINTY_MEASURE_WITH_UNIT (LENGTH_MEASURE( 1.000000000000000082E-05 ), #69140, 'distance_accuracy_value', 'NONE');
#11531 = SURFACE_SIDE_STYLE ('',( #5541 ) ) ;
#11532 = EDGE_LOOP ( 'NONE', ( #29259, #24865, #47352, #28864 ) ) ;
#11533 = ADVANCED_FACE ( 'NONE', ( #21722 ), #66987, .F. ) ;
#11534 = CARTESIAN_POINT ( 'NONE',  ( -4.716976649647097730, 132.2429263765338021, -6.492361379858953896 ) ) ;
#11535 = CARTESIAN_POINT ( 'NONE',  ( -49.94292637653380496, 0.000000000000000000, 9.524999999999991473 ) ) ;
#11536 = AXIS2_PLACEMENT_3D ( 'NONE', #165, #64617, #43552 ) ;
#11537 = VECTOR ( 'NONE', #20329, 1000.000000000000000 ) ;
#11538 = DIRECTION ( 'NONE',  ( -0.000000000000000000, -0.000000000000000000, 1.000000000000000000 ) ) ;
#11539 = ORIENTED_EDGE ( 'NONE', *, *, #4758, .F. ) ;
#11540 = ORIENTED_EDGE ( 'NONE', *, *, #49675, .F. ) ;
#11541 =( LENGTH_UNIT ( ) NAMED_UNIT ( * ) SI_UNIT ( .MILLI., .METRE. ) );
#11542 = DIRECTION ( 'NONE',  ( 1.000000000000000000, 0.000000000000000000, 0.000000000000000000 ) ) ;
#11543 = DIRECTION ( 'NONE',  ( -0.000000000000000000, -0.000000000000000000, -1.000000000000000000 ) ) ;
#11544 =( BOUNDED_CURVE ( )  B_SPLINE_CURVE ( 2, ( #61259, #34523, #55977, #8157, #40180, #7787, #29236, #56685, #61578, #34873, #67231 ),
 .UNSPECIFIED., .F., .F. ) 
 B_SPLINE_CURVE_WITH_KNOTS ( ( 3, 2, 2, 2, 2, 3 ),
 ( 0.8586956521739130821, 0.8608695652173913304, 0.8630434782608695787, 0.8652173913043478271, 0.8673913043478260754, 0.8695652173913043237 ),
 .UNSPECIFIED. ) 
 CURVE ( )  GEOMETRIC_REPRESENTATION_ITEM ( )  RATIONAL_B_SPLINE_CURVE ( ( 1.000000000000000000, 0.9510565162951535312, 1.000000000000000000, 0.9510565162951535312, 1.000000000000000000, 0.9510565162951535312, 1.000000000000000000, 0.9510565162951535312, 1.000000000000000000, 0.9510565162951535312, 1.000000000000000000 ) ) 
 REPRESENTATION_ITEM ( '' )  );
#11545 = COLOUR_RGB ( '', 0.72549020, 0.75294118, 0.79215686) ;
#11546 = CARTESIAN_POINT ( 'NONE',  ( -70.10707362346617799, 8.102448949553172852, -5.886773742842744461 ) ) ;
#11547 = VERTEX_POINT ( 'NONE', #67316 ) ;
#11548 = CARTESIAN_POINT ( 'NONE',  ( -116.4549999999999841, 7.632228543268599452, -2.479861379858951942 ) ) ;
#11549 = ORIENTED_EDGE ( 'NONE', *, *, #19305, .T. ) ;
#11550 =( NAMED_UNIT ( * ) SI_UNIT ( $, .STERADIAN. ) SOLID_ANGLE_UNIT ( ) );
#11551 = SURFACE_SIDE_STYLE ('',( #34047 ) ) ;
#11552 = VERTEX_POINT ( 'NONE', #25786 ) ;
#11553 =( NAMED_UNIT ( * ) SI_UNIT ( $, .STERADIAN. ) SOLID_ANGLE_UNIT ( ) );
#11554 = CYLINDRICAL_SURFACE ( 'NONE', #2889, 0.2500000000000002220 ) ;
#11555 = ORIENTED_EDGE ( 'NONE', *, *, #30195, .F. ) ;
#11556 = AXIS2_PLACEMENT_3D ( 'NONE', #68271, #68973, #10220 ) ;
#11557 = STYLED_ITEM ( 'NONE', ( #42754 ), #61368 ) ;
#11558 = CARTESIAN_POINT ( 'NONE',  ( 15.98999599679679839, 146.9999999999999716, 7.500000000000000000 ) ) ;
#11559 = FILL_AREA_STYLE ('',( #39029 ) ) ;
#11560 = ORIENTED_EDGE ( 'NONE', *, *, #52752, .T. ) ;
#11561 = ADVANCED_FACE ( 'NONE', ( #20154 ), #8003, .T. ) ;
#11562 = ORIENTED_EDGE ( 'NONE', *, *, #52420, .T. ) ;
#11563 = STYLED_ITEM ( 'NONE', ( #58295 ), #46620 ) ;
#11564 = CARTESIAN_POINT ( 'NONE',  ( -117.3570736234661780, 5.598654528085804216, 7.705886871421366635 ) ) ;
#11565 = DIRECTION ( 'NONE',  ( 0.000000000000000000, 0.000000000000000000, 1.000000000000000000 ) ) ;
#11566 = CARTESIAN_POINT ( 'NONE',  ( -130.7929263765344956, -3.094860106607001171, 9.525000000008295942 ) ) ;
#11567 = ORIENTED_EDGE ( 'NONE', *, *, #61128, .F. ) ;
#11568 = CARTESIAN_POINT ( 'NONE',  ( 7.632228543268608334, 137.3429263765337964, -2.479861379858951942 ) ) ;
#11569 = DIRECTION ( 'NONE',  ( 0.000000000000000000, 1.000000000000000000, 0.000000000000000000 ) ) ;
#11570 =( NAMED_UNIT ( * ) SI_UNIT ( $, .STERADIAN. ) SOLID_ANGLE_UNIT ( ) );
#11571 =( LENGTH_UNIT ( ) NAMED_UNIT ( * ) SI_UNIT ( .MILLI., .METRE. ) );
#11572 = ORIENTED_EDGE ( 'NONE', *, *, #69568, .T. ) ;
#11573 = CIRCLE ( 'NONE', #22788, 0.2500000000000002220 ) ;
#11574 = ORIENTED_EDGE ( 'NONE', *, *, #63383, .F. ) ;
#11575 = CARTESIAN_POINT ( 'NONE',  ( -52.49292637653380211, -8.102448949553172852, 5.886773742842742685 ) ) ;
#11576 = FILL_AREA_STYLE_COLOUR ( '', #40839 ) ;
#11577 = DIRECTION ( 'NONE',  ( -0.000000000000000000, 1.000000000000000000, -0.000000000000000000 ) ) ;
#11578 = CARTESIAN_POINT ( 'NONE',  ( -138.9549999999999841, -7.632228543268599452, 2.479861379858951054 ) ) ;
#11579 = CIRCLE ( 'NONE', #36335, 0.5000000000000004441 ) ;
#11580 = CARTESIAN_POINT ( 'NONE',  ( -7.794228634059947147, -2.500000000000000000, -4.500000000000000000 ) ) ;
#11581 = CARTESIAN_POINT ( 'NONE',  ( -71.62068965517239860, 36.41396814395972115, -9.500000000000000000 ) ) ;
#11582 = UNCERTAINTY_MEASURE_WITH_UNIT (LENGTH_MEASURE( 1.000000000000000082E-05 ), #4760, 'distance_accuracy_value', 'NONE');
#11583 = ORIENTED_EDGE ( 'NONE', *, *, #7711, .F. ) ;
#11584 = AXIS2_PLACEMENT_3D ( 'NONE', #31996, #37330, #43314 ) ;
#11585 = EDGE_CURVE ( 'NONE', #2325, #53882, #63080, .T. ) ;
#11586 = DIRECTION ( 'NONE',  ( 0.000000000000000000, 1.000000000000000000, 0.000000000000000000 ) ) ;
#11588 = DIRECTION ( 'NONE',  ( 0.000000000000000000, 0.000000000000000000, 1.000000000000000000 ) ) ;
#11587 = CIRCLE ( 'NONE', #59890, 0.2500000000000002220 ) ;
#11589 = CARTESIAN_POINT ( 'NONE',  ( 41.68184459379349249, 107.4432011401419516, 3.569690802405922625 ) ) ;
#11590 = ORIENTED_EDGE ( 'NONE', *, *, #24200, .F. ) ;
#11591 = VERTEX_POINT ( 'NONE', #35321 ) ;
#11592 = SPHERICAL_SURFACE ( 'NONE', #64259, 0.2500000000000000000 ) ;
#11593 = AXIS2_PLACEMENT_3D ( 'NONE', #66231, #29655, #24357 ) ;
#11594 = EDGE_CURVE ( 'NONE', #65459, #47666, #9285, .T. ) ;
#11595 = CARTESIAN_POINT ( 'NONE',  ( -54.80499999999999261, -8.437984349512085203, 5.166775262442717831E-16 ) ) ;
#11596 = ORIENTED_EDGE ( 'NONE', *, *, #5633, .F. ) ;
#11597 = CARTESIAN_POINT ( 'NONE',  ( -74.99999999999998579, 50.00000000000000000, -12.00000000000000000 ) ) ;
#11598 = PLANE ( 'NONE',  #10210 ) ;
#11599 = EDGE_CURVE ( 'NONE', #50938, #62878, #17030, .T. ) ;
#11600 = PRESENTATION_STYLE_ASSIGNMENT (( #47923 ) ) ;
#11601 = DIRECTION ( 'NONE',  ( 0.000000000000000000, -0.000000000000000000, 1.000000000000000000 ) ) ;
#11602 = DIRECTION ( 'NONE',  ( 0.000000000000000000, 1.000000000000000000, -0.000000000000000000 ) ) ;
#11603 = CARTESIAN_POINT ( 'NONE',  ( -97.19292637653379074, -10.01517768586948698, 6.132527647946031529E-16 ) ) ;
#11604 = VERTEX_POINT ( 'NONE', #34962 ) ;
#11605 = VECTOR ( 'NONE', #44007, 1000.000000000000000 ) ;
#11606 = EDGE_CURVE ( 'NONE', #48365, #24376, #15938, .T. ) ;
#11607 = FILL_AREA_STYLE_COLOUR ( '', #40271 ) ;
#11608 = CARTESIAN_POINT ( 'NONE',  ( 12.72792206135785875, 115.4999999999999574, -10.00000000000000000 ) ) ;
#11609 = FILL_AREA_STYLE ('',( #22871 ) ) ;
#11610 = DIRECTION ( 'NONE',  ( -0.000000000000000000, -0.000000000000000000, 1.000000000000000000 ) ) ;
#11611 = DIRECTION ( 'NONE',  ( 1.000000000000000000, 0.000000000000000000, 0.000000000000000000 ) ) ;
#11612 = EDGE_CURVE ( 'NONE', #31530, #11393, #58580, .T. ) ;
#11613 = B_SPLINE_CURVE_WITH_KNOTS ( 'NONE', 3,
 ( #21299, #42469, #58255, #26898, #129, #53343 ),
 .UNSPECIFIED., .F., .F.,
 ( 4, 2, 4 ),
 ( 0.005386537104126977275, 0.008060814333094816833, 0.01073509156206265552 ),
 .UNSPECIFIED. ) ;
#11614 = CARTESIAN_POINT ( 'NONE',  ( -111.7449999999999903, 4.716976649647094177, 6.492361379858945902 ) ) ;
#11615 = CARTESIAN_POINT ( 'NONE',  ( 8.102448949553183510, 156.9949999999999761, -5.886773742842746238 ) ) ;
#11616 = CARTESIAN_POINT ( 'NONE',  ( -89.24499999999999034, -4.716976649647093289, -6.492361379858945902 ) ) ;
#11617 = CARTESIAN_POINT ( 'NONE',  ( -6.826472737025120807, 113.1070736234661496, 4.959722759717906548 ) ) ;
#11618 = CARTESIAN_POINT ( 'NONE',  ( -190.0000000000000000, 6.735557395310424274E-16, -5.499999999999984901 ) ) ;
#11619 = CIRCLE ( 'NONE', #48724, 5.000000000000004441 ) ;
#11620 = CARTESIAN_POINT ( 'NONE',  ( 0.000000000000000000, 0.000000000000000000, 0.000000000000000000 ) ) ;
#11621 = LINE ( 'NONE', #22882, #35068 ) ;
#11622 = UNCERTAINTY_MEASURE_WITH_UNIT (LENGTH_MEASURE( 1.000000000000000082E-05 ), #21426, 'distance_accuracy_value', 'NONE');
#11623 = DIRECTION ( 'NONE',  ( 1.300977106640429960E-16, 0.000000000000000000, 1.000000000000000000 ) ) ;
#11624 =( GEOMETRIC_REPRESENTATION_CONTEXT ( 3 ) GLOBAL_UNCERTAINTY_ASSIGNED_CONTEXT ( ( #67771 ) ) GLOBAL_UNIT_ASSIGNED_CONTEXT ( ( #63060, #52538, #43051 ) ) REPRESENTATION_CONTEXT ( 'NONE', 'WORKASPACE' ) );
#11625 = ORIENTED_EDGE ( 'NONE', *, *, #17291, .T. ) ;
#11626 = CARTESIAN_POINT ( 'NONE',  ( -127.1929263765338050, -10.01517768586948698, 6.132527647946031529E-16 ) ) ;
#11627 = CARTESIAN_POINT ( 'NONE',  ( -145.1949999999999648, 8.437984349512085203, -1.550032578732815448E-15 ) ) ;
#11628 = LINE ( 'NONE', #64048, #41505 ) ;
#11629 = CARTESIAN_POINT ( 'NONE',  ( -47.84499999999997044, -7.632228543268599452, 2.479861379858951054 ) ) ;
#11630 =( NAMED_UNIT ( * ) SI_UNIT ( $, .STERADIAN. ) SOLID_ANGLE_UNIT ( ) );
#11631 = ORIENTED_EDGE ( 'NONE', *, *, #59095, .T. ) ;
#11632 = ORIENTED_EDGE ( 'NONE', *, *, #2824, .T. ) ;
#11633 = COLOUR_RGB ( '', 0.31764706, 0.68627451, 0.89019608) ;
#11634 = EDGE_CURVE ( 'NONE', #1012, #65204, #18156, .T. ) ;
#11635 = FACE_OUTER_BOUND ( 'NONE', #54201, .T. ) ;
#11636 = CARTESIAN_POINT ( 'NONE',  ( -60.00000000000000000, -2.024042244987997205E-14, 10.50000000000000000 ) ) ;
#11637 = CARTESIAN_POINT ( 'NONE',  ( 0.000000000000000000, 0.000000000000000000, 0.000000000000000000 ) ) ;
#11638 = SURFACE_STYLE_USAGE ( .BOTH. , #26750 ) ;
#11639 = VECTOR ( 'NONE', #66060, 1000.000000000000000 ) ;
#11640 = CYLINDRICAL_SURFACE ( 'NONE', #30803, 0.2500000000000002220 ) ;
#11641 = EDGE_LOOP ( 'NONE', ( #19200, #46554, #38379, #45358 ) ) ;
#11642 = CARTESIAN_POINT ( 'NONE',  ( -136.7049999999999841, 2.607480562269072433, 8.024999999999991473 ) ) ;
#11643 = ORIENTED_EDGE ( 'NONE', *, *, #26932, .T. ) ;
#11644 = AXIS2_PLACEMENT_3D ( 'NONE', #51964, #41782, #57216 ) ;
#11645 = VERTEX_POINT ( 'NONE', #52554 ) ;
#11646 = DIRECTION ( 'NONE',  ( 0.000000000000000000, 1.000000000000000000, 0.000000000000000000 ) ) ;
#11647 = VERTEX_POINT ( 'NONE', #13491 ) ;
#11648 = AXIS2_PLACEMENT_3D ( 'NONE', #51369, #13372, #2423 ) ;
#11649 = CARTESIAN_POINT ( 'NONE',  ( -55.74597125125978181, -8.678695864509879954, -1.659950873073223976 ) ) ;
#11650 = CARTESIAN_POINT ( 'NONE',  ( -9.058813317711337021, 128.0449999999999875, -2.943386871421374895 ) ) ;
#11651 = COLOUR_RGB ( '', 0.08235294, 0.09019608, 0.10196078) ;
#11652 = ORIENTED_EDGE ( 'NONE', *, *, #60054, .F. ) ;
#11653 = CIRCLE ( 'NONE', #36416, 1.000000000000000888 ) ;
#11654 = CARTESIAN_POINT ( 'NONE',  ( -94.85707362346616378, -5.598654528085803328, -7.705886871421366635 ) ) ;
#11655 = CARTESIAN_POINT ( 'NONE',  ( -8.102448949553179958, 129.0049999999999670, -5.886773742842749790 ) ) ;
#11656 = CARTESIAN_POINT ( 'NONE',  ( -51.05499999999999261, -9.827790563157499189E-16, -8.024999999999991473 ) ) ;
#11657 = CARTESIAN_POINT ( 'NONE',  ( -117.8949999999999676, 6.826472737025116366, 4.959722759717898555 ) ) ;
#11658 = CARTESIAN_POINT ( 'NONE',  ( -41.12443333818656299, 107.5641524110674112, -3.336502945398625908 ) ) ;
#11659 = ORIENTED_EDGE ( 'NONE', *, *, #34541, .F. ) ;
#11660 = CARTESIAN_POINT ( 'NONE',  ( 9.058813317711338797, 160.9549999999999841, -2.943386871421372675 ) ) ;
#11661 = DIRECTION ( 'NONE',  ( 0.000000000000000000, 0.000000000000000000, -1.000000000000000000 ) ) ;
#11662 = UNCERTAINTY_MEASURE_WITH_UNIT (LENGTH_MEASURE( 1.000000000000000082E-05 ), #11321, 'distance_accuracy_value', 'NONE');
#11663 = AXIS2_PLACEMENT_3D ( 'NONE', #535, #59677, #17159 ) ;
#11664 = ADVANCED_FACE ( 'NONE', ( #18779 ), #62713, .F. ) ;
#11665 = DIRECTION ( 'NONE',  ( 0.000000000000000000, -1.000000000000000000, 0.000000000000000000 ) ) ;
#11666 = ORIENTED_EDGE ( 'NONE', *, *, #38361, .F. ) ;
#11667 = AXIS2_PLACEMENT_3D ( 'NONE', #58969, #47419, #30472 ) ;
#11668 = VECTOR ( 'NONE', #34478, 1000.000000000000000 ) ;
#11669 = DIRECTION ( 'NONE',  ( -0.000000000000000000, -0.000000000000000000, 1.000000000000000000 ) ) ;
#11670 = CARTESIAN_POINT ( 'NONE',  ( -173.7549999999999955, 4.716976649647091513, -6.492361379858946790 ) ) ;
#11671 = EDGE_LOOP ( 'NONE', ( #67707, #47417, #27615, #32754 ) ) ;
#11672 = CARTESIAN_POINT ( 'NONE',  ( -87.80707362346616662, 10.01517768586948698, -1.839758294383808966E-15 ) ) ;
#11673 = UNCERTAINTY_MEASURE_WITH_UNIT (LENGTH_MEASURE( 1.000000000000000082E-05 ), #5090, 'distance_accuracy_value', 'NONE');
#11674 = FILL_AREA_STYLE_COLOUR ( '', #15599 ) ;
#11675 = EDGE_CURVE ( 'NONE', #51271, #34471, #57104, .T. ) ;
#11676 = CARTESIAN_POINT ( 'NONE',  ( -20.71231517720798010, 147.4999999999999716, 9.500000000000000000 ) ) ;
#11677 = FILL_AREA_STYLE ('',( #1415 ) ) ;
#11678 = ORIENTED_EDGE ( 'NONE', *, *, #39501, .T. ) ;
#11679 = FACE_OUTER_BOUND ( 'NONE', #64029, .T. ) ;
#11681 = ADVANCED_FACE ( 'NONE', ( #51851 ), #3599, .T. ) ;
#11680 =( NAMED_UNIT ( * ) PLANE_ANGLE_UNIT ( ) SI_UNIT ( $, .RADIAN. ) );
#11682 = CARTESIAN_POINT ( 'NONE',  ( -84.65500000000000114, -7.632228543268600340, -2.479861379858950166 ) ) ;
#11684 = VERTEX_POINT ( 'NONE', #19822 ) ;
#11683 = AXIS2_PLACEMENT_3D ( 'NONE', #1724, #1368, #49630 ) ;
#11685 = LINE ( 'NONE', #16311, #8159 ) ;
#11686 = VECTOR ( 'NONE', #52959, 1000.000000000000000 ) ;
#11687 = SURFACE_SIDE_STYLE ('',( #59873 ) ) ;
#11688 = FACE_OUTER_BOUND ( 'NONE', #1674, .T. ) ;
#11689 = CARTESIAN_POINT ( 'NONE',  ( -66.65707362346616094, 9.058813317711329915, 2.943386871421369566 ) ) ;
#11690 =( GEOMETRIC_REPRESENTATION_CONTEXT ( 3 ) GLOBAL_UNCERTAINTY_ASSIGNED_CONTEXT ( ( #40453 ) ) GLOBAL_UNIT_ASSIGNED_CONTEXT ( ( #22319, #28246, #54667 ) ) REPRESENTATION_CONTEXT ( 'NONE', 'WORKASPACE' ) );
#11691 =( BOUNDED_CURVE ( )  B_SPLINE_CURVE ( 2, ( #9074, #68168, #68509, #10118, #25568, #62168, #30493, #47443, #4818, #63227, #40752 ),
 .UNSPECIFIED., .F., .F. ) 
 B_SPLINE_CURVE_WITH_KNOTS ( ( 3, 2, 2, 2, 2, 3 ),
 ( 0.1304347826086927065, 0.1326086956521709270, 0.1347826086956491198, 0.1369565217391273404, 0.1391304347826055610, 0.1413043478260837538 ),
 .UNSPECIFIED. ) 
 CURVE ( )  GEOMETRIC_REPRESENTATION_ITEM ( )  RATIONAL_B_SPLINE_CURVE ( ( 1.000000000000066169, 0.9510565162950872509, 1.000000000000000000, 0.9510565162951535312, 1.000000000000000000, 0.9510565162951535312, 1.000000000000000000, 0.9510565162951535312, 1.000000000000000000, 0.9510565162952253626, 0.9999999999999281686 ) ) 
 REPRESENTATION_ITEM ( '' )  );
#11692 = AXIS2_PLACEMENT_3D ( 'NONE', #26057, #60477, #43349 ) ;
#11693 = ORIENTED_EDGE ( 'NONE', *, *, #22167, .F. ) ;
#11694 = CARTESIAN_POINT ( 'NONE',  ( -18.00000000000000711, 30.74999999999999289, -3.750000000000000000 ) ) ;
#11695 = DIRECTION ( 'NONE',  ( 0.000000000000000000, 0.000000000000000000, -1.000000000000000000 ) ) ;
#11696 = EDGE_CURVE ( 'NONE', #65002, #66039, #41310, .T. ) ;
#11697 =( GEOMETRIC_REPRESENTATION_CONTEXT ( 3 ) GLOBAL_UNCERTAINTY_ASSIGNED_CONTEXT ( ( #41994 ) ) GLOBAL_UNIT_ASSIGNED_CONTEXT ( ( #51106, #23655, #57055 ) ) REPRESENTATION_CONTEXT ( 'NONE', 'WORKASPACE' ) );
#11698 = CARTESIAN_POINT ( 'NONE',  ( -105.9549999999999983, -7.632228543268599452, 2.479861379858951054 ) ) ;
#11699 = CARTESIAN_POINT ( 'NONE',  ( -8.102448949553181734, 133.8950000000000102, -5.886773742842749790 ) ) ;
#11700 = CARTESIAN_POINT ( 'NONE',  ( -113.3949999999999818, -6.826472737025115478, -4.959722759717899443 ) ) ;
#11701 = AXIS2_PLACEMENT_3D ( 'NONE', #56018, #18743, #56739 ) ;
#11702 = DIRECTION ( 'NONE',  ( 1.000000000000000000, 0.000000000000000000, 0.000000000000000000 ) ) ;
#11703 = STYLED_ITEM ( 'NONE', ( #25523 ), #26844 ) ;
#11705 = LINE ( 'NONE', #48013, #59501 ) ;
#11704 = DIRECTION ( 'NONE',  ( -0.000000000000000000, 1.000000000000000000, -0.000000000000000000 ) ) ;
#11706 = VECTOR ( 'NONE', #62008, 1000.000000000000000 ) ;
#11707 = CARTESIAN_POINT ( 'NONE',  ( -155.6929263765338192, 10.01517768586948698, -1.839758294383808571E-15 ) ) ;
#11708 = SURFACE_STYLE_FILL_AREA ( #730 ) ;
#11709 = CARTESIAN_POINT ( 'NONE',  ( -173.0949999999999989, -2.607480562269071545, -8.024999999999991473 ) ) ;
#11710 = AXIS2_PLACEMENT_3D ( 'NONE', #64111, #49024, #65144 ) ;
#11711 =( NAMED_UNIT ( * ) PLANE_ANGLE_UNIT ( ) SI_UNIT ( $, .RADIAN. ) );
#11712 = AXIS2_PLACEMENT_3D ( 'NONE', #48037, #10368, #14589 ) ;
#11713 = CARTESIAN_POINT ( 'NONE',  ( -47.54356174116917089, -13.47739874223435130, 2.712348457220836728 ) ) ;
#11714 = ORIENTED_EDGE ( 'NONE', *, *, #36207, .T. ) ;
#11715 =( LENGTH_UNIT ( ) NAMED_UNIT ( * ) SI_UNIT ( .MILLI., .METRE. ) );
#11716 = EDGE_LOOP ( 'NONE', ( #17657, #30621, #44474, #5405 ) ) ;
#11717 = CARTESIAN_POINT ( 'NONE',  ( -70.04292637653379927, -9.058813317711329915, -2.943386871421370898 ) ) ;
#11718 = EDGE_CURVE ( 'NONE', #61535, #35366, #4645, .T. ) ;
#11719 =( NAMED_UNIT ( * ) PLANE_ANGLE_UNIT ( ) SI_UNIT ( $, .RADIAN. ) );
#11720 = CARTESIAN_POINT ( 'NONE',  ( 17.00000000000000711, 25.24999999999998224, -3.750000000000000000 ) ) ;
#11721 = DIRECTION ( 'NONE',  ( 1.000000000000000000, 1.224646799147353207E-16, 0.000000000000000000 ) ) ;
#11722 = DIRECTION ( 'NONE',  ( 0.000000000000000000, 0.000000000000000000, -1.000000000000000000 ) ) ;
#11723 = CYLINDRICAL_SURFACE ( 'NONE', #58337, 9.524999999999991473 ) ;
#11724 = LINE ( 'NONE', #69181, #45439 ) ;
#11725 = ORIENTED_EDGE ( 'NONE', *, *, #65183, .T. ) ;
#11726 = CARTESIAN_POINT ( 'NONE',  ( -174.8049999999999784, -8.437984349512086979, 5.166775262442717831E-16 ) ) ;
#11727 = VECTOR ( 'NONE', #21856, 1000.000000000000000 ) ;
#11728 = ORIENTED_EDGE ( 'NONE', *, *, #17180, .T. ) ;
#11729 = LINE ( 'NONE', #60937, #24630 ) ;
#11730 = FACE_OUTER_BOUND ( 'NONE', #54729, .T. ) ;
#11731 = FACE_OUTER_BOUND ( 'NONE', #43767, .T. ) ;
#11732 = DIRECTION ( 'NONE',  ( -0.000000000000000000, -0.000000000000000000, 1.000000000000000000 ) ) ;
#11733 = CARTESIAN_POINT ( 'NONE',  ( -7.632228543268608334, 151.9570736234661581, 2.479861379858952830 ) ) ;
#11734 = PRESENTATION_LAYER_ASSIGNMENT (  '', '', ( #47763 ) ) ;
#11735 = ORIENTED_EDGE ( 'NONE', *, *, #44451, .F. ) ;
#11736 = CARTESIAN_POINT ( 'NONE',  ( -79.85499999999997556, 4.716976649647094177, 6.492361379858945902 ) ) ;
#11737 = UNCERTAINTY_MEASURE_WITH_UNIT (LENGTH_MEASURE( 1.000000000000000082E-05 ), #10034, 'distance_accuracy_value', 'NONE');
#11738 = PRESENTATION_STYLE_ASSIGNMENT (( #12413 ) ) ;
#11739 = DIRECTION ( 'NONE',  ( 0.000000000000000000, -1.000000000000000000, 0.000000000000000000 ) ) ;
#11740 = CARTESIAN_POINT ( 'NONE',  ( 25.00000000000000000, 1.000000000000000888, -3.000000000000000000 ) ) ;
#11741 = EDGE_CURVE ( 'NONE', #36619, #52251, #44019, .T. ) ;
#11742 = ORIENTED_EDGE ( 'NONE', *, *, #24126, .F. ) ;
#11743 = LINE ( 'NONE', #33548, #58681 ) ;
#11744 = PRESENTATION_STYLE_ASSIGNMENT (( #21972 ) ) ;
#11745 = CARTESIAN_POINT ( 'NONE',  ( -65.99499999999996191, -6.826472737025115478, 4.959722759717900331 ) ) ;
#11746 = ORIENTED_EDGE ( 'NONE', *, *, #59964, .T. ) ;
#11747 = FACE_OUTER_BOUND ( 'NONE', #477, .T. ) ;
#11748 = DIRECTION ( 'NONE',  ( -0.000000000000000000, 0.000000000000000000, 1.000000000000000000 ) ) ;
#11749 = CARTESIAN_POINT ( 'NONE',  ( -45.00000000000000000, 9.517485987480714726, -6.449082597785445792 ) ) ;
#11750 = ORIENTED_EDGE ( 'NONE', *, *, #69176, .T. ) ;
#11751 = DIRECTION ( 'NONE',  ( -0.000000000000000000, -1.000000000000000000, -0.000000000000000000 ) ) ;
#11752 = CYLINDRICAL_SURFACE ( 'NONE', #1052, 25.00000000000001421 ) ;
#11753 = ORIENTED_EDGE ( 'NONE', *, *, #23147, .F. ) ;
#11755 = CARTESIAN_POINT ( 'NONE',  ( 44.99999999999999289, 10.00000000017111290, -6.065867531378238198 ) ) ;
#11754 = CIRCLE ( 'NONE', #23019, 0.2500000000000002220 ) ;
#11757 = EDGE_CURVE ( 'NONE', #31954, #33911, #27503, .T. ) ;
#11756 = CARTESIAN_POINT ( 'NONE',  ( -74.45892860114929590, 7.944008872641778574, 6.500000000000004441 ) ) ;
#11758 = CARTESIAN_POINT ( 'NONE',  ( -115.8549999999999898, 4.716976649647094177, 6.492361379858945902 ) ) ;
#11759 = ORIENTED_EDGE ( 'NONE', *, *, #43657, .F. ) ;
#11760 = CARTESIAN_POINT ( 'NONE',  ( 0.7093150608672392776, 2.499999999999994227, -7.000000000000001776 ) ) ;
#11761 = CARTESIAN_POINT ( 'NONE',  ( -72.44292637653379074, -1.166476076187852838E-15, -9.524999999999991473 ) ) ;
#11762 = DIRECTION ( 'NONE',  ( -0.000000000000000000, -1.000000000000000000, -0.000000000000000000 ) ) ;
#11763 = SURFACE_STYLE_FILL_AREA ( #43816 ) ;
#11764 = PRESENTATION_LAYER_ASSIGNMENT (  '', '', ( #41021 ) ) ;
#11765 = VECTOR ( 'NONE', #28672, 1000.000000000000000 ) ;
#11766 = CARTESIAN_POINT ( 'NONE',  ( -146.9070736234661467, -3.094860106618429807, 9.524999999999991473 ) ) ;
#11767 = CIRCLE ( 'NONE', #51099, 0.2500000000000002220 ) ;
#11768 = EDGE_CURVE ( 'NONE', #30865, #23696, #42718, .T. ) ;
#11769 = CARTESIAN_POINT ( 'NONE',  ( -10.01517768586949408, 131.1949999999999363, -6.132527647946036459E-16 ) ) ;
#11770 = CARTESIAN_POINT ( 'NONE',  ( -96.80707362346618083, 10.01517768586948698, -1.839758294383808571E-15 ) ) ;
#11771 = EDGE_CURVE ( 'NONE', #59012, #36722, #61935, .T. ) ;
#11772 = LINE ( 'NONE', #38200, #66155 ) ;
#11773 = ORIENTED_EDGE ( 'NONE', *, *, #40286, .T. ) ;
#11774 = CARTESIAN_POINT ( 'NONE',  ( 7.750000000000000000, 33.99999999999998579, -3.750000000000000000 ) ) ;
#11775 = COLOUR_RGB ( '', 0.08235294, 0.09019608, 0.10196078) ;
#11777 = FACE_BOUND ( 'NONE', #38333, .T. ) ;
#11776 = CARTESIAN_POINT ( 'NONE',  ( 51.99999999999998579, 1.797044900979284448E-15, 12.00000000000000000 ) ) ;
#11778 = CARTESIAN_POINT ( 'NONE',  ( -7.632228543268607446, 130.6570736234661467, -2.479861379858953718 ) ) ;
#11779 = EDGE_CURVE ( 'NONE', #22240, #6197, #20522, .T. ) ;
#11780 = CARTESIAN_POINT ( 'NONE',  ( -128.9050000000000011, 2.607480562269068880, -8.024999999999993250 ) ) ;
#11781 = LINE ( 'NONE', #28266, #34203 ) ;
#11782 = DIRECTION ( 'NONE',  ( 0.000000000000000000, 0.000000000000000000, 1.000000000000000000 ) ) ;
#11783 = CARTESIAN_POINT ( 'NONE',  ( -149.3949999999999818, -6.826472737025115478, -4.959722759717899443 ) ) ;
#11784 = CARTESIAN_POINT ( 'NONE',  ( -133.1950000000000216, 8.437984349512086979, -1.550032578732815448E-15 ) ) ;
#11785 = ORIENTED_EDGE ( 'NONE', *, *, #17518, .T. ) ;
#11786 = CONICAL_SURFACE ( 'NONE', #26395, 5.500000000000005329, 0.7853981633974309595 ) ;
#11787 = FILL_AREA_STYLE ('',( #10758 ) ) ;
#11788 = DIRECTION ( 'NONE',  ( 0.000000000000000000, 0.000000000000000000, -1.000000000000000000 ) ) ;
#11789 = AXIS2_PLACEMENT_3D ( 'NONE', #62819, #67776, #19576 ) ;
#11790 = CARTESIAN_POINT ( 'NONE',  ( -48.35499999999998266, -4.716976649647093289, -6.492361379858945902 ) ) ;
#11791 = CARTESIAN_POINT ( 'NONE',  ( -57.29499999999998039, -2.607480562269069768, 8.024999999999991473 ) ) ;
#11792 = DIRECTION ( 'NONE',  ( 1.000000000000000000, 0.000000000000000000, 0.000000000000000000 ) ) ;
#11793 = FACE_OUTER_BOUND ( 'NONE', #14556, .T. ) ;
#11794 = DIRECTION ( 'NONE',  ( 0.6216216216216191581, 0.7833176619561879050, 0.000000000000000000 ) ) ;
#11795 = CARTESIAN_POINT ( 'NONE',  ( -91.19292637653380496, -10.01517768586948698, 6.132527647946031529E-16 ) ) ;
#11796 = PRODUCT_CONTEXT ( 'NONE', #28885, 'mechanical' ) ;
#11797 = DIRECTION ( 'NONE',  ( -1.000000000000000000, 0.000000000000000000, 0.000000000000000000 ) ) ;
#11798 = STYLED_ITEM ( 'NONE', ( #22519 ), #27374 ) ;
#11799 = CIRCLE ( 'NONE', #31983, 0.5000000000000004441 ) ;
#11800 = DIRECTION ( 'NONE',  ( 0.000000000000000000, 0.000000000000000000, 1.000000000000000000 ) ) ;
#11801 = CARTESIAN_POINT ( 'NONE',  ( 57.00000000000000000, 13.00000000000000178, -79.00402776293826435 ) ) ;
#11802 = COLOUR_RGB ( '', 0.31764706, 0.68627451, 0.89019608) ;
#11803 = DIRECTION ( 'NONE',  ( 0.000000000000000000, 0.000000000000000000, 1.000000000000000000 ) ) ;
#11804 = EDGE_LOOP ( 'NONE', ( #27389, #46415, #30759, #13612 ) ) ;
#11805 =( NAMED_UNIT ( * ) PLANE_ANGLE_UNIT ( ) SI_UNIT ( $, .RADIAN. ) );
#11806 = ORIENTED_EDGE ( 'NONE', *, *, #49656, .F. ) ;
#11807 = DIRECTION ( 'NONE',  ( 1.000000000000000000, 0.000000000000000000, 0.000000000000000000 ) ) ;
#11808 = AXIS2_PLACEMENT_3D ( 'NONE', #52375, #42523, #25593 ) ;
#11809 = CARTESIAN_POINT ( 'NONE',  ( -2.607480562269073765, 127.2070736234661723, -8.025000000000000355 ) ) ;
#11810 = CARTESIAN_POINT ( 'NONE',  ( 15.98999599679679839, 118.4999999999999716, 7.500000000000000000 ) ) ;
#11811 = DIRECTION ( 'NONE',  ( 1.000000000000000000, 0.000000000000000000, -0.000000000000000000 ) ) ;
#11812 = ORIENTED_EDGE ( 'NONE', *, *, #66553, .T. ) ;
#11813 = ORIENTED_EDGE ( 'NONE', *, *, #34019, .T. ) ;
#11814 = PRESENTATION_LAYER_ASSIGNMENT (  '', '', ( #16336 ) ) ;
#11815 = DIRECTION ( 'NONE',  ( -0.000000000000000000, 0.000000000000000000, -1.000000000000000000 ) ) ;
#11816 = ORIENTED_EDGE ( 'NONE', *, *, #18790, .T. ) ;
#11817 =( LENGTH_UNIT ( ) NAMED_UNIT ( * ) SI_UNIT ( .MILLI., .METRE. ) );
#11818 = DIRECTION ( 'NONE',  ( 0.000000000000000000, 1.000000000000000000, 0.000000000000000000 ) ) ;
#11819 = COLOUR_RGB ( '', 0.08235294, 0.09019608, 0.10196078) ;
#11820 = ADVANCED_FACE ( 'NONE', ( #68726 ), #10295, .T. ) ;
#11821 = CARTESIAN_POINT ( 'NONE',  ( 2.607480562269113733, 133.5929263765338249, 8.024999999999973710 ) ) ;
#11822 = CARTESIAN_POINT ( 'NONE',  ( -95.84499999999998465, -7.632228543268599452, 2.479861379858951054 ) ) ;
#11823 = ORIENTED_EDGE ( 'NONE', *, *, #35897, .F. ) ;
#11824 = MECHANICAL_DESIGN_GEOMETRIC_PRESENTATION_REPRESENTATION (  '', ( #63507 ), #65818 ) ;
#11825 = EDGE_CURVE ( 'NONE', #35623, #41276, #25878, .T. ) ;
#11826 = EDGE_CURVE ( 'NONE', #60007, #67106, #65195, .T. ) ;
#11827 = CARTESIAN_POINT ( 'NONE',  ( 45.00000000000000000, 9.639620389971918613, 7.000000000000000888 ) ) ;
#11828 = DIRECTION ( 'NONE',  ( 0.000000000000000000, -0.000000000000000000, 1.000000000000000000 ) ) ;
#11829 = AXIS2_PLACEMENT_3D ( 'NONE', #61011, #2574, #23056 ) ;
#11830 = VERTEX_POINT ( 'NONE', #63437 ) ;
#11831 = CARTESIAN_POINT ( 'NONE',  ( -174.4429263765337907, -1.166476076187852838E-15, -9.524999999999991473 ) ) ;
#11832 = PRESENTATION_STYLE_ASSIGNMENT (( #27979 ) ) ;
#11833 = ADVANCED_FACE ( 'NONE', ( #20876 ), #36747, .F. ) ;
#11834 = DIRECTION ( 'NONE',  ( 0.000000000000000000, 0.000000000000000000, -1.000000000000000000 ) ) ;
#11835 = ADVANCED_FACE ( 'NONE', ( #31398 ), #10342, .T. ) ;
#11836 = ORIENTED_EDGE ( 'NONE', *, *, #45924, .F. ) ;
#11837 = DIRECTION ( 'NONE',  ( 1.000000000000000000, 0.000000000000000000, -1.300977106640442040E-16 ) ) ;
#11838 = ADVANCED_FACE ( 'NONE', ( #43425 ), #13524, .T. ) ;
#11839 = EDGE_LOOP ( 'NONE', ( #20965, #44004, #28833, #54101 ) ) ;
#11840 = DIRECTION ( 'NONE',  ( 1.000000000000000000, -0.000000000000000000, -0.000000000000000000 ) ) ;
#11841 = CARTESIAN_POINT ( 'NONE',  ( -18.00000000000000711, 33.74999999999999289, -3.750000000000000000 ) ) ;
#11842 = CARTESIAN_POINT ( 'NONE',  ( 0.000000000000000000, 0.000000000000000000, 0.000000000000000000 ) ) ;
#11843 =( NAMED_UNIT ( * ) PLANE_ANGLE_UNIT ( ) SI_UNIT ( $, .RADIAN. ) );
#11844 = CARTESIAN_POINT ( 'NONE',  ( -182.4570736234661865, -9.058813317711329915, 2.943386871421371787 ) ) ;
#11845 = CARTESIAN_POINT ( 'NONE',  ( 34.99999999999992895, 110.4999999999999858, 10.00000000000000000 ) ) ;
#11846 =( REPRESENTATION_RELATIONSHIP ('NONE','NONE', #5102, #46015 ) REPRESENTATION_RELATIONSHIP_WITH_TRANSFORMATION ( #48708 )SHAPE_REPRESENTATION_RELATIONSHIP( ) );
#11847 = TOROIDAL_SURFACE ( 'NONE', #1656, 6.000000000000000000, 1.000000000000000000 ) ;
#11848 = DIRECTION ( 'NONE',  ( 0.000000000000000000, 0.000000000000000000, -1.000000000000000000 ) ) ;
#11849 = ADVANCED_FACE ( 'NONE', ( #10327 ), #27834, .T. ) ;
#11850 = CARTESIAN_POINT ( 'NONE',  ( -114.5929263765346917, -3.094860106633086083, -9.524999999989345767 ) ) ;
#11851 = VERTEX_POINT ( 'NONE', #39859 ) ;
#11852 = CARTESIAN_POINT ( 'NONE',  ( -160.9429263765338192, 0.000000000000000000, 9.524999999999991473 ) ) ;
#11853 = LINE ( 'NONE', #38984, #48970 ) ;
#11854 = FILL_AREA_STYLE_COLOUR ( '', #54808 ) ;
#11856 = FACE_OUTER_BOUND ( 'NONE', #8565, .T. ) ;
#11855 = VECTOR ( 'NONE', #62189, 1000.000000000000000 ) ;
#11857 = VERTEX_POINT ( 'NONE', #22953 ) ;
#11858 =( NAMED_UNIT ( * ) SI_UNIT ( $, .STERADIAN. ) SOLID_ANGLE_UNIT ( ) );
#11859 = CARTESIAN_POINT ( 'NONE',  ( -162.0550000000000068, -9.827790563157499189E-16, -8.024999999999991473 ) ) ;
#11860 = CARTESIAN_POINT ( 'NONE',  ( -24.00000000000000355, 36.75000000000000000, -3.000000000000000000 ) ) ;
#11861 = DIRECTION ( 'NONE',  ( 1.000000000000000000, 0.000000000000000000, 0.000000000000000000 ) ) ;
#11862 = CARTESIAN_POINT ( 'NONE',  ( -178.6450000000000102, 4.716976649647091513, -6.492361379858946790 ) ) ;
#11863 = MECHANICAL_DESIGN_GEOMETRIC_PRESENTATION_REPRESENTATION (  '', ( #29830 ), #37790 ) ;
#11864 = AXIS2_PLACEMENT_3D ( 'NONE', #13936, #57183, #56855 ) ;
#11865 = CARTESIAN_POINT ( 'NONE',  ( -162.2949999999999875, -2.607480562269069768, 8.024999999999991473 ) ) ;
#11866 = EDGE_LOOP ( 'NONE', ( #57914, #42930 ) ) ;
#11867 = SPHERICAL_SURFACE ( 'NONE', #69525, 0.5000000000000000000 ) ;
#11868 = CARTESIAN_POINT ( 'NONE',  ( 30.50000000000000711, 18.74999999999997868, 3.750000000000000000 ) ) ;
#11869 = CARTESIAN_POINT ( 'NONE',  ( 0.000000000000000000, 149.9429263765338476, -8.025000000000000355 ) ) ;
#11870 = CARTESIAN_POINT ( 'NONE',  ( -69.05499999999999261, -9.827790563157499189E-16, -8.024999999999991473 ) ) ;
#11871 = FACE_OUTER_BOUND ( 'NONE', #39442, .T. ) ;
#11872 = DIRECTION ( 'NONE',  ( 0.000000000000000000, 0.000000000000000000, -1.000000000000000000 ) ) ;
#11873 = PRESENTATION_LAYER_ASSIGNMENT (  '', '', ( #16384 ) ) ;
#11874 = CARTESIAN_POINT ( 'NONE',  ( -81.44499999999999318, 0.000000000000000000, 8.024999999999991473 ) ) ;
#11875 = CARTESIAN_POINT ( 'NONE',  ( -9.058813317711337021, 141.1549999999999727, -2.943386871421374895 ) ) ;
#11876 = CARTESIAN_POINT ( 'NONE',  ( 0.000000000000000000, -2.500000000000000000, 0.000000000000000000 ) ) ;
#11877 = CIRCLE ( 'NONE', #29851, 0.5000000000000004441 ) ;
#11878 = AXIS2_PLACEMENT_3D ( 'NONE', #55273, #66536, #28529 ) ;
#11879 = FACE_OUTER_BOUND ( 'NONE', #59064, .T. ) ;
#11880 = AXIS2_PLACEMENT_3D ( 'NONE', #15832, #4898, #69285 ) ;
#11881 =( BOUNDED_CURVE ( )  B_SPLINE_CURVE ( 2, ( #53718, #42886, #64279, #26293, #69231, #47832, #16131, #53051, #4845, #15437, #37607 ),
 .UNSPECIFIED., .F., .F. ) 
 B_SPLINE_CURVE_WITH_KNOTS ( ( 3, 2, 2, 2, 2, 3 ),
 ( 0.08695652173912847560, 0.08913043478260668229, 0.09130434782608488897, 0.09347826086956310954, 0.09565217391304131622, 0.09782608695651952291 ),
 .UNSPECIFIED. ) 
 CURVE ( )  GEOMETRIC_REPRESENTATION_ITEM ( )  RATIONAL_B_SPLINE_CURVE ( ( 1.000000000000044187, 0.9510565162951095664, 1.000000000000000000, 0.9510565162951535312, 1.000000000000000000, 0.9510565162951535312, 1.000000000000000000, 0.9510565162951535312, 1.000000000000000000, 0.9510565162952034912, 0.9999999999999500400 ) ) 
 REPRESENTATION_ITEM ( '' )  );
#11882 = EDGE_CURVE ( 'NONE', #39909, #4746, #55256, .T. ) ;
#11883 = DIRECTION ( 'NONE',  ( -1.000000000000000000, 0.000000000000000000, 0.000000000000000000 ) ) ;
#11884 = EDGE_LOOP ( 'NONE', ( #15567, #38959, #53398, #31440 ) ) ;
#11885 = MECHANICAL_DESIGN_GEOMETRIC_PRESENTATION_REPRESENTATION (  '', ( #574 ), #35500 ) ;
#11886 = DIRECTION ( 'NONE',  ( 1.000000000000000000, 0.000000000000000000, 0.000000000000000000 ) ) ;
#11887 = FACE_OUTER_BOUND ( 'NONE', #58265, .T. ) ;
#11888 = DIRECTION ( 'NONE',  ( -1.000000000000000000, 0.000000000000000000, 0.000000000000000000 ) ) ;
#11889 = CARTESIAN_POINT ( 'NONE',  ( -5.000000000000000000, 0.000000000000000000, 42.50000000000000000 ) ) ;
#11890 = DIRECTION ( 'NONE',  ( 0.000000000000000000, 1.000000000000000000, 0.000000000000000000 ) ) ;
#11891 = ORIENTED_EDGE ( 'NONE', *, *, #12796, .T. ) ;
#11892 = ORIENTED_EDGE ( 'NONE', *, *, #37850, .F. ) ;
#11893 = DIRECTION ( 'NONE',  ( 0.000000000000000000, 0.000000000000000000, -1.000000000000000000 ) ) ;
#11894 = VECTOR ( 'NONE', #32899, 1000.000000000000000 ) ;
#11895 = CARTESIAN_POINT ( 'NONE',  ( -53.18756747357285519, -10.02680648607945102, -3.500000000000002220 ) ) ;
#11896 = PRESENTATION_STYLE_ASSIGNMENT (( #27701 ) ) ;
#11897 = CARTESIAN_POINT ( 'NONE',  ( -70.55707362346616662, -1.166476076187852838E-15, -9.524999999999991473 ) ) ;
#11898 = ORIENTED_EDGE ( 'NONE', *, *, #21755, .F. ) ;
#11899 = CARTESIAN_POINT ( 'NONE',  ( -107.7549999999999955, 4.716976649647091513, -6.492361379858946790 ) ) ;
#11900 = ORIENTED_EDGE ( 'NONE', *, *, #23989, .F. ) ;
#11901 =( GEOMETRIC_REPRESENTATION_CONTEXT ( 3 ) GLOBAL_UNCERTAINTY_ASSIGNED_CONTEXT ( ( #15798 ) ) GLOBAL_UNIT_ASSIGNED_CONTEXT ( ( #28420, #23189, #38014 ) ) REPRESENTATION_CONTEXT ( 'NONE', 'WORKASPACE' ) );
#11902 = CARTESIAN_POINT ( 'NONE',  ( -45.50000000000000000, 99.99999999999992895, 10.00000000000000000 ) ) ;
#11903 = EDGE_CURVE ( 'NONE', #52357, #17965, #60440, .T. ) ;
#11904 = ORIENTED_EDGE ( 'NONE', *, *, #37705, .T. ) ;
#11905 = DIRECTION ( 'NONE',  ( -0.000000000000000000, -0.000000000000000000, -1.000000000000000000 ) ) ;
#11906 = CARTESIAN_POINT ( 'NONE',  ( 0.000000000000000000, 109.9999999999999858, -10.02500000000000568 ) ) ;
#11907 = ORIENTED_EDGE ( 'NONE', *, *, #35606, .F. ) ;
#11908 = PRESENTATION_LAYER_ASSIGNMENT (  '', '', ( #7404 ) ) ;
#11909 = AXIS2_PLACEMENT_3D ( 'NONE', #12181, #18845, #55804 ) ;
#11910 = DIRECTION ( 'NONE',  ( 9.376883653928687363E-17, 1.000000000000000000, 0.000000000000000000 ) ) ;
#11911 = CARTESIAN_POINT ( 'NONE',  ( 10.01517768586949231, 159.6949999999999648, 1.839758294383810543E-15 ) ) ;
#11912 = ORIENTED_EDGE ( 'NONE', *, *, #19932, .F. ) ;
#11913 = ADVANCED_FACE ( 'NONE', ( #59876 ), #44454, .T. ) ;
#11914 = ORIENTED_EDGE ( 'NONE', *, *, #34880, .T. ) ;
#11915 = FACE_OUTER_BOUND ( 'NONE', #47265, .T. ) ;
#11916 = FILL_AREA_STYLE_COLOUR ( '', #59731 ) ;
#11917 = CARTESIAN_POINT ( 'NONE',  ( -153.0570736234661808, 0.000000000000000000, 9.524999999999991473 ) ) ;
#11918 = CARTESIAN_POINT ( 'NONE',  ( -180.5929263765338817, -3.094860106619338413, -9.524999999999332445 ) ) ;
#11919 = ORIENTED_EDGE ( 'NONE', *, *, #26564, .T. ) ;
#11920 = CARTESIAN_POINT ( 'NONE',  ( 2.607480562269076430, 131.7929263765337851, -8.025000000000000355 ) ) ;
#11921 = CYLINDRICAL_SURFACE ( 'NONE', #35690, 8.025000000000000355 ) ;
#11922 = SURFACE_SIDE_STYLE ('',( #23181 ) ) ;
#11923 = CARTESIAN_POINT ( 'NONE',  ( 8.437984349512095861, 125.1929263765338192, 1.550032578732816828E-15 ) ) ;
#11924 = AXIS2_PLACEMENT_3D ( 'NONE', #24870, #19602, #66404 ) ;
#11925 = DIRECTION ( 'NONE',  ( 0.000000000000000000, 0.000000000000000000, -1.000000000000000000 ) ) ;
#11926 = VERTEX_POINT ( 'NONE', #39497 ) ;
#11927 = FILL_AREA_STYLE_COLOUR ( '', #67780 ) ;
#11928 = EDGE_CURVE ( 'NONE', #40021, #11113, #18373, .T. ) ;
#11929 = VERTEX_POINT ( 'NONE', #65859 ) ;
#11930 = FILL_AREA_STYLE ('',( #6624 ) ) ;
#11931 = AXIS2_PLACEMENT_3D ( 'NONE', #36386, #47283, #42015 ) ;
#11932 = FILL_AREA_STYLE_COLOUR ( '', #28902 ) ;
#11933 =( NAMED_UNIT ( * ) SI_UNIT ( $, .STERADIAN. ) SOLID_ANGLE_UNIT ( ) );
#11934 = LINE ( 'NONE', #60446, #35467 ) ;
#11935 = CARTESIAN_POINT ( 'NONE',  ( -141.2050000000000125, -2.607480562269071545, -8.024999999999991473 ) ) ;
#11936 = CARTESIAN_POINT ( 'NONE',  ( -65.00000000000000000, -2.024042244987997205E-14, 6.999999999999995559 ) ) ;
#11937 = ORIENTED_EDGE ( 'NONE', *, *, #65936, .F. ) ;
#11938 = VECTOR ( 'NONE', #27552, 1000.000000000000000 ) ;
#11939 = FACE_OUTER_BOUND ( 'NONE', #36065, .T. ) ;
#11940 = EDGE_CURVE ( 'NONE', #44352, #24951, #55647, .T. ) ;
#11941 = LINE ( 'NONE', #43994, #56341 ) ;
#11942 = ORIENTED_EDGE ( 'NONE', *, *, #68333, .F. ) ;
#11943 = ORIENTED_EDGE ( 'NONE', *, *, #9650, .F. ) ;
#11944 = CARTESIAN_POINT ( 'NONE',  ( -44.99626276708967509, 9.641083881037339154, 3.381873653971033455 ) ) ;
#11945 = FACE_OUTER_BOUND ( 'NONE', #49831, .T. ) ;
#11946 = CARTESIAN_POINT ( 'NONE',  ( -52.10499999999998266, -6.826472737025115478, 4.959722759717900331 ) ) ;
#11947 = ORIENTED_EDGE ( 'NONE', *, *, #53258, .T. ) ;
#11948 = FILL_AREA_STYLE ('',( #16569 ) ) ;
#11949 = CARTESIAN_POINT ( 'NONE',  ( 60.00000000000000000, 112.4999999999999858, -9.500000000000000000 ) ) ;
#11950 = FACE_OUTER_BOUND ( 'NONE', #24876, .T. ) ;
#11951 = CARTESIAN_POINT ( 'NONE',  ( -128.8429263765337964, 9.058813317711329915, -2.943386871421373119 ) ) ;
#11952 = ORIENTED_EDGE ( 'NONE', *, *, #20439, .T. ) ;
#11953 = CARTESIAN_POINT ( 'NONE',  ( -144.8070736234661808, 10.01517768586948698, -1.839758294383808966E-15 ) ) ;
#11954 = CARTESIAN_POINT ( 'NONE',  ( 22.75000000000000711, 34.24999999999999289, 4.000000000000000000 ) ) ;
#11955 = PRESENTATION_STYLE_ASSIGNMENT (( #42983 ) ) ;
#11956 = CYLINDRICAL_SURFACE ( 'NONE', #30270, 110.0000000000000142 ) ;
#11957 = CARTESIAN_POINT ( 'NONE',  ( -44.99999999999977973, 146.4999999999999716, 7.000000000000000000 ) ) ;
#11958 = AXIS2_PLACEMENT_3D ( 'NONE', #55082, #6539, #27988 ) ;
#11959 = CARTESIAN_POINT ( 'NONE',  ( -113.8449999999999847, -7.632228543268599452, 2.479861379858951054 ) ) ;
#11960 = CARTESIAN_POINT ( 'NONE',  ( -3.094860106618434248, 158.7949999999999875, 9.525000000000000355 ) ) ;
#11961 = MECHANICAL_DESIGN_GEOMETRIC_PRESENTATION_REPRESENTATION (  '', ( #44592 ), #14227 ) ;
#11962 = CARTESIAN_POINT ( 'NONE',  ( -74.54499999999998749, -7.632228543268600340, -2.479861379858950166 ) ) ;
#11963 = CARTESIAN_POINT ( 'NONE',  ( -21.02379604162863913, 110.4999999999999858, 9.500000000000000000 ) ) ;
#11964 = COLOUR_RGB ( '', 0.08235294, 0.09019608, 0.10196078) ;
#11965 = CARTESIAN_POINT ( 'NONE',  ( -5.885195493260865440, 2.499999999999996447, -3.806542393196803431 ) ) ;
#11966 = ADVANCED_FACE ( 'NONE', ( #33164 ), #5, .T. ) ;
#11967 = CARTESIAN_POINT ( 'NONE',  ( 29.00000000000000000, 42.00000000000000000, -80.00402776293826435 ) ) ;
#11968 = FACE_OUTER_BOUND ( 'NONE', #37854, .T. ) ;
#11969 = EDGE_LOOP ( 'NONE', ( #60760, #161, #66521, #28880 ) ) ;
#11970 = CARTESIAN_POINT ( 'NONE',  ( -124.9429263765338192, 0.000000000000000000, 9.524999999999991473 ) ) ;
#11971 = CARTESIAN_POINT ( 'NONE',  ( -152.0949999999999420, -2.607480562269071545, -8.024999999999991473 ) ) ;
#11972 =( NAMED_UNIT ( * ) PLANE_ANGLE_UNIT ( ) SI_UNIT ( $, .RADIAN. ) );
#11973 = CIRCLE ( 'NONE', #5228, 113.0000000000000142 ) ;
#11974 = LINE ( 'NONE', #33431, #37512 ) ;
#11975 = DIRECTION ( 'NONE',  ( 0.000000000000000000, 0.000000000000000000, -1.000000000000000000 ) ) ;
#11976 = VERTEX_POINT ( 'NONE', #23290 ) ;
#11977 = ORIENTED_EDGE ( 'NONE', *, *, #65674, .F. ) ;
#11978 = CARTESIAN_POINT ( 'NONE',  ( -47.48752445902327679, -11.75819929757497206, 3.312120501307041387 ) ) ;
#11979 = CARTESIAN_POINT ( 'NONE',  ( -45.50000000000000000, -2.024042244987997205E-14, -6.999999999999999112 ) ) ;
#11980 = DIRECTION ( 'NONE',  ( 0.000000000000000000, -1.000000000000000000, 0.000000000000000000 ) ) ;
#11981 = MECHANICAL_DESIGN_GEOMETRIC_PRESENTATION_REPRESENTATION (  '', ( #54660 ), #5246 ) ;
#11982 = CARTESIAN_POINT ( 'NONE',  ( -7.731910350068054619E-16, -6.500000000000000888, 21.00000000000000000 ) ) ;
#11983 = CARTESIAN_POINT ( 'NONE',  ( 8.000000000000024869, 5.000000000000000000, 32.00402776293825724 ) ) ;
#11984 = ORIENTED_EDGE ( 'NONE', *, *, #13495, .F. ) ;
#11985 = CARTESIAN_POINT ( 'NONE',  ( -141.0549999999999784, -9.827790563157499189E-16, -8.024999999999991473 ) ) ;
#11987 = ADVANCED_FACE ( 'NONE', ( #60232 ), #66186, .F. ) ;
#11986 = VERTEX_POINT ( 'NONE', #6405 ) ;
#11988 = EDGE_CURVE ( 'NONE', #67189, #3488, #19141, .T. ) ;
#11989 = EDGE_LOOP ( 'NONE', ( #52499, #5215, #59498, #34876 ) ) ;
#11990 = DIRECTION ( 'NONE',  ( -1.000000000000000000, 0.000000000000000000, 0.000000000000000000 ) ) ;
#11991 = DIRECTION ( 'NONE',  ( 0.000000000000000000, 0.000000000000000000, 1.000000000000000000 ) ) ;
#11992 = ORIENTED_EDGE ( 'NONE', *, *, #63706, .F. ) ;
#11993 = FACE_OUTER_BOUND ( 'NONE', #46474, .T. ) ;
#11994 = PRESENTATION_STYLE_ASSIGNMENT (( #50003 ) ) ;
#11995 = CARTESIAN_POINT ( 'NONE',  ( 3.094860106618431583, 135.0949999999999420, 9.525000000000000355 ) ) ;
#11996 =( NAMED_UNIT ( * ) PLANE_ANGLE_UNIT ( ) SI_UNIT ( $, .RADIAN. ) );
#11997 = EDGE_LOOP ( 'NONE', ( #57151, #9002, #66716, #66268 ) ) ;
#11998 =( LENGTH_UNIT ( ) NAMED_UNIT ( * ) SI_UNIT ( .MILLI., .METRE. ) );
#12000 = EDGE_CURVE ( 'NONE', #33368, #20590, #58855, .T. ) ;
#11999 = CARTESIAN_POINT ( 'NONE',  ( -3.094860106618432471, 134.7049999999999841, -9.525000000000000355 ) ) ;
#12001 = CARTESIAN_POINT ( 'NONE',  ( -52.25499999999999545, -4.716976649647092401, 6.492361379858946790 ) ) ;
#12002 = DIRECTION ( 'NONE',  ( 0.000000000000000000, 0.000000000000000000, 1.000000000000000000 ) ) ;
#12003 = VERTEX_POINT ( 'NONE', #24649 ) ;
#12004 = CARTESIAN_POINT ( 'NONE',  ( -9.058813317711337021, 156.1550000000000011, -2.943386871421374895 ) ) ;
#12005 = CARTESIAN_POINT ( 'NONE',  ( 16.00000000000001776, 43.00000000000000000, 29.68999999999999417 ) ) ;
#12006 = DIRECTION ( 'NONE',  ( 1.000000000000000000, 0.000000000000000000, 0.000000000000000000 ) ) ;
#12007 = EDGE_CURVE ( 'NONE', #52838, #22382, #48793, .T. ) ;
#12008 = VECTOR ( 'NONE', #50187, 1000.000000000000000 ) ;
#12009 = DIRECTION ( 'NONE',  ( 0.000000000000000000, -0.000000000000000000, -1.000000000000000000 ) ) ;
#12010 = MECHANICAL_DESIGN_GEOMETRIC_PRESENTATION_REPRESENTATION (  '', ( #9772 ), #37920 ) ;
#12011 = ORIENTED_EDGE ( 'NONE', *, *, #62267, .T. ) ;
#12012 = DIRECTION ( 'NONE',  ( -1.000000000000000000, 0.000000000000000000, -0.000000000000000000 ) ) ;
#12013 = ADVANCED_FACE ( 'NONE', ( #62309 ), #34877, .T. ) ;
#12014 = EDGE_LOOP ( 'NONE', ( #57021, #44437, #47376, #11539 ) ) ;
#12015 = DIRECTION ( 'NONE',  ( 1.000000000000000000, 0.000000000000000000, 0.000000000000000000 ) ) ;
#12016 = CARTESIAN_POINT ( 'NONE',  ( 92.41620014002536720, 0.000000000000000000, 29.00402776293826079 ) ) ;
#12017 = CARTESIAN_POINT ( 'NONE',  ( -176.1550000000000011, 7.632228543268600340, 2.479861379858949277 ) ) ;
#12018 = ORIENTED_EDGE ( 'NONE', *, *, #54012, .F. ) ;
#12019 =( NAMED_UNIT ( * ) PLANE_ANGLE_UNIT ( ) SI_UNIT ( $, .RADIAN. ) );
#12020 = PRESENTATION_STYLE_ASSIGNMENT (( #60214 ) ) ;
#12021 = CARTESIAN_POINT ( 'NONE',  ( 20.71231517720798010, 146.4999999999999716, -7.500000000000000000 ) ) ;
#12022 = EDGE_CURVE ( 'NONE', #48570, #26152, #13775, .T. ) ;
#12023 = CARTESIAN_POINT ( 'NONE',  ( 7.750000000000001776, 31.24999999999998579, -4.000000000000000000 ) ) ;
#12024 = CARTESIAN_POINT ( 'NONE',  ( -4.041451884327381450, -7.000000000000002665, 7.500000000000000000 ) ) ;
#12025 = ORIENTED_EDGE ( 'NONE', *, *, #12369, .T. ) ;
#12026 =( LENGTH_UNIT ( ) NAMED_UNIT ( * ) SI_UNIT ( .MILLI., .METRE. ) );
#12027 = DIRECTION ( 'NONE',  ( 0.000000000000000000, 1.000000000000000000, 0.000000000000000000 ) ) ;
#12028 = CARTESIAN_POINT ( 'NONE',  ( -85.10499999999997556, -6.826472737025115478, 4.959722759717900331 ) ) ;
#12029 = ORIENTED_EDGE ( 'NONE', *, *, #6056, .F. ) ;
#12030 = DIRECTION ( 'NONE',  ( 0.9604119879385738523, 0.2638002197014291950, 0.08954472351487077764 ) ) ;
#12031 = CARTESIAN_POINT ( 'NONE',  ( 4.716976649647096842, 143.8570736234661638, 6.492361379858953896 ) ) ;
#12032 = CARTESIAN_POINT ( 'NONE',  ( -55.10707362346616378, 8.102448949553171076, -5.886773742842744461 ) ) ;
#12033 = FACE_OUTER_BOUND ( 'NONE', #30570, .T. ) ;
#12034 = VERTEX_POINT ( 'NONE', #41234 ) ;
#12035 = SURFACE_STYLE_FILL_AREA ( #49692 ) ;
#12036 = CARTESIAN_POINT ( 'NONE',  ( -1.166476076187854022E-15, 128.9449999999999648, 9.525000000000000355 ) ) ;
#12037 = CARTESIAN_POINT ( 'NONE',  ( -106.1949999999999932, 8.437984349512085203, -1.550032578732815448E-15 ) ) ;
#12038 = DIRECTION ( 'NONE',  ( 0.000000000000000000, 0.000000000000000000, -1.000000000000000000 ) ) ;
#12039 = CARTESIAN_POINT ( 'NONE',  ( -15.00000000000000000, 10.90871211463577239, 5.000000000000000888 ) ) ;
#12040 = CARTESIAN_POINT ( 'NONE',  ( -148.9429263765338192, 0.000000000000000000, 9.524999999999991473 ) ) ;
#12041 = CARTESIAN_POINT ( 'NONE',  ( -180.8949999999999534, 6.826472737025116366, 4.959722759717898555 ) ) ;
#12042 = COLOUR_RGB ( '', 0.09019608, 0.27058824, 0.51372549) ;
#12043 = CIRCLE ( 'NONE', #65976, 3.100000000000003642 ) ;
#12044 = FACE_OUTER_BOUND ( 'NONE', #22476, .T. ) ;
#12045 = CARTESIAN_POINT ( 'NONE',  ( -45.98142172590127075, -12.02919239290969955, 3.220909842096380871 ) ) ;
#12046 = ORIENTED_EDGE ( 'NONE', *, *, #6761, .F. ) ;
#12047 = CYLINDRICAL_SURFACE ( 'NONE', #2037, 0.2500000000000002220 ) ;
#12048 = CARTESIAN_POINT ( 'NONE',  ( 57.00000000000000000, 0.9999999999999991118, -60.00402776293827145 ) ) ;
#12049 = EDGE_LOOP ( 'NONE', ( #42778, #68262, #36480 ) ) ;
#12050 = CARTESIAN_POINT ( 'NONE',  ( -68.39292637653380780, 8.102448949553176405, 5.886773742842740909 ) ) ;
#12051 = DIRECTION ( 'NONE',  ( 1.000000000000000000, 0.000000000000000000, 0.000000000000000000 ) ) ;
#12052 = DIRECTION ( 'NONE',  ( -1.000000000000000000, 0.000000000000000000, 0.000000000000000000 ) ) ;
#12053 = EDGE_CURVE ( 'NONE', #44244, #17222, #35935, .T. ) ;
#12054 = FACE_OUTER_BOUND ( 'NONE', #18906, .T. ) ;
#12055 = DIRECTION ( 'NONE',  ( -0.7713892158398705234, 0.000000000000000000, -0.6363636363636357984 ) ) ;
#12056 = CARTESIAN_POINT ( 'NONE',  ( 44.86929803721407239, 9.999999999999982236, -3.235899272506259639 ) ) ;
#12057 = EDGE_CURVE ( 'NONE', #42596, #53696, #44099, .T. ) ;
#12058 = CARTESIAN_POINT ( 'NONE',  ( -79.34292637653379643, -9.058813317711329915, 2.943386871421371787 ) ) ;
#12059 = AXIS2_PLACEMENT_3D ( 'NONE', #50257, #43976, #59759 ) ;
#12060 = ORIENTED_EDGE ( 'NONE', *, *, #20834, .F. ) ;
#12061 = CARTESIAN_POINT ( 'NONE',  ( -167.7549999999999955, 4.716976649647091513, -6.492361379858946790 ) ) ;
#12062 = EDGE_CURVE ( 'NONE', #38434, #34665, #32358, .T. ) ;
#12063 = ORIENTED_EDGE ( 'NONE', *, *, #37047, .F. ) ;
#12064 = EDGE_CURVE ( 'NONE', #29393, #8546, #24761, .T. ) ;
#12065 = DIRECTION ( 'NONE',  ( -0.07854820085872887825, -0.9914125719358882760, 0.1045528208578022367 ) ) ;
#12066 =( LENGTH_UNIT ( ) NAMED_UNIT ( * ) SI_UNIT ( .MILLI., .METRE. ) );
#12067 = CARTESIAN_POINT ( 'NONE',  ( -60.00000000000000000, -2.024042244987997205E-14, 11.50000000000000000 ) ) ;
#12068 =( LENGTH_UNIT ( ) NAMED_UNIT ( * ) SI_UNIT ( .MILLI., .METRE. ) );
#12069 = CARTESIAN_POINT ( 'NONE',  ( 6.826472737025119919, 153.0070736234661126, 4.959722759717908325 ) ) ;
#12070 = ORIENTED_EDGE ( 'NONE', *, *, #63915, .F. ) ;
#12071 = CARTESIAN_POINT ( 'NONE',  ( -85.10499999999997556, -6.826472737025113702, 4.959722759717902107 ) ) ;
#12072 = SURFACE_SIDE_STYLE ('',( #28223 ) ) ;
#12073 = EDGE_CURVE ( 'NONE', #39475, #59038, #63349, .T. ) ;
#12074 = CARTESIAN_POINT ( 'NONE',  ( -72.80707362346615241, 10.01517768586948698, -1.839758294383808966E-15 ) ) ;
#12075 = PRESENTATION_STYLE_ASSIGNMENT (( #48048 ) ) ;
#12076 = DIRECTION ( 'NONE',  ( -0.000000000000000000, -0.000000000000000000, 1.000000000000000000 ) ) ;
#12077 = VERTEX_POINT ( 'NONE', #15204 ) ;
#12078 = DIRECTION ( 'NONE',  ( 1.000000000000000000, 0.000000000000000000, 0.000000000000000000 ) ) ;
#12079 = CYLINDRICAL_SURFACE ( 'NONE', #39673, 5.000000000000004441 ) ;
#12080 = CARTESIAN_POINT ( 'NONE',  ( -67.19499999999999318, 8.437984349512085203, -1.550032578732815448E-15 ) ) ;
#12081 = ORIENTED_EDGE ( 'NONE', *, *, #44051, .F. ) ;
#12082 = PRESENTATION_STYLE_ASSIGNMENT (( #11047 ) ) ;
#12083 = CARTESIAN_POINT ( 'NONE',  ( -48.89292637653380780, -8.102448949553174629, -5.886773742842741797 ) ) ;
#12084 = DIRECTION ( 'NONE',  ( -0.000000000000000000, -0.6691306063588591257, 0.7431448254773933559 ) ) ;
#12085 = VECTOR ( 'NONE', #29421, 1000.000000000000000 ) ;
#12086 = ORIENTED_EDGE ( 'NONE', *, *, #4379, .T. ) ;
#12087 = CARTESIAN_POINT ( 'NONE',  ( -72.49999999999998579, 1.797044900979284448E-15, -9.500000000000000000 ) ) ;
#12088 = CARTESIAN_POINT ( 'NONE',  ( 65.00000000000000000, 1.797044900979284448E-15, -11.50000000000001066 ) ) ;
#12089 = ORIENTED_EDGE ( 'NONE', *, *, #60406, .F. ) ;
#12090 = CIRCLE ( 'NONE', #67179, 22.50000000000000000 ) ;
#12091 = CARTESIAN_POINT ( 'NONE',  ( 93.00000000000000000, 0.000000000000000000, 0.000000000000000000 ) ) ;
#12092 = CARTESIAN_POINT ( 'NONE',  ( -115.7049999999999983, 2.607480562269073321, 8.024999999999991473 ) ) ;
#12093 = ORIENTED_EDGE ( 'NONE', *, *, #17368, .F. ) ;
#12094 = EDGE_CURVE ( 'NONE', #9643, #48114, #69658, .T. ) ;
#12095 = DIRECTION ( 'NONE',  ( -0.000000000000000000, 1.000000000000000000, -0.000000000000000000 ) ) ;
#12096 = PRESENTATION_STYLE_ASSIGNMENT (( #22671 ) ) ;
#12097 = DIRECTION ( 'NONE',  ( -1.000000000000000000, 0.000000000000000000, 0.000000000000000000 ) ) ;
#12098 = DIRECTION ( 'NONE',  ( 1.000000000000000000, 0.000000000000000000, 0.000000000000000000 ) ) ;
#12099 =( NAMED_UNIT ( * ) PLANE_ANGLE_UNIT ( ) SI_UNIT ( $, .RADIAN. ) );
#12100 = CARTESIAN_POINT ( 'NONE',  ( -148.2570736234661979, 5.598654528085800663, -7.705886871421367523 ) ) ;
#12101 = EDGE_CURVE ( 'NONE', #30410, #27898, #9903, .T. ) ;
#12102 = LINE ( 'NONE', #16479, #2393 ) ;
#12103 = CARTESIAN_POINT ( 'NONE',  ( 3.094860106618431583, 129.0949999999999704, 9.525000000000000355 ) ) ;
#12104 = CARTESIAN_POINT ( 'NONE',  ( -82.55707362346618083, -1.166476076187852838E-15, -9.524999999999991473 ) ) ;
#12105 = AXIS2_PLACEMENT_3D ( 'NONE', #41535, #23678, #50423 ) ;
#12106 = CARTESIAN_POINT ( 'NONE',  ( -53.78456796010189578, -9.630272325962776492, -3.117062346851436683 ) ) ;
#12107 = VERTEX_POINT ( 'NONE', #10241 ) ;
#12108 = PRESENTATION_STYLE_ASSIGNMENT (( #2903 ) ) ;
#12109 = PRESENTATION_LAYER_ASSIGNMENT (  '', '', ( #43600 ) ) ;
#12111 = SPHERICAL_SURFACE ( 'NONE', #45978, 1.000000000000000000 ) ;
#12110 =( LENGTH_UNIT ( ) NAMED_UNIT ( * ) SI_UNIT ( .MILLI., .METRE. ) );
#12112 = FILL_AREA_STYLE ('',( #60306 ) ) ;
#12113 = AXIS2_PLACEMENT_3D ( 'NONE', #18477, #65615, #11797 ) ;
#12114 = CARTESIAN_POINT ( 'NONE',  ( -131.6049999999999898, 6.826472737025113702, -4.959722759717902107 ) ) ;
#12115 = DIRECTION ( 'NONE',  ( 0.000000000000000000, -1.000000000000000000, 0.000000000000000000 ) ) ;
#12116 = DIRECTION ( 'NONE',  ( 0.000000000000000000, -1.000000000000000000, 0.000000000000000000 ) ) ;
#12117 =( NAMED_UNIT ( * ) PLANE_ANGLE_UNIT ( ) SI_UNIT ( $, .RADIAN. ) );
#12118 = CARTESIAN_POINT ( 'NONE',  ( -149.0949999999999704, -2.607480562269071545, -8.024999999999991473 ) ) ;
#12119 = CARTESIAN_POINT ( 'NONE',  ( -128.5449999999999875, -7.632228543268600340, -2.479861379858950166 ) ) ;
#12120 = ORIENTED_EDGE ( 'NONE', *, *, #10669, .T. ) ;
#12121 = CARTESIAN_POINT ( 'NONE',  ( -195.0000000000000000, 0.000000000000000000, 0.000000000000000000 ) ) ;
#12122 = CARTESIAN_POINT ( 'NONE',  ( -74.75000000000000000, -3.000000000000000000, 7.000000000000001776 ) ) ;
#12123 = LINE ( 'NONE', #1162, #24920 ) ;
#12124 = UNCERTAINTY_MEASURE_WITH_UNIT (LENGTH_MEASURE( 1.000000000000000082E-05 ), #30999, 'distance_accuracy_value', 'NONE');
#12125 = CARTESIAN_POINT ( 'NONE',  ( -47.75499999999999545, 4.716976649647091513, -6.492361379858946790 ) ) ;
#12126 = CARTESIAN_POINT ( 'NONE',  ( -62.69499999999998607, -8.437984349512085203, 5.166775262442717831E-16 ) ) ;
#12127 = ADVANCED_FACE ( 'NONE', ( #64388 ), #21473, .F. ) ;
#12128 = DIRECTION ( 'NONE',  ( 2.312964634635740689E-15, -1.000000000000000000, 0.000000000000000000 ) ) ;
#12129 = LINE ( 'NONE', #28288, #32731 ) ;
#12130 = UNCERTAINTY_MEASURE_WITH_UNIT (LENGTH_MEASURE( 1.000000000000000082E-05 ), #39093, 'distance_accuracy_value', 'NONE');
#12131 = CARTESIAN_POINT ( 'NONE',  ( -97.49292637653380211, -8.102448949553172852, 5.886773742842742685 ) ) ;
#12132 = PRODUCT_CONTEXT ( 'NONE', #14129, 'mechanical' ) ;
#12133 = FILL_AREA_STYLE ('',( #48789 ) ) ;
#12134 = CARTESIAN_POINT ( 'NONE',  ( -81.05707362346618083, 0.000000000000000000, 9.524999999999991473 ) ) ;
#12135 = CARTESIAN_POINT ( 'NONE',  ( -41.12389261647926730, 107.5649728523252833, 3.335908204272032940 ) ) ;
#12136 = PRESENTATION_LAYER_ASSIGNMENT (  '', '', ( #54861 ) ) ;
#12137 = CIRCLE ( 'NONE', #48102, 0.5000000000000004441 ) ;
#12138 = LINE ( 'NONE', #59991, #27080 ) ;
#12139 = ADVANCED_FACE ( 'NONE', ( #64736 ), #68990, .T. ) ;
#12140 = EDGE_LOOP ( 'NONE', ( #38769, #44147, #8535 ) ) ;
#12141 = CARTESIAN_POINT ( 'NONE',  ( 0.000000000000000000, 14.00000000000000000, 80.00402776293826435 ) ) ;
#12142 = DIRECTION ( 'NONE',  ( -1.000000000000000000, 1.445602896647339656E-16, -0.000000000000000000 ) ) ;
#12143 = EDGE_LOOP ( 'NONE', ( #30857, #17974, #36155, #37342 ) ) ;
#12144 = FILL_AREA_STYLE ('',( #17126 ) ) ;
#12145 = AXIS2_PLACEMENT_3D ( 'NONE', #67695, #40993, #39609 ) ;
#12146 = CARTESIAN_POINT ( 'NONE',  ( -4.716976649647097730, 121.3570736234661638, -6.492361379858953896 ) ) ;
#12147 = CARTESIAN_POINT ( 'NONE',  ( 2.607480562269155921, 137.7070736234661297, 8.024999999999941735 ) ) ;
#12148 = CARTESIAN_POINT ( 'NONE',  ( -13.75000000000000355, 28.24999999999998934, -4.000000000000000000 ) ) ;
#12149 = ORIENTED_EDGE ( 'NONE', *, *, #33765, .F. ) ;
#12150 = CARTESIAN_POINT ( 'NONE',  ( 0.000000000000000000, 36.74999999999999289, -3.000000000000000000 ) ) ;
#12151 = EDGE_CURVE ( 'NONE', #6652, #30380, #4221, .T. ) ;
#12152 = PLANE ( 'NONE',  #47371 ) ;
#12153 = ORIENTED_EDGE ( 'NONE', *, *, #60605, .T. ) ;
#12154 = SPHERICAL_SURFACE ( 'NONE', #29951, 0.2500000000000000000 ) ;
#12155 = DIRECTION ( 'NONE',  ( 0.000000000000000000, 0.000000000000000000, 1.000000000000000000 ) ) ;
#12156 = CARTESIAN_POINT ( 'NONE',  ( -92.39499999999998181, -6.826472737025115478, -4.959722759717899443 ) ) ;
#12157 = VERTEX_POINT ( 'NONE', #69329 ) ;
#12158 = CARTESIAN_POINT ( 'NONE',  ( 45.00000000000000711, 9.639620389971920389, 6.500000000000007105 ) ) ;
#12159 = CYLINDRICAL_SURFACE ( 'NONE', #45276, 5.000000000000004441 ) ;
#12160 = VECTOR ( 'NONE', #16579, 1000.000000000000000 ) ;
#12161 = EDGE_LOOP ( 'NONE', ( #27544, #55232, #60223 ) ) ;
#12162 = CARTESIAN_POINT ( 'NONE',  ( 17.00000000000000711, 27.74999999999998224, 4.000000000000000000 ) ) ;
#12163 = VECTOR ( 'NONE', #18702, 1000.000000000000000 ) ;
#12164 = CARTESIAN_POINT ( 'NONE',  ( 12.72792206135785698, 115.4999999999999574, 10.50000000000000000 ) ) ;
#12165 = VERTEX_POINT ( 'NONE', #58766 ) ;
#12166 =( NAMED_UNIT ( * ) PLANE_ANGLE_UNIT ( ) SI_UNIT ( $, .RADIAN. ) );
#12167 = ORIENTED_EDGE ( 'NONE', *, *, #51801, .F. ) ;
#12168 = DIRECTION ( 'NONE',  ( -1.000000000000000000, 0.000000000000000000, 0.000000000000000000 ) ) ;
#12169 = CARTESIAN_POINT ( 'NONE',  ( 10.00000000000002309, 43.00000000000000000, 74.38749456993816978 ) ) ;
#12170 = DIRECTION ( 'NONE',  ( 0.000000000000000000, 0.000000000000000000, 1.000000000000000000 ) ) ;
#12171 = AXIS2_PLACEMENT_3D ( 'NONE', #66137, #11646, #60180 ) ;
#12172 = CARTESIAN_POINT ( 'NONE',  ( -178.1070736234661922, 8.102448949553171076, -5.886773742842744461 ) ) ;
#12173 = CARTESIAN_POINT ( 'NONE',  ( 3.673940397442060361E-16, 2.299999999999999822, 3.000000000000000444 ) ) ;
#12174 = AXIS2_PLACEMENT_3D ( 'NONE', #14343, #4828, #36556 ) ;
#12175 = DIRECTION ( 'NONE',  ( -0.000000000000000000, -0.000000000000000000, -1.000000000000000000 ) ) ;
#12176 = CARTESIAN_POINT ( 'NONE',  ( -84.20707362346615810, 3.094860106618433360, 9.524999999999991473 ) ) ;
#12177 = ORIENTED_EDGE ( 'NONE', *, *, #21684, .F. ) ;
#12178 =( GEOMETRIC_REPRESENTATION_CONTEXT ( 3 ) GLOBAL_UNCERTAINTY_ASSIGNED_CONTEXT ( ( #9574 ) ) GLOBAL_UNIT_ASSIGNED_CONTEXT ( ( #20454, #25379, #28985 ) ) REPRESENTATION_CONTEXT ( 'NONE', 'WORKASPACE' ) );
#12179 =( NAMED_UNIT ( * ) PLANE_ANGLE_UNIT ( ) SI_UNIT ( $, .RADIAN. ) );
#12180 = VECTOR ( 'NONE', #32518, 1000.000000000000000 ) ;
#12181 = CARTESIAN_POINT ( 'NONE',  ( 24.21231517720798010, 113.4999999999999858, -7.500000000000000000 ) ) ;
#12182 = SURFACE_SIDE_STYLE ('',( #48845 ) ) ;
#12183 =( NAMED_UNIT ( * ) PLANE_ANGLE_UNIT ( ) SI_UNIT ( $, .RADIAN. ) );
#12184 = VERTEX_POINT ( 'NONE', #47928 ) ;
#12185 = CARTESIAN_POINT ( 'NONE',  ( -155.7549999999999955, 4.716976649647091513, -6.492361379858946790 ) ) ;
#12186 = DIRECTION ( 'NONE',  ( -1.000000000000000000, 0.000000000000000000, 0.000000000000000000 ) ) ;
#12187 = CARTESIAN_POINT ( 'NONE',  ( 59.00000000000000000, 11.99999999999999822, 3.499999999999992895 ) ) ;
#12188 = CARTESIAN_POINT ( 'NONE',  ( -174.1449999999999818, -4.716976649647092401, 6.492361379858946790 ) ) ;
#12189 = CARTESIAN_POINT ( 'NONE',  ( -155.9949999999999761, -6.826472737025113702, 4.959722759717902107 ) ) ;
#12190 = ORIENTED_EDGE ( 'NONE', *, *, #23461, .F. ) ;
#12191 = DIRECTION ( 'NONE',  ( -0.000000000000000000, -0.000000000000000000, -1.000000000000000000 ) ) ;
#12192 = CARTESIAN_POINT ( 'NONE',  ( 45.61109309484437802, 10.20369769828145579, 3.650011426053806574 ) ) ;
#12193 = CARTESIAN_POINT ( 'NONE',  ( -24.00000000000000355, 36.75000000000000000, 3.000000000000000000 ) ) ;
#12194 = CARTESIAN_POINT ( 'NONE',  ( -75.50499999999998124, -6.826472737025115478, -4.959722759717899443 ) ) ;
#12195 = CARTESIAN_POINT ( 'NONE',  ( -37.66801306575244013, -11.00887909414482380, 3.663666223797411803 ) ) ;
#12196 = VECTOR ( 'NONE', #69563, 1000.000000000000000 ) ;
#12197 = CARTESIAN_POINT ( 'NONE',  ( -66.89499999999996760, 6.826472737025115478, 4.959722759717899443 ) ) ;
#12198 = CARTESIAN_POINT ( 'NONE',  ( 9.058813317711337021, 145.6549999999999727, 2.943386871421375783 ) ) ;
#12199 = EDGE_CURVE ( 'NONE', #30149, #28517, #25695, .T. ) ;
#12200 = CARTESIAN_POINT ( 'NONE',  ( 4.041451884327379673, -7.000000000000002665, 1.082903768654758903 ) ) ;
#12201 = UNCERTAINTY_MEASURE_WITH_UNIT (LENGTH_MEASURE( 1.000000000000000082E-05 ), #15648, 'distance_accuracy_value', 'NONE');
#12202 = FACE_OUTER_BOUND ( 'NONE', #39790, .T. ) ;
#12203 = ORIENTED_EDGE ( 'NONE', *, *, #37448, .T. ) ;
#12204 = VECTOR ( 'NONE', #5885, 1000.000000000000000 ) ;
#12205 = DIRECTION ( 'NONE',  ( 0.000000000000000000, 0.000000000000000000, 1.000000000000000000 ) ) ;
#12206 = EDGE_CURVE ( 'NONE', #59091, #27365, #47216, .T. ) ;
#12207 = STYLED_ITEM ( 'NONE', ( #19890 ), #42555 ) ;
#12208 = CARTESIAN_POINT ( 'NONE',  ( 20.57648123223228254, 114.4999999999999574, -10.27659574468085069 ) ) ;
#12209 = EDGE_CURVE ( 'NONE', #17689, #29817, #16234, .T. ) ;
#12210 = EDGE_CURVE ( 'NONE', #5687, #66803, #65250, .T. ) ;
#12211 = VECTOR ( 'NONE', #35498, 1000.000000000000000 ) ;
#12212 = DIRECTION ( 'NONE',  ( 0.000000000000000000, 0.000000000000000000, 1.000000000000000000 ) ) ;
#12213 = SURFACE_STYLE_USAGE ( .BOTH. , #61438 ) ;
#12214 = ORIENTED_EDGE ( 'NONE', *, *, #29984, .F. ) ;
#12215 = AXIS2_PLACEMENT_3D ( 'NONE', #3467, #39803, #61218 ) ;
#12216 = EDGE_LOOP ( 'NONE', ( #20202, #29225, #20468, #18400 ) ) ;
#12217 = FILL_AREA_STYLE ('',( #60749 ) ) ;
#12218 = EDGE_CURVE ( 'NONE', #31971, #44642, #61876, .T. ) ;
#12219 = AXIS2_PLACEMENT_3D ( 'NONE', #66339, #28337, #34670 ) ;
#12220 = EDGE_CURVE ( 'NONE', #59162, #8712, #64580, .T. ) ;
#12221 = CARTESIAN_POINT ( 'NONE',  ( 21.02379604162863913, 110.4999999999999858, -10.50000000000000000 ) ) ;
#12222 = CARTESIAN_POINT ( 'NONE',  ( 6.062177826491071286, -3.500000000000002220, 0.000000000000000000 ) ) ;
#12223 = AXIS2_PLACEMENT_3D ( 'NONE', #8163, #56326, #40536 ) ;
#12224 = VERTEX_POINT ( 'NONE', #38739 ) ;
#12225 = CARTESIAN_POINT ( 'NONE',  ( -117.0549999999999926, -9.827790563157499189E-16, -8.024999999999991473 ) ) ;
#12226 = ORIENTED_EDGE ( 'NONE', *, *, #63462, .T. ) ;
#12227 = SURFACE_SIDE_STYLE ('',( #911 ) ) ;
#12228 = CARTESIAN_POINT ( 'NONE',  ( 25.00000000000000355, 36.75000000000000000, 3.000000000000000000 ) ) ;
#12229 = VERTEX_POINT ( 'NONE', #12636 ) ;
#12230 = DIRECTION ( 'NONE',  ( 0.000000000000000000, 0.000000000000000000, 1.000000000000000000 ) ) ;
#12231 = CARTESIAN_POINT ( 'NONE',  ( 15.98999599679679839, 118.4999999999999716, -7.500000000000000000 ) ) ;
#12232 = ORIENTED_EDGE ( 'NONE', *, *, #41423, .T. ) ;
#12233 = CARTESIAN_POINT ( 'NONE',  ( -139.5570736234661808, -1.166476076187852838E-15, -9.524999999999991473 ) ) ;
#12234 = SURFACE_STYLE_USAGE ( .BOTH. , #60427 ) ;
#12235 = DIRECTION ( 'NONE',  ( -0.4999999999999997780, 0.8660254037844387076, 0.000000000000000000 ) ) ;
#12236 = ORIENTED_EDGE ( 'NONE', *, *, #57961, .T. ) ;
#12237 = MECHANICAL_DESIGN_GEOMETRIC_PRESENTATION_REPRESENTATION (  '', ( #33600 ), #61622 ) ;
#12238 = ORIENTED_EDGE ( 'NONE', *, *, #61518, .T. ) ;
#12239 = CARTESIAN_POINT ( 'NONE',  ( -8.313367756837561018, 110.4999999999999858, -4.669448307627880546 ) ) ;
#12240 = CARTESIAN_POINT ( 'NONE',  ( -151.7070736234666128, -3.094860106624918394, -9.524999999995278799 ) ) ;
#12241 = FILL_AREA_STYLE_COLOUR ( '', #30760 ) ;
#12242 = ORIENTED_EDGE ( 'NONE', *, *, #8275, .T. ) ;
#12243 = CARTESIAN_POINT ( 'NONE',  ( -2.607480562269075097, 139.2929263765338419, 8.025000000000000355 ) ) ;
#12244 = DIRECTION ( 'NONE',  ( -1.000000000000000000, -0.000000000000000000, -0.000000000000000000 ) ) ;
#12245 = CARTESIAN_POINT ( 'NONE',  ( -46.55707362346617373, -1.166476076187852838E-15, -9.524999999999991473 ) ) ;
#12246 = VECTOR ( 'NONE', #45299, 1000.000000000000000 ) ;
#12247 = LINE ( 'NONE', #38359, #57567 ) ;
#12248 = DIRECTION ( 'NONE',  ( -0.000000000000000000, -0.000000000000000000, 1.000000000000000000 ) ) ;
#12249 = ORIENTED_EDGE ( 'NONE', *, *, #26378, .F. ) ;
#12250 = DIRECTION ( 'NONE',  ( -0.000000000000000000, -0.000000000000000000, 1.000000000000000000 ) ) ;
#12251 = ORIENTED_EDGE ( 'NONE', *, *, #11606, .F. ) ;
#12252 = DIRECTION ( 'NONE',  ( 0.000000000000000000, 1.000000000000000000, 0.000000000000000000 ) ) ;
#12253 = CARTESIAN_POINT ( 'NONE',  ( -75.46551724137930250, 63.49197145334878201, 9.500000000000001776 ) ) ;
#12254 = CARTESIAN_POINT ( 'NONE',  ( -130.2549999999999955, -4.716976649647092401, 6.492361379858946790 ) ) ;
#12255 = VERTEX_POINT ( 'NONE', #11608 ) ;
#12256 = VECTOR ( 'NONE', #64820, 1000.000000000000000 ) ;
#12257 = CARTESIAN_POINT ( 'NONE',  ( 0.000000000000000000, 115.0570736234661666, -8.025000000000000355 ) ) ;
#12258 = CARTESIAN_POINT ( 'NONE',  ( 4.793647677013320951, 9.000000000000008882, 1.191052472566604292 ) ) ;
#12259 = CYLINDRICAL_SURFACE ( 'NONE', #50551, 0.2500000000000002220 ) ;
#12260 = EDGE_LOOP ( 'NONE', ( #26211, #31571, #44676, #27351, #30210 ) ) ;
#12261 = VERTEX_POINT ( 'NONE', #60470 ) ;
#12262 = DIRECTION ( 'NONE',  ( 0.000000000000000000, 0.000000000000000000, 1.000000000000000000 ) ) ;
#12263 = CARTESIAN_POINT ( 'NONE',  ( -55.85499999999998977, 4.716976649647094177, 6.492361379858945902 ) ) ;
#12264 = ORIENTED_EDGE ( 'NONE', *, *, #20898, .F. ) ;
#12265 =( LENGTH_UNIT ( ) NAMED_UNIT ( * ) SI_UNIT ( .MILLI., .METRE. ) );
#12266 =( NAMED_UNIT ( * ) PLANE_ANGLE_UNIT ( ) SI_UNIT ( $, .RADIAN. ) );
#12267 = FILL_AREA_STYLE ('',( #61492 ) ) ;
#12268 = VECTOR ( 'NONE', #52978, 1000.000000000000000 ) ;
#12269 = FACE_OUTER_BOUND ( 'NONE', #38475, .T. ) ;
#12270 = AXIS2_PLACEMENT_3D ( 'NONE', #63796, #11373, #53272 ) ;
#12271 = DIRECTION ( 'NONE',  ( 0.000000000000000000, 0.000000000000000000, -1.000000000000000000 ) ) ;
#12272 = AXIS2_PLACEMENT_3D ( 'NONE', #28248, #60623, #65573 ) ;
#12273 = ORIENTED_EDGE ( 'NONE', *, *, #20310, .F. ) ;
#12274 = SHAPE_REPRESENTATION ( '16. Bolt M6x25', ( #42840 ), #43934 ) ;
#12275 = MECHANICAL_DESIGN_GEOMETRIC_PRESENTATION_REPRESENTATION (  '', ( #29142 ), #32513 ) ;
#12276 = DIRECTION ( 'NONE',  ( 0.000000000000000000, 3.118022522272251586E-15, -1.000000000000000000 ) ) ;
#12277 = DIRECTION ( 'NONE',  ( 1.000000000000000000, 0.000000000000000000, 0.000000000000000000 ) ) ;
#12278 = SURFACE_STYLE_FILL_AREA ( #59426 ) ;
#12279 = CARTESIAN_POINT ( 'NONE',  ( -26.79538245034556709, -8.499999999999998224, 0.000000000000000000 ) ) ;
#12280 = SURFACE_STYLE_USAGE ( .BOTH. , #34448 ) ;
#12281 = DIRECTION ( 'NONE',  ( 0.000000000000000000, 1.000000000000000000, 0.000000000000000000 ) ) ;
#12282 = CARTESIAN_POINT ( 'NONE',  ( -95.99499999999997613, -6.826472737025113702, 4.959722759717902107 ) ) ;
#12283 = CARTESIAN_POINT ( 'NONE',  ( -9.058813317711337021, 111.1549999999999869, -2.943386871421374895 ) ) ;
#12284 = CARTESIAN_POINT ( 'NONE',  ( -78.89499999999999602, 6.826472737025116366, 4.959722759717898555 ) ) ;
#12285 = CARTESIAN_POINT ( 'NONE',  ( 28.00000000000002842, 38.70020753820971748, 90.00000000000000000 ) ) ;
#12286 = EDGE_CURVE ( 'NONE', #6589, #6975, #22870, .T. ) ;
#12287 = LINE ( 'NONE', #49268, #54129 ) ;
#12288 = SURFACE_STYLE_FILL_AREA ( #28460 ) ;
#12289 = LINE ( 'NONE', #28823, #5826 ) ;
#12290 = UNCERTAINTY_MEASURE_WITH_UNIT (LENGTH_MEASURE( 1.000000000000000082E-05 ), #56295, 'distance_accuracy_value', 'NONE');
#12291 = ADVANCED_FACE ( 'NONE', ( #65058 ), #30426, .T. ) ;
#12292 =( LENGTH_UNIT ( ) NAMED_UNIT ( * ) SI_UNIT ( .MILLI., .METRE. ) );
#12293 = CARTESIAN_POINT ( 'NONE',  ( -24.21231517720798010, 112.9999999999999858, 7.000000000000000000 ) ) ;
#12294 = ORIENTED_EDGE ( 'NONE', *, *, #12064, .T. ) ;
#12295 = CARTESIAN_POINT ( 'NONE',  ( -121.3429263765338106, -9.058813317711329915, 2.943386871421371787 ) ) ;
#12296 = CARTESIAN_POINT ( 'NONE',  ( -142.1949999999999932, 8.437984349512085203, -1.550032578732815448E-15 ) ) ;
#12297 = VECTOR ( 'NONE', #12116, 1000.000000000000000 ) ;
#12298 = EDGE_CURVE ( 'NONE', #51304, #60615, #44016, .T. ) ;
#12299 = CARTESIAN_POINT ( 'NONE',  ( -173.2429263765338305, 5.598654528085804216, 7.705886871421366635 ) ) ;
#12300 = VERTEX_POINT ( 'NONE', #18277 ) ;
#12301 = VERTEX_POINT ( 'NONE', #11954 ) ;
#12302 = CIRCLE ( 'NONE', #60604, 1.000000000000000888 ) ;
#12303 = COLOUR_RGB ( '', 0.08235294, 0.09019608, 0.10196078) ;
#12304 = FACE_OUTER_BOUND ( 'NONE', #58519, .T. ) ;
#12305 = AXIS2_PLACEMENT_3D ( 'NONE', #19399, #14842, #25028 ) ;
#12306 = EDGE_CURVE ( 'NONE', #66039, #49491, #49959, .T. ) ;
#12307 = CARTESIAN_POINT ( 'NONE',  ( -98.90707362346724096, -3.094860106601085459, 9.525000000012594725 ) ) ;
#12308 =( LENGTH_UNIT ( ) NAMED_UNIT ( * ) SI_UNIT ( .MILLI., .METRE. ) );
#12309 = CARTESIAN_POINT ( 'NONE',  ( 10.00000000000000533, 43.00000000000000000, -45.61250543006183733 ) ) ;
#12310 = ORIENTED_EDGE ( 'NONE', *, *, #26432, .T. ) ;
#12311 = CARTESIAN_POINT ( 'NONE',  ( -139.5549999999999784, 0.000000000000000000, 8.024999999999991473 ) ) ;
#12312 = EDGE_LOOP ( 'NONE', ( #62149, #21004 ) ) ;
#12313 = ORIENTED_EDGE ( 'NONE', *, *, #13321, .F. ) ;
#12314 = DIRECTION ( 'NONE',  ( 1.000000000000000000, 0.000000000000000000, 0.000000000000000000 ) ) ;
#12315 = FACE_OUTER_BOUND ( 'NONE', #27209, .T. ) ;
#12316 = VERTEX_POINT ( 'NONE', #55559 ) ;
#12317 = CIRCLE ( 'NONE', #51665, 1.000000000000000000 ) ;
#12318 = CARTESIAN_POINT ( 'NONE',  ( -55.36563020516651790, -8.495980172839733058, -2.204722216948698854 ) ) ;
#12319 = CIRCLE ( 'NONE', #69632, 9.525000000000000355 ) ;
#12320 = CARTESIAN_POINT ( 'NONE',  ( 5.598654528085809545, 130.1449999999999818, -7.705886871421373741 ) ) ;
#12321 = FILL_AREA_STYLE_COLOUR ( '', #36282 ) ;
#12322 = ORIENTED_EDGE ( 'NONE', *, *, #31912, .F. ) ;
#12323 =( NAMED_UNIT ( * ) PLANE_ANGLE_UNIT ( ) SI_UNIT ( $, .RADIAN. ) );
#12324 = CARTESIAN_POINT ( 'NONE',  ( 5.598654528085805993, 130.3549999999999898, 7.705886871421374629 ) ) ;
#12325 = CARTESIAN_POINT ( 'NONE',  ( -58.85499999999998977, 4.716976649647094177, 6.492361379858945902 ) ) ;
#12326 = CIRCLE ( 'NONE', #35960, 3.499999999999999556 ) ;
#12327 = VERTEX_POINT ( 'NONE', #23537 ) ;
#12328 = CARTESIAN_POINT ( 'NONE',  ( -3.094860106618434248, 159.9050000000000011, 9.525000000000000355 ) ) ;
#12329 = CARTESIAN_POINT ( 'NONE',  ( 34.99999999999992895, 109.9999999999999858, 9.500000000000000000 ) ) ;
#12330 = UNCERTAINTY_MEASURE_WITH_UNIT (LENGTH_MEASURE( 1.000000000000000082E-05 ), #27814, 'distance_accuracy_value', 'NONE');
#12331 = AXIS2_PLACEMENT_3D ( 'NONE', #60069, #54440, #11886 ) ;
#12332 = EDGE_CURVE ( 'NONE', #38874, #11216, #51813, .T. ) ;
#12333 = DIRECTION ( 'NONE',  ( -1.000000000000000000, -0.000000000000000000, -0.000000000000000000 ) ) ;
#12334 = SURFACE_STYLE_USAGE ( .BOTH. , #356 ) ;
#12335 = DIRECTION ( 'NONE',  ( -1.224646799147353207E-16, 1.000000000000000000, 0.000000000000000000 ) ) ;
#12336 = EDGE_LOOP ( 'NONE', ( #29496, #27081, #38362, #7674 ) ) ;
#12337 = PRESENTATION_STYLE_ASSIGNMENT (( #60524 ) ) ;
#12338 = EDGE_LOOP ( 'NONE', ( #29419, #59590, #11126, #32841 ) ) ;
#12339 = MECHANICAL_DESIGN_GEOMETRIC_PRESENTATION_REPRESENTATION (  '', ( #33688 ), #51685 ) ;
#12340 = CARTESIAN_POINT ( 'NONE',  ( -32.80478667408987548, -9.106085870130632642, -2.687031549326329039 ) ) ;
#12341 = CARTESIAN_POINT ( 'NONE',  ( -24.00000000000000000, -2.250452076942884869E-15, 3.000000000000000000 ) ) ;
#12342 = CARTESIAN_POINT ( 'NONE',  ( -160.1049999999999613, -6.826472737025115478, 4.959722759717900331 ) ) ;
#12343 = EDGE_LOOP ( 'NONE', ( #35332, #39013, #24784, #16592 ) ) ;
#12344 = DIRECTION ( 'NONE',  ( 0.000000000000000000, 0.000000000000000000, -1.000000000000000000 ) ) ;
#12345 = UNCERTAINTY_MEASURE_WITH_UNIT (LENGTH_MEASURE( 1.000000000000000082E-05 ), #30522, 'distance_accuracy_value', 'NONE');
#12346 = STYLED_ITEM ( 'NONE', ( #15544 ), #16264 ) ;
#12347 = EDGE_CURVE ( 'NONE', #29858, #43604, #10770, .T. ) ;
#12348 = DIRECTION ( 'NONE',  ( -1.000000000000000000, -0.000000000000000000, -0.000000000000000000 ) ) ;
#12349 = DIRECTION ( 'NONE',  ( -0.000000000000000000, -0.000000000000000000, 1.000000000000000000 ) ) ;
#12350 = DIRECTION ( 'NONE',  ( 1.000000000000000000, 0.000000000000000000, -0.000000000000000000 ) ) ;
#12351 = ORIENTED_EDGE ( 'NONE', *, *, #11940, .F. ) ;
#12352 = COLOUR_RGB ( '', 0.40784314, 0.44705882, 0.49803922) ;
#12353 = ORIENTED_EDGE ( 'NONE', *, *, #66305, .F. ) ;
#12354 = CARTESIAN_POINT ( 'NONE',  ( -184.0000000000000000, 0.000000000000000000, 8.024999999999991473 ) ) ;
#12355 = CARTESIAN_POINT ( 'NONE',  ( -111.0570736234661808, 0.000000000000000000, 9.524999999999991473 ) ) ;
#12356 = CARTESIAN_POINT ( 'NONE',  ( -81.05499999999999261, -9.827790563157499189E-16, -8.024999999999991473 ) ) ;
#12357 = VERTEX_POINT ( 'NONE', #61179 ) ;
#12358 = LINE ( 'NONE', #55283, #41940 ) ;
#12359 = AXIS2_PLACEMENT_3D ( 'NONE', #66801, #17594, #40091 ) ;
#12360 = DIRECTION ( 'NONE',  ( -1.000000000000000000, 0.000000000000000000, 0.000000000000000000 ) ) ;
#12361 = DIRECTION ( 'NONE',  ( 1.000000000000000000, 0.000000000000000000, 0.000000000000000000 ) ) ;
#12362 = AXIS2_PLACEMENT_3D ( 'NONE', #2380, #22527, #55571 ) ;
#12363 = DIRECTION ( 'NONE',  ( -1.000000000000000000, 0.000000000000000000, 0.000000000000000000 ) ) ;
#12364 = ORIENTED_EDGE ( 'NONE', *, *, #7932, .T. ) ;
#12365 = SURFACE_STYLE_USAGE ( .BOTH. , #50372 ) ;
#12367 = DIRECTION ( 'NONE',  ( -0.000000000000000000, 0.000000000000000000, -1.000000000000000000 ) ) ;
#12366 = LINE ( 'NONE', #60908, #62747 ) ;
#12368 = EDGE_CURVE ( 'NONE', #68401, #59464, #56598, .T. ) ;
#12369 = EDGE_CURVE ( 'NONE', #13981, #47647, #45401, .T. ) ;
#12370 = CARTESIAN_POINT ( 'NONE',  ( 9.058813317711338797, 126.8449999999999847, -2.943386871421372675 ) ) ;
#12371 = CARTESIAN_POINT ( 'NONE',  ( -111.5949999999999704, 2.607480562269073321, 8.024999999999991473 ) ) ;
#12372 = CIRCLE ( 'NONE', #4482, 0.2500000000000002220 ) ;
#12373 =( GEOMETRIC_REPRESENTATION_CONTEXT ( 3 ) GLOBAL_UNCERTAINTY_ASSIGNED_CONTEXT ( ( #1762 ) ) GLOBAL_UNIT_ASSIGNED_CONTEXT ( ( #2360, #35827, #66446 ) ) REPRESENTATION_CONTEXT ( 'NONE', 'WORKASPACE' ) );
#12374 = CARTESIAN_POINT ( 'NONE',  ( 53.24999999999999289, 27.74999999999998579, 3.750000000000000000 ) ) ;
#12375 = VECTOR ( 'NONE', #47158, 1000.000000000000000 ) ;
#12376 = CARTESIAN_POINT ( 'NONE',  ( -20.71231517720798010, 149.9999999999999716, 9.500000000000000000 ) ) ;
#12377 = EDGE_CURVE ( 'NONE', #10966, #68484, #29146, .T. ) ;
#12378 = CARTESIAN_POINT ( 'NONE',  ( -157.1929263765337907, -10.01517768586948698, 6.132527647946031529E-16 ) ) ;
#12379 = CARTESIAN_POINT ( 'NONE',  ( -163.0449999999999875, 7.632228543268600340, 2.479861379858949277 ) ) ;
#12380 = CIRCLE ( 'NONE', #37151, 8.000000000000007105 ) ;
#12381 = CARTESIAN_POINT ( 'NONE',  ( -70.75000000000000000, -0.9999999999999995559, 24.00000000000000000 ) ) ;
#12382 = EDGE_CURVE ( 'NONE', #17887, #40838, #3071, .T. ) ;
#12383 = AXIS2_PLACEMENT_3D ( 'NONE', #37967, #11521, #28725 ) ;
#12384 = CARTESIAN_POINT ( 'NONE',  ( -40.79052781025667684, -13.69784301587829667, 2.689112900518555005 ) ) ;
#12385 = VERTEX_POINT ( 'NONE', #14040 ) ;
#12386 = CARTESIAN_POINT ( 'NONE',  ( 0.000000000000000000, 0.000000000000000000, 0.2500000000000011102 ) ) ;
#12387 = VERTEX_POINT ( 'NONE', #40110 ) ;
#12388 = CARTESIAN_POINT ( 'NONE',  ( -63.89292637653380780, -8.102448949553172852, -5.886773742842741797 ) ) ;
#12389 = CARTESIAN_POINT ( 'NONE',  ( -45.75849432247279935, 8.825695369645321975, 6.400617768950438879 ) ) ;
#12390 = DIRECTION ( 'NONE',  ( 0.000000000000000000, 0.000000000000000000, -1.000000000000000000 ) ) ;
#12391 = AXIS2_PLACEMENT_3D ( 'NONE', #16758, #11095, #31860 ) ;
#12392 = EDGE_CURVE ( 'NONE', #54537, #5489, #30534, .T. ) ;
#12393 = DIRECTION ( 'NONE',  ( 1.000000000000000000, 0.000000000000000000, 0.000000000000000000 ) ) ;
#12394 = SURFACE_STYLE_FILL_AREA ( #61287 ) ;
#12395 = CARTESIAN_POINT ( 'NONE',  ( 44.48123910951614590, 9.999999999999978684, -3.378119344631853149 ) ) ;
#12396 = PRESENTATION_LAYER_ASSIGNMENT (  '', '', ( #15805 ) ) ;
#12397 = DIRECTION ( 'NONE',  ( 0.000000000000000000, 0.000000000000000000, -1.000000000000000000 ) ) ;
#12398 = EDGE_LOOP ( 'NONE', ( #29461, #6969, #12696, #43690 ) ) ;
#12399 = CARTESIAN_POINT ( 'NONE',  ( -168.6550000000000011, -7.632228543268600340, -2.479861379858950166 ) ) ;
#12400 = ORIENTED_EDGE ( 'NONE', *, *, #4998, .T. ) ;
#12401 = CARTESIAN_POINT ( 'NONE',  ( -111.4429263765338050, -1.166476076187852838E-15, -9.524999999999991473 ) ) ;
#12402 = DIRECTION ( 'NONE',  ( 0.000000000000000000, 1.000000000000000000, -0.000000000000000000 ) ) ;
#12403 =( NAMED_UNIT ( * ) PLANE_ANGLE_UNIT ( ) SI_UNIT ( $, .RADIAN. ) );
#12404 = VECTOR ( 'NONE', #5865, 1000.000000000000000 ) ;
#12405 = FACE_BOUND ( 'NONE', #55139, .T. ) ;
#12406 = CARTESIAN_POINT ( 'NONE',  ( -7.632228543268607446, 148.6570736234661751, -2.479861379858953718 ) ) ;
#12407 = ORIENTED_EDGE ( 'NONE', *, *, #63722, .T. ) ;
#12408 = AXIS2_PLACEMENT_3D ( 'NONE', #8161, #14457, #68286 ) ;
#12409 = CARTESIAN_POINT ( 'NONE',  ( -85.40499999999998693, -2.607480562269069768, 8.024999999999991473 ) ) ;
#12410 = CARTESIAN_POINT ( 'NONE',  ( -4.716976649647098618, 122.2570736234661553, 6.492361379858953008 ) ) ;
#12411 = CARTESIAN_POINT ( 'NONE',  ( 9.058813317711337021, 130.6550000000000011, 2.943386871421375783 ) ) ;
#12412 = UNCERTAINTY_MEASURE_WITH_UNIT (LENGTH_MEASURE( 1.000000000000000082E-05 ), #24972, 'distance_accuracy_value', 'NONE');
#12413 = SURFACE_STYLE_USAGE ( .BOTH. , #50770 ) ;
#12414 = FACE_OUTER_BOUND ( 'NONE', #47618, .T. ) ;
#12415 = CARTESIAN_POINT ( 'NONE',  ( -169.7929263765340124, -3.094860106615421547, 9.525000000002178169 ) ) ;
#12416 = CARTESIAN_POINT ( 'NONE',  ( 4.000000000000030198, 38.00000000000000711, 90.00000000000000000 ) ) ;
#12417 = COLOUR_RGB ( '', 0.66274510, 0.83137255, 0.94901961) ;
#12418 =( NAMED_UNIT ( * ) SI_UNIT ( $, .STERADIAN. ) SOLID_ANGLE_UNIT ( ) );
#12419 = ORIENTED_EDGE ( 'NONE', *, *, #24684, .T. ) ;
#12420 = CARTESIAN_POINT ( 'NONE',  ( -66.89499999999996760, 6.826472737025116366, 4.959722759717898555 ) ) ;
#12421 = VERTEX_POINT ( 'NONE', #61498 ) ;
#12422 = CARTESIAN_POINT ( 'NONE',  ( 0.000000000000000000, -2.500000000000000000, 0.000000000000000000 ) ) ;
#12423 = ADVANCED_FACE ( 'NONE', ( #13684 ), #56256, .F. ) ;
#12424 = VECTOR ( 'NONE', #30826, 1000.000000000000000 ) ;
#12425 = DIRECTION ( 'NONE',  ( 0.000000000000000000, 0.000000000000000000, 1.000000000000000000 ) ) ;
#12426 = CARTESIAN_POINT ( 'NONE',  ( -44.99999999999998579, 8.254931070086806599, -5.606557580296886556 ) ) ;
#12427 = ORIENTED_EDGE ( 'NONE', *, *, #43018, .F. ) ;
#12428 = CARTESIAN_POINT ( 'NONE',  ( -51.25481733270894580, -11.82219366972335095, 1.525841347188607422 ) ) ;
#12429 = CARTESIAN_POINT ( 'NONE',  ( -54.29499999999998039, -2.607480562269069768, 8.024999999999991473 ) ) ;
#12430 = FACE_OUTER_BOUND ( 'NONE', #30703, .T. ) ;
#12431 = STYLED_ITEM ( 'NONE', ( #21583 ), #52368 ) ;
#12432 = ORIENTED_EDGE ( 'NONE', *, *, #31834, .F. ) ;
#12433 = CARTESIAN_POINT ( 'NONE',  ( -74.11226636805670864, 9.324829141677559718, 6.185705318536756536 ) ) ;
#12434 = CARTESIAN_POINT ( 'NONE',  ( -111.5049999999999955, -6.826472737025115478, -4.959722759717899443 ) ) ;
#12435 = ORIENTED_EDGE ( 'NONE', *, *, #10722, .F. ) ;
#12436 = CARTESIAN_POINT ( 'NONE',  ( -6.826472737025120807, 119.1070736234661496, 4.959722759717906548 ) ) ;
#12437 = DIRECTION ( 'NONE',  ( 1.000000000000000000, 0.000000000000000000, 0.000000000000000000 ) ) ;
#12438 =( LENGTH_UNIT ( ) NAMED_UNIT ( * ) SI_UNIT ( .MILLI., .METRE. ) );
#12439 = PLANE ( 'NONE',  #61129 ) ;
#12440 = PRESENTATION_STYLE_ASSIGNMENT (( #62299 ) ) ;
#12441 = CARTESIAN_POINT ( 'NONE',  ( -149.0070736234661979, -8.102448949553172852, -5.886773742842741797 ) ) ;
#12442 = DIRECTION ( 'NONE',  ( 1.000000000000000000, 0.000000000000000000, 0.000000000000000000 ) ) ;
#12443 = CIRCLE ( 'NONE', #31524, 23.00000000000000000 ) ;
#12444 = CARTESIAN_POINT ( 'NONE',  ( 9.058813317711337021, 132.5449999999999875, 2.943386871421375783 ) ) ;
#12445 = CARTESIAN_POINT ( 'NONE',  ( -84.65707362346616094, 9.058813317711329915, 2.943386871421369566 ) ) ;
#12446 = DIRECTION ( 'NONE',  ( -0.000000000000000000, 0.000000000000000000, -1.000000000000000000 ) ) ;
#12447 = EDGE_CURVE ( 'NONE', #46073, #41197, #39764, .T. ) ;
#12448 = FACE_OUTER_BOUND ( 'NONE', #2180, .T. ) ;
#12449 = ORIENTED_EDGE ( 'NONE', *, *, #51084, .F. ) ;
#12450 = CYLINDRICAL_SURFACE ( 'NONE', #27278, 1.000000000000000888 ) ;
#12451 = FILL_AREA_STYLE ('',( #23037 ) ) ;
#12452 = ADVANCED_FACE ( 'NONE', ( #50632 ), #12990, .F. ) ;
#12453 = CARTESIAN_POINT ( 'NONE',  ( -130.2549999999999955, -4.716976649647092401, 6.492361379858946790 ) ) ;
#12454 = EDGE_CURVE ( 'NONE', #27631, #10139, #59025, .T. ) ;
#12455 = PLANE ( 'NONE',  #26837 ) ;
#12456 = CARTESIAN_POINT ( 'NONE',  ( -55.34292637653378932, -9.058813317711329915, 2.943386871421371787 ) ) ;
#12457 = CARTESIAN_POINT ( 'NONE',  ( -138.4449999999999932, 0.000000000000000000, 8.024999999999991473 ) ) ;
#12458 = CARTESIAN_POINT ( 'NONE',  ( -131.6949999999999648, -8.437984349512086979, 5.166775262442717831E-16 ) ) ;
#12459 = DIRECTION ( 'NONE',  ( -0.000000000000000000, -0.000000000000000000, 1.000000000000000000 ) ) ;
#12460 = ORIENTED_EDGE ( 'NONE', *, *, #45772, .T. ) ;
#12461 = CARTESIAN_POINT ( 'NONE',  ( -146.9070736234666015, -3.094860106611035722, 9.525000000005366729 ) ) ;
#12462 = PRESENTATION_STYLE_ASSIGNMENT (( #27243 ) ) ;
#12463 = VECTOR ( 'NONE', #7747, 1000.000000000000000 ) ;
#12464 = EDGE_CURVE ( 'NONE', #11299, #37145, #63692, .T. ) ;
#12466 = VECTOR ( 'NONE', #28809, 1000.000000000000000 ) ;
#12465 = FACE_OUTER_BOUND ( 'NONE', #17211, .T. ) ;
#12467 = CARTESIAN_POINT ( 'NONE',  ( -48.95499999999996987, -7.632228543268599452, 2.479861379858951054 ) ) ;
#12468 = CARTESIAN_POINT ( 'NONE',  ( -47.84499999999997044, -7.632228543268599452, 2.479861379858951054 ) ) ;
#12469 = EDGE_CURVE ( 'NONE', #34584, #58716, #707, .T. ) ;
#12470 = AXIS2_PLACEMENT_3D ( 'NONE', #39004, #6254, #60065 ) ;
#12471 = CARTESIAN_POINT ( 'NONE',  ( 31.00000000000002132, 43.00000000000000000, 79.00402776293826435 ) ) ;
#12472 = CARTESIAN_POINT ( 'NONE',  ( 51.99999999999998579, 1.797044900979284448E-15, -10.49999999999999822 ) ) ;
#12473 =( NAMED_UNIT ( * ) SI_UNIT ( $, .STERADIAN. ) SOLID_ANGLE_UNIT ( ) );
#12474 =( NAMED_UNIT ( * ) PLANE_ANGLE_UNIT ( ) SI_UNIT ( $, .RADIAN. ) );
#12475 = PRESENTATION_LAYER_ASSIGNMENT (  '', '', ( #61943 ) ) ;
#12476 = CARTESIAN_POINT ( 'NONE',  ( -98.69292637653380496, 10.01517768586948698, -1.839758294383808571E-15 ) ) ;
#12477 = PRODUCT_CONTEXT ( 'NONE', #47872, 'mechanical' ) ;
#12478 = CARTESIAN_POINT ( 'NONE',  ( -48.29019130588075370, -13.25700720320236847, 0.9673485149590689280 ) ) ;
#12479 = DIRECTION ( 'NONE',  ( 0.000000000000000000, 1.000000000000000000, 0.000000000000000000 ) ) ;
#12480 = TOROIDAL_SURFACE ( 'NONE', #19246, 8.500000000000012434, 0.5000000000000000000 ) ;
#12481 = DIRECTION ( 'NONE',  ( 0.000000000000000000, -1.000000000000000000, 0.000000000000000000 ) ) ;
#12482 = FILL_AREA_STYLE_COLOUR ( '', #38239 ) ;
#12483 = PRESENTATION_STYLE_ASSIGNMENT (( #2212 ) ) ;
#12484 = CARTESIAN_POINT ( 'NONE',  ( 60.00000000000000000, 1.797044900979284448E-15, 10.50000000000000000 ) ) ;
#12485 = EDGE_CURVE ( 'NONE', #35021, #31124, #1163, .T. ) ;
#12486 = ORIENTED_EDGE ( 'NONE', *, *, #61868, .F. ) ;
#12487 = AXIS2_PLACEMENT_3D ( 'NONE', #23425, #7599, #7950 ) ;
#12488 = SURFACE_STYLE_USAGE ( .BOTH. , #18485 ) ;
#12489 = LINE ( 'NONE', #33950, #18310 ) ;
#12490 = VERTEX_POINT ( 'NONE', #31227 ) ;
#12491 = ADVANCED_FACE ( 'NONE', ( #48161 ), #14742, .T. ) ;
#12492 = MECHANICAL_DESIGN_GEOMETRIC_PRESENTATION_REPRESENTATION (  '', ( #14788 ), #42895 ) ;
#12493 = CARTESIAN_POINT ( 'NONE',  ( -2.607480562269075097, 125.4070736234661609, 8.025000000000000355 ) ) ;
#12494 = SURFACE_STYLE_FILL_AREA ( #27623 ) ;
#12495 = DIRECTION ( 'NONE',  ( -1.000000000000000000, -0.000000000000000000, -0.000000000000000000 ) ) ;
#12496 = EDGE_LOOP ( 'NONE', ( #54075, #6447, #62280, #18347 ) ) ;
#12497 = FACE_OUTER_BOUND ( 'NONE', #60457, .T. ) ;
#12498 = LINE ( 'NONE', #2231, #59661 ) ;
#12499 = ORIENTED_EDGE ( 'NONE', *, *, #2893, .T. ) ;
#12500 = CARTESIAN_POINT ( 'NONE',  ( -93.05707362346616662, 0.000000000000000000, 9.524999999999991473 ) ) ;
#12501 = DIRECTION ( 'NONE',  ( -0.000000000000000000, 1.000000000000000000, -0.000000000000000000 ) ) ;
#12502 = CARTESIAN_POINT ( 'NONE',  ( -88.49500000000000455, 6.826472737025113702, -4.959722759717902107 ) ) ;
#12503 = ORIENTED_EDGE ( 'NONE', *, *, #44371, .F. ) ;
#12504 = PRESENTATION_STYLE_ASSIGNMENT (( #65983 ) ) ;
#12505 = STYLED_ITEM ( 'NONE', ( #57511 ), #45698 ) ;
#12506 = CARTESIAN_POINT ( 'NONE',  ( 0.000000000000000000, 0.000000000000000000, 0.000000000000000000 ) ) ;
#12507 = MECHANICAL_DESIGN_GEOMETRIC_PRESENTATION_REPRESENTATION (  '', ( #65298 ), #38395 ) ;
#12508 = SURFACE_STYLE_USAGE ( .BOTH. , #33298 ) ;
#12509 = EDGE_LOOP ( 'NONE', ( #17942, #57992, #154, #20953 ) ) ;
#12510 = LINE ( 'NONE', #54391, #66200 ) ;
#12511 = AXIS2_PLACEMENT_3D ( 'NONE', #40972, #3243, #47298 ) ;
#12512 = SURFACE_STYLE_FILL_AREA ( #60701 ) ;
#12513 = VERTEX_POINT ( 'NONE', #6935 ) ;
#12514 = EDGE_CURVE ( 'NONE', #7755, #18998, #37312, .T. ) ;
#12515 = CIRCLE ( 'NONE', #8012, 0.5000000000000004441 ) ;
#12516 = DIRECTION ( 'NONE',  ( -1.099520432716498623E-15, 1.000000000000000000, 1.099520432716496848E-15 ) ) ;
#12517 = ORIENTED_EDGE ( 'NONE', *, *, #64819, .T. ) ;
#12518 = LINE ( 'NONE', #29394, #4668 ) ;
#12519 = DIRECTION ( 'NONE',  ( 0.000000000000000000, 0.000000000000000000, 1.000000000000000000 ) ) ;
#12520 = CARTESIAN_POINT ( 'NONE',  ( 60.00000000000000000, 1.797044900979284448E-15, -7.000000000000017764 ) ) ;
#12521 = CARTESIAN_POINT ( 'NONE',  ( -181.2570736234661979, 5.598654528085800663, -7.705886871421367523 ) ) ;
#12522 = MECHANICAL_DESIGN_GEOMETRIC_PRESENTATION_REPRESENTATION (  '', ( #6960 ), #6912 ) ;
#12523 = CARTESIAN_POINT ( 'NONE',  ( 21.02379604162863913, 109.9999999999999858, -10.50000000000000000 ) ) ;
#12525 = B_SPLINE_CURVE_WITH_KNOTS ( 'NONE', 3,
 ( #41878, #63296, #30926, #9843, #30216, #69274, #53100, #56975 ),
 .UNSPECIFIED., .F., .F.,
 ( 4, 2, 2, 4 ),
 ( 2.544313220892954975E-07, 0.002693395767724533589, 0.004039966435925755432, 0.005386537104126977275 ),
 .UNSPECIFIED. ) ;
#12524 = DIRECTION ( 'NONE',  ( 0.000000000000000000, 0.000000000000000000, 1.000000000000000000 ) ) ;
#12526 = CARTESIAN_POINT ( 'NONE',  ( -111.3570736234661780, 5.598654528085804216, 7.705886871421366635 ) ) ;
#12527 = ADVANCED_FACE ( 'NONE', ( #6566 ), #17526, .F. ) ;
#12528 = CARTESIAN_POINT ( 'NONE',  ( -84.95707362346617231, 9.058813317711329915, -2.943386871421373119 ) ) ;
#12529 = ORIENTED_EDGE ( 'NONE', *, *, #27850, .T. ) ;
#12530 = AXIS2_PLACEMENT_3D ( 'NONE', #56798, #36040, #24413 ) ;
#12531 = CARTESIAN_POINT ( 'NONE',  ( -9.827790563157511022E-16, 121.4429263765338050, 8.025000000000000355 ) ) ;
#12532 = SURFACE_SIDE_STYLE ('',( #66009 ) ) ;
#12533 = FACE_OUTER_BOUND ( 'NONE', #57687, .T. ) ;
#12534 = CARTESIAN_POINT ( 'NONE',  ( -71.49999999999998579, 64.07124727947029896, 9.500000000000000000 ) ) ;
#12535 = ORIENTED_EDGE ( 'NONE', *, *, #41702, .F. ) ;
#12536 = EDGE_CURVE ( 'NONE', #20383, #2500, #1250, .T. ) ;
#12537 = MECHANICAL_DESIGN_GEOMETRIC_PRESENTATION_REPRESENTATION (  '', ( #64210 ), #10362 ) ;
#12538 = CARTESIAN_POINT ( 'NONE',  ( -156.0550000000000068, -9.827790563157499189E-16, -8.024999999999991473 ) ) ;
#12539 = DIRECTION ( 'NONE',  ( 1.000000000000000000, 0.000000000000000000, 0.000000000000000000 ) ) ;
#12540 = CARTESIAN_POINT ( 'NONE',  ( 13.75000000000000355, 28.24999999999998934, 4.000000000000000000 ) ) ;
#12541 = STYLED_ITEM ( 'NONE', ( #67578 ), #18531 ) ;
#12542 = CARTESIAN_POINT ( 'NONE',  ( -168.8949999999999818, 6.826472737025116366, 4.959722759717898555 ) ) ;
#12543 = CARTESIAN_POINT ( 'NONE',  ( -153.4449999999999932, 0.000000000000000000, 8.024999999999991473 ) ) ;
#12544 = ORIENTED_EDGE ( 'NONE', *, *, #43444, .F. ) ;
#12545 = AXIS2_PLACEMENT_3D ( 'NONE', #66794, #1316, #12965 ) ;
#12546 = CARTESIAN_POINT ( 'NONE',  ( 45.65811388300841855, 10.21937129433613478, 4.000000000000000000 ) ) ;
#12547 = CARTESIAN_POINT ( 'NONE',  ( -76.10500000000000398, -6.826472737025115478, 4.959722759717900331 ) ) ;
#12548 = DIRECTION ( 'NONE',  ( 0.000000000000000000, -1.000000000000000000, 0.000000000000000000 ) ) ;
#12549 = AXIS2_PLACEMENT_3D ( 'NONE', #25495, #62772, #57882 ) ;
#12550 = ADVANCED_FACE ( 'NONE', ( #28011 ), #49522, .F. ) ;
#12551 = CARTESIAN_POINT ( 'NONE',  ( -70.64499999999998181, 4.716976649647091513, -6.492361379858946790 ) ) ;
#12552 = CARTESIAN_POINT ( 'NONE',  ( 8.102448949553181734, 145.5049999999999670, 5.886773742842750679 ) ) ;
#12553 = CARTESIAN_POINT ( 'NONE',  ( 11.00000000000001776, -60.04052944165106709, -35.50000000000000000 ) ) ;
#12554 = COLOUR_RGB ( '', 0.72549020, 0.75294118, 0.79215686) ;
#12555 = CARTESIAN_POINT ( 'NONE',  ( -176.2429263765338021, 5.598654528085804216, 7.705886871421366635 ) ) ;
#12556 = CIRCLE ( 'NONE', #14857, 5.499999999999976907 ) ;
#12557 = CIRCLE ( 'NONE', #39580, 1.000000000000000888 ) ;
#12558 = DIRECTION ( 'NONE',  ( -1.000000000000000000, 0.000000000000000000, 0.000000000000000000 ) ) ;
#12559 = STYLED_ITEM ( 'NONE', ( #29465 ), #23057 ) ;
#12560 = DIRECTION ( 'NONE',  ( -1.000000000000000000, -0.000000000000000000, -0.000000000000000000 ) ) ;
#12561 = AXIS2_PLACEMENT_3D ( 'NONE', #66393, #62501, #46018 ) ;
#12562 = CARTESIAN_POINT ( 'NONE',  ( 0.000000000000000000, 114.9999999999999574, 0.000000000000000000 ) ) ;
#12563 = SURFACE_STYLE_FILL_AREA ( #45675 ) ;
#12564 = ORIENTED_EDGE ( 'NONE', *, *, #21267, .F. ) ;
#12565 = ORIENTED_EDGE ( 'NONE', *, *, #6006, .T. ) ;
#12566 = CARTESIAN_POINT ( 'NONE',  ( -4.716976649647097730, 135.2429263765338305, -6.492361379858953896 ) ) ;
#12567 = STYLED_ITEM ( 'NONE', ( #3384 ), #35614 ) ;
#12568 = EDGE_CURVE ( 'NONE', #35085, #6425, #33853, .T. ) ;
#12569 =( LENGTH_UNIT ( ) NAMED_UNIT ( * ) SI_UNIT ( .MILLI., .METRE. ) );
#12570 = AXIS2_PLACEMENT_3D ( 'NONE', #17571, #49564, #54802 ) ;
#12571 = CARTESIAN_POINT ( 'NONE',  ( 15.98999599679679839, 99.99999999999998579, -7.000000000000000000 ) ) ;
#12572 = CARTESIAN_POINT ( 'NONE',  ( 34.99999999999999289, 99.99999999999997158, 4.000000000000000000 ) ) ;
#12573 =( GEOMETRIC_REPRESENTATION_CONTEXT ( 3 ) GLOBAL_UNCERTAINTY_ASSIGNED_CONTEXT ( ( #8168 ) ) GLOBAL_UNIT_ASSIGNED_CONTEXT ( ( #54097, #68312, #59041 ) ) REPRESENTATION_CONTEXT ( 'NONE', 'WORKASPACE' ) );
#12574 = CARTESIAN_POINT ( 'NONE',  ( 0.000000000000000000, 2.500000000000000000, 9.000000000000001776 ) ) ;
#12575 = ORIENTED_EDGE ( 'NONE', *, *, #39837, .F. ) ;
#12576 = CARTESIAN_POINT ( 'NONE',  ( -104.7549999999999812, 4.716976649647091513, -6.492361379858946790 ) ) ;
#12577 = ORIENTED_EDGE ( 'NONE', *, *, #21455, .F. ) ;
#12578 = SPHERICAL_SURFACE ( 'NONE', #27509, 1.000000000000000000 ) ;
#12579 = LINE ( 'NONE', #11902, #32113 ) ;
#12580 = MECHANICAL_DESIGN_GEOMETRIC_PRESENTATION_REPRESENTATION (  '', ( #50819 ), #5850 ) ;
#12581 = ORIENTED_EDGE ( 'NONE', *, *, #61937, .T. ) ;
#12582 = CARTESIAN_POINT ( 'NONE',  ( -56.69292637653380496, 10.01517768586948698, -1.839758294383808966E-15 ) ) ;
#12583 = CARTESIAN_POINT ( 'NONE',  ( -6.062177826491069510, -2.500000000000000000, 3.499999999999999556 ) ) ;
#12584 = ORIENTED_EDGE ( 'NONE', *, *, #41201, .T. ) ;
#12585 = DIRECTION ( 'NONE',  ( -1.000000000000000000, 0.000000000000000000, 0.000000000000000000 ) ) ;
#12586 =( BOUNDED_SURFACE ( )  B_SPLINE_SURFACE ( 3, 2, ( 
 ( #50783, #44846, #40242 ),
 ( #60613, #50105, #34946 ),
 ( #61321, #7180, #55710 ),
 ( #39213, #45548, #13132 ),
 ( #56391, #18077, #39564 ),
 ( #45193, #60967, #28942 ),
 ( #12428, #2534, #66970 ),
 ( #18431, #2161, #23693 ),
 ( #50434, #18765, #66616 ),
 ( #33889, #66250, #55357 ),
 ( #28608, #1834, #11978 ),
 ( #44730, #322, #55224 ) ),
 .UNSPECIFIED., .F., .F., .F. ) 
 B_SPLINE_SURFACE_WITH_KNOTS ( ( 4, 2, 2, 2, 2, 4 ),
 ( 3, 3 ),
 ( 8.673617379884035472E-19, 0.001495124371074673829, 0.002242686556612010201, 0.002990248742149346790, 0.004485373113224019534, 0.005980497484298692712 ),
 ( 0.000000000000000000, 1.000000000000000000 ),
 .UNSPECIFIED. ) 
 GEOMETRIC_REPRESENTATION_ITEM ( )  RATIONAL_B_SPLINE_SURFACE ( (
 ( 1.000000000000000000, 0.8674236696762898102, 1.000000000000000000),
 ( 1.000000000000000000, 0.8646670541289291911, 1.000000000000000000),
 ( 1.000000000000000000, 0.8610282887621616421, 1.000000000000000000),
 ( 1.000000000000000000, 0.8545310245463959564, 1.000000000000000000),
 ( 1.000000000000000000, 0.8521934417079706225, 1.000000000000000000),
 ( 1.000000000000000000, 0.8472483593196091789, 1.000000000000000000),
 ( 1.000000000000000000, 0.8446295995112632626, 1.000000000000000000),
 ( 1.000000000000000000, 0.8366484175561841319, 1.000000000000000000),
 ( 1.000000000000000000, 0.8311340418845757361, 1.000000000000000000),
 ( 1.000000000000000000, 0.8205640772812347050, 1.000000000000000000),
 ( 1.000000000000000000, 0.8154939450290221714, 1.000000000000000000),
 ( 1.000000000000000000, 0.8111477107414829524, 1.000000000000000000) ) ) 
 REPRESENTATION_ITEM ( '' )  SURFACE ( )  );
#12587 = ORIENTED_EDGE ( 'NONE', *, *, #53670, .F. ) ;
#12588 = VERTEX_POINT ( 'NONE', #40714 ) ;
#12589 = MECHANICAL_DESIGN_GEOMETRIC_PRESENTATION_REPRESENTATION (  '', ( #30563 ), #37370 ) ;
#12590 = SURFACE_SIDE_STYLE ('',( #61136 ) ) ;
#12591 = CYLINDRICAL_SURFACE ( 'NONE', #54159, 0.2500000000000002220 ) ;
#12592 = SURFACE_STYLE_USAGE ( .BOTH. , #65387 ) ;
#12593 = FACE_OUTER_BOUND ( 'NONE', #57267, .T. ) ;
#12594 = ORIENTED_EDGE ( 'NONE', *, *, #30154, .T. ) ;
#12595 = CARTESIAN_POINT ( 'NONE',  ( -7.632228543268608334, 135.8429263765337964, 2.479861379858952830 ) ) ;
#12596 = DIRECTION ( 'NONE',  ( -0.000000000000000000, 1.000000000000000000, -0.000000000000000000 ) ) ;
#12597 = CARTESIAN_POINT ( 'NONE',  ( 185.0000000000000000, 0.000000000000000000, 0.000000000000000000 ) ) ;
#12598 = AXIS2_PLACEMENT_3D ( 'NONE', #44508, #56756, #56386 ) ;
#12599 = DIRECTION ( 'NONE',  ( -0.000000000000000000, -0.000000000000000000, -1.000000000000000000 ) ) ;
#12600 = CARTESIAN_POINT ( 'NONE',  ( 72.50000000000000000, 36.32520566882265456, -10.00000000000000000 ) ) ;
#12601 = ORIENTED_EDGE ( 'NONE', *, *, #31995, .T. ) ;
#12602 = EDGE_CURVE ( 'NONE', #53207, #20985, #30107, .T. ) ;
#12603 = FACE_OUTER_BOUND ( 'NONE', #66335, .T. ) ;
#12604 = VERTEX_POINT ( 'NONE', #45657 ) ;
#12605 = DIRECTION ( 'NONE',  ( 0.000000000000000000, 1.000000000000000000, -0.000000000000000000 ) ) ;
#12606 = CARTESIAN_POINT ( 'NONE',  ( -4.716976649647097730, 139.3570736234661638, -6.492361379858953896 ) ) ;
#12607 = CARTESIAN_POINT ( 'NONE',  ( -30.38025804287905629, -13.49999999999999822, -7.000000000000000000 ) ) ;
#12608 = DIRECTION ( 'NONE',  ( 0.7071067811865425767, 8.659560562354873694E-17, -0.7071067811865525687 ) ) ;
#12610 = CARTESIAN_POINT ( 'NONE',  ( -129.5049999999999670, -6.826472737025115478, -4.959722759717899443 ) ) ;
#12609 = STYLED_ITEM ( 'NONE', ( #46458 ), #60579 ) ;
#12611 = CARTESIAN_POINT ( 'NONE',  ( -195.0000000000000000, 0.000000000000000000, 0.000000000000000000 ) ) ;
#12612 = SPHERICAL_SURFACE ( 'NONE', #68722, 1.000000000000000000 ) ;
#12613 = ORIENTED_EDGE ( 'NONE', *, *, #52743, .T. ) ;
#12614 = LINE ( 'NONE', #60452, #10429 ) ;
#12615 = DIRECTION ( 'NONE',  ( 0.000000000000000000, 0.000000000000000000, -1.000000000000000000 ) ) ;
#12616 = VERTEX_POINT ( 'NONE', #13950 ) ;
#12617 = CIRCLE ( 'NONE', #32875, 0.5000000000000004441 ) ;
#12618 = VERTEX_POINT ( 'NONE', #62125 ) ;
#12619 = SURFACE_STYLE_USAGE ( .BOTH. , #61485 ) ;
#12620 = DIRECTION ( 'NONE',  ( 0.000000000000000000, 0.000000000000000000, 1.000000000000000000 ) ) ;
#12621 = CARTESIAN_POINT ( 'NONE',  ( 25.75000000000001066, 21.99999999999998224, 3.750000000000000000 ) ) ;
#12622 = ORIENTED_EDGE ( 'NONE', *, *, #19130, .T. ) ;
#12623 = SURFACE_SIDE_STYLE ('',( #23205 ) ) ;
#12624 = EDGE_CURVE ( 'NONE', #18241, #23764, #14295, .T. ) ;
#12625 = CARTESIAN_POINT ( 'NONE',  ( -45.00000000000000000, 9.708372675170618749, 10.00000000000000000 ) ) ;
#12626 = AXIS2_PLACEMENT_3D ( 'NONE', #35550, #8475, #50678 ) ;
#12627 = CARTESIAN_POINT ( 'NONE',  ( 0.7098900097155618205, 7.000000000000007105, -1.987393404142764886E-14 ) ) ;
#12629 = ADVANCED_FACE ( 'NONE', ( #34368, #35419 ), #29057, .F. ) ;
#12628 = AXIS2_PLACEMENT_3D ( 'NONE', #55263, #364, #21894 ) ;
#12630 = CARTESIAN_POINT ( 'NONE',  ( -182.2450000000000045, -4.716976649647093289, -6.492361379858945902 ) ) ;
#12631 = DIRECTION ( 'NONE',  ( -0.000000000000000000, -0.000000000000000000, -1.000000000000000000 ) ) ;
#12632 = VERTEX_POINT ( 'NONE', #50213 ) ;
#12633 = AXIS2_PLACEMENT_3D ( 'NONE', #45860, #57076, #8897 ) ;
#12634 = EDGE_CURVE ( 'NONE', #49593, #40233, #1934, .T. ) ;
#12635 = CARTESIAN_POINT ( 'NONE',  ( -144.5070736234661695, 8.102448949553176405, 5.886773742842740909 ) ) ;
#12636 = CARTESIAN_POINT ( 'NONE',  ( 0.000000000000000000, 134.9429263765338192, -8.025000000000000355 ) ) ;
#12637 = CARTESIAN_POINT ( 'NONE',  ( 6.724456118907052193, 154.5000000000000853, -6.760243897016276371 ) ) ;
#12638 = CARTESIAN_POINT ( 'NONE',  ( 52.49999999999998579, 2.715530000339800426E-15, 11.50000000000000000 ) ) ;
#12639 = CARTESIAN_POINT ( 'NONE',  ( 17.25000000000000711, 24.99999999999998224, 4.000000000000000000 ) ) ;
#12640 = EDGE_CURVE ( 'NONE', #53362, #16904, #62056, .T. ) ;
#12641 = CONICAL_SURFACE ( 'NONE', #17205, 5.499999999999976907, 0.7853981633974300713 ) ;
#12642 = CARTESIAN_POINT ( 'NONE',  ( -100.9449999999999932, -9.827790563157499189E-16, -8.024999999999991473 ) ) ;
#12643 = CARTESIAN_POINT ( 'NONE',  ( 10.01517768586949231, 121.8049999999999784, 1.839758294383810543E-15 ) ) ;
#12644 = CARTESIAN_POINT ( 'NONE',  ( -74.99499999999999034, -6.826472737025115478, 4.959722759717900331 ) ) ;
#12645 = CIRCLE ( 'NONE', #41934, 0.5000000000000004441 ) ;
#12646 = CARTESIAN_POINT ( 'NONE',  ( 0.9728900412908074724, 111.9999999999999858, -7.965808808122197604 ) ) ;
#12647 = PLANE ( 'NONE',  #12362 ) ;
#12648 = CARTESIAN_POINT ( 'NONE',  ( -5.705565085145811288, 2.472216779103303175, -4.117671386636410524 ) ) ;
#12649 = CARTESIAN_POINT ( 'NONE',  ( 3.000000000000030198, 42.00000000000000000, 80.00402776293826435 ) ) ;
#12650 = CYLINDRICAL_SURFACE ( 'NONE', #39770, 9.524999999999991473 ) ;
#12651 = ORIENTED_EDGE ( 'NONE', *, *, #18019, .F. ) ;
#12653 = MECHANICAL_DESIGN_GEOMETRIC_PRESENTATION_REPRESENTATION (  '', ( #43050 ), #37432 ) ;
#12652 = CARTESIAN_POINT ( 'NONE',  ( -127.4929263765338163, -8.102448949553172852, 5.886773742842742685 ) ) ;
#12654 = CARTESIAN_POINT ( 'NONE',  ( -138.5949999999999420, 2.607480562269073321, 8.024999999999991473 ) ) ;
#12655 =( NAMED_UNIT ( * ) SI_UNIT ( $, .STERADIAN. ) SOLID_ANGLE_UNIT ( ) );
#12656 =( GEOMETRIC_REPRESENTATION_CONTEXT ( 3 ) GLOBAL_UNCERTAINTY_ASSIGNED_CONTEXT ( ( #23001 ) ) GLOBAL_UNIT_ASSIGNED_CONTEXT ( ( #60531, #54903, #7771 ) ) REPRESENTATION_CONTEXT ( 'NONE', 'WORKASPACE' ) );
#12657 = FILL_AREA_STYLE_COLOUR ( '', #9351 ) ;
#12658 = EDGE_LOOP ( 'NONE', ( #67135, #55323, #24517, #63603 ) ) ;
#12660 = ORIENTED_EDGE ( 'NONE', *, *, #28394, .T. ) ;
#12659 = PRESENTATION_LAYER_ASSIGNMENT (  '', '', ( #39663 ) ) ;
#12661 = DIRECTION ( 'NONE',  ( 0.000000000000000000, 0.000000000000000000, 1.000000000000000000 ) ) ;
#12662 = CONICAL_SURFACE ( 'NONE', #38591, 5.000000000000000000, 0.7853981633974415066 ) ;
#12663 = FILL_AREA_STYLE_COLOUR ( '', #7970 ) ;
#12664 = SURFACE_SIDE_STYLE ('',( #17637 ) ) ;
#12665 = STYLED_ITEM ( 'NONE', ( #1826 ), #23821 ) ;
#12666 = CARTESIAN_POINT ( 'NONE',  ( 7.511572993685799101E-16, -2.500000000000000000, -6.999999999999997335 ) ) ;
#12667 = CARTESIAN_POINT ( 'NONE',  ( -126.0570736234661808, 0.000000000000000000, 9.524999999999991473 ) ) ;
#12668 = EDGE_LOOP ( 'NONE', ( #24640, #43479, #12029, #4093 ) ) ;
#12669 = CARTESIAN_POINT ( 'NONE',  ( -139.1049999999999898, -6.826472737025113702, 4.959722759717902107 ) ) ;
#12670 = ORIENTED_EDGE ( 'NONE', *, *, #65724, .F. ) ;
#12671 = ORIENTED_EDGE ( 'NONE', *, *, #36879, .T. ) ;
#12672 = DIRECTION ( 'NONE',  ( -0.000000000000000000, -1.000000000000000000, -0.000000000000000000 ) ) ;
#12673 =( NAMED_UNIT ( * ) SI_UNIT ( $, .STERADIAN. ) SOLID_ANGLE_UNIT ( ) );
#12674 = AXIS2_PLACEMENT_3D ( 'NONE', #10880, #69612, #41891 ) ;
#12675 = ORIENTED_EDGE ( 'NONE', *, *, #20697, .T. ) ;
#12676 = LINE ( 'NONE', #54882, #57898 ) ;
#12677 = CARTESIAN_POINT ( 'NONE',  ( -9.058813317711338797, 131.3449999999999989, 2.943386871421373563 ) ) ;
#12678 = FILL_AREA_STYLE ('',( #39461 ) ) ;
#12679 = CIRCLE ( 'NONE', #23934, 1.000000000000000000 ) ;
#12680 = ORIENTED_EDGE ( 'NONE', *, *, #25736, .T. ) ;
#12681 = CARTESIAN_POINT ( 'NONE',  ( 9.058813317711337021, 142.6549999999999727, 2.943386871421375783 ) ) ;
#12682 = CARTESIAN_POINT ( 'NONE',  ( -52.70499999999996277, 2.607480562269072433, 8.024999999999991473 ) ) ;
#12683 = CARTESIAN_POINT ( 'NONE',  ( 41.68104242135559190, 107.4439537334017984, -3.570039632082178116 ) ) ;
#12684 = ORIENTED_EDGE ( 'NONE', *, *, #7553, .T. ) ;
#12685 = CARTESIAN_POINT ( 'NONE',  ( 10.01517768586949231, 160.8049999999999216, 1.839758294383810543E-15 ) ) ;
#12686 = DIRECTION ( 'NONE',  ( 0.000000000000000000, 0.000000000000000000, 1.000000000000000000 ) ) ;
#12687 = CARTESIAN_POINT ( 'NONE',  ( -88.64292637653380780, -5.598654528085801552, 7.705886871421367523 ) ) ;
#12688 = AXIS2_PLACEMENT_3D ( 'NONE', #54388, #6529, #6210 ) ;
#12689 = CIRCLE ( 'NONE', #2556, 5.000000000000000000 ) ;
#12690 = SURFACE_SIDE_STYLE ('',( #60877 ) ) ;
#12691 = PLANE ( 'NONE',  #39942 ) ;
#12692 = STYLED_ITEM ( 'NONE', ( #32193 ), #19531 ) ;
#12693 = ORIENTED_EDGE ( 'NONE', *, *, #38726, .F. ) ;
#12694 = EDGE_CURVE ( 'NONE', #32736, #48045, #55816, .T. ) ;
#12695 = CARTESIAN_POINT ( 'NONE',  ( 23.71231517720798365, 117.4999999999999716, -10.00000000000000000 ) ) ;
#12696 = ORIENTED_EDGE ( 'NONE', *, *, #63706, .T. ) ;
#12697 = CARTESIAN_POINT ( 'NONE',  ( -32.56443198605217049, -8.762778093183483108, -2.500000000007921219 ) ) ;
#12698 = DIRECTION ( 'NONE',  ( -1.000000000000000000, -0.000000000000000000, -0.000000000000000000 ) ) ;
#12699 = CARTESIAN_POINT ( 'NONE',  ( -157.5550000000000068, 0.000000000000000000, 8.024999999999991473 ) ) ;
#12700 = ORIENTED_EDGE ( 'NONE', *, *, #47959, .F. ) ;
#12701 = EDGE_CURVE ( 'NONE', #31165, #56538, #34578, .T. ) ;
#12702 =( BOUNDED_CURVE ( )  B_SPLINE_CURVE ( 2, ( #54307, #49745, #32493, #23012, #53955, #60286, #33555, #12083, #65912, #28604, #48743 ),
 .UNSPECIFIED., .F., .F. ) 
 B_SPLINE_CURVE_WITH_KNOTS ( ( 3, 2, 2, 2, 2, 3 ),
 ( 0.9782608695652174058, 0.9804347826086956541, 0.9826086956521739024, 0.9847826086956521507, 0.9869565217391303991, 0.9891304347826086474 ),
 .UNSPECIFIED. ) 
 CURVE ( )  GEOMETRIC_REPRESENTATION_ITEM ( )  RATIONAL_B_SPLINE_CURVE ( ( 1.000000000000000000, 0.9510565162951535312, 1.000000000000000000, 0.9510565162951535312, 1.000000000000000000, 0.9510565162951535312, 1.000000000000000000, 0.9510565162951535312, 1.000000000000000000, 0.9510565162951535312, 1.000000000000000000 ) ) 
 REPRESENTATION_ITEM ( '' )  );
#12703 = CONICAL_SURFACE ( 'NONE', #21695, 5.500000000000005329, 0.7853981633974579379 ) ;
#12704 = PRESENTATION_STYLE_ASSIGNMENT (( #49676 ) ) ;
#12705 = FILL_AREA_STYLE_COLOUR ( '', #19757 ) ;
#12706 = EDGE_LOOP ( 'NONE', ( #36528, #36659, #8453, #54685 ) ) ;
#12707 = ADVANCED_FACE ( 'NONE', ( #29785 ), #37184, .F. ) ;
#12708 = VERTEX_POINT ( 'NONE', #5117 ) ;
#12709 = DIRECTION ( 'NONE',  ( 1.000000000000000000, -0.000000000000000000, 0.000000000000000000 ) ) ;
#12710 = CARTESIAN_POINT ( 'NONE',  ( -45.91547277936962956, 9.430195807687217879, -3.508932040081443660 ) ) ;
#12711 = CARTESIAN_POINT ( 'NONE',  ( -76.25499999999999545, -4.716976649647092401, 6.492361379858946790 ) ) ;
#12712 = ORIENTED_EDGE ( 'NONE', *, *, #40214, .F. ) ;
#12713 = EDGE_CURVE ( 'NONE', #6337, #31668, #21514, .T. ) ;
#12714 = EDGE_CURVE ( 'NONE', #11684, #22849, #60813, .T. ) ;
#12715 = COLOUR_RGB ( '', 0.72549020, 0.75294118, 0.79215686) ;
#12717 = VECTOR ( 'NONE', #65554, 1000.000000000000000 ) ;
#12716 = CIRCLE ( 'NONE', #44202, 1.000000000000000888 ) ;
#12718 = CARTESIAN_POINT ( 'NONE',  ( 6.117035285937315159, 43.00000000000000000, -28.67160620906788537 ) ) ;
#12719 = DIRECTION ( 'NONE',  ( 1.000000000000000000, -0.000000000000000000, 0.000000000000000000 ) ) ;
#12720 = MECHANICAL_DESIGN_GEOMETRIC_PRESENTATION_REPRESENTATION (  '', ( #311 ), #11624 ) ;
#12721 = EDGE_CURVE ( 'NONE', #24442, #47284, #57424, .T. ) ;
#12722 = DIRECTION ( 'NONE',  ( -0.000000000000000000, -1.000000000000000000, -0.000000000000000000 ) ) ;
#12723 = VERTEX_POINT ( 'NONE', #30810 ) ;
#12724 = FILL_AREA_STYLE ('',( #45133 ) ) ;
#12726 =( NAMED_UNIT ( * ) SI_UNIT ( $, .STERADIAN. ) SOLID_ANGLE_UNIT ( ) );
#12725 = DIRECTION ( 'NONE',  ( -1.000000000000000000, 0.000000000000000000, 0.000000000000000000 ) ) ;
#12727 = AXIS2_PLACEMENT_3D ( 'NONE', #28908, #27527, #28563 ) ;
#12728 = CARTESIAN_POINT ( 'NONE',  ( -5.598654528085808657, 140.6449999999999818, 7.705886871421373741 ) ) ;
#12729 = CARTESIAN_POINT ( 'NONE',  ( -110.8449999999999847, -7.632228543268599452, 2.479861379858951054 ) ) ;
#12730 = FILL_AREA_STYLE_COLOUR ( '', #61658 ) ;
#12731 = AXIS2_PLACEMENT_3D ( 'NONE', #17820, #5855, #64623 ) ;
#12733 =( LENGTH_UNIT ( ) NAMED_UNIT ( * ) SI_UNIT ( .MILLI., .METRE. ) );
#12732 = DIRECTION ( 'NONE',  ( 6.938893903907222067E-15, 0.000000000000000000, 1.000000000000000000 ) ) ;
#12734 = CARTESIAN_POINT ( 'NONE',  ( -156.4429263765338192, -1.166476076187852838E-15, -9.524999999999991473 ) ) ;
#12735 = TOROIDAL_SURFACE ( 'NONE', #2600, 111.0000000000000142, 1.000000000000000000 ) ;
#12736 = FILL_AREA_STYLE_COLOUR ( '', #51852 ) ;
#12737 = CARTESIAN_POINT ( 'NONE',  ( -165.8949999999999818, 6.826472737025116366, 4.959722759717898555 ) ) ;
#12738 = VECTOR ( 'NONE', #48294, 1000.000000000000000 ) ;
#12739 = CIRCLE ( 'NONE', #61036, 2.000000000000001776 ) ;
#12740 = DIRECTION ( 'NONE',  ( -1.000000000000000000, 0.000000000000000000, 0.000000000000000000 ) ) ;
#12741 = ORIENTED_EDGE ( 'NONE', *, *, #31369, .F. ) ;
#12742 = SURFACE_STYLE_FILL_AREA ( #28197 ) ;
#12743 = ORIENTED_EDGE ( 'NONE', *, *, #55426, .T. ) ;
#12744 = CARTESIAN_POINT ( 'NONE',  ( -67.34292637653379643, -9.058813317711329915, 2.943386871421371787 ) ) ;
#12745 = CARTESIAN_POINT ( 'NONE',  ( 35.99999999999999289, 5.000000000000000000, -37.00402776293825724 ) ) ;
#12746 = EDGE_CURVE ( 'NONE', #53049, #23835, #37547, .T. ) ;
#12747 = COLOUR_RGB ( '', 0.66274510, 0.83137255, 0.94901961) ;
#12748 = DIRECTION ( 'NONE',  ( 1.000000000000000000, 0.000000000000000000, 0.000000000000000000 ) ) ;
#12749 = DIRECTION ( 'NONE',  ( 7.709882115452441682E-16, -1.000000000000000000, 0.000000000000000000 ) ) ;
#12750 = EDGE_LOOP ( 'NONE', ( #16203, #48412, #34808, #31904, #59442 ) ) ;
#12751 = CARTESIAN_POINT ( 'NONE',  ( -174.3549999999999898, -4.716976649647093289, -6.492361379858945902 ) ) ;
#12752 = VERTEX_POINT ( 'NONE', #58948 ) ;
#12753 = CARTESIAN_POINT ( 'NONE',  ( 20.57648123223228254, 114.4999999999999574, 10.27659574468085069 ) ) ;
#12754 = MECHANICAL_DESIGN_GEOMETRIC_PRESENTATION_REPRESENTATION (  '', ( #54341 ), #2630 ) ;
#12755 = VECTOR ( 'NONE', #68581, 1000.000000000000000 ) ;
#12756 = DIRECTION ( 'NONE',  ( -1.000000000000000000, 0.000000000000000000, 0.000000000000000000 ) ) ;
#12757 = SURFACE_SIDE_STYLE ('',( #28922 ) ) ;
#12758 = CARTESIAN_POINT ( 'NONE',  ( 4.716976649647096842, 149.8570736234661638, 6.492361379858953896 ) ) ;
#12759 =( GEOMETRIC_REPRESENTATION_CONTEXT ( 3 ) GLOBAL_UNCERTAINTY_ASSIGNED_CONTEXT ( ( #3703 ) ) GLOBAL_UNIT_ASSIGNED_CONTEXT ( ( #703, #1041, #38802 ) ) REPRESENTATION_CONTEXT ( 'NONE', 'WORKASPACE' ) );
#12760 = ORIENTED_EDGE ( 'NONE', *, *, #23132, .T. ) ;
#12761 = AXIS2_PLACEMENT_3D ( 'NONE', #60943, #28583, #29986 ) ;
#12762 = DIRECTION ( 'NONE',  ( -0.9704308468600219006, -0.2413793103448194366, 0.000000000000000000 ) ) ;
#12763 = CARTESIAN_POINT ( 'NONE',  ( -4.750000000000002665, 0.000000000000000000, 3.750000000000000000 ) ) ;
#12764 = CARTESIAN_POINT ( 'NONE',  ( -83.45499999999998408, 7.632228543268599452, -2.479861379858951942 ) ) ;
#12765 = CARTESIAN_POINT ( 'NONE',  ( -4.716976649647097730, 121.3570736234661638, -6.492361379858953896 ) ) ;
#12766 = CARTESIAN_POINT ( 'NONE',  ( -1.166476076187854022E-15, 130.0549999999999784, 9.525000000000000355 ) ) ;
#12767 = CYLINDRICAL_SURFACE ( 'NONE', #19485, 9.524999999999991473 ) ;
#12768 = DIRECTION ( 'NONE',  ( 0.000000000000000000, 0.000000000000000000, -1.000000000000000000 ) ) ;
#12769 = EDGE_CURVE ( 'NONE', #44423, #14638, #66392, .T. ) ;
#12770 = CARTESIAN_POINT ( 'NONE',  ( -73.25707362346616947, 5.598654528085800663, -7.705886871421367523 ) ) ;
#12771 = TOROIDAL_SURFACE ( 'NONE', #13940, 0.5000000000000000000, 0.2500000000000000000 ) ;
#12772 = ADVANCED_FACE ( 'NONE', ( #20257 ), #47044, .T. ) ;
#12773 = SURFACE_SIDE_STYLE ('',( #21602 ) ) ;
#12774 = CARTESIAN_POINT ( 'NONE',  ( 12.00000000000001776, 14.00000000000000000, -29.68999999999999417 ) ) ;
#12775 = CARTESIAN_POINT ( 'NONE',  ( -113.6070736234661638, -8.102448949553174629, 5.886773742842742685 ) ) ;
#12776 = ORIENTED_EDGE ( 'NONE', *, *, #68555, .T. ) ;
#12778 = CARTESIAN_POINT ( 'NONE',  ( -74.99999999999998579, 50.00000000000000000, 6.500000000000000000 ) ) ;
#12777 = AXIS2_PLACEMENT_3D ( 'NONE', #46323, #46689, #9715 ) ;
#12779 = CARTESIAN_POINT ( 'NONE',  ( -53.09499999999997755, -2.607480562269071545, -8.024999999999991473 ) ) ;
#12780 = ORIENTED_EDGE ( 'NONE', *, *, #11357, .T. ) ;
#12781 = FILL_AREA_STYLE_COLOUR ( '', #43000 ) ;
#12782 = AXIS2_PLACEMENT_3D ( 'NONE', #49155, #43561, #37935 ) ;
#12783 = EDGE_CURVE ( 'NONE', #197, #37399, #68823, .T. ) ;
#12784 = DIRECTION ( 'NONE',  ( 0.000000000000000000, 0.000000000000000000, 1.000000000000000000 ) ) ;
#12785 = DIRECTION ( 'NONE',  ( 0.000000000000000000, 0.000000000000000000, 1.000000000000000000 ) ) ;
#12786 = EDGE_LOOP ( 'NONE', ( #13050, #49358, #4471 ) ) ;
#12787 = CARTESIAN_POINT ( 'NONE',  ( -54.44499999999999318, 0.000000000000000000, 8.024999999999991473 ) ) ;
#12788 = CARTESIAN_POINT ( 'NONE',  ( -83.49999999999998579, 4.336808689942018722E-16, 24.00000000000000000 ) ) ;
#12789 = ORIENTED_EDGE ( 'NONE', *, *, #8990, .T. ) ;
#12790 = CIRCLE ( 'NONE', #7184, 10.00000000000000000 ) ;
#12791 = AXIS2_PLACEMENT_3D ( 'NONE', #54446, #897, #43941 ) ;
#12792 = CARTESIAN_POINT ( 'NONE',  ( -75.00000000000000000, 9.581012678897810275, 6.371410634540560558 ) ) ;
#12793 = CARTESIAN_POINT ( 'NONE',  ( -104.4549999999999983, 7.632228543268599452, -2.479861379858951942 ) ) ;
#12794 = VERTEX_POINT ( 'NONE', #31497 ) ;
#12795 = SURFACE_STYLE_USAGE ( .BOTH. , #7189 ) ;
#12796 = EDGE_CURVE ( 'NONE', #58139, #44514, #58712, .T. ) ;
#12797 = FILL_AREA_STYLE ('',( #45202 ) ) ;
#12798 = CARTESIAN_POINT ( 'NONE',  ( 18.00000000000000711, 30.74999999999999289, -3.750000000000000000 ) ) ;
#12799 = CARTESIAN_POINT ( 'NONE',  ( -150.5070736234661410, 8.102448949553176405, 5.886773742842740909 ) ) ;
#12800 = CARTESIAN_POINT ( 'NONE',  ( -52.74999999999999289, 0.000000000000000000, -2.000000000000000000 ) ) ;
#12801 = CARTESIAN_POINT ( 'NONE',  ( 5.598654528085805993, 138.2449999999999761, 7.705886871421374629 ) ) ;
#12802 = CARTESIAN_POINT ( 'NONE',  ( -80.75707362346616947, -5.598654528085801552, 7.705886871421367523 ) ) ;
#12803 = AXIS2_PLACEMENT_3D ( 'NONE', #61412, #13229, #12186 ) ;
#12804 = ADVANCED_FACE ( 'NONE', ( #42463 ), #63860, .T. ) ;
#12805 = PLANE ( 'NONE',  #6694 ) ;
#12806 = ORIENTED_EDGE ( 'NONE', *, *, #26813, .T. ) ;
#12808 =( LENGTH_UNIT ( ) NAMED_UNIT ( * ) SI_UNIT ( .MILLI., .METRE. ) );
#12807 = LINE ( 'NONE', #19471, #9964 ) ;
#12809 = SURFACE_SIDE_STYLE ('',( #28632 ) ) ;
#12810 = CIRCLE ( 'NONE', #49887, 1.000000000000000888 ) ;
#12811 = CARTESIAN_POINT ( 'NONE',  ( -132.2049999999999841, -2.607480562269071545, -8.024999999999991473 ) ) ;
#12812 = CARTESIAN_POINT ( 'NONE',  ( 0.000000000000000000, 0.000000000000000000, 0.000000000000000000 ) ) ;
#12813 = CARTESIAN_POINT ( 'NONE',  ( -146.2429263765338021, 5.598654528085804216, 7.705886871421366635 ) ) ;
#12814 =( NAMED_UNIT ( * ) PLANE_ANGLE_UNIT ( ) SI_UNIT ( $, .RADIAN. ) );
#12815 = CARTESIAN_POINT ( 'NONE',  ( -134.2450000000000045, -4.716976649647093289, -6.492361379858945902 ) ) ;
#12816 =( GEOMETRIC_REPRESENTATION_CONTEXT ( 3 ) GLOBAL_UNCERTAINTY_ASSIGNED_CONTEXT ( ( #57921 ) ) GLOBAL_UNIT_ASSIGNED_CONTEXT ( ( #61028, #26514, #20195 ) ) REPRESENTATION_CONTEXT ( 'NONE', 'WORKASPACE' ) );
#12817 = CARTESIAN_POINT ( 'NONE',  ( -130.3449999999999989, 7.632228543268599452, -2.479861379858951942 ) ) ;
#12818 = CARTESIAN_POINT ( 'NONE',  ( -35.65778776279520912, -9.947368421052624754, 4.481646853389230856 ) ) ;
#12819 = EDGE_LOOP ( 'NONE', ( #58699, #53405, #23789, #64622 ) ) ;
#12820 = CARTESIAN_POINT ( 'NONE',  ( 71.99999999999998579, 119.9999999999997868, -7.500000000000000000 ) ) ;
#12821 = SURFACE_STYLE_USAGE ( .BOTH. , #46629 ) ;
#12822 =( NAMED_UNIT ( * ) SI_UNIT ( $, .STERADIAN. ) SOLID_ANGLE_UNIT ( ) );
#12823 = CARTESIAN_POINT ( 'NONE',  ( -182.6929263765338192, 10.01517768586948698, -1.839758294383808571E-15 ) ) ;
#12824 = CARTESIAN_POINT ( 'NONE',  ( -46.64499999999998892, 4.716976649647091513, -6.492361379858946790 ) ) ;
#12825 = CIRCLE ( 'NONE', #27420, 0.9999999999999992228 ) ;
#12826 = FACE_OUTER_BOUND ( 'NONE', #29053, .T. ) ;
#12827 = FACE_OUTER_BOUND ( 'NONE', #50680, .T. ) ;
#12828 = ADVANCED_BREP_SHAPE_REPRESENTATION ( '', ( #3235, #42840 ), #37166 ) ;
#12829 = AXIS2_PLACEMENT_3D ( 'NONE', #12520, #7269, #28696 ) ;
#12830 = DIRECTION ( 'NONE',  ( -0.000000000000000000, 1.000000000000000000, 0.000000000000000000 ) ) ;
#12831 = CARTESIAN_POINT ( 'NONE',  ( 21.02379604162863913, 110.4999999999999858, 10.50000000000000000 ) ) ;
#12832 = CARTESIAN_POINT ( 'NONE',  ( -95.99292637653377369, 8.102448949553171076, -5.886773742842744461 ) ) ;
#12833 = SHAPE_DEFINITION_REPRESENTATION ( #41167, #5102 ) ;
#12834 = CARTESIAN_POINT ( 'NONE',  ( -51.93475478252885580, -11.36189310745057846, 1.762106798099256411 ) ) ;
#12835 = CARTESIAN_POINT ( 'NONE',  ( -52.74999999999999289, 0.000000000000000000, -7.000000000000000000 ) ) ;
#12836 = EDGE_CURVE ( 'NONE', #12357, #65192, #12123, .T. ) ;
#12837 = AXIS2_PLACEMENT_3D ( 'NONE', #57957, #63815, #37141 ) ;
#12838 = VECTOR ( 'NONE', #41159, 1000.000000000000000 ) ;
#12839 = DIRECTION ( 'NONE',  ( -0.000000000000000000, 0.000000000000000000, 1.000000000000000000 ) ) ;
#12840 = CARTESIAN_POINT ( 'NONE',  ( -40.82708550458224295, 108.1272155206434320, 3.301554093733328088 ) ) ;
#12841 = PRESENTATION_LAYER_ASSIGNMENT (  '', '', ( #35305 ) ) ;
#12842 = ORIENTED_EDGE ( 'NONE', *, *, #34366, .T. ) ;
#12843 = CARTESIAN_POINT ( 'NONE',  ( 16.00000000000001776, 15.00000000000000000, 29.68999999999999417 ) ) ;
#12844 = FILL_AREA_STYLE_COLOUR ( '', #44429 ) ;
#12845 =( NAMED_UNIT ( * ) PLANE_ANGLE_UNIT ( ) SI_UNIT ( $, .RADIAN. ) );
#12846 = EDGE_LOOP ( 'NONE', ( #28392, #29939, #16482, #51287 ) ) ;
#12847 = SURFACE_SIDE_STYLE ('',( #29728 ) ) ;
#12848 = CARTESIAN_POINT ( 'NONE',  ( -6.826472737025120807, 122.1070736234661780, 4.959722759717906548 ) ) ;
#12849 =( GEOMETRIC_REPRESENTATION_CONTEXT ( 3 ) GLOBAL_UNCERTAINTY_ASSIGNED_CONTEXT ( ( #7501 ) ) GLOBAL_UNIT_ASSIGNED_CONTEXT ( ( #9904, #42627, #64033 ) ) REPRESENTATION_CONTEXT ( 'NONE', 'WORKASPACE' ) );
#12850 = COLOUR_RGB ( '', 0.31764706, 0.68627451, 0.89019608) ;
#12851 = EDGE_CURVE ( 'NONE', #19928, #34574, #5441, .T. ) ;
#12852 = FACE_OUTER_BOUND ( 'NONE', #14407, .T. ) ;
#12853 = CARTESIAN_POINT ( 'NONE',  ( 74.52070078832288402, 19.38218994716114452, -6.500000000000000888 ) ) ;
#12854 = DIRECTION ( 'NONE',  ( 0.000000000000000000, 0.000000000000000000, 1.000000000000000000 ) ) ;
#12855 = ORIENTED_EDGE ( 'NONE', *, *, #27212, .T. ) ;
#12856 = CARTESIAN_POINT ( 'NONE',  ( -94.64292637653380780, -5.598654528085801552, 7.705886871421367523 ) ) ;
#12857 = EDGE_CURVE ( 'NONE', #37037, #33122, #22679, .T. ) ;
#12858 = AXIS2_PLACEMENT_3D ( 'NONE', #52126, #52476, #20793 ) ;
#12859 =( NAMED_UNIT ( * ) SI_UNIT ( $, .STERADIAN. ) SOLID_ANGLE_UNIT ( ) );
#12860 = EDGE_CURVE ( 'NONE', #43417, #17125, #39249, .T. ) ;
#12861 = FILL_AREA_STYLE ('',( #61039 ) ) ;
#12862 = CIRCLE ( 'NONE', #52221, 1.000000000000000888 ) ;
#12863 = CARTESIAN_POINT ( 'NONE',  ( 57.00000000000000000, 5.000000000000000000, 77.00402776293825013 ) ) ;
#12864 = CARTESIAN_POINT ( 'NONE',  ( -82.19499999999999318, 8.437984349512085203, -1.550032578732815448E-15 ) ) ;
#12865 = ORIENTED_EDGE ( 'NONE', *, *, #7233, .F. ) ;
#12866 = SURFACE_STYLE_FILL_AREA ( #45271 ) ;
#12867 = EDGE_CURVE ( 'NONE', #2945, #23924, #47424, .T. ) ;
#12868 = PLANE ( 'NONE',  #30656 ) ;
#12869 = VERTEX_POINT ( 'NONE', #64574 ) ;
#12870 = EDGE_CURVE ( 'NONE', #31971, #11259, #18198, .T. ) ;
#12871 = DIRECTION ( 'NONE',  ( 0.000000000000000000, 0.000000000000000000, -1.000000000000000000 ) ) ;
#12872 = AXIS2_PLACEMENT_3D ( 'NONE', #67352, #19148, #8966 ) ;
#12873 = ORIENTED_EDGE ( 'NONE', *, *, #8895, .T. ) ;
#12874 = CARTESIAN_POINT ( 'NONE',  ( 10.00000000000002309, 60.69879356856722552, 69.02971849933236115 ) ) ;
#12875 = ORIENTED_EDGE ( 'NONE', *, *, #64581, .T. ) ;
#12876 =( NAMED_UNIT ( * ) SI_UNIT ( $, .STERADIAN. ) SOLID_ANGLE_UNIT ( ) );
#12877 = FILL_AREA_STYLE ('',( #60706 ) ) ;
#12878 = CARTESIAN_POINT ( 'NONE',  ( 1.400957079539665084, -2.390838073342431702, 7.000000000000000888 ) ) ;
#12879 = COLOUR_RGB ( '', 0.09019608, 0.27058824, 0.51372549) ;
#12880 = CARTESIAN_POINT ( 'NONE',  ( -175.5570736234661808, -1.166476076187852838E-15, -9.524999999999991473 ) ) ;
#12881 = UNCERTAINTY_MEASURE_WITH_UNIT (LENGTH_MEASURE( 1.000000000000000082E-05 ), #51486, 'distance_accuracy_value', 'NONE');
#12882 = DIRECTION ( 'NONE',  ( 0.000000000000000000, 0.000000000000000000, 1.000000000000000000 ) ) ;
#12883 = CARTESIAN_POINT ( 'NONE',  ( 10.01517768586949408, 114.6949999999999932, 1.839758294383810543E-15 ) ) ;
#12884 = CIRCLE ( 'NONE', #52240, 0.5000000000000000000 ) ;
#12885 = CARTESIAN_POINT ( 'NONE',  ( -116.0070736234661553, -8.102448949553172852, -5.886773742842741797 ) ) ;
#12886 = CARTESIAN_POINT ( 'NONE',  ( -43.75000000000000000, 4.336808689942018722E-16, 0.000000000000000000 ) ) ;
#12887 = AXIS2_PLACEMENT_3D ( 'NONE', #12553, #23458, #18192 ) ;
#12888 = DIRECTION ( 'NONE',  ( 0.000000000000000000, -0.000000000000000000, 1.000000000000000000 ) ) ;
#12889 = ORIENTED_EDGE ( 'NONE', *, *, #50599, .F. ) ;
#12890 = CARTESIAN_POINT ( 'NONE',  ( 4.716976649647096842, 121.7429263765338163, 6.492361379858953896 ) ) ;
#12891 = CARTESIAN_POINT ( 'NONE',  ( -74.99999999999998579, 50.00000000000000000, 6.499999999999999112 ) ) ;
#12892 = FACE_OUTER_BOUND ( 'NONE', #53778, .T. ) ;
#12893 = CYLINDRICAL_SURFACE ( 'NONE', #51181, 0.2500000000000002220 ) ;
#12894 = ORIENTED_EDGE ( 'NONE', *, *, #3209, .F. ) ;
#12895 = CARTESIAN_POINT ( 'NONE',  ( -155.1550000000000011, 7.632228543268600340, 2.479861379858949277 ) ) ;
#12896 = CARTESIAN_POINT ( 'NONE',  ( -183.3769980489784643, -0.6272992113221751431, -9.148001951021605294 ) ) ;
#12897 = CARTESIAN_POINT ( 'NONE',  ( -168.7450000000000045, 4.716976649647094177, 6.492361379858945902 ) ) ;
#12898 = CARTESIAN_POINT ( 'NONE',  ( -157.3449999999999989, 7.632228543268599452, -2.479861379858951942 ) ) ;
#12899 = ADVANCED_FACE ( 'NONE', ( #6164 ), #38913, .T. ) ;
#12900 = EDGE_LOOP ( 'NONE', ( #18132, #47650, #33075, #4210, #18755, #68254, #14777, #45590, #21371, #55290 ) ) ;
#12901 = AXIS2_PLACEMENT_3D ( 'NONE', #10502, #31939, #4661 ) ;
#12902 = DIRECTION ( 'NONE',  ( -0.000000000000000000, -0.000000000000000000, -1.000000000000000000 ) ) ;
#12903 = SURFACE_STYLE_USAGE ( .BOTH. , #45985 ) ;
#12904 = CARTESIAN_POINT ( 'NONE',  ( -77.75499999999999545, 4.716976649647091513, -6.492361379858946790 ) ) ;
#12905 = CARTESIAN_POINT ( 'NONE',  ( -35.20898490747966747, -11.12536675346265724, 3.476728976952998096 ) ) ;
#12906 = CARTESIAN_POINT ( 'NONE',  ( -167.8429263765337964, 9.058813317711329915, -2.943386871421373119 ) ) ;
#12907 = AXIS2_PLACEMENT_3D ( 'NONE', #26882, #19978, #41476 ) ;
#12908 = CARTESIAN_POINT ( 'NONE',  ( -68.69499999999999318, -8.437984349512086979, 5.166775262442717831E-16 ) ) ;
#12909 = CARTESIAN_POINT ( 'NONE',  ( -9.058813317711337021, 144.1549999999999727, -2.943386871421374895 ) ) ;
#12910 = SURFACE_STYLE_FILL_AREA ( #55824 ) ;
#12911 = UNCERTAINTY_MEASURE_WITH_UNIT (LENGTH_MEASURE( 1.000000000000000082E-05 ), #5440, 'distance_accuracy_value', 'NONE');
#12912 = B_SPLINE_CURVE_WITH_KNOTS ( 'NONE', 3,
 ( #38019, #1676, #23195, #32689, #54143, #64718, #16559, #59407, #2349, #8737 ),
 .UNSPECIFIED., .F., .F.,
 ( 4, 2, 2, 2, 4 ),
 ( 0.000000000000000000, 0.001951620466334530717, 0.003903240932669061435, 0.005854861399003591718, 0.007806481865338122869 ),
 .UNSPECIFIED. ) ;
#12913 = SURFACE_STYLE_FILL_AREA ( #27341 ) ;
#12914 = CARTESIAN_POINT ( 'NONE',  ( 52.75000000000000000, 25.24999999999998579, -3.750000000000000000 ) ) ;
#12915 = PRESENTATION_STYLE_ASSIGNMENT (( #18561 ) ) ;
#12916 = PRESENTATION_STYLE_ASSIGNMENT (( #7636 ) ) ;
#12917 = STYLED_ITEM ( 'NONE', ( #38519 ), #38903 ) ;
#12918 = AXIS2_PLACEMENT_3D ( 'NONE', #29205, #18683, #2436 ) ;
#12919 = LINE ( 'NONE', #50229, #44285 ) ;
#12920 = ORIENTED_EDGE ( 'NONE', *, *, #59354, .T. ) ;
#12921 = ORIENTED_EDGE ( 'NONE', *, *, #7782, .F. ) ;
#12922 = SURFACE_STYLE_USAGE ( .BOTH. , #61115 ) ;
#12924 = SURFACE_SIDE_STYLE ('',( #66040 ) ) ;
#12923 = MECHANICAL_DESIGN_GEOMETRIC_PRESENTATION_REPRESENTATION (  '', ( #3931 ), #47860 ) ;
#12925 = EDGE_CURVE ( 'NONE', #51005, #53684, #32532, .T. ) ;
#12926 = AXIS2_PLACEMENT_3D ( 'NONE', #6494, #27937, #55035 ) ;
#12927 = CARTESIAN_POINT ( 'NONE',  ( 0.000000000000000000, 2.299999999999999822, 0.000000000000000000 ) ) ;
#12928 =( NAMED_UNIT ( * ) SI_UNIT ( $, .STERADIAN. ) SOLID_ANGLE_UNIT ( ) );
#12929 = PRESENTATION_STYLE_ASSIGNMENT (( #61118 ) ) ;
#12930 =( NAMED_UNIT ( * ) SI_UNIT ( $, .STERADIAN. ) SOLID_ANGLE_UNIT ( ) );
#12931 = ORIENTED_EDGE ( 'NONE', *, *, #10112, .T. ) ;
#12932 = ORIENTED_EDGE ( 'NONE', *, *, #801, .F. ) ;
#12933 =( LENGTH_UNIT ( ) NAMED_UNIT ( * ) SI_UNIT ( .MILLI., .METRE. ) );
#12934 = DIRECTION ( 'NONE',  ( 0.000000000000000000, 0.000000000000000000, 1.000000000000000000 ) ) ;
#12935 = EDGE_CURVE ( 'NONE', #67106, #59375, #55027, .T. ) ;
#12936 = EDGE_LOOP ( 'NONE', ( #7004, #58923, #52180, #46669 ) ) ;
#12937 = CARTESIAN_POINT ( 'NONE',  ( 3.094860106618435136, 113.4050000000000011, -9.525000000000000355 ) ) ;
#12938 = DIRECTION ( 'NONE',  ( -0.000000000000000000, 1.000000000000000000, -0.000000000000000000 ) ) ;
#12939 = ORIENTED_EDGE ( 'NONE', *, *, #5972, .F. ) ;
#12940 = DIRECTION ( 'NONE',  ( 0.000000000000000000, 0.000000000000000000, 1.000000000000000000 ) ) ;
#12941 = CARTESIAN_POINT ( 'NONE',  ( -122.8449999999999847, -7.632228543268599452, 2.479861379858951054 ) ) ;
#12942 = ORIENTED_EDGE ( 'NONE', *, *, #48423, .F. ) ;
#12943 = AXIS2_PLACEMENT_3D ( 'NONE', #11676, #11326, #32790 ) ;
#12944 = ORIENTED_EDGE ( 'NONE', *, *, #31299, .F. ) ;
#12945 = PRESENTATION_LAYER_ASSIGNMENT (  '', '', ( #32043 ) ) ;
#12946 = CARTESIAN_POINT ( 'NONE',  ( -10.44806848068614258, -11.82018413492187747, 2.075183112132959362 ) ) ;
#12947 = CARTESIAN_POINT ( 'NONE',  ( -10.39230484541326938, -1.107695154586735509, -1.661048719643172847E-15 ) ) ;
#12948 = VERTEX_POINT ( 'NONE', #18110 ) ;
#12949 = CARTESIAN_POINT ( 'NONE',  ( -7.632228543268607446, 141.5429263765338135, -2.479861379858953718 ) ) ;
#12950 = CARTESIAN_POINT ( 'NONE',  ( -13.75000000000000533, 30.74999999999999289, -4.000000000000000000 ) ) ;
#12951 = DIRECTION ( 'NONE',  ( 1.000000000000000000, -0.000000000000000000, 0.000000000000000000 ) ) ;
#12952 = EDGE_CURVE ( 'NONE', #40860, #31338, #28643, .T. ) ;
#12953 =( GEOMETRIC_REPRESENTATION_CONTEXT ( 3 ) GLOBAL_UNCERTAINTY_ASSIGNED_CONTEXT ( ( #36925 ) ) GLOBAL_UNIT_ASSIGNED_CONTEXT ( ( #56067, #57109, #66992 ) ) REPRESENTATION_CONTEXT ( 'NONE', 'WORKASPACE' ) );
#12954 = CARTESIAN_POINT ( 'NONE',  ( -34.99999999999999289, 99.99999999999998579, -7.000000000000000000 ) ) ;
#12955 = DIRECTION ( 'NONE',  ( 0.000000000000000000, 0.000000000000000000, -1.000000000000000000 ) ) ;
#12956 = ORIENTED_EDGE ( 'NONE', *, *, #43634, .T. ) ;
#12957 = CARTESIAN_POINT ( 'NONE',  ( 1.000000000000000888, 1.000000000000000222, -4.000000000000000000 ) ) ;
#12958 = ORIENTED_EDGE ( 'NONE', *, *, #22979, .T. ) ;
#12959 = VECTOR ( 'NONE', #47430, 1000.000000000000000 ) ;
#12960 = PLANE ( 'NONE',  #13197 ) ;
#12961 = DIRECTION ( 'NONE',  ( -0.000000000000000000, -1.000000000000000000, -0.000000000000000000 ) ) ;
#12962 = DIRECTION ( 'NONE',  ( -0.5000000000000002220, 0.000000000000000000, 0.8660254037844384856 ) ) ;
#12963 = AXIS2_PLACEMENT_3D ( 'NONE', #42885, #64278, #16130 ) ;
#12964 = CARTESIAN_POINT ( 'NONE',  ( -133.5549999999999784, 0.000000000000000000, 8.024999999999991473 ) ) ;
#12965 = DIRECTION ( 'NONE',  ( 0.000000000000000000, 0.000000000000000000, -1.000000000000000000 ) ) ;
#12966 = ORIENTED_EDGE ( 'NONE', *, *, #12514, .F. ) ;
#12967 = PLANE ( 'NONE',  #8216 ) ;
#12968 = CARTESIAN_POINT ( 'NONE',  ( 3.108481029118195238, 9.000000000000007105, 0.5125184569636095366 ) ) ;
#12969 = CARTESIAN_POINT ( 'NONE',  ( -45.00000000000000000, 8.749900610107136600, -6.882725987574755955 ) ) ;
#12970 = ORIENTED_EDGE ( 'NONE', *, *, #33679, .T. ) ;
#12971 = ORIENTED_EDGE ( 'NONE', *, *, #34383, .T. ) ;
#12972 =( LENGTH_UNIT ( ) NAMED_UNIT ( * ) SI_UNIT ( .MILLI., .METRE. ) );
#12973 = CARTESIAN_POINT ( 'NONE',  ( -20.44164625062140317, 115.3859073845563756, 10.00000000000000000 ) ) ;
#12974 = CARTESIAN_POINT ( 'NONE',  ( -51.65707362346616804, 9.058813317711329915, 2.943386871421369566 ) ) ;
#12975 = CARTESIAN_POINT ( 'NONE',  ( -48.50499999999998835, -6.826472737025115478, -4.959722759717899443 ) ) ;
#12977 = VERTEX_POINT ( 'NONE', #45225 ) ;
#12976 = AXIS2_PLACEMENT_3D ( 'NONE', #40837, #29184, #24966 ) ;
#12978 = CARTESIAN_POINT ( 'NONE',  ( -184.1049999999999613, -6.826472737025115478, 4.959722759717900331 ) ) ;
#12979 = SURFACE_SIDE_STYLE ('',( #29132 ) ) ;
#12980 = EDGE_CURVE ( 'NONE', #49536, #26439, #50469, .T. ) ;
#12981 = AXIS2_PLACEMENT_3D ( 'NONE', #25335, #62276, #62955 ) ;
#12982 = DIRECTION ( 'NONE',  ( -0.2413793103448194644, -0.9704308468600220117, 0.000000000000000000 ) ) ;
#12983 = EDGE_CURVE ( 'NONE', #12794, #28517, #32764, .T. ) ;
#12984 = CARTESIAN_POINT ( 'NONE',  ( 109.0067032876572455, 0.9999999999999991118, -19.20378738324562207 ) ) ;
#12985 = MECHANICAL_DESIGN_GEOMETRIC_PRESENTATION_REPRESENTATION (  '', ( #64666 ), #19724 ) ;
#12986 = VERTEX_POINT ( 'NONE', #1869 ) ;
#12987 = CARTESIAN_POINT ( 'NONE',  ( 24.00000000000000000, -2.250452076942884869E-15, 3.000000000000000000 ) ) ;
#12988 = DIRECTION ( 'NONE',  ( 0.000000000000000000, 0.000000000000000000, -1.000000000000000000 ) ) ;
#12989 = PRESENTATION_LAYER_ASSIGNMENT (  '', '', ( #574 ) ) ;
#12990 = CYLINDRICAL_SURFACE ( 'NONE', #31546, 1.000000000000000888 ) ;
#12991 = CARTESIAN_POINT ( 'NONE',  ( -103.5549999999999926, 0.000000000000000000, 8.024999999999991473 ) ) ;
#12992 = CARTESIAN_POINT ( 'NONE',  ( 0.000000000000000000, 143.9429263765338192, -8.025000000000000355 ) ) ;
#12993 = FACE_OUTER_BOUND ( 'NONE', #59466, .T. ) ;
#12994 = LINE ( 'NONE', #12639, #65166 ) ;
#12995 = CARTESIAN_POINT ( 'NONE',  ( -104.8449999999999989, -7.632228543268599452, 2.479861379858951054 ) ) ;
#12996 = CARTESIAN_POINT ( 'NONE',  ( 0.000000000000000000, 113.5549999999999926, -9.525000000000000355 ) ) ;
#12997 = CARTESIAN_POINT ( 'NONE',  ( -77.54499999999998749, -7.632228543268600340, -2.479861379858950166 ) ) ;
#12998 = FACE_OUTER_BOUND ( 'NONE', #21088, .T. ) ;
#12999 = CARTESIAN_POINT ( 'NONE',  ( -6.062177826491070398, 2.500000000000000000, -3.499999999999998224 ) ) ;
#13000 = UNCERTAINTY_MEASURE_WITH_UNIT (LENGTH_MEASURE( 1.000000000000000082E-05 ), #34505, 'distance_accuracy_value', 'NONE');
#13001 = CARTESIAN_POINT ( 'NONE',  ( 60.00000000000000000, 1.797044900979284448E-15, -12.00000000000000000 ) ) ;
#13002 = MECHANICAL_DESIGN_GEOMETRIC_PRESENTATION_REPRESENTATION (  '', ( #19738 ), #8551 ) ;
#13003 = CARTESIAN_POINT ( 'NONE',  ( 41.06080360525773187, 107.9551383427286737, -3.682527553402531240 ) ) ;
#13004 = ORIENTED_EDGE ( 'NONE', *, *, #49144, .T. ) ;
#13005 = CARTESIAN_POINT ( 'NONE',  ( -117.4429263765338050, -1.166476076187852838E-15, -9.524999999999991473 ) ) ;
#13006 = SURFACE_SIDE_STYLE ('',( #14664 ) ) ;
#13007 = CARTESIAN_POINT ( 'NONE',  ( -134.8449999999999989, -7.632228543268599452, 2.479861379858951054 ) ) ;
#13008 = TOROIDAL_SURFACE ( 'NONE', #22014, 9.499999999999998224, 0.5000000000000000000 ) ;
#13009 = DIRECTION ( 'NONE',  ( -0.000000000000000000, -1.000000000000000000, -0.000000000000000000 ) ) ;
#13010 = ADVANCED_FACE ( 'NONE', ( #12465 ), #66999, .T. ) ;
#13012 = TOROIDAL_SURFACE ( 'NONE', #23169, 0.5000000000000000000, 0.2500000000000000000 ) ;
#13011 = FACE_OUTER_BOUND ( 'NONE', #24668, .T. ) ;
#13013 = VERTEX_POINT ( 'NONE', #56427 ) ;
#13014 = ORIENTED_EDGE ( 'NONE', *, *, #31756, .T. ) ;
#13015 =( GEOMETRIC_REPRESENTATION_CONTEXT ( 3 ) GLOBAL_UNCERTAINTY_ASSIGNED_CONTEXT ( ( #27818 ) ) GLOBAL_UNIT_ASSIGNED_CONTEXT ( ( #43958, #54791, #43613 ) ) REPRESENTATION_CONTEXT ( 'NONE', 'WORKASPACE' ) );
#13016 =( BOUNDED_CURVE ( )  B_SPLINE_CURVE ( 2, ( #5126, #32217, #52321, #68473, #64218, #53665, #37560, #41775, #26902, #63193, #36507 ),
 .UNSPECIFIED., .F., .F. ) 
 B_SPLINE_CURVE_WITH_KNOTS ( ( 3, 2, 2, 2, 2, 3 ),
 ( 0.2282608695652119657, 0.2304347826086901863, 0.2326086956521683791, 0.2347826086956465996, 0.2369565217391247924, 0.2391304347826030130 ),
 .UNSPECIFIED. ) 
 CURVE ( )  GEOMETRIC_REPRESENTATION_ITEM ( )  RATIONAL_B_SPLINE_CURVE ( ( 1.000000000000121680, 0.9510565162950315177, 1.000000000000000000, 0.9510565162951535312, 1.000000000000000000, 0.9510565162951535312, 1.000000000000000000, 0.9510565162951535312, 1.000000000000000000, 0.9510565162952816509, 0.9999999999998718803 ) ) 
 REPRESENTATION_ITEM ( '' )  );
#13017 = CARTESIAN_POINT ( 'NONE',  ( -24.00000000000000355, 37.00000000000000000, -4.000000000000000000 ) ) ;
#13018 = CARTESIAN_POINT ( 'NONE',  ( -62.39292637653380069, 8.102448949553176405, 5.886773742842740909 ) ) ;
#13019 =( LENGTH_UNIT ( ) NAMED_UNIT ( * ) SI_UNIT ( .MILLI., .METRE. ) );
#13020 = FILL_AREA_STYLE ('',( #44044 ) ) ;
#13021 = DIRECTION ( 'NONE',  ( 0.000000000000000000, 0.000000000000000000, -1.000000000000000000 ) ) ;
#13022 = CARTESIAN_POINT ( 'NONE',  ( 16.75000000000000711, 27.74999999999998224, 3.750000000000000000 ) ) ;
#13023 = ORIENTED_EDGE ( 'NONE', *, *, #44208, .T. ) ;
#13024 = CARTESIAN_POINT ( 'NONE',  ( -135.2050000000000125, -2.607480562269071545, -8.024999999999991473 ) ) ;
#13025 = ORIENTED_EDGE ( 'NONE', *, *, #21926, .T. ) ;
#13026 = AXIS2_PLACEMENT_3D ( 'NONE', #18224, #40388, #61126 ) ;
#13027 = EDGE_CURVE ( 'NONE', #25731, #41380, #61351, .T. ) ;
#13028 = ORIENTED_EDGE ( 'NONE', *, *, #27092, .T. ) ;
#13029 = DIRECTION ( 'NONE',  ( -1.000000000000000000, 0.000000000000000000, 0.000000000000000000 ) ) ;
#13030 = FACE_BOUND ( 'NONE', #68660, .T. ) ;
#13031 = ORIENTED_EDGE ( 'NONE', *, *, #49556, .T. ) ;
#13032 = VECTOR ( 'NONE', #31382, 1000.000000000000000 ) ;
#13033 = PRESENTATION_STYLE_ASSIGNMENT (( #20291 ) ) ;
#13034 = EDGE_CURVE ( 'NONE', #31626, #67110, #13159, .T. ) ;
#13035 = DIRECTION ( 'NONE',  ( 0.000000000000000000, 0.000000000000000000, 1.000000000000000000 ) ) ;
#13036 = CARTESIAN_POINT ( 'NONE',  ( 8.102448949553183510, 135.9950000000000045, -5.886773742842746238 ) ) ;
#13037 = CARTESIAN_POINT ( 'NONE',  ( -72.50000000000000000, 14.49137674618942562, 9.500000000000000000 ) ) ;
#13038 = AXIS2_PLACEMENT_3D ( 'NONE', #16871, #1653, #33702 ) ;
#13039 = ORIENTED_EDGE ( 'NONE', *, *, #15916, .F. ) ;
#13040 = CARTESIAN_POINT ( 'NONE',  ( -8.102448949553179958, 144.6049999999999613, 5.886773742842747126 ) ) ;
#13041 = CARTESIAN_POINT ( 'NONE',  ( -50.00499999999998835, 6.826472737025115478, 4.959722759717899443 ) ) ;
#13042 = CARTESIAN_POINT ( 'NONE',  ( 41.05030025768302693, 107.9631293162027674, -3.671816393059894157 ) ) ;
#13043 = ORIENTED_EDGE ( 'NONE', *, *, #69649, .T. ) ;
#13044 = CARTESIAN_POINT ( 'NONE',  ( 10.01517768586949231, 154.8050000000000352, 1.839758294383810543E-15 ) ) ;
#13045 = DIRECTION ( 'NONE',  ( 0.000000000000000000, -1.000000000000000000, 0.000000000000000000 ) ) ;
#13046 = UNCERTAINTY_MEASURE_WITH_UNIT (LENGTH_MEASURE( 1.000000000000000082E-05 ), #60929, 'distance_accuracy_value', 'NONE');
#13047 = CARTESIAN_POINT ( 'NONE',  ( -88.79292637653379927, -3.094860106618429807, 9.524999999999991473 ) ) ;
#13048 = EDGE_CURVE ( 'NONE', #53214, #6337, #45580, .T. ) ;
#13049 = CARTESIAN_POINT ( 'NONE',  ( 20.71231517720798010, 149.4999999999999716, 10.00000000000000000 ) ) ;
#13050 = ORIENTED_EDGE ( 'NONE', *, *, #63509, .T. ) ;
#13051 = ORIENTED_EDGE ( 'NONE', *, *, #22813, .T. ) ;
#13052 = DIRECTION ( 'NONE',  ( -1.000000000000000000, -0.000000000000000000, -0.000000000000000000 ) ) ;
#13053 = DIRECTION ( 'NONE',  ( 0.6216216216216311485, -0.7833176619561784682, 0.000000000000000000 ) ) ;
#13054 = CARTESIAN_POINT ( 'NONE',  ( -195.0000000000000000, 0.000000000000000000, 9.524999999999991473 ) ) ;
#13055 = CARTESIAN_POINT ( 'NONE',  ( -159.6550000000000011, -7.632228543268600340, -2.479861379858950166 ) ) ;
#13056 = VERTEX_POINT ( 'NONE', #60649 ) ;
#13057 = UNCERTAINTY_MEASURE_WITH_UNIT (LENGTH_MEASURE( 1.000000000000000082E-05 ), #23975, 'distance_accuracy_value', 'NONE');
#13058 = CIRCLE ( 'NONE', #10798, 0.5000000000000004441 ) ;
#13059 = DIRECTION ( 'NONE',  ( 0.000000000000000000, 0.000000000000000000, 1.000000000000000000 ) ) ;
#13060 = CARTESIAN_POINT ( 'NONE',  ( 45.64107345563247975, 10.15688972729190809, -6.260993343996352323 ) ) ;
#13061 =( LENGTH_UNIT ( ) NAMED_UNIT ( * ) SI_UNIT ( .MILLI., .METRE. ) );
#13062 = ORIENTED_EDGE ( 'NONE', *, *, #28224, .T. ) ;
#13063 = VERTEX_POINT ( 'NONE', #7892 ) ;
#13064 = AXIS2_PLACEMENT_3D ( 'NONE', #34421, #67830, #29485 ) ;
#13065 = DIRECTION ( 'NONE',  ( 0.000000000000000000, 0.000000000000000000, 1.000000000000000000 ) ) ;
#13066 = CARTESIAN_POINT ( 'NONE',  ( -75.05499999999997840, -9.827790563157499189E-16, -8.024999999999991473 ) ) ;
#13067 = VERTEX_POINT ( 'NONE', #44878 ) ;
#13068 =( GEOMETRIC_REPRESENTATION_CONTEXT ( 3 ) GLOBAL_UNCERTAINTY_ASSIGNED_CONTEXT ( ( #51083 ) ) GLOBAL_UNIT_ASSIGNED_CONTEXT ( ( #19792, #3943, #37056 ) ) REPRESENTATION_CONTEXT ( 'NONE', 'WORKASPACE' ) );
#13069 = DIRECTION ( 'NONE',  ( 0.000000000000000000, 0.000000000000000000, -1.000000000000000000 ) ) ;
#13070 = CARTESIAN_POINT ( 'NONE',  ( -151.4070736234665162, 3.094860106611941220, -9.525000000004705925 ) ) ;
#13071 = CARTESIAN_POINT ( 'NONE',  ( 33.00000000000002132, 15.00000000000000000, 80.00402776293826435 ) ) ;
#13072 = ORIENTED_EDGE ( 'NONE', *, *, #31533, .T. ) ;
#13073 = DIRECTION ( 'NONE',  ( 0.000000000000000000, 0.000000000000000000, 1.000000000000000000 ) ) ;
#13075 =( LENGTH_UNIT ( ) NAMED_UNIT ( * ) SI_UNIT ( .MILLI., .METRE. ) );
#13074 = CARTESIAN_POINT ( 'NONE',  ( -53.15707362346616804, -9.058813317711329915, -2.943386871421370898 ) ) ;
#13076 = AXIS2_PLACEMENT_3D ( 'NONE', #61038, #7582, #39986 ) ;
#13077 = CARTESIAN_POINT ( 'NONE',  ( 5.598654528085805993, 138.2449999999999761, 7.705886871421374629 ) ) ;
#13078 = CARTESIAN_POINT ( 'NONE',  ( -103.3449999999999989, 7.632228543268599452, -2.479861379858951942 ) ) ;
#13079 = DIRECTION ( 'NONE',  ( 1.000000000000000000, 0.000000000000000000, 0.000000000000000000 ) ) ;
#13081 = CARTESIAN_POINT ( 'NONE',  ( -18.97010937149592280, 11.60744552740335855, 3.056979887745398194 ) ) ;
#13080 = FACE_OUTER_BOUND ( 'NONE', #54613, .T. ) ;
#13082 = CARTESIAN_POINT ( 'NONE',  ( -146.2429263765338021, 5.598654528085804216, 7.705886871421366635 ) ) ;
#13083 =( NAMED_UNIT ( * ) SI_UNIT ( $, .STERADIAN. ) SOLID_ANGLE_UNIT ( ) );
#13084 = CARTESIAN_POINT ( 'NONE',  ( -167.8449999999999989, -7.632228543268599452, 2.479861379858951054 ) ) ;
#13085 = EDGE_CURVE ( 'NONE', #56538, #3684, #6241, .T. ) ;
#13086 = EDGE_LOOP ( 'NONE', ( #49086, #33712, #61373, #25009, #50648, #38751, #24465, #27619, #57415, #43543, #18168, #44083, #3059, #65308 ) ) ;
#13087 = CARTESIAN_POINT ( 'NONE',  ( -2.607480562269053781, 130.2929263765338135, 8.025000000000016342 ) ) ;
#13088 = ORIENTED_EDGE ( 'NONE', *, *, #2240, .F. ) ;
#13090 = EDGE_CURVE ( 'NONE', #50571, #43604, #40270, .T. ) ;
#13089 = FACE_OUTER_BOUND ( 'NONE', #65755, .T. ) ;
#13091 = EDGE_CURVE ( 'NONE', #417, #51841, #41825, .T. ) ;
#13092 = CARTESIAN_POINT ( 'NONE',  ( 60.00000000000000000, 149.4999999999999716, 9.500000000000000000 ) ) ;
#13093 = CARTESIAN_POINT ( 'NONE',  ( 0.000000000000000000, 148.0570736234661524, -8.025000000000000355 ) ) ;
#13094 = DIRECTION ( 'NONE',  ( -1.000000000000000000, 0.000000000000000000, 0.000000000000000000 ) ) ;
#13095 = MECHANICAL_DESIGN_GEOMETRIC_PRESENTATION_REPRESENTATION (  '', ( #33346 ), #17613 ) ;
#13096 = ORIENTED_EDGE ( 'NONE', *, *, #26530, .F. ) ;
#13097 = CARTESIAN_POINT ( 'NONE',  ( -158.1550000000000011, 7.632228543268600340, 2.479861379858949277 ) ) ;
#13098 = EDGE_CURVE ( 'NONE', #46060, #62390, #5285, .T. ) ;
#13099 = AXIS2_PLACEMENT_3D ( 'NONE', #61044, #54721, #38954 ) ;
#13100 = ORIENTED_EDGE ( 'NONE', *, *, #49026, .T. ) ;
#13101 = PRESENTATION_STYLE_ASSIGNMENT (( #23661 ) ) ;
#13102 = FILL_AREA_STYLE ('',( #27868 ) ) ;
#13104 = EDGE_CURVE ( 'NONE', #16901, #29002, #49395, .T. ) ;
#13103 = FILL_AREA_STYLE ('',( #18402 ) ) ;
#13105 = MECHANICAL_DESIGN_GEOMETRIC_PRESENTATION_REPRESENTATION (  '', ( #36721 ), #58086 ) ;
#13106 = CARTESIAN_POINT ( 'NONE',  ( 4.000000000000030198, 43.00000000000000000, 79.00402776293826435 ) ) ;
#13107 = ADVANCED_FACE ( 'NONE', ( #30362 ), #20173, .T. ) ;
#13108 =( LENGTH_UNIT ( ) NAMED_UNIT ( * ) SI_UNIT ( .MILLI., .METRE. ) );
#13109 = CARTESIAN_POINT ( 'NONE',  ( 8.437984349512095861, 159.3070736234661240, 1.550032578732817026E-15 ) ) ;
#13110 =( BOUNDED_CURVE ( )  B_SPLINE_CURVE ( 2, ( #37033, #52159, #35961, #47608, #3916, #21145, #15229, #4619, #20822, #31009, #30652 ),
 .UNSPECIFIED., .F., .F. ) 
 B_SPLINE_CURVE_WITH_KNOTS ( ( 3, 2, 2, 2, 2, 3 ),
 ( 0.2934782608695582495, 0.2956521739130364423, 0.2978260869565146907, 0.2999999999999928835, 0.3021739130434711318, 0.3043478260869493801 ),
 .UNSPECIFIED. ) 
 CURVE ( )  GEOMETRIC_REPRESENTATION_ITEM ( )  RATIONAL_B_SPLINE_CURVE ( ( 1.000000000000157430, 0.9510565162949961016, 1.000000000000000000, 0.9510565162951535312, 1.000000000000000000, 0.9510565162951535312, 1.000000000000000000, 0.9510565162951535312, 1.000000000000000000, 0.9510565162953147356, 0.9999999999998387956 ) ) 
 REPRESENTATION_ITEM ( '' )  );
#13111 = EDGE_LOOP ( 'NONE', ( #15981, #61134, #35450, #18908 ) ) ;
#13112 = SURFACE_STYLE_USAGE ( .BOTH. , #35277 ) ;
#13114 = EDGE_CURVE ( 'NONE', #67128, #5051, #21839, .T. ) ;
#13113 = CARTESIAN_POINT ( 'NONE',  ( -1.166476076187854022E-15, 115.0549999999999926, 9.525000000000000355 ) ) ;
#13115 = CARTESIAN_POINT ( 'NONE',  ( -87.50499999999995282, -6.826472737025113702, -4.959722759717900331 ) ) ;
#13116 = CARTESIAN_POINT ( 'NONE',  ( -1.166476076187854022E-15, 124.0549999999999784, 9.525000000000000355 ) ) ;
#13117 = UNCERTAINTY_MEASURE_WITH_UNIT (LENGTH_MEASURE( 1.000000000000000082E-05 ), #18254, 'distance_accuracy_value', 'NONE');
#13118 = PRESENTATION_STYLE_ASSIGNMENT (( #51457 ) ) ;
#13119 = CARTESIAN_POINT ( 'NONE',  ( 20.51914007124930706, 114.9043000146497207, 10.00000000000000000 ) ) ;
#13120 = DIRECTION ( 'NONE',  ( 1.000000000000000000, 3.469446951953611033E-15, 0.000000000000000000 ) ) ;
#13121 = CARTESIAN_POINT ( 'NONE',  ( -113.4570736234661723, -9.058813317711329915, 2.943386871421371787 ) ) ;
#13122 = ORIENTED_EDGE ( 'NONE', *, *, #11585, .T. ) ;
#13123 = DIRECTION ( 'NONE',  ( 0.000000000000000000, 0.000000000000000000, -1.000000000000000000 ) ) ;
#13124 = FILL_AREA_STYLE_COLOUR ( '', #37452 ) ;
#13125 = CARTESIAN_POINT ( 'NONE',  ( -50.39499999999999602, -6.826472737025115478, -4.959722759717899443 ) ) ;
#13126 = VERTEX_POINT ( 'NONE', #36418 ) ;
#13127 = CARTESIAN_POINT ( 'NONE',  ( 57.49999999999998579, 30.74999999999999289, 3.750000000000000000 ) ) ;
#13128 = VECTOR ( 'NONE', #839, 1000.000000000000000 ) ;
#13129 = CARTESIAN_POINT ( 'NONE',  ( -45.58243994668686838, 8.116436936526458368, -6.493641663363978189 ) ) ;
#13130 = FILL_AREA_STYLE_COLOUR ( '', #68930 ) ;
#13131 = VERTEX_POINT ( 'NONE', #62403 ) ;
#13132 = CARTESIAN_POINT ( 'NONE',  ( -50.68995449411814036, -10.61513085179375970, 3.914528793814394891 ) ) ;
#13133 = CARTESIAN_POINT ( 'NONE',  ( -50.84499999999997044, -7.632228543268599452, 2.479861379858951054 ) ) ;
#13134 = FILL_AREA_STYLE_COLOUR ( '', #45665 ) ;
#13135 = EDGE_LOOP ( 'NONE', ( #9409, #19790, #8844, #59837 ) ) ;
#13136 = CARTESIAN_POINT ( 'NONE',  ( -74.09581123568146666, 9.387410786201540347, 6.121260521433846691 ) ) ;
#13137 = CARTESIAN_POINT ( 'NONE',  ( -99.95499999999998408, -7.632228543268599452, 2.479861379858951054 ) ) ;
#13138 = EDGE_LOOP ( 'NONE', ( #51739, #1308, #12577, #12565 ) ) ;
#13139 =( NAMED_UNIT ( * ) PLANE_ANGLE_UNIT ( ) SI_UNIT ( $, .RADIAN. ) );
#13140 = DIRECTION ( 'NONE',  ( 1.000000000000000000, 0.000000000000000000, -0.000000000000000000 ) ) ;
#13141 = CARTESIAN_POINT ( 'NONE',  ( -141.0570736234661808, 0.000000000000000000, 9.524999999999991473 ) ) ;
#13142 = SURFACE_SIDE_STYLE ('',( #39929 ) ) ;
#13143 = CARTESIAN_POINT ( 'NONE',  ( -5.598654528085808657, 140.6449999999999818, 7.705886871421373741 ) ) ;
#13144 = CARTESIAN_POINT ( 'NONE',  ( -83.45707362346617231, -9.058813317711329915, 2.943386871421371787 ) ) ;
#13145 = CARTESIAN_POINT ( 'NONE',  ( -95.69292637653379074, 10.01517768586948698, -1.839758294383808966E-15 ) ) ;
#13147 = PRESENTATION_STYLE_ASSIGNMENT (( #39937 ) ) ;
#13146 = CARTESIAN_POINT ( 'NONE',  ( -43.99999999999999289, 0.000000000000000000, 9.525000000000000355 ) ) ;
#13148 = CIRCLE ( 'NONE', #22154, 0.5000000000000004441 ) ;
#13149 = CARTESIAN_POINT ( 'NONE',  ( -122.7549999999999955, 4.716976649647091513, -6.492361379858946790 ) ) ;
#13150 = LINE ( 'NONE', #22337, #51085 ) ;
#13151 = LINE ( 'NONE', #68370, #50487 ) ;
#13152 = CARTESIAN_POINT ( 'NONE',  ( 9.058813317711338797, 114.8449999999999847, -2.943386871421372675 ) ) ;
#13153 = CARTESIAN_POINT ( 'NONE',  ( -136.0449999999999875, 7.632228543268600340, 2.479861379858949277 ) ) ;
#13154 = CARTESIAN_POINT ( 'NONE',  ( -122.3949999999999818, -6.826472737025113702, -4.959722759717900331 ) ) ;
#13155 = DIRECTION ( 'NONE',  ( -1.000000000000000000, 0.000000000000000000, 0.000000000000000000 ) ) ;
#13156 = ORIENTED_EDGE ( 'NONE', *, *, #4119, .T. ) ;
#13157 = CARTESIAN_POINT ( 'NONE',  ( 48.75000000000004974, 1.127570259384924864E-13, 3.750000000000000000 ) ) ;
#13158 = CYLINDRICAL_SURFACE ( 'NONE', #833, 5.000000000000004441 ) ;
#13159 = LINE ( 'NONE', #30037, #42964 ) ;
#13160 = CARTESIAN_POINT ( 'NONE',  ( -179.5429263765338135, 9.058813317711329915, 2.943386871421369566 ) ) ;
#13161 = PRESENTATION_STYLE_ASSIGNMENT (( #22700 ) ) ;
#13162 = CARTESIAN_POINT ( 'NONE',  ( 61.99999999999998579, 30.99999999999999289, 4.000000000000000000 ) ) ;
#13163 = MECHANICAL_DESIGN_GEOMETRIC_PRESENTATION_REPRESENTATION (  '', ( #58136 ), #28915 ) ;
#13164 = EDGE_CURVE ( 'NONE', #17330, #21751, #14221, .T. ) ;
#13165 = CARTESIAN_POINT ( 'NONE',  ( 10.00000000000002132, 50.00000000000000000, 60.00000000000000711 ) ) ;
#13166 = CARTESIAN_POINT ( 'NONE',  ( -18.25000000000000711, 33.74999999999999289, -3.750000000000000000 ) ) ;
#13167 = EDGE_CURVE ( 'NONE', #58485, #26613, #20416, .T. ) ;
#13168 = DIRECTION ( 'NONE',  ( -0.000000000000000000, -0.000000000000000000, -1.000000000000000000 ) ) ;
#13169 = CARTESIAN_POINT ( 'NONE',  ( -34.99999999999999289, 99.99999999999998579, -10.00000000000000000 ) ) ;
#13170 = CARTESIAN_POINT ( 'NONE',  ( -93.44292637653380496, -1.166476076187852838E-15, -9.524999999999991473 ) ) ;
#13171 = PRODUCT_CONTEXT ( 'NONE', #17723, 'mechanical' ) ;
#13173 = ADVANCED_FACE ( 'NONE', ( #8943 ), #11418, .T. ) ;
#13172 = FACE_OUTER_BOUND ( 'NONE', #64316, .T. ) ;
#13174 = FACE_OUTER_BOUND ( 'NONE', #11997, .T. ) ;
#13175 = APPLICATION_CONTEXT ( 'automotive_design' ) ;
#13176 = CARTESIAN_POINT ( 'NONE',  ( -69.99999999999998579, 50.00000000000000000, -11.50000000000001066 ) ) ;
#13177 = CARTESIAN_POINT ( 'NONE',  ( -195.0000000000000000, 0.000000000000000000, 0.000000000000000000 ) ) ;
#13178 = DIRECTION ( 'NONE',  ( 1.000000000000000000, 1.084202172485503448E-16, 0.000000000000000000 ) ) ;
#13179 = ORIENTED_EDGE ( 'NONE', *, *, #24928, .F. ) ;
#13180 = FILL_AREA_STYLE ('',( #39617 ) ) ;
#13181 = DIRECTION ( 'NONE',  ( 0.000000000000000000, 0.000000000000000000, 1.000000000000000000 ) ) ;
#13182 = EDGE_CURVE ( 'NONE', #33055, #10616, #5779, .T. ) ;
#13183 = CARTESIAN_POINT ( 'NONE',  ( -57.58629378005873889, -7.761720733523185700, -0.7755720678490086728 ) ) ;
#13184 = VERTEX_POINT ( 'NONE', #25116 ) ;
#13185 = CARTESIAN_POINT ( 'NONE',  ( 11.00000000000001776, 15.00000000000000000, 29.68999999999999417 ) ) ;
#13186 = CARTESIAN_POINT ( 'NONE',  ( 0.000000000000000000, 124.0570736234661524, -8.025000000000000355 ) ) ;
#13188 = EDGE_CURVE ( 'NONE', #38790, #60581, #10338, .T. ) ;
#13187 = DIRECTION ( 'NONE',  ( -1.000000000000000000, 0.000000000000000000, 0.000000000000000000 ) ) ;
#13189 = CARTESIAN_POINT ( 'NONE',  ( 25.75000000000001066, 21.74999999999998224, -3.750000000000000000 ) ) ;
#13190 = AXIS2_PLACEMENT_3D ( 'NONE', #41454, #30862, #46400 ) ;
#13191 = ORIENTED_EDGE ( 'NONE', *, *, #9650, .T. ) ;
#13192 = AXIS2_PLACEMENT_3D ( 'NONE', #63679, #285, #21815 ) ;
#13193 = DIRECTION ( 'NONE',  ( 1.156482317317873451E-16, -1.000000000000000000, 0.000000000000000000 ) ) ;
#13194 = DIRECTION ( 'NONE',  ( -1.000000000000000000, 0.000000000000000000, 0.000000000000000000 ) ) ;
#13196 = PLANE ( 'NONE',  #8672 ) ;
#13195 = B_SPLINE_CURVE_WITH_KNOTS ( 'NONE', 3,
 ( #62610, #40164, #66882, #14426, #67559, #29574, #35899, #62278, #45790, #14106, #35563, #19716 ),
 .UNSPECIFIED., .F., .F.,
 ( 4, 2, 2, 2, 2, 4 ),
 ( 0.01082081597914125344, 0.01149352919195929454, 0.01216624240477733390, 0.01351166883041341610, 0.01485709525604949656, 0.01620252168168557702 ),
 .UNSPECIFIED. ) ;
#13197 = AXIS2_PLACEMENT_3D ( 'NONE', #60785, #28783, #13651 ) ;
#13198 = DIRECTION ( 'NONE',  ( 0.000000000000000000, 0.000000000000000000, 1.000000000000000000 ) ) ;
#13199 = B_SPLINE_CURVE_WITH_KNOTS ( 'NONE', 3,
 ( #66401, #55141, #49905, #7649, #60420, #60089 ),
 .UNSPECIFIED., .F., .F.,
 ( 4, 2, 4 ),
 ( 0.005386537104126976408, 0.008060814333094815098, 0.01073509156206265552 ),
 .UNSPECIFIED. ) ;
#13200 = CARTESIAN_POINT ( 'NONE',  ( -15.98999599679679839, 117.4999999999999716, -9.500000000000000000 ) ) ;
#13201 = CARTESIAN_POINT ( 'NONE',  ( -80.09499999999998465, -2.607480562269071545, -8.024999999999991473 ) ) ;
#13202 = VERTEX_POINT ( 'NONE', #11269 ) ;
#13203 = DIRECTION ( 'NONE',  ( 0.000000000000000000, -0.9396926207859105373, -0.3420201433256629953 ) ) ;
#13204 = CARTESIAN_POINT ( 'NONE',  ( 0.04677136509298115974, 68.99999999999998579, -2.000000000000000000 ) ) ;
#13205 = ORIENTED_EDGE ( 'NONE', *, *, #20842, .F. ) ;
#13206 = CARTESIAN_POINT ( 'NONE',  ( -9.827790563157511022E-16, 121.4429263765338050, 8.025000000000000355 ) ) ;
#13207 = FILL_AREA_STYLE_COLOUR ( '', #52766 ) ;
#13208 =( GEOMETRIC_REPRESENTATION_CONTEXT ( 3 ) GLOBAL_UNCERTAINTY_ASSIGNED_CONTEXT ( ( #50221 ) ) GLOBAL_UNIT_ASSIGNED_CONTEXT ( ( #55025, #32531, #64898 ) ) REPRESENTATION_CONTEXT ( 'NONE', 'WORKASPACE' ) );
#13209 = AXIS2_PLACEMENT_3D ( 'NONE', #16882, #66063, #38357 ) ;
#13210 = CARTESIAN_POINT ( 'NONE',  ( 21.25000000000000711, 22.24999999999998224, 4.000000000000000000 ) ) ;
#13211 = VERTEX_POINT ( 'NONE', #26731 ) ;
#13212 = ORIENTED_EDGE ( 'NONE', *, *, #8533, .T. ) ;
#13213 = CARTESIAN_POINT ( 'NONE',  ( -137.2429263765338021, 5.598654528085804216, 7.705886871421366635 ) ) ;
#13214 = SURFACE_SIDE_STYLE ('',( #40005 ) ) ;
#13215 =( LENGTH_UNIT ( ) NAMED_UNIT ( * ) SI_UNIT ( .MILLI., .METRE. ) );
#13216 = CARTESIAN_POINT ( 'NONE',  ( -178.8570736234661638, -5.598654528085803328, -7.705886871421366635 ) ) ;
#13217 = CARTESIAN_POINT ( 'NONE',  ( 2.000000000000009326, 26.00000000000000355, -20.50000000000000355 ) ) ;
#13218 = CARTESIAN_POINT ( 'NONE',  ( -3.094860106618432471, 115.5949999999999704, -9.525000000000000355 ) ) ;
#13219 = CARTESIAN_POINT ( 'NONE',  ( -109.1070736234661922, 8.102448949553171076, -5.886773742842744461 ) ) ;
#13220 = EDGE_CURVE ( 'NONE', #34097, #46742, #55248, .T. ) ;
#13221 = CARTESIAN_POINT ( 'NONE',  ( -183.1015393889102256, 5.789891952623192672, -7.443705283220353408 ) ) ;
#13222 = DIRECTION ( 'NONE',  ( -1.000000000000000000, 1.224646799147349509E-16, 0.000000000000000000 ) ) ;
#13223 = VERTEX_POINT ( 'NONE', #9299 ) ;
#13224 = CARTESIAN_POINT ( 'NONE',  ( 17.00000000000000711, 27.74999999999998224, -3.750000000000000000 ) ) ;
#13225 = FILL_AREA_STYLE_COLOUR ( '', #1722 ) ;
#13226 = CARTESIAN_POINT ( 'NONE',  ( 44.97237157117559292, 9.999999999999980460, -3.164074568774566387 ) ) ;
#13227 =( LENGTH_UNIT ( ) NAMED_UNIT ( * ) SI_UNIT ( .MILLI., .METRE. ) );
#13228 = CARTESIAN_POINT ( 'NONE',  ( -148.1049999999999898, -6.826472737025115478, 4.959722759717900331 ) ) ;
#13229 = DIRECTION ( 'NONE',  ( 0.000000000000000000, 1.000000000000000000, 0.000000000000000000 ) ) ;
#13230 = CARTESIAN_POINT ( 'NONE',  ( -183.7787065195572609, -7.888957336882999272, -3.789685084752649313 ) ) ;
#13231 = CARTESIAN_POINT ( 'NONE',  ( -168.1449999999999818, -4.716976649647092401, 6.492361379858946790 ) ) ;
#13232 = CARTESIAN_POINT ( 'NONE',  ( -161.0949999999999704, -2.607480562269071545, -8.024999999999991473 ) ) ;
#13233 = ORIENTED_EDGE ( 'NONE', *, *, #17116, .T. ) ;
#13234 = CARTESIAN_POINT ( 'NONE',  ( -66.44292637653380496, -1.166476076187852838E-15, -9.524999999999991473 ) ) ;
#13235 = PRESENTATION_STYLE_ASSIGNMENT (( #13588 ) ) ;
#13236 = VECTOR ( 'NONE', #66363, 1000.000000000000000 ) ;
#13237 = CARTESIAN_POINT ( 'NONE',  ( -122.3929263765337936, 8.102448949553176405, 5.886773742842740909 ) ) ;
#13238 = CARTESIAN_POINT ( 'NONE',  ( -70.40499999999997272, -2.607480562269069768, 8.024999999999991473 ) ) ;
#13239 = DIRECTION ( 'NONE',  ( -0.000000000000000000, -1.000000000000000000, -0.000000000000000000 ) ) ;
#13240 = CARTESIAN_POINT ( 'NONE',  ( 11.00000000000001776, 15.00000000000000000, -29.68999999999999417 ) ) ;
#13241 = VECTOR ( 'NONE', #11748, 1000.000000000000000 ) ;
#13242 = VECTOR ( 'NONE', #67756, 1000.000000000000000 ) ;
#13243 = EDGE_CURVE ( 'NONE', #68594, #1306, #54092, .T. ) ;
#13244 = CARTESIAN_POINT ( 'NONE',  ( -68.24499999999999034, -4.716976649647093289, -6.492361379858945902 ) ) ;
#13245 = EDGE_CURVE ( 'NONE', #68902, #28179, #12557, .T. ) ;
#13246 = CARTESIAN_POINT ( 'NONE',  ( 8.102448949553181734, 148.5049999999999955, 5.886773742842750679 ) ) ;
#13247 = CARTESIAN_POINT ( 'NONE',  ( 17.25000000000000711, 24.99999999999998224, -3.750000000000000000 ) ) ;
#13248 = FACE_OUTER_BOUND ( 'NONE', #11884, .T. ) ;
#13249 = CARTESIAN_POINT ( 'NONE',  ( 74.50000000000000000, -2.135340797662720349E-14, -10.00000000000000000 ) ) ;
#13250 = CARTESIAN_POINT ( 'NONE',  ( -19.98288066869250201, 115.0281754944747235, -9.999999999997170264 ) ) ;
#13251 = EDGE_CURVE ( 'NONE', #67765, #68848, #23767, .T. ) ;
#13252 = DIRECTION ( 'NONE',  ( 1.000000000000000000, 0.000000000000000000, 0.000000000000000000 ) ) ;
#13253 = VECTOR ( 'NONE', #64486, 1000.000000000000000 ) ;
#13254 = EDGE_CURVE ( 'NONE', #30142, #25818, #30914, .T. ) ;
#13255 = LINE ( 'NONE', #39345, #21422 ) ;
#13256 = LINE ( 'NONE', #22802, #48751 ) ;
#13257 = ADVANCED_FACE ( 'NONE', ( #65783 ), #61192, .T. ) ;
#13258 = CYLINDRICAL_SURFACE ( 'NONE', #55297, 0.5000000000000004441 ) ;
#13259 = VERTEX_POINT ( 'NONE', #54524 ) ;
#13260 = ORIENTED_EDGE ( 'NONE', *, *, #16162, .T. ) ;
#13261 = CYLINDRICAL_SURFACE ( 'NONE', #1517, 4.999999999999997335 ) ;
#13262 = CARTESIAN_POINT ( 'NONE',  ( 71.18918918918917882, 14.09971791521133433, -7.500000000000000000 ) ) ;
#13263 = ADVANCED_FACE ( 'NONE', ( #28461 ), #1706, .T. ) ;
#13264 = SURFACE_STYLE_FILL_AREA ( #39696 ) ;
#13265 = PLANE ( 'NONE',  #67808 ) ;
#13266 = ORIENTED_EDGE ( 'NONE', *, *, #53170, .T. ) ;
#13267 = ORIENTED_EDGE ( 'NONE', *, *, #66134, .T. ) ;
#13268 = CARTESIAN_POINT ( 'NONE',  ( 0.000000000000000000, 36.75000000000000000, 4.000000000000000000 ) ) ;
#13269 = LINE ( 'NONE', #19942, #60064 ) ;
#13270 = ORIENTED_EDGE ( 'NONE', *, *, #728, .F. ) ;
#13271 = CARTESIAN_POINT ( 'NONE',  ( -5.598654528085806881, 110.8549999999999756, -7.705886871421374629 ) ) ;
#13272 = CARTESIAN_POINT ( 'NONE',  ( -0.3545099074454313715, 7.000000000000007994, -2.047617446692545640E-14 ) ) ;
#13273 = ORIENTED_EDGE ( 'NONE', *, *, #3137, .T. ) ;
#13274 = CARTESIAN_POINT ( 'NONE',  ( -82.85707362346616378, -5.598654528085803328, -7.705886871421366635 ) ) ;
#13275 = CARTESIAN_POINT ( 'NONE',  ( 8.082903768654762899, -1.105959442090949618E-15, 7.500000000000000000 ) ) ;
#13276 = CARTESIAN_POINT ( 'NONE',  ( -108.8949999999999960, 6.826472737025116366, 4.959722759717898555 ) ) ;
#13277 = VERTEX_POINT ( 'NONE', #55914 ) ;
#13278 = AXIS2_PLACEMENT_3D ( 'NONE', #58997, #48837, #26943 ) ;
#13279 = ORIENTED_EDGE ( 'NONE', *, *, #25182, .F. ) ;
#13280 = CARTESIAN_POINT ( 'NONE',  ( -0.4422543624570795529, 110.4999999999999716, -9.524999999999996803 ) ) ;
#13281 = CARTESIAN_POINT ( 'NONE',  ( -10.06570109130832336, -11.97273657574575090, -0.8246214522176227302 ) ) ;
#13282 = CARTESIAN_POINT ( 'NONE',  ( -44.99999999999977263, 147.4999999999999716, 10.00000000000000000 ) ) ;
#13283 = ORIENTED_EDGE ( 'NONE', *, *, #48807, .F. ) ;
#13284 = CARTESIAN_POINT ( 'NONE',  ( 2.607480562269076430, 143.7929263765338135, -8.025000000000000355 ) ) ;
#13285 = DIRECTION ( 'NONE',  ( -1.000000000000000000, 0.000000000000000000, 0.000000000000000000 ) ) ;
#13286 = DIRECTION ( 'NONE',  ( 0.000000000000000000, 0.000000000000000000, -1.000000000000000000 ) ) ;
#13287 = VECTOR ( 'NONE', #33239, 1000.000000000000000 ) ;
#13288 = SURFACE_SIDE_STYLE ('',( #18905 ) ) ;
#13289 = CARTESIAN_POINT ( 'NONE',  ( -141.0570736234661808, 0.000000000000000000, 9.524999999999991473 ) ) ;
#13290 = ORIENTED_EDGE ( 'NONE', *, *, #54481, .F. ) ;
#13291 = LINE ( 'NONE', #35470, #67836 ) ;
#13292 = ORIENTED_EDGE ( 'NONE', *, *, #62077, .F. ) ;
#13293 = CARTESIAN_POINT ( 'NONE',  ( -4.716976649647098618, 140.2570736234661410, 6.492361379858953008 ) ) ;
#13294 = CARTESIAN_POINT ( 'NONE',  ( -19.89974874213239886, 114.9999999999999574, 10.49999999999999645 ) ) ;
#13296 = AXIS2_PLACEMENT_3D ( 'NONE', #19131, #39954, #61359 ) ;
#13295 = CARTESIAN_POINT ( 'NONE',  ( -168.4429263765337907, -1.166476076187852838E-15, -9.524999999999991473 ) ) ;
#13297 = CARTESIAN_POINT ( 'NONE',  ( -135.8049999999999500, -8.437984349512085203, 5.166775262442717831E-16 ) ) ;
#13298 = CYLINDRICAL_SURFACE ( 'NONE', #17411, 5.499999999999985789 ) ;
#13299 = DIRECTION ( 'NONE',  ( -0.000000000000000000, 0.6691306063588591257, 0.7431448254773933559 ) ) ;
#13300 = ORIENTED_EDGE ( 'NONE', *, *, #59279, .T. ) ;
#13301 = EDGE_CURVE ( 'NONE', #10952, #55126, #29435, .T. ) ;
#13302 = DIRECTION ( 'NONE',  ( 0.000000000000000000, 0.000000000000000000, 1.000000000000000000 ) ) ;
#13303 = DIRECTION ( 'NONE',  ( -0.000000000000000000, -0.000000000000000000, 1.000000000000000000 ) ) ;
#13304 = FACE_OUTER_BOUND ( 'NONE', #22653, .T. ) ;
#13305 = ORIENTED_EDGE ( 'NONE', *, *, #50526, .T. ) ;
#13306 = AXIS2_PLACEMENT_3D ( 'NONE', #42619, #32022, #292 ) ;
#13307 = EDGE_LOOP ( 'NONE', ( #55244, #8023, #8783, #33447 ) ) ;
#13308 = CARTESIAN_POINT ( 'NONE',  ( -32.76851741822089537, -9.107254030097822195, -1.999999999999996225 ) ) ;
#13309 = DIRECTION ( 'NONE',  ( -7.080503983578803083E-17, -1.000000000000000000, 0.000000000000000000 ) ) ;
#13310 = DIRECTION ( 'NONE',  ( -1.000000000000000000, 0.000000000000000000, 0.000000000000000000 ) ) ;
#13311 = ORIENTED_EDGE ( 'NONE', *, *, #51136, .F. ) ;
#13312 = DIRECTION ( 'NONE',  ( -1.000000000000000000, 0.000000000000000000, 0.000000000000000000 ) ) ;
#13313 =( NAMED_UNIT ( * ) PLANE_ANGLE_UNIT ( ) SI_UNIT ( $, .RADIAN. ) );
#13314 = DIRECTION ( 'NONE',  ( 1.000000000000000000, 0.000000000000000000, 0.000000000000000000 ) ) ;
#13315 = SURFACE_STYLE_USAGE ( .BOTH. , #24225 ) ;
#13316 = CARTESIAN_POINT ( 'NONE',  ( -57.35707362346617799, 5.598654528085804216, 7.705886871421366635 ) ) ;
#13317 = CARTESIAN_POINT ( 'NONE',  ( 39.24999999999999289, 15.74999999999997513, -4.000000000000000000 ) ) ;
#13318 = SURFACE_SIDE_STYLE ('',( #55190 ) ) ;
#13319 = ORIENTED_EDGE ( 'NONE', *, *, #19846, .T. ) ;
#13320 = CARTESIAN_POINT ( 'NONE',  ( -74.59575606080316845, 36.31161697799826271, -9.993293536547614764 ) ) ;
#13321 = EDGE_CURVE ( 'NONE', #30278, #60536, #11621, .T. ) ;
#13323 =( GEOMETRIC_REPRESENTATION_CONTEXT ( 3 ) GLOBAL_UNCERTAINTY_ASSIGNED_CONTEXT ( ( #69297 ) ) GLOBAL_UNIT_ASSIGNED_CONTEXT ( ( #28097, #44365, #60468 ) ) REPRESENTATION_CONTEXT ( 'NONE', 'WORKASPACE' ) );
#13322 =( NAMED_UNIT ( * ) PLANE_ANGLE_UNIT ( ) SI_UNIT ( $, .RADIAN. ) );
#13324 = FILL_AREA_STYLE ('',( #3790 ) ) ;
#13325 = CARTESIAN_POINT ( 'NONE',  ( -97.70499999999998408, 2.607480562269073321, 8.024999999999991473 ) ) ;
#13326 = CARTESIAN_POINT ( 'NONE',  ( -26.79538245034556709, -8.499999999999996447, 1.000000000000000000 ) ) ;
#13327 = CARTESIAN_POINT ( 'NONE',  ( 179.4361977533490347, 0.9999999999999991118, -103.7004518695263044 ) ) ;
#13328 = SURFACE_SIDE_STYLE ('',( #61502 ) ) ;
#13329 = CIRCLE ( 'NONE', #35786, 4.999999999999997335 ) ;
#13330 = EDGE_CURVE ( 'NONE', #37089, #4040, #14858, .T. ) ;
#13331 = CARTESIAN_POINT ( 'NONE',  ( -101.3949999999999676, -6.826472737025113702, -4.959722759717900331 ) ) ;
#13332 = EDGE_CURVE ( 'NONE', #40021, #1731, #6671, .T. ) ;
#13333 = CARTESIAN_POINT ( 'NONE',  ( -8.102448949553181734, 117.6049999999999898, 5.886773742842747126 ) ) ;
#13334 = CARTESIAN_POINT ( 'NONE',  ( -75.74499999999999034, 4.716976649647094177, 6.492361379858945902 ) ) ;
#13335 = DIRECTION ( 'NONE',  ( 0.000000000000000000, 0.000000000000000000, 1.000000000000000000 ) ) ;
#13336 = PRESENTATION_STYLE_ASSIGNMENT (( #13695 ) ) ;
#13337 = AXIS2_PLACEMENT_3D ( 'NONE', #4747, #92, #26202 ) ;
#13338 = PRESENTATION_STYLE_ASSIGNMENT (( #4150 ) ) ;
#13339 = DIRECTION ( 'NONE',  ( -1.000000000000000000, 0.000000000000000000, 0.000000000000000000 ) ) ;
#13340 = ORIENTED_EDGE ( 'NONE', *, *, #63383, .T. ) ;
#13341 = ADVANCED_FACE ( 'NONE', ( #54852 ), #28109, .T. ) ;
#13342 = CARTESIAN_POINT ( 'NONE',  ( -113.2429263765338163, 5.598654528085804216, 7.705886871421366635 ) ) ;
#13343 = CARTESIAN_POINT ( 'NONE',  ( -138.2949999999999591, -2.607480562269069768, 8.024999999999991473 ) ) ;
#13344 = FILL_AREA_STYLE_COLOUR ( '', #66173 ) ;
#13345 = STYLED_ITEM ( 'NONE', ( #27936 ), #51101 ) ;
#13346 = VECTOR ( 'NONE', #58504, 1000.000000000000000 ) ;
#13347 = ADVANCED_FACE ( 'NONE', ( #34458 ), #68787, .T. ) ;
#13348 = DIRECTION ( 'NONE',  ( 0.000000000000000000, 0.000000000000000000, -1.000000000000000000 ) ) ;
#13349 = CARTESIAN_POINT ( 'NONE',  ( -174.1429263765338078, 5.598654528085800663, -7.705886871421367523 ) ) ;
#13350 = ORIENTED_EDGE ( 'NONE', *, *, #67041, .F. ) ;
#13351 = COLOUR_RGB ( '', 0.09019608, 0.27058824, 0.51372549) ;
#13352 = EDGE_LOOP ( 'NONE', ( #56978, #69105, #49028, #7508 ) ) ;
#13353 = LINE ( 'NONE', #4077, #31022 ) ;
#13354 = DIRECTION ( 'NONE',  ( -0.000000000000000000, -1.000000000000000000, -0.000000000000000000 ) ) ;
#13355 = DIRECTION ( 'NONE',  ( -0.000000000000000000, -0.000000000000000000, 1.000000000000000000 ) ) ;
#13356 = FACE_OUTER_BOUND ( 'NONE', #14020, .T. ) ;
#13357 = AXIS2_PLACEMENT_3D ( 'NONE', #16493, #21365, #26298 ) ;
#13358 = DIRECTION ( 'NONE',  ( 1.000000000000000000, -0.000000000000000000, 0.000000000000000000 ) ) ;
#13359 = ORIENTED_EDGE ( 'NONE', *, *, #53344, .T. ) ;
#13360 = CARTESIAN_POINT ( 'NONE',  ( -129.2049999999999841, -2.607480562269071545, -8.024999999999991473 ) ) ;
#13361 = EDGE_LOOP ( 'NONE', ( #57401, #26762, #40766, #18488 ) ) ;
#13362 = CARTESIAN_POINT ( 'NONE',  ( -121.1070736234661922, 8.102448949553171076, -5.886773742842744461 ) ) ;
#13363 = EDGE_CURVE ( 'NONE', #4175, #3674, #23225, .T. ) ;
#13364 = ORIENTED_EDGE ( 'NONE', *, *, #14226, .F. ) ;
#13365 = FACE_OUTER_BOUND ( 'NONE', #43722, .T. ) ;
#13366 = CARTESIAN_POINT ( 'NONE',  ( 0.000000000000000000, 36.74999999999999289, 4.000000000000000000 ) ) ;
#13367 = ORIENTED_EDGE ( 'NONE', *, *, #38841, .T. ) ;
#13368 = LINE ( 'NONE', #8111, #45061 ) ;
#13369 = EDGE_CURVE ( 'NONE', #48755, #10834, #12289, .T. ) ;
#13370 = CARTESIAN_POINT ( 'NONE',  ( 10.01517768586949231, 144.6949999999999932, 1.839758294383810543E-15 ) ) ;
#13371 = ORIENTED_EDGE ( 'NONE', *, *, #30604, .F. ) ;
#13372 = DIRECTION ( 'NONE',  ( 0.000000000000000000, 0.6691306063588592368, -0.7431448254773934670 ) ) ;
#13373 = CARTESIAN_POINT ( 'NONE',  ( -3.094860106618432471, 140.7049999999999557, -9.525000000000000355 ) ) ;
#13374 = FILL_AREA_STYLE ('',( #9169 ) ) ;
#13375 = AXIS2_PLACEMENT_3D ( 'NONE', #55739, #59702, #13155 ) ;
#13376 = DIRECTION ( 'NONE',  ( -1.000000000000000000, 0.000000000000000000, 0.000000000000000000 ) ) ;
#13377 = ORIENTED_EDGE ( 'NONE', *, *, #23700, .T. ) ;
#13378 = CARTESIAN_POINT ( 'NONE',  ( 7.632228543268608334, 116.3429263765338106, -2.479861379858951942 ) ) ;
#13379 =( NAMED_UNIT ( * ) SI_UNIT ( $, .STERADIAN. ) SOLID_ANGLE_UNIT ( ) );
#13380 = AXIS2_PLACEMENT_3D ( 'NONE', #61744, #49851, #8326 ) ;
#13381 = LINE ( 'NONE', #56660, #40776 ) ;
#13382 = DIRECTION ( 'NONE',  ( -0.000000000000000000, -0.000000000000000000, -1.000000000000000000 ) ) ;
#13383 = ORIENTED_EDGE ( 'NONE', *, *, #1274, .F. ) ;
#13384 = MECHANICAL_DESIGN_GEOMETRIC_PRESENTATION_REPRESENTATION (  '', ( #65050 ), #62888 ) ;
#13385 = CARTESIAN_POINT ( 'NONE',  ( 41.45361433042954502, 107.0152407614178856, 3.499999999999999556 ) ) ;
#13386 = ORIENTED_EDGE ( 'NONE', *, *, #48167, .T. ) ;
#13387 = CARTESIAN_POINT ( 'NONE',  ( 15.98999599679679839, 117.9999999999999716, 9.500000000000000000 ) ) ;
#13388 = AXIS2_PLACEMENT_3D ( 'NONE', #4033, #4365, #47014 ) ;
#13389 = CARTESIAN_POINT ( 'NONE',  ( 20.46001754528041161, 114.7916627990982192, 10.31416700829639588 ) ) ;
#13390 = CARTESIAN_POINT ( 'NONE',  ( 30.25000000000000711, 18.74999999999997868, -3.750000000000000000 ) ) ;
#13391 = CARTESIAN_POINT ( 'NONE',  ( -158.1550000000000011, 7.632228543268600340, 2.479861379858949277 ) ) ;
#13392 = ORIENTED_EDGE ( 'NONE', *, *, #38801, .F. ) ;
#13393 = AXIS2_PLACEMENT_3D ( 'NONE', #18200, #39686, #34709 ) ;
#13394 =( NAMED_UNIT ( * ) SI_UNIT ( $, .STERADIAN. ) SOLID_ANGLE_UNIT ( ) );
#13395 = CIRCLE ( 'NONE', #17924, 0.4999999999999993339 ) ;
#13396 = CARTESIAN_POINT ( 'NONE',  ( -75.50000000000000000, 64.49137674618943095, -41.30495168499704306 ) ) ;
#13397 = CARTESIAN_POINT ( 'NONE',  ( 45.54151037965925752, 9.791825115386158629, -6.500000000000000888 ) ) ;
#13398 = DIRECTION ( 'NONE',  ( 1.000000000000000000, 0.000000000000000000, 0.000000000000000000 ) ) ;
#13399 =( BOUNDED_CURVE ( )  B_SPLINE_CURVE ( 2, ( #68436, #14628, #24804, #41041, #9359, #41735, #31473, #3317, #63160, #26203, #10048 ),
 .UNSPECIFIED., .F., .F. ) 
 B_SPLINE_CURVE_WITH_KNOTS ( ( 3, 2, 2, 2, 2, 3 ),
 ( 0.2499999999999940603, 0.2521739130434722531, 0.2543478260869504459, 0.2565217391304287498, 0.2586956521739069426, 0.2608695652173851354 ),
 .UNSPECIFIED. ) 
 CURVE ( )  GEOMETRIC_REPRESENTATION_ITEM ( )  RATIONAL_B_SPLINE_CURVE ( ( 1.000000000000133671, 0.9510565162950198603, 1.000000000000000000, 0.9510565162951535312, 1.000000000000000000, 0.9510565162951535312, 1.000000000000000000, 0.9510565162951535312, 1.000000000000000000, 0.9510565162952923091, 0.9999999999998612221 ) ) 
 REPRESENTATION_ITEM ( '' )  );
#13400 = ORIENTED_EDGE ( 'NONE', *, *, #33752, .F. ) ;
#13401 = ORIENTED_EDGE ( 'NONE', *, *, #64162, .F. ) ;
#13402 = CARTESIAN_POINT ( 'NONE',  ( -47.75499999999999545, 4.716976649647091513, -6.492361379858946790 ) ) ;
#13403 = CARTESIAN_POINT ( 'NONE',  ( 0.000000000000000000, 152.9429263765338192, -8.025000000000000355 ) ) ;
#13404 = CARTESIAN_POINT ( 'NONE',  ( -80.30499999999999261, 8.437984349512085203, -1.550032578732815448E-15 ) ) ;
#13405 = EDGE_LOOP ( 'NONE', ( #31380, #36789, #14883, #57577 ) ) ;
#13406 = EDGE_CURVE ( 'NONE', #19259, #30231, #33760, .T. ) ;
#13407 = PRESENTATION_LAYER_ASSIGNMENT (  '', '', ( #53825 ) ) ;
#13408 = FILL_AREA_STYLE_COLOUR ( '', #1402 ) ;
#13409 = CYLINDRICAL_SURFACE ( 'NONE', #58919, 8.025000000000000355 ) ;
#13410 = EDGE_CURVE ( 'NONE', #1680, #34386, #63146, .T. ) ;
#13411 = CARTESIAN_POINT ( 'NONE',  ( -75.00000000000000000, 9.581381838473308932, -6.370847823861820025 ) ) ;
#13412 = ORIENTED_EDGE ( 'NONE', *, *, #24456, .F. ) ;
#13413 = VECTOR ( 'NONE', #27236, 1000.000000000000000 ) ;
#13415 = FILL_AREA_STYLE_COLOUR ( '', #7829 ) ;
#13414 = DIRECTION ( 'NONE',  ( 0.000000000000000000, 0.000000000000000000, -1.000000000000000000 ) ) ;
#13416 = ADVANCED_FACE ( 'NONE', ( #50304 ), #29156, .T. ) ;
#13417 = CARTESIAN_POINT ( 'NONE',  ( 10.01517768586949231, 141.6949999999999363, 1.839758294383810543E-15 ) ) ;
#13418 = CARTESIAN_POINT ( 'NONE',  ( -103.9449999999999932, -9.827790563157499189E-16, -8.024999999999991473 ) ) ;
#13419 = CARTESIAN_POINT ( 'NONE',  ( -14.95322863490701870, 69.00000000000000000, 6.349999999999997868 ) ) ;
#13420 =( BOUNDED_CURVE ( )  B_SPLINE_CURVE ( 2, ( #10185, #25995, #20744, #4535, #48547, #52760, #32312, #36950, #58360, #47523, #5229 ),
 .UNSPECIFIED., .F., .F. ) 
 B_SPLINE_CURVE_WITH_KNOTS ( ( 3, 2, 2, 2, 2, 3 ),
 ( 0.3823529411764706176, 0.3882352941176471228, 0.3941176470588235725, 0.4000000000000001332, 0.4058823529411765829, 0.4117647058823530326 ),
 .UNSPECIFIED. ) 
 CURVE ( )  GEOMETRIC_REPRESENTATION_ITEM ( )  RATIONAL_B_SPLINE_CURVE ( ( 0.9999999999999995559, 0.9510565162951539753, 1.000000000000000000, 0.9510565162951535312, 1.000000000000000000, 0.9510565162951535312, 1.000000000000000000, 0.9510565162951535312, 1.000000000000000000, 0.9510565162951526430, 1.000000000000000888 ) ) 
 REPRESENTATION_ITEM ( '' )  );
#13422 = PRESENTATION_STYLE_ASSIGNMENT (( #22962 ) ) ;
#13421 = CARTESIAN_POINT ( 'NONE',  ( -97.10707362346616378, 8.102448949553172852, -5.886773742842744461 ) ) ;
#13423 =( GEOMETRIC_REPRESENTATION_CONTEXT ( 3 ) GLOBAL_UNCERTAINTY_ASSIGNED_CONTEXT ( ( #17101 ) ) GLOBAL_UNIT_ASSIGNED_CONTEXT ( ( #62400, #46259, #57468 ) ) REPRESENTATION_CONTEXT ( 'NONE', 'WORKASPACE' ) );
#13424 = CARTESIAN_POINT ( 'NONE',  ( -145.4929263765338021, -8.102448949553172852, 5.886773742842742685 ) ) ;
#13425 = CARTESIAN_POINT ( 'NONE',  ( -166.4950000000000045, 6.826472737025113702, -4.959722759717902107 ) ) ;
#13426 = AXIS2_PLACEMENT_3D ( 'NONE', #3242, #25101, #56774 ) ;
#13427 = EDGE_CURVE ( 'NONE', #6296, #34825, #17129, .T. ) ;
#13428 = DIRECTION ( 'NONE',  ( -0.000000000000000000, -0.000000000000000000, -1.000000000000000000 ) ) ;
#13429 = PRESENTATION_LAYER_ASSIGNMENT (  '', '', ( #11230 ) ) ;
#13430 = STYLED_ITEM ( 'NONE', ( #17743 ), #10848 ) ;
#13431 =( NAMED_UNIT ( * ) PLANE_ANGLE_UNIT ( ) SI_UNIT ( $, .RADIAN. ) );
#13432 = ORIENTED_EDGE ( 'NONE', *, *, #61433, .F. ) ;
#13433 = CARTESIAN_POINT ( 'NONE',  ( -4.716976649647098618, 130.1429263765338362, 6.492361379858953008 ) ) ;
#13434 = ORIENTED_EDGE ( 'NONE', *, *, #43281, .F. ) ;
#13435 = VECTOR ( 'NONE', #57856, 1000.000000000000000 ) ;
#13436 =( GEOMETRIC_REPRESENTATION_CONTEXT ( 3 ) GLOBAL_UNCERTAINTY_ASSIGNED_CONTEXT ( ( #60212 ) ) GLOBAL_UNIT_ASSIGNED_CONTEXT ( ( #63756, #58840, #43061 ) ) REPRESENTATION_CONTEXT ( 'NONE', 'WORKASPACE' ) );
#13437 = CIRCLE ( 'NONE', #62839, 8.025000000000000355 ) ;
#13438 = CYLINDRICAL_SURFACE ( 'NONE', #15896, 0.5000000000000004441 ) ;
#13439 = CARTESIAN_POINT ( 'NONE',  ( -45.00000000000000711, 7.768687147774683943, 6.500000000000007105 ) ) ;
#13440 = CARTESIAN_POINT ( 'NONE',  ( 0.000000000000000000, -1.999999999999995337, 5.000000000000000000 ) ) ;
#13441 = CIRCLE ( 'NONE', #1023, 5.000000000000000888 ) ;
#13442 = DIRECTION ( 'NONE',  ( 0.000000000000000000, 1.000000000000000000, 0.000000000000000000 ) ) ;
#13443 = VERTEX_POINT ( 'NONE', #18293 ) ;
#13444 = CARTESIAN_POINT ( 'NONE',  ( -158.4549999999999841, 7.632228543268599452, -2.479861379858951942 ) ) ;
#13445 = ORIENTED_EDGE ( 'NONE', *, *, #47865, .T. ) ;
#13446 = CARTESIAN_POINT ( 'NONE',  ( -20.86636340060661610, 115.0297054428233707, -10.00000000000000000 ) ) ;
#13447 = SURFACE_STYLE_USAGE ( .BOTH. , #61620 ) ;
#13448 = ORIENTED_EDGE ( 'NONE', *, *, #61239, .T. ) ;
#13449 = MECHANICAL_DESIGN_GEOMETRIC_PRESENTATION_REPRESENTATION (  '', ( #33643 ), #16852 ) ;
#13450 = FILL_AREA_STYLE ('',( #56734 ) ) ;
#13451 = FILL_AREA_STYLE_COLOUR ( '', #67994 ) ;
#13452 = CARTESIAN_POINT ( 'NONE',  ( -5.598654528085808657, 113.6449999999999818, 7.705886871421373741 ) ) ;
#13453 = EDGE_LOOP ( 'NONE', ( #40457, #3566, #9454, #20309, #28493, #54675 ) ) ;
#13454 = DIRECTION ( 'NONE',  ( -0.9968761159932768567, 0.07898106964430656740, 0.000000000000000000 ) ) ;
#13455 = DIRECTION ( 'NONE',  ( 1.000000000000000000, 0.000000000000000000, 0.000000000000000000 ) ) ;
#13456 = CARTESIAN_POINT ( 'NONE',  ( -77.60499999999997556, 6.826472737025113702, -4.959722759717902107 ) ) ;
#13457 = LINE ( 'NONE', #29989, #67785 ) ;
#13458 = CARTESIAN_POINT ( 'NONE',  ( -9.058813317711338797, 141.4549999999999841, 2.943386871421373563 ) ) ;
#13459 = AXIS2_PLACEMENT_3D ( 'NONE', #62554, #46078, #58009 ) ;
#13460 = SURFACE_STYLE_FILL_AREA ( #18750 ) ;
#13461 = SURFACE_STYLE_USAGE ( .BOTH. , #45180 ) ;
#13462 = DIRECTION ( 'NONE',  ( 0.000000000000000000, -1.000000000000000000, 0.000000000000000000 ) ) ;
#13463 = ORIENTED_EDGE ( 'NONE', *, *, #36212, .F. ) ;
#13464 =( NAMED_UNIT ( * ) SI_UNIT ( $, .STERADIAN. ) SOLID_ANGLE_UNIT ( ) );
#13465 = AXIS2_PLACEMENT_3D ( 'NONE', #25500, #10040, #65564 ) ;
#13467 = CARTESIAN_POINT ( 'NONE',  ( -50.24499999999998323, -4.716976649647093289, -6.492361379858945902 ) ) ;
#13466 = PRESENTATION_LAYER_ASSIGNMENT (  '', '', ( #23564 ) ) ;
#13468 = ORIENTED_EDGE ( 'NONE', *, *, #47772, .F. ) ;
#13469 = LINE ( 'NONE', #40592, #45240 ) ;
#13470 = FILL_AREA_STYLE ('',( #61643 ) ) ;
#13471 = CARTESIAN_POINT ( 'NONE',  ( -45.00000000000000000, 7.966012280117821476, -7.000000003579909702 ) ) ;
#13472 = CARTESIAN_POINT ( 'NONE',  ( 72.50000000000000000, 14.49137674618942562, -9.500000000000000000 ) ) ;
#13473 = ORIENTED_EDGE ( 'NONE', *, *, #16945, .T. ) ;
#13474 = DIRECTION ( 'NONE',  ( 0.000000000000000000, 0.000000000000000000, 1.000000000000000000 ) ) ;
#13475 = CARTESIAN_POINT ( 'NONE',  ( -54.89499999999997470, 6.826472737025115478, 4.959722759717899443 ) ) ;
#13476 = DIRECTION ( 'NONE',  ( 1.000000000000000000, 0.000000000000000000, 0.000000000000000000 ) ) ;
#13477 = ORIENTED_EDGE ( 'NONE', *, *, #15183, .F. ) ;
#13478 = CARTESIAN_POINT ( 'NONE',  ( -108.2049999999999983, -2.607480562269071545, -8.024999999999991473 ) ) ;
#13479 = ORIENTED_EDGE ( 'NONE', *, *, #2130, .F. ) ;
#13480 = CARTESIAN_POINT ( 'NONE',  ( 7.750000000000000000, 33.99999999999998579, 3.750000000000000000 ) ) ;
#13481 = EDGE_CURVE ( 'NONE', #42335, #44124, #56408, .T. ) ;
#13482 = FACE_OUTER_BOUND ( 'NONE', #37576, .T. ) ;
#13483 = AXIS2_PLACEMENT_3D ( 'NONE', #47573, #37350, #5607 ) ;
#13484 = CARTESIAN_POINT ( 'NONE',  ( -141.5070736234661126, 8.102448949553176405, 5.886773742842740909 ) ) ;
#13485 = CIRCLE ( 'NONE', #26913, 16.00000000000000000 ) ;
#13486 = DIRECTION ( 'NONE',  ( -0.000000000000000000, 1.000000000000000000, -0.000000000000000000 ) ) ;
#13487 = CARTESIAN_POINT ( 'NONE',  ( 3.094860106618435136, 139.2949999999999875, -9.525000000000000355 ) ) ;
#13488 = CARTESIAN_POINT ( 'NONE',  ( -89.45707362346618652, -9.058813317711329915, 2.943386871421371787 ) ) ;
#13489 = AXIS2_PLACEMENT_3D ( 'NONE', #54611, #19041, #20088 ) ;
#13490 = CARTESIAN_POINT ( 'NONE',  ( -95.99292637653378790, 8.102448949553172852, -5.886773742842744461 ) ) ;
#13491 = CARTESIAN_POINT ( 'NONE',  ( 14.59999999999998721, 11.99999999999999289, 4.000000000000000000 ) ) ;
#13492 = DIRECTION ( 'NONE',  ( -0.000000000000000000, 1.000000000000000000, -0.000000000000000000 ) ) ;
#13493 = CARTESIAN_POINT ( 'NONE',  ( 4.716976649647099507, 120.7570736234661553, -6.492361379858953008 ) ) ;
#13494 = CARTESIAN_POINT ( 'NONE',  ( -117.2049999999999841, -2.607480562269071545, -8.024999999999991473 ) ) ;
#13495 = EDGE_CURVE ( 'NONE', #51146, #7911, #2425, .T. ) ;
#13496 = CARTESIAN_POINT ( 'NONE',  ( -133.9449999999999932, -9.827790563157499189E-16, -8.024999999999991473 ) ) ;
#13497 = EDGE_CURVE ( 'NONE', #22057, #59357, #66835, .T. ) ;
#13498 = AXIS2_PLACEMENT_3D ( 'NONE', #67884, #14764, #30557 ) ;
#13499 = CARTESIAN_POINT ( 'NONE',  ( -115.9449999999999932, -9.827790563157499189E-16, -8.024999999999991473 ) ) ;
#13500 = EDGE_CURVE ( 'NONE', #15255, #14152, #20362, .T. ) ;
#13501 = DIRECTION ( 'NONE',  ( 0.000000000000000000, 0.000000000000000000, -1.000000000000000000 ) ) ;
#13502 = VERTEX_POINT ( 'NONE', #23902 ) ;
#13503 = STYLED_ITEM ( 'NONE', ( #16508 ), #16648 ) ;
#13504 = CYLINDRICAL_SURFACE ( 'NONE', #25735, 0.2500000000000002220 ) ;
#13505 = CARTESIAN_POINT ( 'NONE',  ( 92.41620014002536720, 5.000000000000000000, -24.00402776293825369 ) ) ;
#13506 = ADVANCED_FACE ( 'NONE', ( #36228 ), #8440, .F. ) ;
#13507 = DIRECTION ( 'NONE',  ( -0.000000000000000000, 1.000000000000000000, -0.000000000000000000 ) ) ;
#13508 = CARTESIAN_POINT ( 'NONE',  ( -168.2929263765337851, 3.094860106618428031, -9.524999999999993250 ) ) ;
#13509 = VECTOR ( 'NONE', #67410, 1000.000000000000000 ) ;
#13510 = CARTESIAN_POINT ( 'NONE',  ( -52.94499999999999318, -9.827790563157499189E-16, -8.024999999999991473 ) ) ;
#13511 = EDGE_CURVE ( 'NONE', #29168, #10038, #51821, .T. ) ;
#13512 = FACE_OUTER_BOUND ( 'NONE', #8372, .T. ) ;
#13513 = CARTESIAN_POINT ( 'NONE',  ( 71.18918918918917882, 14.09971791521133255, 7.000000000000000000 ) ) ;
#13514 = DIRECTION ( 'NONE',  ( 7.304098846218139598E-16, 0.000000000000000000, -1.000000000000000000 ) ) ;
#13515 = CARTESIAN_POINT ( 'NONE',  ( -9.827790563157511022E-16, 136.4429263765338192, 8.025000000000000355 ) ) ;
#13516 = ORIENTED_EDGE ( 'NONE', *, *, #67271, .F. ) ;
#13517 = AXIS2_PLACEMENT_3D ( 'NONE', #61833, #18923, #3050 ) ;
#13518 = CARTESIAN_POINT ( 'NONE',  ( -86.84292637653381064, 9.058813317711329915, -2.943386871421373119 ) ) ;
#13519 = CONTEXT_DEPENDENT_SHAPE_REPRESENTATION ( #28463, #28857 ) ;
#13520 = DIRECTION ( 'NONE',  ( 1.300977106640434891E-16, 0.000000000000000000, 1.000000000000000000 ) ) ;
#13521 =( BOUNDED_CURVE ( )  B_SPLINE_CURVE ( 2, ( #6798, #66236, #12770, #55696, #18062, #12074, #21966, #17732, #50090, #28225, #39547 ),
 .UNSPECIFIED., .F., .F. ) 
 B_SPLINE_CURVE_WITH_KNOTS ( ( 3, 2, 2, 2, 2, 3 ),
 ( 0.7934782608695651884, 0.7956521739130434367, 0.7978260869565216851, 0.8000000000000000444, 0.8021739130434782927, 0.8043478260869565410 ),
 .UNSPECIFIED. ) 
 CURVE ( )  GEOMETRIC_REPRESENTATION_ITEM ( )  RATIONAL_B_SPLINE_CURVE ( ( 1.000000000000000000, 0.9510565162951535312, 1.000000000000000000, 0.9510565162951535312, 1.000000000000000000, 0.9510565162951535312, 1.000000000000000000, 0.9510565162951535312, 1.000000000000000000, 0.9510565162951535312, 1.000000000000000000 ) ) 
 REPRESENTATION_ITEM ( '' )  );
#13522 = CARTESIAN_POINT ( 'NONE',  ( -60.00000000000000000, -2.024042244987997205E-14, 11.50000000000000000 ) ) ;
#13523 =( GEOMETRIC_REPRESENTATION_CONTEXT ( 3 ) GLOBAL_UNCERTAINTY_ASSIGNED_CONTEXT ( ( #27596 ) ) GLOBAL_UNIT_ASSIGNED_CONTEXT ( ( #6669, #28108, #1349 ) ) REPRESENTATION_CONTEXT ( 'NONE', 'WORKASPACE' ) );
#13524 = TOROIDAL_SURFACE ( 'NONE', #49657, 0.5000000000000000000, 0.2500000000000000000 ) ;
#13525 = DIRECTION ( 'NONE',  ( 0.000000000000000000, 0.000000000000000000, 1.000000000000000000 ) ) ;
#13526 = CARTESIAN_POINT ( 'NONE',  ( -41.03152803655121517, 107.9804733858014032, 3.206774974534162048 ) ) ;
#13527 = CARTESIAN_POINT ( 'NONE',  ( -124.5570736234661808, -1.166476076187852838E-15, -9.524999999999991473 ) ) ;
#13528 = EDGE_LOOP ( 'NONE', ( #7285, #5313, #68088, #20437 ) ) ;
#13529 = DIRECTION ( 'NONE',  ( 0.000000000000000000, 0.000000000000000000, -1.000000000000000000 ) ) ;
#13530 = CARTESIAN_POINT ( 'NONE',  ( -15.48999599679679662, 146.4999999999999716, -9.500000000000000000 ) ) ;
#13531 = FILL_AREA_STYLE_COLOUR ( '', #38585 ) ;
#13532 = PRESENTATION_LAYER_ASSIGNMENT (  '', '', ( #36010 ) ) ;
#13533 = EDGE_LOOP ( 'NONE', ( #27707, #43286, #29377, #27288 ) ) ;
#13534 = DIRECTION ( 'NONE',  ( 0.000000000000000000, 0.000000000000000000, -1.000000000000000000 ) ) ;
#13535 = VECTOR ( 'NONE', #44647, 1000.000000000000000 ) ;
#13536 = CARTESIAN_POINT ( 'NONE',  ( -9.827790563157511022E-16, 137.5570736234661808, 8.025000000000000355 ) ) ;
#13538 =( GEOMETRIC_REPRESENTATION_CONTEXT ( 3 ) GLOBAL_UNCERTAINTY_ASSIGNED_CONTEXT ( ( #40501 ) ) GLOBAL_UNIT_ASSIGNED_CONTEXT ( ( #1882, #60666, #18482 ) ) REPRESENTATION_CONTEXT ( 'NONE', 'WORKASPACE' ) );
#13537 = DIRECTION ( 'NONE',  ( -0.000000000000000000, 1.000000000000000000, -0.000000000000000000 ) ) ;
#13539 = FILL_AREA_STYLE_COLOUR ( '', #67625 ) ;
#13540 = PRESENTATION_LAYER_ASSIGNMENT (  '', '', ( #12431 ) ) ;
#13541 = PRESENTATION_STYLE_ASSIGNMENT (( #55773 ) ) ;
#13542 = ORIENTED_EDGE ( 'NONE', *, *, #33203, .F. ) ;
#13543 = DIRECTION ( 'NONE',  ( 1.000000000000000000, 1.156482317317866302E-16, 0.000000000000000000 ) ) ;
#13544 = CARTESIAN_POINT ( 'NONE',  ( 6.750018943533633298, 42.91041480136897945, 27.90050555725692405 ) ) ;
#13545 = PRESENTATION_LAYER_ASSIGNMENT (  '', '', ( #28134 ) ) ;
#13546 = SURFACE_STYLE_FILL_AREA ( #61040 ) ;
#13547 = CARTESIAN_POINT ( 'NONE',  ( -83.39499999999998181, -6.826472737025115478, -4.959722759717899443 ) ) ;
#13548 = ORIENTED_EDGE ( 'NONE', *, *, #49481, .T. ) ;
#13549 =( GEOMETRIC_REPRESENTATION_CONTEXT ( 3 ) GLOBAL_UNCERTAINTY_ASSIGNED_CONTEXT ( ( #9502 ) ) GLOBAL_UNIT_ASSIGNED_CONTEXT ( ( #1539, #44560, #33941 ) ) REPRESENTATION_CONTEXT ( 'NONE', 'WORKASPACE' ) );
#13550 = MECHANICAL_DESIGN_GEOMETRIC_PRESENTATION_REPRESENTATION (  '', ( #26989 ), #59601 ) ;
#13551 = LINE ( 'NONE', #31730, #65939 ) ;
#13552 = CARTESIAN_POINT ( 'NONE',  ( -30.38025804287905629, -8.499999999999996447, 8.000000000000000000 ) ) ;
#13553 = UNCERTAINTY_MEASURE_WITH_UNIT (LENGTH_MEASURE( 1.000000000000000082E-05 ), #25679, 'distance_accuracy_value', 'NONE');
#13554 = ORIENTED_EDGE ( 'NONE', *, *, #48169, .T. ) ;
#13555 = CARTESIAN_POINT ( 'NONE',  ( -76.19292637653380496, -10.01517768586948698, 6.132527647946031529E-16 ) ) ;
#13556 = COLOUR_RGB ( '', 0.72549020, 0.75294118, 0.79215686) ;
#13557 = CARTESIAN_POINT ( 'NONE',  ( 66.49999999999998579, 33.74999999999999289, -3.750000000000000000 ) ) ;
#13558 = ORIENTED_EDGE ( 'NONE', *, *, #68972, .T. ) ;
#13560 = ORIENTED_EDGE ( 'NONE', *, *, #57741, .T. ) ;
#13559 = EDGE_CURVE ( 'NONE', #3068, #20313, #34930, .T. ) ;
#13561 = CARTESIAN_POINT ( 'NONE',  ( -60.00000000000000000, -2.024042244987997205E-14, 9.500000000000000000 ) ) ;
#13562 =( NAMED_UNIT ( * ) SI_UNIT ( $, .STERADIAN. ) SOLID_ANGLE_UNIT ( ) );
#13563 =( NAMED_UNIT ( * ) PLANE_ANGLE_UNIT ( ) SI_UNIT ( $, .RADIAN. ) );
#13564 = CARTESIAN_POINT ( 'NONE',  ( -174.2070736234661581, 3.094860106618433360, 9.524999999999991473 ) ) ;
#13565 = AXIS2_PLACEMENT_3D ( 'NONE', #1943, #50908, #1621 ) ;
#13566 = FILL_AREA_STYLE ('',( #3320 ) ) ;
#13567 = CARTESIAN_POINT ( 'NONE',  ( 5.598654528085809545, 112.1449999999999818, -7.705886871421373741 ) ) ;
#13568 = EDGE_CURVE ( 'NONE', #33368, #51912, #49548, .T. ) ;
#13569 = CARTESIAN_POINT ( 'NONE',  ( -113.6070736234661780, -8.102448949553172852, 5.886773742842742685 ) ) ;
#13570 = CARTESIAN_POINT ( 'NONE',  ( -183.2934834974413718, 1.440814635842406100, -9.147492737475964475 ) ) ;
#13571 = VECTOR ( 'NONE', #40441, 1000.000000000000000 ) ;
#13572 = DIRECTION ( 'NONE',  ( 1.000000000000000000, 0.000000000000000000, 0.000000000000000000 ) ) ;
#13573 = VERTEX_POINT ( 'NONE', #3081 ) ;
#13574 = LINE ( 'NONE', #56492, #32905 ) ;
#13575 = ADVANCED_FACE ( 'NONE', ( #45747 ), #40811, .F. ) ;
#13576 = DIRECTION ( 'NONE',  ( 0.000000000000000000, 0.000000000000000000, -1.000000000000000000 ) ) ;
#13577 = CARTESIAN_POINT ( 'NONE',  ( 31.00000000000002132, 42.00000000000000000, 75.00000000000000000 ) ) ;
#13578 = FACE_OUTER_BOUND ( 'NONE', #59220, .T. ) ;
#13579 = CARTESIAN_POINT ( 'NONE',  ( -153.6549999999999727, -7.632228543268600340, -2.479861379858950166 ) ) ;
#13580 = DIRECTION ( 'NONE',  ( 0.000000000000000000, 1.000000000000000000, 0.000000000000000000 ) ) ;
#13581 = CARTESIAN_POINT ( 'NONE',  ( -1.601699666116353837, 110.6836774114466664, -9.211824715481125025 ) ) ;
#13582 = STYLED_ITEM ( 'NONE', ( #67527 ), #21929 ) ;
#13583 = CARTESIAN_POINT ( 'NONE',  ( -160.0449999999999875, 7.632228543268600340, 2.479861379858949277 ) ) ;
#13584 = ADVANCED_FACE ( 'NONE', ( #30546 ), #47329, .F. ) ;
#13585 = CARTESIAN_POINT ( 'NONE',  ( -152.8449999999999989, -7.632228543268599452, 2.479861379858951054 ) ) ;
#13586 = VERTEX_POINT ( 'NONE', #61871 ) ;
#13587 = PRESENTATION_LAYER_ASSIGNMENT (  '', '', ( #7975 ) ) ;
#13588 = SURFACE_STYLE_USAGE ( .BOTH. , #9026 ) ;
#13589 = EDGE_CURVE ( 'NONE', #21322, #9702, #21054, .T. ) ;
#13590 = CARTESIAN_POINT ( 'NONE',  ( -121.9429263765338050, 0.000000000000000000, 9.524999999999991473 ) ) ;
#13591 = CARTESIAN_POINT ( 'NONE',  ( -62.60499999999998266, 6.826472737025113702, -4.959722759717902107 ) ) ;
#13592 = AXIS2_PLACEMENT_3D ( 'NONE', #57945, #46738, #57580 ) ;
#13593 = CARTESIAN_POINT ( 'NONE',  ( -167.0929263765340238, 3.094860106622062901, 9.524999999997353584 ) ) ;
#13594 = CARTESIAN_POINT ( 'NONE',  ( -75.89499999999998181, 6.826472737025115478, 4.959722759717899443 ) ) ;
#13595 = CARTESIAN_POINT ( 'NONE',  ( 3.094860106618431583, 145.2049999999999272, 9.525000000000000355 ) ) ;
#13596 = DIRECTION ( 'NONE',  ( 0.000000000000000000, 0.000000000000000000, 1.000000000000000000 ) ) ;
#13597 = AXIS2_PLACEMENT_3D ( 'NONE', #55873, #45710, #28781 ) ;
#13598 =( NAMED_UNIT ( * ) SI_UNIT ( $, .STERADIAN. ) SOLID_ANGLE_UNIT ( ) );
#13599 = UNCERTAINTY_MEASURE_WITH_UNIT (LENGTH_MEASURE( 1.000000000000000082E-05 ), #10340, 'distance_accuracy_value', 'NONE');
#13600 = AXIS2_PLACEMENT_3D ( 'NONE', #32460, #27528, #7135 ) ;
#13601 = ADVANCED_FACE ( 'NONE', ( #21651 ), #64578, .T. ) ;
#13602 = CARTESIAN_POINT ( 'NONE',  ( -160.5570736234661808, -1.166476076187852838E-15, -9.524999999999991473 ) ) ;
#13603 = CARTESIAN_POINT ( 'NONE',  ( -58.75000000000000000, -13.99999999999999822, 15.00000000000000178 ) ) ;
#13604 = DIRECTION ( 'NONE',  ( 0.000000000000000000, 0.000000000000000000, -1.000000000000000000 ) ) ;
#13605 = MECHANICAL_DESIGN_GEOMETRIC_PRESENTATION_REPRESENTATION (  '', ( #20346 ), #47360 ) ;
#13606 = CARTESIAN_POINT ( 'NONE',  ( 24.00000000000000355, 37.00000000000000000, 3.000000000000000000 ) ) ;
#13607 = AXIS2_PLACEMENT_3D ( 'NONE', #3140, #13758, #20418 ) ;
#13608 = DIRECTION ( 'NONE',  ( 0.000000000000000000, 0.000000000000000000, 1.000000000000000000 ) ) ;
#13609 = CARTESIAN_POINT ( 'NONE',  ( -119.6929263765338050, 10.01517768586948698, -1.839758294383808966E-15 ) ) ;
#13610 =( LENGTH_UNIT ( ) NAMED_UNIT ( * ) SI_UNIT ( .MILLI., .METRE. ) );
#13611 = ORIENTED_EDGE ( 'NONE', *, *, #49053, .F. ) ;
#13612 = ORIENTED_EDGE ( 'NONE', *, *, #32613, .F. ) ;
#13613 = TOROIDAL_SURFACE ( 'NONE', #21506, 27.49999999999999645, 0.5000000000000000000 ) ;
#13615 = UNCERTAINTY_MEASURE_WITH_UNIT (LENGTH_MEASURE( 1.000000000000000082E-05 ), #16571, 'distance_accuracy_value', 'NONE');
#13614 = SURFACE_STYLE_FILL_AREA ( #3011 ) ;
#13616 = ADVANCED_FACE ( 'NONE', ( #37281 ), #42549, .T. ) ;
#13617 = AXIS2_PLACEMENT_3D ( 'NONE', #62476, #18184, #67770 ) ;
#13618 = CARTESIAN_POINT ( 'NONE',  ( -44.99999999999999289, 9.708372675170620525, 6.100541755698618118 ) ) ;
#13619 = ORIENTED_EDGE ( 'NONE', *, *, #56619, .T. ) ;
#13620 = VECTOR ( 'NONE', #32807, 1000.000000000000000 ) ;
#13621 = VERTEX_POINT ( 'NONE', #25968 ) ;
#13622 = PRESENTATION_STYLE_ASSIGNMENT (( #24507 ) ) ;
#13623 = PRESENTATION_STYLE_ASSIGNMENT (( #2685 ) ) ;
#13624 = ORIENTED_EDGE ( 'NONE', *, *, #56809, .T. ) ;
#13625 = CARTESIAN_POINT ( 'NONE',  ( 3.094860106618431583, 112.2049999999999841, 9.525000000000000355 ) ) ;
#13626 = CARTESIAN_POINT ( 'NONE',  ( -195.0000000000000000, 0.000000000000000000, 9.524999999999991473 ) ) ;
#13627 = ORIENTED_EDGE ( 'NONE', *, *, #22043, .F. ) ;
#13628 = COLOUR_RGB ( '', 0.08235294, 0.09019608, 0.10196078) ;
#13629 = SURFACE_STYLE_FILL_AREA ( #24515 ) ;
#13630 = VECTOR ( 'NONE', #60677, 1000.000000000000000 ) ;
#13631 = DIRECTION ( 'NONE',  ( -1.000000000000000000, 0.000000000000000000, 0.000000000000000000 ) ) ;
#13632 = CARTESIAN_POINT ( 'NONE',  ( -109.6449999999999960, 4.716976649647091513, -6.492361379858946790 ) ) ;
#13633 = ORIENTED_EDGE ( 'NONE', *, *, #1057, .F. ) ;
#13634 = AXIS2_PLACEMENT_3D ( 'NONE', #43859, #49131, #66304 ) ;
#13635 = CARTESIAN_POINT ( 'NONE',  ( -2.185379354980680588, 110.5000000000000000, -9.281319716557792532 ) ) ;
#13636 = DIRECTION ( 'NONE',  ( 0.000000000000000000, 0.000000000000000000, -1.000000000000000000 ) ) ;
#13637 = CARTESIAN_POINT ( 'NONE',  ( -14.67032170310171146, -10.90871211463571200, -5.000000000000000000 ) ) ;
#13638 = DIRECTION ( 'NONE',  ( 1.000000000000000000, 0.000000000000000000, 0.000000000000000000 ) ) ;
#13639 = EDGE_LOOP ( 'NONE', ( #15057, #12427, #48113, #32225 ) ) ;
#13640 = CARTESIAN_POINT ( 'NONE',  ( 0.000000000000000000, 143.9429263765338192, -8.025000000000000355 ) ) ;
#13641 = CARTESIAN_POINT ( 'NONE',  ( -54.73909702325379101, -9.103123100731311368, -2.346905346906726031 ) ) ;
#13642 = SURFACE_SIDE_STYLE ('',( #68173 ) ) ;
#13643 =( GEOMETRIC_REPRESENTATION_CONTEXT ( 3 ) GLOBAL_UNCERTAINTY_ASSIGNED_CONTEXT ( ( #53166 ) ) GLOBAL_UNIT_ASSIGNED_CONTEXT ( ( #69092, #32454, #42739 ) ) REPRESENTATION_CONTEXT ( 'NONE', 'WORKASPACE' ) );
#13644 = ADVANCED_FACE ( 'NONE', ( #11179 ), #15124, .F. ) ;
#13645 = SURFACE_STYLE_USAGE ( .BOTH. , #51637 ) ;
#13646 = ADVANCED_FACE ( 'NONE', ( #21746 ), #4503, .T. ) ;
#13647 = ORIENTED_EDGE ( 'NONE', *, *, #3209, .T. ) ;
#13648 = COLOUR_RGB ( '', 0.09019608, 0.27058824, 0.51372549) ;
#13649 = VERTEX_POINT ( 'NONE', #10847 ) ;
#13650 = CARTESIAN_POINT ( 'NONE',  ( 3.851859888774471706E-31, -7.500000000000000888, 1.000000000000000000 ) ) ;
#13651 = DIRECTION ( 'NONE',  ( 5.782411586589351722E-16, -1.000000000000000000, 0.000000000000000000 ) ) ;
#13652 = FILL_AREA_STYLE ('',( #1988 ) ) ;
#13653 = DIRECTION ( 'NONE',  ( -1.000000000000000000, 0.000000000000000000, 0.000000000000000000 ) ) ;
#13654 = CARTESIAN_POINT ( 'NONE',  ( -136.2549999999999955, -4.716976649647092401, 6.492361379858946790 ) ) ;
#13655 = FILL_AREA_STYLE ('',( #14347 ) ) ;
#13656 = LINE ( 'NONE', #9441, #26004 ) ;
#13657 = ORIENTED_EDGE ( 'NONE', *, *, #35751, .F. ) ;
#13658 = EDGE_CURVE ( 'NONE', #67222, #62684, #61881, .T. ) ;
#13659 =( GEOMETRIC_REPRESENTATION_CONTEXT ( 3 ) GLOBAL_UNCERTAINTY_ASSIGNED_CONTEXT ( ( #59568 ) ) GLOBAL_UNIT_ASSIGNED_CONTEXT ( ( #52366, #61825, #24538 ) ) REPRESENTATION_CONTEXT ( 'NONE', 'WORKASPACE' ) );
#13660 = CARTESIAN_POINT ( 'NONE',  ( -74.91375090774572243, 36.08647711726809604, 9.790149245326144722 ) ) ;
#13661 = CARTESIAN_POINT ( 'NONE',  ( 15.98999599679679839, 118.4999999999999716, 7.000000000000000000 ) ) ;
#13662 = B_SPLINE_CURVE_WITH_KNOTS ( 'NONE', 3,
 ( #17071, #38550, #48756, #54318, #49756, #47460, #11760, #23023 ),
 .UNSPECIFIED., .F., .F.,
 ( 4, 2, 2, 4 ),
 ( 0.004228133357766583958, 0.005276243923116602161, 0.006324354488466620364, 0.008420575619166656769 ),
 .UNSPECIFIED. ) ;
#13663 = ORIENTED_EDGE ( 'NONE', *, *, #56423, .T. ) ;
#13664 = CIRCLE ( 'NONE', #32808, 0.5000000000000004441 ) ;
#13665 = EDGE_LOOP ( 'NONE', ( #23643, #52885, #63972, #19718 ) ) ;
#13666 = CARTESIAN_POINT ( 'NONE',  ( -44.99154893926771592, 9.591540375271078389, 3.113444503357928994 ) ) ;
#13667 = CARTESIAN_POINT ( 'NONE',  ( 45.50000000000000000, 9.639620389971920389, 6.500000000000000000 ) ) ;
#13668 = CARTESIAN_POINT ( 'NONE',  ( 12.50000000000000533, 28.24999999999998224, -4.000000000000000000 ) ) ;
#13669 = CARTESIAN_POINT ( 'NONE',  ( -48.20499999999999829, -2.607480562269071545, -8.024999999999991473 ) ) ;
#13670 = VERTEX_POINT ( 'NONE', #37975 ) ;
#13671 = CARTESIAN_POINT ( 'NONE',  ( 27.00000000000001776, -60.04052944165106709, 34.49999999999999289 ) ) ;
#13672 = CARTESIAN_POINT ( 'NONE',  ( -176.3050000000000068, 8.437984349512085203, -1.550032578732815448E-15 ) ) ;
#13673 = CARTESIAN_POINT ( 'NONE',  ( -9.568252947146932641, 1.861307952554190237, 1.427299755870870435 ) ) ;
#13674 = CARTESIAN_POINT ( 'NONE',  ( -59.00707362346616236, -8.102448949553172852, -5.886773742842741797 ) ) ;
#13675 = ADVANCED_FACE ( 'NONE', ( #31950 ), #64303, .T. ) ;
#13676 = COLOUR_RGB ( '', 0.08235294, 0.09019608, 0.10196078) ;
#13677 = CARTESIAN_POINT ( 'NONE',  ( -181.1949999999999363, 8.437984349512086979, -1.550032578732815448E-15 ) ) ;
#13678 = CARTESIAN_POINT ( 'NONE',  ( -3.000000000000000000, -2.499999999999999556, 0.000000000000000000 ) ) ;
#13679 = VERTEX_POINT ( 'NONE', #53741 ) ;
#13680 = CIRCLE ( 'NONE', #58618, 1.000000000000000888 ) ;
#13681 = AXIS2_PLACEMENT_3D ( 'NONE', #14562, #69668, #57473 ) ;
#13682 = DIRECTION ( 'NONE',  ( 0.000000000000000000, -0.000000000000000000, 1.000000000000000000 ) ) ;
#13683 = EDGE_CURVE ( 'NONE', #35027, #60834, #37235, .T. ) ;
#13684 = FACE_OUTER_BOUND ( 'NONE', #46519, .T. ) ;
#13685 = CARTESIAN_POINT ( 'NONE',  ( -104.4549999999999983, 7.632228543268599452, -2.479861379858951942 ) ) ;
#13686 = CARTESIAN_POINT ( 'NONE',  ( 0.4393420241418015126, 154.5000000000000853, -9.524999999999996803 ) ) ;
#13687 = DIRECTION ( 'NONE',  ( 0.000000000000000000, 0.000000000000000000, -1.000000000000000000 ) ) ;
#13688 = MECHANICAL_DESIGN_GEOMETRIC_PRESENTATION_REPRESENTATION (  '', ( #12559 ), #4693 ) ;
#13689 = PRESENTATION_STYLE_ASSIGNMENT (( #24239 ) ) ;
#13690 = CARTESIAN_POINT ( 'NONE',  ( -100.1949999999999790, 8.437984349512086979, -1.550032578732815448E-15 ) ) ;
#13691 = CARTESIAN_POINT ( 'NONE',  ( -1.166476076187854022E-15, 121.0549999999999784, 9.525000000000000355 ) ) ;
#13692 = CARTESIAN_POINT ( 'NONE',  ( -65.09499999999998465, -2.607480562269071545, -8.024999999999991473 ) ) ;
#13693 = AXIS2_PLACEMENT_3D ( 'NONE', #23078, #22727, #54370 ) ;
#13694 = CARTESIAN_POINT ( 'NONE',  ( -56.60707362346617089, -8.102448949553174629, 5.886773742842742685 ) ) ;
#13695 = SURFACE_STYLE_USAGE ( .BOTH. , #14051 ) ;
#13696 = UNCERTAINTY_MEASURE_WITH_UNIT (LENGTH_MEASURE( 1.000000000000000082E-05 ), #38964, 'distance_accuracy_value', 'NONE');
#13697 = STYLED_ITEM ( 'NONE', ( #3475 ), #54393 ) ;
#13698 = CARTESIAN_POINT ( 'NONE',  ( 0.000000000000000000, 33.74999999999999289, 4.000000000000000000 ) ) ;
#13699 = ORIENTED_EDGE ( 'NONE', *, *, #34707, .F. ) ;
#13700 = CARTESIAN_POINT ( 'NONE',  ( -112.4929263765337879, -8.102448949553172852, 5.886773742842742685 ) ) ;
#13701 = CARTESIAN_POINT ( 'NONE',  ( -127.9449999999999790, -9.827790563157499189E-16, -8.024999999999991473 ) ) ;
#13702 = STYLED_ITEM ( 'NONE', ( #4241 ), #53599 ) ;
#13703 = VECTOR ( 'NONE', #2546, 1000.000000000000000 ) ;
#13704 = DIRECTION ( 'NONE',  ( 0.000000000000000000, 0.000000000000000000, 1.000000000000000000 ) ) ;
#13705 = AXIS2_PLACEMENT_3D ( 'NONE', #62197, #66804, #23520 ) ;
#13706 = ADVANCED_BREP_SHAPE_REPRESENTATION ( '', ( #26844, #42840 ), #29323 ) ;
#13707 =( NAMED_UNIT ( * ) PLANE_ANGLE_UNIT ( ) SI_UNIT ( $, .RADIAN. ) );
#13708 = ORIENTED_EDGE ( 'NONE', *, *, #35192, .F. ) ;
#13709 = VERTEX_POINT ( 'NONE', #68561 ) ;
#13710 = CARTESIAN_POINT ( 'NONE',  ( -63.14292637653380780, 5.598654528085800663, -7.705886871421367523 ) ) ;
#13711 = EDGE_CURVE ( 'NONE', #35184, #34574, #68916, .T. ) ;
#13712 = AXIS2_PLACEMENT_3D ( 'NONE', #54995, #33227, #28245 ) ;
#13713 = CARTESIAN_POINT ( 'NONE',  ( 33.00000000000000000, 15.00000000000000000, -80.00402776293826435 ) ) ;
#13714 = CARTESIAN_POINT ( 'NONE',  ( 34.99999999999999289, 99.99999999999997158, 9.500000000000000000 ) ) ;
#13715 = AXIS2_PLACEMENT_3D ( 'NONE', #15948, #37774, #59154 ) ;
#13716 = CARTESIAN_POINT ( 'NONE',  ( 61.99999999999998579, 31.24999999999999289, 4.000000000000000000 ) ) ;
#13717 = ORIENTED_EDGE ( 'NONE', *, *, #27819, .F. ) ;
#13718 = CARTESIAN_POINT ( 'NONE',  ( -135.8049999999999784, -8.437984349512086979, 5.166775262442717831E-16 ) ) ;
#13719 = ORIENTED_EDGE ( 'NONE', *, *, #43920, .T. ) ;
#13720 = DIRECTION ( 'NONE',  ( 0.000000000000000000, 0.000000000000000000, -1.000000000000000000 ) ) ;
#13721 = CARTESIAN_POINT ( 'NONE',  ( -121.5570736234661808, -1.166476076187852838E-15, -9.524999999999991473 ) ) ;
#13722 = VERTEX_POINT ( 'NONE', #36924 ) ;
#13723 = DIRECTION ( 'NONE',  ( 0.5000000000000003331, 0.8660254037844384856, 0.000000000000000000 ) ) ;
#13724 = DIRECTION ( 'NONE',  ( 1.000000000000000000, 0.000000000000000000, -0.000000000000000000 ) ) ;
#13725 = VERTEX_POINT ( 'NONE', #4871 ) ;
#13726 = LINE ( 'NONE', #46479, #21993 ) ;
#13727 = CARTESIAN_POINT ( 'NONE',  ( -10.01517768586949231, 140.1949999999999932, -6.132527647946036459E-16 ) ) ;
#13728 = PRESENTATION_STYLE_ASSIGNMENT (( #40493 ) ) ;
#13729 = ORIENTED_EDGE ( 'NONE', *, *, #49812, .F. ) ;
#13730 =( GEOMETRIC_REPRESENTATION_CONTEXT ( 3 ) GLOBAL_UNCERTAINTY_ASSIGNED_CONTEXT ( ( #64208 ) ) GLOBAL_UNIT_ASSIGNED_CONTEXT ( ( #68007, #67640, #29995 ) ) REPRESENTATION_CONTEXT ( 'NONE', 'WORKASPACE' ) );
#13731 = EDGE_CURVE ( 'NONE', #22750, #51627, #43555, .T. ) ;
#13732 = CARTESIAN_POINT ( 'NONE',  ( -5.598654528085808657, 135.7549999999999955, 7.705886871421373741 ) ) ;
#13733 = CARTESIAN_POINT ( 'NONE',  ( -195.0000000000000000, 1.166476076187852838E-15, -9.524999999999991473 ) ) ;
#13734 = DIRECTION ( 'NONE',  ( -1.000000000000000000, 0.000000000000000000, 0.000000000000000000 ) ) ;
#13735 = VERTEX_POINT ( 'NONE', #1259 ) ;
#13736 = CARTESIAN_POINT ( 'NONE',  ( -6.826472737025120807, 117.3929263765338078, -4.959722759717907437 ) ) ;
#13737 = SURFACE_STYLE_USAGE ( .BOTH. , #40500 ) ;
#13738 = UNCERTAINTY_MEASURE_WITH_UNIT (LENGTH_MEASURE( 1.000000000000000082E-05 ), #66394, 'distance_accuracy_value', 'NONE');
#13739 = CIRCLE ( 'NONE', #59782, 0.2500000000000002220 ) ;
#13740 = DIRECTION ( 'NONE',  ( 0.000000000000000000, 0.000000000000000000, 1.000000000000000000 ) ) ;
#13741 = EDGE_CURVE ( 'NONE', #2194, #1270, #26946, .T. ) ;
#13742 =( NAMED_UNIT ( * ) SI_UNIT ( $, .STERADIAN. ) SOLID_ANGLE_UNIT ( ) );
#13743 = EDGE_CURVE ( 'NONE', #54598, #26367, #18115, .T. ) ;
#13744 = VERTEX_POINT ( 'NONE', #61103 ) ;
#13745 = CARTESIAN_POINT ( 'NONE',  ( 41.49999999999998579, 106.9282032302754999, 3.500000000000000000 ) ) ;
#13746 = ORIENTED_EDGE ( 'NONE', *, *, #67837, .T. ) ;
#13747 = CARTESIAN_POINT ( 'NONE',  ( -195.0000000000000000, 1.166476076187852838E-15, -9.524999999999991473 ) ) ;
#13748 = DIRECTION ( 'NONE',  ( 1.000000000000000000, 0.000000000000000000, 0.000000000000000000 ) ) ;
#13749 = CARTESIAN_POINT ( 'NONE',  ( -195.0000000000000000, 0.000000000000000000, 9.524999999999991473 ) ) ;
#13750 = CARTESIAN_POINT ( 'NONE',  ( -161.3050000000000068, 8.437984349512085203, -1.550032578732815448E-15 ) ) ;
#13752 = EDGE_LOOP ( 'NONE', ( #39643, #37908, #57667, #7036 ) ) ;
#13751 = PRESENTATION_LAYER_ASSIGNMENT (  '', '', ( #17138 ) ) ;
#13753 = DIRECTION ( 'NONE',  ( 1.000000000000000000, 0.000000000000000000, 0.000000000000000000 ) ) ;
#13754 = UNCERTAINTY_MEASURE_WITH_UNIT (LENGTH_MEASURE( 1.000000000000000082E-05 ), #5820, 'distance_accuracy_value', 'NONE');
#13755 = CIRCLE ( 'NONE', #63166, 0.4999999999999994449 ) ;
#13756 = EDGE_CURVE ( 'NONE', #36746, #17595, #17855, .T. ) ;
#13757 =( NAMED_UNIT ( * ) PLANE_ANGLE_UNIT ( ) SI_UNIT ( $, .RADIAN. ) );
#13758 = DIRECTION ( 'NONE',  ( 0.000000000000000000, -1.000000000000000000, -0.000000000000000000 ) ) ;
#13759 = SURFACE_STYLE_USAGE ( .BOTH. , #7777 ) ;
#13760 = VERTEX_POINT ( 'NONE', #44291 ) ;
#13762 = EDGE_CURVE ( 'NONE', #51323, #61490, #36107, .T. ) ;
#13761 = ORIENTED_EDGE ( 'NONE', *, *, #801, .T. ) ;
#13763 = CARTESIAN_POINT ( 'NONE',  ( 0.000000000000000000, 0.000000000000000000, 0.000000000000000000 ) ) ;
#13764 = CARTESIAN_POINT ( 'NONE',  ( 8.750000000000001776, 24.99999999999998579, -3.750000000000000000 ) ) ;
#13765 = AXIS2_PLACEMENT_3D ( 'NONE', #41304, #30342, #36743 ) ;
#13766 = CARTESIAN_POINT ( 'NONE',  ( -78.65499999999998693, -7.632228543268600340, -2.479861379858950166 ) ) ;
#13767 = ORIENTED_EDGE ( 'NONE', *, *, #2739, .F. ) ;
#13768 = CARTESIAN_POINT ( 'NONE',  ( 23.21231517720797655, 117.4999999999999716, 9.500000000000000000 ) ) ;
#13769 = CIRCLE ( 'NONE', #225, 0.5000000000000004441 ) ;
#13770 = CARTESIAN_POINT ( 'NONE',  ( 17.75000000000000711, 31.24999999999999289, -3.750000000000000000 ) ) ;
#13771 = SURFACE_STYLE_FILL_AREA ( #54243 ) ;
#13772 = PRESENTATION_LAYER_ASSIGNMENT (  '', '', ( #48667 ) ) ;
#13773 = CARTESIAN_POINT ( 'NONE',  ( -74.08452722063037754, 9.430195807687219656, -6.000000000000000000 ) ) ;
#13774 = EDGE_LOOP ( 'NONE', ( #28052, #41845 ) ) ;
#13775 = LINE ( 'NONE', #25019, #51768 ) ;
#13776 = AXIS2_PLACEMENT_3D ( 'NONE', #10305, #43405, #10644 ) ;
#13778 = SURFACE_SIDE_STYLE ('',( #23977 ) ) ;
#13777 = CARTESIAN_POINT ( 'NONE',  ( 44.00000000000000000, 18.99999999999998224, 3.750000000000000000 ) ) ;
#13779 = CARTESIAN_POINT ( 'NONE',  ( -5.598654528085806881, 139.7449999999999761, -7.705886871421374629 ) ) ;
#13780 = CARTESIAN_POINT ( 'NONE',  ( -101.8449999999999847, -7.632228543268599452, 2.479861379858951054 ) ) ;
#13781 =( LENGTH_UNIT ( ) NAMED_UNIT ( * ) SI_UNIT ( .MILLI., .METRE. ) );
#13782 = VECTOR ( 'NONE', #56925, 1000.000000000000000 ) ;
#13783 = VECTOR ( 'NONE', #12142, 1000.000000000000000 ) ;
#13784 = CARTESIAN_POINT ( 'NONE',  ( 74.50000000000000000, -2.220952357103124925E-14, 9.500000000000000000 ) ) ;
#13785 = EDGE_CURVE ( 'NONE', #34416, #46628, #33820, .T. ) ;
#13786 = UNCERTAINTY_MEASURE_WITH_UNIT (LENGTH_MEASURE( 1.000000000000000082E-05 ), #5457, 'distance_accuracy_value', 'NONE');
#13787 = FACE_OUTER_BOUND ( 'NONE', #27493, .T. ) ;
#13788 =( GEOMETRIC_REPRESENTATION_CONTEXT ( 3 ) GLOBAL_UNCERTAINTY_ASSIGNED_CONTEXT ( ( #68461 ) ) GLOBAL_UNIT_ASSIGNED_CONTEXT ( ( #55868, #35468, #56200 ) ) REPRESENTATION_CONTEXT ( 'NONE', 'WORKASPACE' ) );
#13789 = CARTESIAN_POINT ( 'NONE',  ( -147.1429263765338078, 5.598654528085800663, -7.705886871421367523 ) ) ;
#13790 = PRESENTATION_STYLE_ASSIGNMENT (( #14471 ) ) ;
#13791 = CARTESIAN_POINT ( 'NONE',  ( -167.2450000000000045, -4.716976649647093289, -6.492361379858945902 ) ) ;
#13792 = SURFACE_STYLE_FILL_AREA ( #67252 ) ;
#13793 =( GEOMETRIC_REPRESENTATION_CONTEXT ( 3 ) GLOBAL_UNCERTAINTY_ASSIGNED_CONTEXT ( ( #63808 ) ) GLOBAL_UNIT_ASSIGNED_CONTEXT ( ( #59382, #54466, #27713 ) ) REPRESENTATION_CONTEXT ( 'NONE', 'WORKASPACE' ) );
#13794 = FILL_AREA_STYLE ('',( #61966 ) ) ;
#13795 = VERTEX_POINT ( 'NONE', #7306 ) ;
#13796 = ORIENTED_EDGE ( 'NONE', *, *, #29619, .F. ) ;
#13797 = AXIS2_PLACEMENT_3D ( 'NONE', #41214, #45111, #45467 ) ;
#13798 =( GEOMETRIC_REPRESENTATION_CONTEXT ( 3 ) GLOBAL_UNCERTAINTY_ASSIGNED_CONTEXT ( ( #50305 ) ) GLOBAL_UNIT_ASSIGNED_CONTEXT ( ( #9617, #4273, #43043 ) ) REPRESENTATION_CONTEXT ( 'NONE', 'WORKASPACE' ) );
#13799 =( NAMED_UNIT ( * ) SI_UNIT ( $, .STERADIAN. ) SOLID_ANGLE_UNIT ( ) );
#13800 = CARTESIAN_POINT ( 'NONE',  ( -45.54132543224191210, 7.945093266342319716, 6.500000000000000888 ) ) ;
#13801 = CARTESIAN_POINT ( 'NONE',  ( 44.28021770739998431, 9.999999999999980460, 3.500000000000000000 ) ) ;
#13802 = CIRCLE ( 'NONE', #34030, 0.5000000000000004441 ) ;
#13803 = ORIENTED_EDGE ( 'NONE', *, *, #10492, .T. ) ;
#13804 = CARTESIAN_POINT ( 'NONE',  ( -157.8549999999999898, 4.716976649647094177, 6.492361379858945902 ) ) ;
#13805 = MECHANICAL_DESIGN_GEOMETRIC_PRESENTATION_REPRESENTATION (  '', ( #64375 ), #60934 ) ;
#13806 = EDGE_LOOP ( 'NONE', ( #50700, #4875, #15046, #512 ) ) ;
#13807 = PRESENTATION_LAYER_ASSIGNMENT (  '', '', ( #48701 ) ) ;
#13808 = DIRECTION ( 'NONE',  ( -1.000000000000000000, -0.000000000000000000, -0.000000000000000000 ) ) ;
#13809 = CARTESIAN_POINT ( 'NONE',  ( -12.34222745343792127, 114.9999999999999574, -10.18181818181818166 ) ) ;
#13810 = ORIENTED_EDGE ( 'NONE', *, *, #45943, .T. ) ;
#13811 = DIRECTION ( 'NONE',  ( 0.000000000000000000, 0.000000000000000000, 1.000000000000000000 ) ) ;
#13812 = CARTESIAN_POINT ( 'NONE',  ( -60.00000000000000000, -2.024042244987997205E-14, -12.00000000000000000 ) ) ;
#13813 = CARTESIAN_POINT ( 'NONE',  ( -8.102448949553181734, 115.8949999999999960, -5.886773742842749790 ) ) ;
#13814 = VERTEX_POINT ( 'NONE', #12200 ) ;
#13815 = EDGE_CURVE ( 'NONE', #25507, #67841, #27338, .T. ) ;
#13816 = CYLINDRICAL_SURFACE ( 'NONE', #11701, 13.99999999999999822 ) ;
#13817 = CARTESIAN_POINT ( 'NONE',  ( -8.102448949553179958, 114.0049999999999670, -5.886773742842749790 ) ) ;
#13818 = CARTESIAN_POINT ( 'NONE',  ( -75.35499999999998977, -4.716976649647093289, -6.492361379858945902 ) ) ;
#13819 = DIRECTION ( 'NONE',  ( -1.000000000000000000, 0.000000000000000000, 0.000000000000000000 ) ) ;
#13820 =( BOUNDED_CURVE ( )  B_SPLINE_CURVE ( 2, ( #8045, #1677, #7686, #60127, #38720, #34761, #65752, #28428, #55540, #49940, #50274 ),
 .UNSPECIFIED., .F., .F. ) 
 B_SPLINE_CURVE_WITH_KNOTS ( ( 3, 2, 2, 2, 2, 3 ),
 ( 0.1956521739130387683, 0.1978260869565169611, 0.1999999999999951816, 0.2021739130434734022, 0.2043478260869516228, 0.2065217391304298156 ),
 .UNSPECIFIED. ) 
 CURVE ( )  GEOMETRIC_REPRESENTATION_ITEM ( )  RATIONAL_B_SPLINE_CURVE ( ( 1.000000000000106137, 0.9510565162950472828, 1.000000000000000000, 0.9510565162951535312, 1.000000000000000000, 0.9510565162951535312, 1.000000000000000000, 0.9510565162951535312, 1.000000000000000000, 0.9510565162952654417, 0.9999999999998880895 ) ) 
 REPRESENTATION_ITEM ( '' )  );
#13821 = VERTEX_POINT ( 'NONE', #16840 ) ;
#13822 = CARTESIAN_POINT ( 'NONE',  ( -10.01517768586949231, 135.3049999999999784, -6.132527647946036459E-16 ) ) ;
#13823 = UNCERTAINTY_MEASURE_WITH_UNIT (LENGTH_MEASURE( 1.000000000000000082E-05 ), #52497, 'distance_accuracy_value', 'NONE');
#13824 = CARTESIAN_POINT ( 'NONE',  ( -41.49999999999997868, 10.49999999999998046, 3.000000000000000000 ) ) ;
#13825 = EDGE_CURVE ( 'NONE', #19539, #29216, #38334, .T. ) ;
#13826 =( NAMED_UNIT ( * ) SI_UNIT ( $, .STERADIAN. ) SOLID_ANGLE_UNIT ( ) );
#13827 = CARTESIAN_POINT ( 'NONE',  ( -41.25908726609139876, 107.3516760703038102, 3.442203282073898141 ) ) ;
#13828 = DIRECTION ( 'NONE',  ( -0.000000000000000000, 1.000000000000000000, -0.000000000000000000 ) ) ;
#13829 = ORIENTED_EDGE ( 'NONE', *, *, #11274, .T. ) ;
#13830 =( GEOMETRIC_REPRESENTATION_CONTEXT ( 3 ) GLOBAL_UNCERTAINTY_ASSIGNED_CONTEXT ( ( #41062 ) ) GLOBAL_UNIT_ASSIGNED_CONTEXT ( ( #47561, #58751, #43644 ) ) REPRESENTATION_CONTEXT ( 'NONE', 'WORKASPACE' ) );
#13831 = MECHANICAL_DESIGN_GEOMETRIC_PRESENTATION_REPRESENTATION (  '', ( #17226 ), #50935 ) ;
#13832 = CARTESIAN_POINT ( 'NONE',  ( 8.000000000000035527, 5.000000000000000000, 77.00402776293825013 ) ) ;
#13833 = CARTESIAN_POINT ( 'NONE',  ( -48.59499999999997755, 2.607480562269073321, 8.024999999999991473 ) ) ;
#13834 = ORIENTED_EDGE ( 'NONE', *, *, #64901, .T. ) ;
#13835 = SURFACE_SIDE_STYLE ('',( #66963 ) ) ;
#13836 = DIRECTION ( 'NONE',  ( 0.000000000000000000, 0.7071067811865469066, 0.7071067811865482389 ) ) ;
#13837 = CARTESIAN_POINT ( 'NONE',  ( 72.50000000000000000, 14.49137674618942562, 10.00000000000000000 ) ) ;
#13838 = EDGE_LOOP ( 'NONE', ( #56436, #37906, #44247, #68388 ) ) ;
#13839 = CARTESIAN_POINT ( 'NONE',  ( -52.94499999999999318, -9.827790563157499189E-16, -8.024999999999991473 ) ) ;
#13840 = CARTESIAN_POINT ( 'NONE',  ( -22.50000000000000711, 36.75000000000000000, -3.750000000000000000 ) ) ;
#13841 = ORIENTED_EDGE ( 'NONE', *, *, #28157, .F. ) ;
#13842 = ADVANCED_FACE ( 'NONE', ( #11879 ), #39336, .T. ) ;
#13843 = CARTESIAN_POINT ( 'NONE',  ( -103.8549999999999898, 4.716976649647094177, 6.492361379858945902 ) ) ;
#13844 = ORIENTED_EDGE ( 'NONE', *, *, #25812, .F. ) ;
#13846 = CIRCLE ( 'NONE', #49655, 0.5000000000000004441 ) ;
#13845 = CARTESIAN_POINT ( 'NONE',  ( -20.29261984882471381, 1.607755262496696869, -6.349999999999987210 ) ) ;
#13847 = DIRECTION ( 'NONE',  ( 1.000000000000000000, 0.000000000000000000, 4.625929269271505635E-16 ) ) ;
#13848 = CARTESIAN_POINT ( 'NONE',  ( -138.5070736234661695, 8.102448949553176405, 5.886773742842740909 ) ) ;
#13849 = STYLED_ITEM ( 'NONE', ( #42599 ), #36174 ) ;
#13850 = CARTESIAN_POINT ( 'NONE',  ( 7.794228634059945371, 2.500000000000000000, 4.500000000000000888 ) ) ;
#13851 = CARTESIAN_POINT ( 'NONE',  ( -8.102448949553179958, 140.4949999999999761, 5.886773742842747126 ) ) ;
#13852 = CARTESIAN_POINT ( 'NONE',  ( -72.95707362346617231, 9.058813317711329915, -2.943386871421373119 ) ) ;
#13853 =( NAMED_UNIT ( * ) SI_UNIT ( $, .STERADIAN. ) SOLID_ANGLE_UNIT ( ) );
#13854 = MECHANICAL_DESIGN_GEOMETRIC_PRESENTATION_REPRESENTATION (  '', ( #17257 ), #33095 ) ;
#13855 = CARTESIAN_POINT ( 'NONE',  ( -4.500000000000002665, 24.74999999999998579, -3.750000000000000000 ) ) ;
#13856 = CARTESIAN_POINT ( 'NONE',  ( -18.97318813750202082, -11.60852854622079455, -3.052579355033961495 ) ) ;
#13858 = DIRECTION ( 'NONE',  ( -1.000000000000000000, -0.000000000000000000, -0.000000000000000000 ) ) ;
#13857 = CARTESIAN_POINT ( 'NONE',  ( 0.000000000000000000, 0.9999999999999991118, 79.00402776293826435 ) ) ;
#13859 = AXIS2_PLACEMENT_3D ( 'NONE', #41506, #52744, #25298 ) ;
#13860 = CARTESIAN_POINT ( 'NONE',  ( -120.2049999999999983, -2.607480562269071545, -8.024999999999991473 ) ) ;
#13861 = DIRECTION ( 'NONE',  ( 0.000000000000000000, 0.000000000000000000, -1.000000000000000000 ) ) ;
#13862 = CARTESIAN_POINT ( 'NONE',  ( -138.1449999999999818, -4.716976649647092401, 6.492361379858946790 ) ) ;
#13863 = CARTESIAN_POINT ( 'NONE',  ( -120.2949999999999733, -2.607480562269069768, 8.024999999999991473 ) ) ;
#13864 = SURFACE_STYLE_FILL_AREA ( #41673 ) ;
#13865 = EDGE_CURVE ( 'NONE', #29661, #51672, #2664, .T. ) ;
#13866 = ORIENTED_EDGE ( 'NONE', *, *, #52172, .F. ) ;
#13867 = PLANE ( 'NONE',  #16785 ) ;
#13868 = CIRCLE ( 'NONE', #47622, 0.2500000000000002220 ) ;
#13869 = DIRECTION ( 'NONE',  ( -0.000000000000000000, -0.000000000000000000, 1.000000000000000000 ) ) ;
#13870 = MECHANICAL_DESIGN_GEOMETRIC_PRESENTATION_REPRESENTATION (  '', ( #16157 ), #53202 ) ;
#13871 = CARTESIAN_POINT ( 'NONE',  ( -171.8929263765338078, -8.102448949553172852, -5.886773742842741797 ) ) ;
#13872 = CARTESIAN_POINT ( 'NONE',  ( -51.89499999999998892, 6.826472737025116366, 4.959722759717898555 ) ) ;
#13873 = FACE_OUTER_BOUND ( 'NONE', #52064, .T. ) ;
#13874 = MECHANICAL_DESIGN_GEOMETRIC_PRESENTATION_REPRESENTATION (  '', ( #39708 ), #67763 ) ;
#13875 = STYLED_ITEM ( 'NONE', ( #56177 ), #61803 ) ;
#13876 = CARTESIAN_POINT ( 'NONE',  ( 57.00000000000000000, 14.00000000000000000, 60.00402776293827145 ) ) ;
#13877 = CARTESIAN_POINT ( 'NONE',  ( 6.759171781091401598, 2.292771058063876932, 0.1074872947962648290 ) ) ;
#13878 = ORIENTED_EDGE ( 'NONE', *, *, #43814, .T. ) ;
#13879 = CARTESIAN_POINT ( 'NONE',  ( -85.94292637653380496, 0.000000000000000000, 9.524999999999991473 ) ) ;
#13880 = CONTEXT_DEPENDENT_SHAPE_REPRESENTATION ( #69389, #18199 ) ;
#13881 = DIRECTION ( 'NONE',  ( -0.000000000000000000, -0.000000000000000000, -1.000000000000000000 ) ) ;
#13882 = LINE ( 'NONE', #40287, #24793 ) ;
#13883 = CIRCLE ( 'NONE', #43108, 1.000000000000000888 ) ;
#13884 = COLOUR_RGB ( '', 0.09019608, 0.27058824, 0.51372549) ;
#13885 = SURFACE_SIDE_STYLE ('',( #45917 ) ) ;
#13886 = CARTESIAN_POINT ( 'NONE',  ( 6.826472737025119919, 123.0070736234661553, 4.959722759717908325 ) ) ;
#13887 = CARTESIAN_POINT ( 'NONE',  ( 43.75000000000000000, 18.74999999999998224, -4.000000000000000000 ) ) ;
#13888 = CARTESIAN_POINT ( 'NONE',  ( -157.2570736234661979, 5.598654528085800663, -7.705886871421367523 ) ) ;
#13889 = CIRCLE ( 'NONE', #21723, 0.5000000000000004441 ) ;
#13890 = ORIENTED_EDGE ( 'NONE', *, *, #55881, .F. ) ;
#13891 = DIRECTION ( 'NONE',  ( -0.000000000000000000, 0.000000000000000000, -1.000000000000000000 ) ) ;
#13893 = ADVANCED_FACE ( 'NONE', ( #13248 ), #26700, .F. ) ;
#13892 = CARTESIAN_POINT ( 'NONE',  ( 1.908195823574488119E-14, 24.75000000000002487, 4.000000000000000000 ) ) ;
#13894 = ORIENTED_EDGE ( 'NONE', *, *, #14225, .T. ) ;
#13895 = DIRECTION ( 'NONE',  ( -1.000000000000000000, -0.000000000000000000, -0.000000000000000000 ) ) ;
#13896 = FACE_OUTER_BOUND ( 'NONE', #14501, .T. ) ;
#13897 = CARTESIAN_POINT ( 'NONE',  ( 2.607480562269071989, 134.7070736234661297, 8.025000000000002132 ) ) ;
#13898 = AXIS2_PLACEMENT_3D ( 'NONE', #8031, #46045, #29480 ) ;
#13899 = ORIENTED_EDGE ( 'NONE', *, *, #44074, .F. ) ;
#13900 = DIRECTION ( 'NONE',  ( 0.000000000000000000, 0.000000000000000000, 1.000000000000000000 ) ) ;
#13901 = CARTESIAN_POINT ( 'NONE',  ( -105.9549999999999983, -7.632228543268599452, 2.479861379858951054 ) ) ;
#13903 = CARTESIAN_POINT ( 'NONE',  ( 0.000000000000000000, 0.000000000000000000, 0.7500000000000000000 ) ) ;
#13902 =( GEOMETRIC_REPRESENTATION_CONTEXT ( 3 ) GLOBAL_UNCERTAINTY_ASSIGNED_CONTEXT ( ( #25070 ) ) GLOBAL_UNIT_ASSIGNED_CONTEXT ( ( #10529, #54455, #42926 ) ) REPRESENTATION_CONTEXT ( 'NONE', 'WORKASPACE' ) );
#13904 = ORIENTED_EDGE ( 'NONE', *, *, #16397, .T. ) ;
#13905 = VECTOR ( 'NONE', #57604, 1000.000000000000000 ) ;
#13906 = AXIS2_PLACEMENT_3D ( 'NONE', #24168, #54776, #2294 ) ;
#13907 = EDGE_CURVE ( 'NONE', #1374, #53049, #62133, .T. ) ;
#13908 = FACE_OUTER_BOUND ( 'NONE', #65563, .T. ) ;
#13909 =( NAMED_UNIT ( * ) PLANE_ANGLE_UNIT ( ) SI_UNIT ( $, .RADIAN. ) );
#13910 = MECHANICAL_DESIGN_GEOMETRIC_PRESENTATION_REPRESENTATION (  '', ( #4919 ), #25155 ) ;
#13911 = EDGE_CURVE ( 'NONE', #67626, #1545, #14303, .T. ) ;
#13912 = CARTESIAN_POINT ( 'NONE',  ( -74.49999999999998579, 1.735173206890467813E-14, -10.00000000000000000 ) ) ;
#13913 = CARTESIAN_POINT ( 'NONE',  ( -81.89499999999999602, 6.826472737025116366, 4.959722759717898555 ) ) ;
#13914 = ORIENTED_EDGE ( 'NONE', *, *, #68679, .T. ) ;
#13915 = AXIS2_PLACEMENT_3D ( 'NONE', #24040, #45546, #45867 ) ;
#13916 = EDGE_CURVE ( 'NONE', #10860, #27560, #34293, .T. ) ;
#13917 = DIRECTION ( 'NONE',  ( -1.000000000000000000, 0.000000000000000000, 0.000000000000000000 ) ) ;
#13918 = ORIENTED_EDGE ( 'NONE', *, *, #32313, .F. ) ;
#13919 = DIRECTION ( 'NONE',  ( 1.000000000000000000, 0.000000000000000000, 0.000000000000000000 ) ) ;
#13920 = EDGE_CURVE ( 'NONE', #34398, #55502, #21101, .T. ) ;
#13921 = CARTESIAN_POINT ( 'NONE',  ( -4.750000000000002665, 22.24999999999998579, 4.000000000000000000 ) ) ;
#13922 = ORIENTED_EDGE ( 'NONE', *, *, #39926, .T. ) ;
#13923 = EDGE_LOOP ( 'NONE', ( #46763, #48105, #64949, #59384 ) ) ;
#13924 = CARTESIAN_POINT ( 'NONE',  ( -44.00000000000000000, 11.99999999999999467, 0.000000000000000000 ) ) ;
#13925 = CARTESIAN_POINT ( 'NONE',  ( -195.0000000000000000, 0.000000000000000000, 9.524999999999991473 ) ) ;
#13926 =( GEOMETRIC_REPRESENTATION_CONTEXT ( 3 ) GLOBAL_UNCERTAINTY_ASSIGNED_CONTEXT ( ( #57197 ) ) GLOBAL_UNIT_ASSIGNED_CONTEXT ( ( #62497, #57220, #13973 ) ) REPRESENTATION_CONTEXT ( 'NONE', 'WORKASPACE' ) );
#13927 = AXIS2_PLACEMENT_3D ( 'NONE', #6515, #47789, #42488 ) ;
#13928 = CARTESIAN_POINT ( 'NONE',  ( -166.1070736234661638, 8.102448949553171076, -5.886773742842744461 ) ) ;
#13929 = DIRECTION ( 'NONE',  ( -1.300977106640434891E-16, 0.000000000000000000, -1.000000000000000000 ) ) ;
#13930 = CARTESIAN_POINT ( 'NONE',  ( -10.01517768586949408, 116.1949999999999932, -6.132527647946036459E-16 ) ) ;
#13931 = CARTESIAN_POINT ( 'NONE',  ( -111.6570736234661751, 9.058813317711329915, 2.943386871421369566 ) ) ;
#13932 = CARTESIAN_POINT ( 'NONE',  ( -183.3230534119037429, 0.7217949698500222278, -9.201946588096255653 ) ) ;
#13933 = CARTESIAN_POINT ( 'NONE',  ( 1.804495846578303864, 51.08602766979955589, -7.112547338523483198 ) ) ;
#13934 = ORIENTED_EDGE ( 'NONE', *, *, #11122, .F. ) ;
#13935 = CARTESIAN_POINT ( 'NONE',  ( -44.50000000000000000, 9.999999999999980460, -3.000000000000000444 ) ) ;
#13936 = CARTESIAN_POINT ( 'NONE',  ( -57.11974195712093660, -13.49999999999999467, -7.000000000000000000 ) ) ;
#13938 = LINE ( 'NONE', #36820, #49332 ) ;
#13937 = CARTESIAN_POINT ( 'NONE',  ( -60.00000000000000000, -2.024042244987997205E-14, 12.00000000000000000 ) ) ;
#13939 = SURFACE_SIDE_STYLE ('',( #62114 ) ) ;
#13940 = AXIS2_PLACEMENT_3D ( 'NONE', #5641, #15903, #9924 ) ;
#13941 = CARTESIAN_POINT ( 'NONE',  ( -151.7049999999999841, 2.607480562269073321, 8.024999999999991473 ) ) ;
#13942 =( NAMED_UNIT ( * ) PLANE_ANGLE_UNIT ( ) SI_UNIT ( $, .RADIAN. ) );
#13943 = CARTESIAN_POINT ( 'NONE',  ( -60.70461754965443646, -7.499999999999992006, 0.000000000000000000 ) ) ;
#13944 = CARTESIAN_POINT ( 'NONE',  ( -162.4449999999999932, 0.000000000000000000, 8.024999999999991473 ) ) ;
#13945 = CARTESIAN_POINT ( 'NONE',  ( -148.3449999999999989, 7.632228543268599452, -2.479861379858951942 ) ) ;
#13946 = EDGE_LOOP ( 'NONE', ( #66929, #39714, #61449 ) ) ;
#13947 =( BOUNDED_CURVE ( )  B_SPLINE_CURVE ( 3, ( #5938, #53460, #68602, #69296 ),
 .UNSPECIFIED., .F., .F. ) 
 B_SPLINE_CURVE_WITH_KNOTS ( ( 4, 4 ),
 ( 5.144579788448437441, 6.283185307179586232 ),
 .UNSPECIFIED. ) 
 CURVE ( )  GEOMETRIC_REPRESENTATION_ITEM ( )  RATIONAL_B_SPLINE_CURVE ( ( 1.000000000000000000, 0.8948513492540277614, 0.8948513492540277614, 1.000000000000000000 ) ) 
 REPRESENTATION_ITEM ( '' )  );
#13948 = CARTESIAN_POINT ( 'NONE',  ( -67.64292637653379359, -5.598654528085801552, 7.705886871421367523 ) ) ;
#13949 = CARTESIAN_POINT ( 'NONE',  ( -4.041451884327381450, 7.000000000000006217, 7.500000000000000000 ) ) ;
#13950 = CARTESIAN_POINT ( 'NONE',  ( 20.57648123223228254, 110.4999999999999858, 10.27659574468085069 ) ) ;
#13951 = STYLED_ITEM ( 'NONE', ( #14137 ), #31262 ) ;
#13952 = CARTESIAN_POINT ( 'NONE',  ( -62.45499999999998408, 7.632228543268599452, -2.479861379858951942 ) ) ;
#13953 = DIRECTION ( 'NONE',  ( 0.000000000000000000, 0.000000000000000000, 1.000000000000000000 ) ) ;
#13954 = FILL_AREA_STYLE_COLOUR ( '', #8955 ) ;
#13955 = COLOUR_RGB ( '', 0.72549020, 0.75294118, 0.79215686) ;
#13956 = CARTESIAN_POINT ( 'NONE',  ( -62.99499999999996902, -6.826472737025113702, 4.959722759717902107 ) ) ;
#13957 = CARTESIAN_POINT ( 'NONE',  ( 8.102448949553183510, 152.1049999999999613, -5.886773742842746238 ) ) ;
#13958 = DIRECTION ( 'NONE',  ( 1.000000000000000000, 0.000000000000000000, 0.000000000000000000 ) ) ;
#13959 = AXIS2_PLACEMENT_3D ( 'NONE', #3200, #1811, #44824 ) ;
#13960 = PLANE ( 'NONE',  #22258 ) ;
#13961 = CARTESIAN_POINT ( 'NONE',  ( 0.7152599553061413928, 42.96841831342781859, -45.59272038898399870 ) ) ;
#13962 =( GEOMETRIC_REPRESENTATION_CONTEXT ( 3 ) GLOBAL_UNCERTAINTY_ASSIGNED_CONTEXT ( ( #55965 ) ) GLOBAL_UNIT_ASSIGNED_CONTEXT ( ( #6629, #44344, #39390 ) ) REPRESENTATION_CONTEXT ( 'NONE', 'WORKASPACE' ) );
#13963 =( NAMED_UNIT ( * ) PLANE_ANGLE_UNIT ( ) SI_UNIT ( $, .RADIAN. ) );
#13964 = COLOUR_RGB ( '', 0.72549020, 0.75294118, 0.79215686) ;
#13965 = CARTESIAN_POINT ( 'NONE',  ( 3.000000000000000444, 3.673940397442059868E-16, 52.50000000000000000 ) ) ;
#13966 = ADVANCED_FACE ( 'NONE', ( #23816, #51955 ), #13960, .T. ) ;
#13967 = SURFACE_STYLE_FILL_AREA ( #51262 ) ;
#13968 = CARTESIAN_POINT ( 'NONE',  ( 57.00000000000000000, 14.00000000000000000, -79.00402776293826435 ) ) ;
#13969 = ORIENTED_EDGE ( 'NONE', *, *, #55922, .F. ) ;
#13971 = ORIENTED_EDGE ( 'NONE', *, *, #17309, .F. ) ;
#13970 = CIRCLE ( 'NONE', #6085, 0.5000000000000004441 ) ;
#13972 = VECTOR ( 'NONE', #8976, 1000.000000000000000 ) ;
#13973 =( NAMED_UNIT ( * ) SI_UNIT ( $, .STERADIAN. ) SOLID_ANGLE_UNIT ( ) );
#13974 = DIRECTION ( 'NONE',  ( 0.000000000000000000, 0.000000000000000000, 1.000000000000000000 ) ) ;
#13975 = EDGE_CURVE ( 'NONE', #33970, #51601, #7632, .T. ) ;
#13976 = EDGE_CURVE ( 'NONE', #30278, #6517, #6470, .T. ) ;
#13977 = FILL_AREA_STYLE_COLOUR ( '', #1172 ) ;
#13978 = DIRECTION ( 'NONE',  ( 0.000000000000000000, 1.000000000000000000, 0.000000000000000000 ) ) ;
#13979 = EDGE_CURVE ( 'NONE', #32866, #52425, #32319, .T. ) ;
#13980 = VERTEX_POINT ( 'NONE', #10767 ) ;
#13981 = VERTEX_POINT ( 'NONE', #9396 ) ;
#13982 =( LENGTH_UNIT ( ) NAMED_UNIT ( * ) SI_UNIT ( .MILLI., .METRE. ) );
#13983 = DIRECTION ( 'NONE',  ( 0.000000000000000000, 0.000000000000000000, -1.000000000000000000 ) ) ;
#13984 = AXIS2_PLACEMENT_3D ( 'NONE', #49284, #11285, #32740 ) ;
#13985 = EDGE_CURVE ( 'NONE', #56915, #67877, #11613, .T. ) ;
#13986 = VERTEX_POINT ( 'NONE', #15033 ) ;
#13987 = CARTESIAN_POINT ( 'NONE',  ( -65.39292637653379359, 8.102448949553176405, 5.886773742842740909 ) ) ;
#13988 = CARTESIAN_POINT ( 'NONE',  ( -71.62068965517239860, 36.41396814395972115, 7.000000000000000000 ) ) ;
#13989 = ORIENTED_EDGE ( 'NONE', *, *, #10355, .T. ) ;
#13990 = EDGE_CURVE ( 'NONE', #35716, #9757, #4784, .T. ) ;
#13991 = AXIS2_PLACEMENT_3D ( 'NONE', #11412, #27217, #16041 ) ;
#13992 = CARTESIAN_POINT ( 'NONE',  ( -71.75000000000000000, -3.000000000000000000, 20.00000000000000000 ) ) ;
#13993 = EDGE_CURVE ( 'NONE', #28559, #10224, #61540, .T. ) ;
#13994 = DIRECTION ( 'NONE',  ( 0.000000000000000000, -0.000000000000000000, 1.000000000000000000 ) ) ;
#13995 = CARTESIAN_POINT ( 'NONE',  ( -109.0449999999999875, 7.632228543268600340, 2.479861379858949277 ) ) ;
#13996 = ORIENTED_EDGE ( 'NONE', *, *, #39135, .T. ) ;
#13997 = CIRCLE ( 'NONE', #35347, 2.499999999999998668 ) ;
#13998 = CARTESIAN_POINT ( 'NONE',  ( -7.647808743681030030, 110.5000000000002984, 5.677732506914710875 ) ) ;
#13999 = ADVANCED_FACE ( 'NONE', ( #26237 ), #15709, .F. ) ;
#14000 = DIRECTION ( 'NONE',  ( -1.156482317317873451E-16, -1.000000000000000000, 0.000000000000000000 ) ) ;
#14001 = STYLED_ITEM ( 'NONE', ( #29154 ), #31599 ) ;
#14002 = ORIENTED_EDGE ( 'NONE', *, *, #8868, .T. ) ;
#14003 = CARTESIAN_POINT ( 'NONE',  ( 2.607480562269071989, 148.5929263765338249, 8.025000000000002132 ) ) ;
#14004 = SURFACE_STYLE_USAGE ( .BOTH. , #13642 ) ;
#14005 =( NAMED_UNIT ( * ) PLANE_ANGLE_UNIT ( ) SI_UNIT ( $, .RADIAN. ) );
#14006 = ORIENTED_EDGE ( 'NONE', *, *, #1527, .T. ) ;
#14007 = ORIENTED_EDGE ( 'NONE', *, *, #37400, .T. ) ;
#14008 = DIRECTION ( 'NONE',  ( 1.000000000000000000, 0.000000000000000000, 0.000000000000000000 ) ) ;
#14009 = CARTESIAN_POINT ( 'NONE',  ( -45.91547277936962956, 9.430195807687221432, 3.508932040081435222 ) ) ;
#14010 = CARTESIAN_POINT ( 'NONE',  ( 31.00000000000002132, 15.00000000000000000, 79.00402776293823592 ) ) ;
#14011 = CARTESIAN_POINT ( 'NONE',  ( 0.000000000000000000, 0.000000000000000000, 0.000000000000000000 ) ) ;
#14012 = CARTESIAN_POINT ( 'NONE',  ( -128.1550000000000011, 7.632228543268600340, 2.479861379858949277 ) ) ;
#14013 = CARTESIAN_POINT ( 'NONE',  ( -184.0000000000000000, -0.7817472717335689492, 8.024999999999995026 ) ) ;
#14014 = LINE ( 'NONE', #24209, #56335 ) ;
#14015 = FILL_AREA_STYLE ('',( #24896 ) ) ;
#14016 = CIRCLE ( 'NONE', #53346, 0.5000000000000004441 ) ;
#14017 = DIRECTION ( 'NONE',  ( -0.000000000000000000, -0.000000000000000000, -1.000000000000000000 ) ) ;
#14018 = LINE ( 'NONE', #62875, #46336 ) ;
#14019 = CARTESIAN_POINT ( 'NONE',  ( -40.04190075645215785, -13.49999999999999822, 0.8979962945199000401 ) ) ;
#14020 = EDGE_LOOP ( 'NONE', ( #4051, #21678, #51554, #46044 ) ) ;
#14021 = VERTEX_POINT ( 'NONE', #41771 ) ;
#14022 = CARTESIAN_POINT ( 'NONE',  ( -8.082903768654762899, 3.516382302766490365E-15, 7.500000000000000000 ) ) ;
#14023 = CARTESIAN_POINT ( 'NONE',  ( -31.53475076290974499, -8.620751121487828073, -1.503968433715946240 ) ) ;
#14024 = DIRECTION ( 'NONE',  ( 0.000000000000000000, -1.000000000000000000, 0.000000000000000000 ) ) ;
#14026 = CARTESIAN_POINT ( 'NONE',  ( 40.99999999999997868, 9.999999999999978684, 3.500000000000000000 ) ) ;
#14025 = PRESENTATION_LAYER_ASSIGNMENT (  '', '', ( #41017 ) ) ;
#14027 = ORIENTED_EDGE ( 'NONE', *, *, #41407, .F. ) ;
#14028 = CARTESIAN_POINT ( 'NONE',  ( 57.00000000000000000, 16.00000000000000000, -72.50402776293826435 ) ) ;
#14029 = CARTESIAN_POINT ( 'NONE',  ( -177.2050000000000125, -2.607480562269071545, -8.024999999999991473 ) ) ;
#14030 = CARTESIAN_POINT ( 'NONE',  ( -8.021777294149472937, 2.499999999999994227, 4.105874159530730871 ) ) ;
#14031 = CARTESIAN_POINT ( 'NONE',  ( 17.25000000000000711, 25.24999999999998224, -3.750000000000000000 ) ) ;
#14032 = CARTESIAN_POINT ( 'NONE',  ( -58.85707362346617799, -5.598654528085803328, -7.705886871421366635 ) ) ;
#14033 = STYLED_ITEM ( 'NONE', ( #61635 ), #62492 ) ;
#14034 = VECTOR ( 'NONE', #13983, 1000.000000000000000 ) ;
#14035 = CARTESIAN_POINT ( 'NONE',  ( -176.6949999999999363, -8.437984349512086979, 5.166775262442717831E-16 ) ) ;
#14036 = CARTESIAN_POINT ( 'NONE',  ( 41.26944598842810308, 107.7917661767790776, 3.849001801206918927 ) ) ;
#14037 = VERTEX_POINT ( 'NONE', #25535 ) ;
#14038 = EDGE_CURVE ( 'NONE', #5042, #48671, #47052, .T. ) ;
#14039 = CARTESIAN_POINT ( 'NONE',  ( -195.0000000000000000, 1.166476076187852838E-15, -9.524999999999991473 ) ) ;
#14040 = CARTESIAN_POINT ( 'NONE',  ( 12.34222745343792127, 149.9999999999999716, -10.18181818181818166 ) ) ;
#14041 = CARTESIAN_POINT ( 'NONE',  ( -96.35499999999997556, -4.716976649647093289, -6.492361379858945902 ) ) ;
#14042 = SURFACE_SIDE_STYLE ('',( #52723 ) ) ;
#14043 = SURFACE_SIDE_STYLE ('',( #24566 ) ) ;
#14044 = COLOUR_RGB ( '', 0.08235294, 0.09019608, 0.10196078) ;
#14045 = MECHANICAL_DESIGN_GEOMETRIC_PRESENTATION_REPRESENTATION (  '', ( #38788 ), #45521 ) ;
#14046 = CARTESIAN_POINT ( 'NONE',  ( -94.04499999999998749, 7.632228543268600340, 2.479861379858949277 ) ) ;
#14047 = CARTESIAN_POINT ( 'NONE',  ( 3.094860106618435136, 122.4049999999999727, -9.525000000000000355 ) ) ;
#14048 = CARTESIAN_POINT ( 'NONE',  ( -69.59499999999999886, 2.607480562269073321, 8.024999999999991473 ) ) ;
#14049 = FILL_AREA_STYLE_COLOUR ( '', #44386 ) ;
#14050 = CARTESIAN_POINT ( 'NONE',  ( 7.227466682572271317, 6.938893903907228378E-15, -12.50000000000000000 ) ) ;
#14051 = SURFACE_SIDE_STYLE ('',( #3433 ) ) ;
#14052 = VECTOR ( 'NONE', #3558, 1000.000000000000114 ) ;
#14053 = CARTESIAN_POINT ( 'NONE',  ( 7.750000000000000000, 33.74999999999998579, 3.750000000000000000 ) ) ;
#14054 = DIRECTION ( 'NONE',  ( 0.000000000000000000, 0.000000000000000000, 1.000000000000000000 ) ) ;
#14055 = ORIENTED_EDGE ( 'NONE', *, *, #13975, .F. ) ;
#14056 = CARTESIAN_POINT ( 'NONE',  ( -114.1429263765338078, 5.598654528085800663, -7.705886871421367523 ) ) ;
#14057 = AXIS2_PLACEMENT_3D ( 'NONE', #63531, #4781, #19913 ) ;
#14058 = CARTESIAN_POINT ( 'NONE',  ( -127.0449999999999875, 7.632228543268600340, 2.479861379858949277 ) ) ;
#14059 = CARTESIAN_POINT ( 'NONE',  ( -15.00000000000000000, -10.90871211463571022, -5.000000000000000000 ) ) ;
#14060 = ADVANCED_FACE ( 'NONE', ( #69501 ), #36853, .T. ) ;
#14061 = DIRECTION ( 'NONE',  ( -1.000000000000000000, -0.000000000000000000, -0.000000000000000000 ) ) ;
#14063 = DIRECTION ( 'NONE',  ( 0.000000000000000000, -1.224646799147353454E-16, 1.000000000000000000 ) ) ;
#14062 = CARTESIAN_POINT ( 'NONE',  ( 6.826472737025119919, 135.0070736234661126, 4.959722759717908325 ) ) ;
#14064 = DIRECTION ( 'NONE',  ( 0.000000000000000000, -1.000000000000000000, 0.000000000000000000 ) ) ;
#14065 = ORIENTED_EDGE ( 'NONE', *, *, #10511, .F. ) ;
#14066 = ORIENTED_EDGE ( 'NONE', *, *, #39521, .F. ) ;
#14067 = LINE ( 'NONE', #67888, #63406 ) ;
#14068 = EDGE_CURVE ( 'NONE', #30995, #50360, #45830, .T. ) ;
#14069 = VECTOR ( 'NONE', #27822, 1000.000000000000000 ) ;
#14070 = AXIS2_PLACEMENT_3D ( 'NONE', #34292, #56083, #66288 ) ;
#14071 = DIRECTION ( 'NONE',  ( 0.000000000000000000, 0.9396926207859082059, 0.3420201433256693790 ) ) ;
#14072 = DIRECTION ( 'NONE',  ( 0.000000000000000000, 1.000000000000000000, 0.000000000000000000 ) ) ;
#14073 = CARTESIAN_POINT ( 'NONE',  ( -6.062177826491072175, -3.499999999999998668, 0.000000000000000000 ) ) ;
#14074 = ORIENTED_EDGE ( 'NONE', *, *, #33430, .F. ) ;
#14075 = CARTESIAN_POINT ( 'NONE',  ( -134.4549999999999841, 7.632228543268599452, -2.479861379858951942 ) ) ;
#14076 = ORIENTED_EDGE ( 'NONE', *, *, #39579, .F. ) ;
#14077 = CIRCLE ( 'NONE', #43362, 0.2500000000000002220 ) ;
#14078 = DIRECTION ( 'NONE',  ( -1.000000000000000000, 0.000000000000000000, 0.000000000000000000 ) ) ;
#14079 = CARTESIAN_POINT ( 'NONE',  ( -124.4070736234661751, 3.094860106618428031, -9.524999999999993250 ) ) ;
#14080 = ORIENTED_EDGE ( 'NONE', *, *, #21828, .T. ) ;
#14081 = CARTESIAN_POINT ( 'NONE',  ( 0.000000000000000000, 42.00000000000000000, -36.49999999999999289 ) ) ;
#14082 = CARTESIAN_POINT ( 'NONE',  ( 60.00000000000000000, 1.797044900979284448E-15, -10.00000000000000000 ) ) ;
#14083 = ORIENTED_EDGE ( 'NONE', *, *, #67914, .F. ) ;
#14084 = EDGE_CURVE ( 'NONE', #13277, #24594, #42684, .T. ) ;
#14085 = AXIS2_PLACEMENT_3D ( 'NONE', #44990, #23163, #17221 ) ;
#14086 = CIRCLE ( 'NONE', #69124, 0.2500000000000002220 ) ;
#14087 = CARTESIAN_POINT ( 'NONE',  ( -4.041451884327381450, 7.000000000000006217, 7.500000000000000000 ) ) ;
#14088 = CARTESIAN_POINT ( 'NONE',  ( -5.598654528085806881, 136.7449999999999761, -7.705886871421374629 ) ) ;
#14089 = CYLINDRICAL_SURFACE ( 'NONE', #20529, 5.000000000000004441 ) ;
#14090 = ORIENTED_EDGE ( 'NONE', *, *, #67171, .F. ) ;
#14091 = DIRECTION ( 'NONE',  ( -0.000000000000000000, -0.000000000000000000, -1.000000000000000000 ) ) ;
#14092 = CARTESIAN_POINT ( 'NONE',  ( 8.102448949553179958, 139.5049999999999955, 5.886773742842750679 ) ) ;
#14093 = DIRECTION ( 'NONE',  ( 0.000000000000000000, 1.000000000000000000, 0.000000000000000000 ) ) ;
#14094 = EDGE_CURVE ( 'NONE', #53491, #33122, #7223, .T. ) ;
#14095 =( NAMED_UNIT ( * ) SI_UNIT ( $, .STERADIAN. ) SOLID_ANGLE_UNIT ( ) );
#14096 = ORIENTED_EDGE ( 'NONE', *, *, #26703, .T. ) ;
#14097 = CARTESIAN_POINT ( 'NONE',  ( -6.826472737025120807, 111.9929263765338021, 4.959722759717906548 ) ) ;
#14098 = FILL_AREA_STYLE_COLOUR ( '', #32253 ) ;
#14099 = FILL_AREA_STYLE ('',( #18418 ) ) ;
#14100 = DIRECTION ( 'NONE',  ( 1.000000000000000000, 0.000000000000000000, -0.000000000000000000 ) ) ;
#14101 =( LENGTH_UNIT ( ) NAMED_UNIT ( * ) SI_UNIT ( .MILLI., .METRE. ) );
#14102 = AXIS2_PLACEMENT_3D ( 'NONE', #20102, #14868, #36352 ) ;
#14103 = CARTESIAN_POINT ( 'NONE',  ( -19.49999999999997513, 8.000000000000000000, -4.000000000000000000 ) ) ;
#14104 = ORIENTED_EDGE ( 'NONE', *, *, #55026, .T. ) ;
#14105 = PRESENTATION_LAYER_ASSIGNMENT (  '', '', ( #68044 ) ) ;
#14106 = CARTESIAN_POINT ( 'NONE',  ( -4.377616827404060551, -9.000000000000007105, 1.000745235317158643 ) ) ;
#14107 = EDGE_LOOP ( 'NONE', ( #69203, #55235, #43617 ) ) ;
#14108 = CARTESIAN_POINT ( 'NONE',  ( -60.70461754965443646, -7.499999999999993783, 1.000000000000000000 ) ) ;
#14109 = CARTESIAN_POINT ( 'NONE',  ( 23.50000000000001776, 42.00000000000000000, -29.68999999999999417 ) ) ;
#14110 = CARTESIAN_POINT ( 'NONE',  ( -154.1049999999999898, -6.826472737025115478, 4.959722759717900331 ) ) ;
#14111 = ORIENTED_EDGE ( 'NONE', *, *, #46454, .T. ) ;
#14112 = DIRECTION ( 'NONE',  ( 1.000000000000000000, -0.000000000000000000, -0.000000000000000000 ) ) ;
#14113 =( GEOMETRIC_REPRESENTATION_CONTEXT ( 3 ) GLOBAL_UNCERTAINTY_ASSIGNED_CONTEXT ( ( #62227 ) ) GLOBAL_UNIT_ASSIGNED_CONTEXT ( ( #49297, #40148, #7068 ) ) REPRESENTATION_CONTEXT ( 'NONE', 'WORKASPACE' ) );
#14114 = PRESENTATION_LAYER_ASSIGNMENT (  '', '', ( #8499 ) ) ;
#14115 = CARTESIAN_POINT ( 'NONE',  ( -57.11974195712091529, -8.499999999999996447, 7.999999999999976019 ) ) ;
#14116 = LINE ( 'NONE', #35574, #66243 ) ;
#14117 = ORIENTED_EDGE ( 'NONE', *, *, #13975, .T. ) ;
#14118 = LINE ( 'NONE', #51759, #30806 ) ;
#14119 = ORIENTED_EDGE ( 'NONE', *, *, #33752, .T. ) ;
#14120 = CARTESIAN_POINT ( 'NONE',  ( 1.000000000000000000, 42.00000000000000000, -79.00402776293826435 ) ) ;
#14121 = CARTESIAN_POINT ( 'NONE',  ( -74.99999999999998579, 50.00000000000000000, 7.500000000000000000 ) ) ;
#14122 = CARTESIAN_POINT ( 'NONE',  ( -79.70499999999995566, 2.607480562269073321, 8.024999999999991473 ) ) ;
#14123 = ORIENTED_EDGE ( 'NONE', *, *, #56962, .F. ) ;
#14124 = DIRECTION ( 'NONE',  ( -1.000000000000000000, 0.000000000000000000, 0.000000000000000000 ) ) ;
#14125 = LINE ( 'NONE', #25689, #16097 ) ;
#14126 = LINE ( 'NONE', #9899, #10615 ) ;
#14127 = ORIENTED_EDGE ( 'NONE', *, *, #61868, .T. ) ;
#14128 = EDGE_CURVE ( 'NONE', #22128, #16768, #11447, .T. ) ;
#14129 = APPLICATION_CONTEXT ( 'automotive_design' ) ;
#14130 = STYLED_ITEM ( 'NONE', ( #10487 ), #8375 ) ;
#14131 = CARTESIAN_POINT ( 'NONE',  ( -74.17525885966198018, 9.083251256839373511, -6.320036396439323134 ) ) ;
#14132 =( NAMED_UNIT ( * ) PLANE_ANGLE_UNIT ( ) SI_UNIT ( $, .RADIAN. ) );
#14133 = CARTESIAN_POINT ( 'NONE',  ( -34.31243252642735087, -10.02680648607962510, -3.499999999999997335 ) ) ;
#14134 = LINE ( 'NONE', #62636, #39101 ) ;
#14135 = CARTESIAN_POINT ( 'NONE',  ( -1.166476076187854022E-15, 134.9449999999999932, 9.525000000000000355 ) ) ;
#14136 = CARTESIAN_POINT ( 'NONE',  ( -97.04499999999998749, 7.632228543268600340, 2.479861379858949277 ) ) ;
#14137 = PRESENTATION_STYLE_ASSIGNMENT (( #56699 ) ) ;
#14138 = CIRCLE ( 'NONE', #59059, 5.000000000000004441 ) ;
#14139 = AXIS2_PLACEMENT_3D ( 'NONE', #12891, #50882, #34354 ) ;
#14140 = CARTESIAN_POINT ( 'NONE',  ( 22.75000000000000711, 36.75000000000000000, -4.000000000000000000 ) ) ;
#14141 = CARTESIAN_POINT ( 'NONE',  ( -23.21231517720798010, 117.4999999999999716, -9.500000000000000000 ) ) ;
#14142 = ORIENTED_EDGE ( 'NONE', *, *, #33871, .F. ) ;
#14143 = CARTESIAN_POINT ( 'NONE',  ( -144.8929263765338362, -8.102448949553172852, -5.886773742842741797 ) ) ;
#14144 = CARTESIAN_POINT ( 'NONE',  ( -152.9950000000000045, -6.826472737025115478, 4.959722759717900331 ) ) ;
#14145 = EDGE_CURVE ( 'NONE', #40918, #29858, #37897, .T. ) ;
#14146 = VECTOR ( 'NONE', #67902, 1000.000000000000000 ) ;
#14147 = ADVANCED_FACE ( 'NONE', ( #50146 ), #6495, .T. ) ;
#14148 = CIRCLE ( 'NONE', #567, 0.2500000000000002220 ) ;
#14149 = DIRECTION ( 'NONE',  ( 0.000000000000000000, 0.000000000000000000, -1.000000000000000000 ) ) ;
#14150 = ORIENTED_EDGE ( 'NONE', *, *, #37482, .T. ) ;
#14151 = DIRECTION ( 'NONE',  ( 1.000000000000000000, 0.000000000000000000, 0.000000000000000000 ) ) ;
#14152 = VERTEX_POINT ( 'NONE', #59265 ) ;
#14153 = AXIS2_PLACEMENT_3D ( 'NONE', #32660, #48553, #16534 ) ;
#14154 = CARTESIAN_POINT ( 'NONE',  ( 60.00000000000000000, 1.797044900979284448E-15, -7.000000000000017764 ) ) ;
#14155 = SHAPE_REPRESENTATION ( '4. Adjustment Screw', ( #42840 ), #4621 ) ;
#14156 = EDGE_CURVE ( 'NONE', #47284, #65666, #43176, .T. ) ;
#14157 = DIRECTION ( 'NONE',  ( 0.000000000000000000, 0.000000000000000000, 1.000000000000000000 ) ) ;
#14158 = CARTESIAN_POINT ( 'NONE',  ( -45.00000000000000000, 8.456227461324044015, 6.943431694471519755 ) ) ;
#14159 = CARTESIAN_POINT ( 'NONE',  ( -110.3070736234661666, -10.01517768586948698, 6.132527647946031529E-16 ) ) ;
#14160 = ADVANCED_FACE ( 'NONE', ( #64906 ), #16756, .F. ) ;
#14161 = CARTESIAN_POINT ( 'NONE',  ( -71.75000000000000000, -0.9999999999999995559, 20.00000000000000000 ) ) ;
#14162 = ORIENTED_EDGE ( 'NONE', *, *, #26056, .T. ) ;
#14163 = CARTESIAN_POINT ( 'NONE',  ( -159.2049999999999841, -2.607480562269071545, -8.024999999999991473 ) ) ;
#14164 = EDGE_LOOP ( 'NONE', ( #38074, #68269, #24095, #53454, #1292, #44530, #41118 ) ) ;
#14165 = LINE ( 'NONE', #56357, #66106 ) ;
#14166 = DIRECTION ( 'NONE',  ( 0.000000000000000000, 0.000000000000000000, 1.000000000000000000 ) ) ;
#14167 = ORIENTED_EDGE ( 'NONE', *, *, #53279, .T. ) ;
#14168 = EDGE_CURVE ( 'NONE', #46059, #25577, #23058, .T. ) ;
#14169 = CARTESIAN_POINT ( 'NONE',  ( 1.000000000000000000, 0.000000000000000000, -79.00402776293826435 ) ) ;
#14170 = CARTESIAN_POINT ( 'NONE',  ( -58.25707362346617657, 5.598654528085800663, -7.705886871421367523 ) ) ;
#14171 = CARTESIAN_POINT ( 'NONE',  ( -9.058813317711338797, 110.3449999999999847, 2.943386871421373563 ) ) ;
#14172 = MECHANICAL_DESIGN_GEOMETRIC_PRESENTATION_REPRESENTATION (  '', ( #60213 ), #50081 ) ;
#14173 = ORIENTED_EDGE ( 'NONE', *, *, #47455, .T. ) ;
#14174 = CARTESIAN_POINT ( 'NONE',  ( -58.19292637653381206, -10.01517768586948698, 6.132527647946031529E-16 ) ) ;
#14175 = CARTESIAN_POINT ( 'NONE',  ( -74.99999999999998579, 50.00000000000000000, 10.50000000000000000 ) ) ;
#14176 = CARTESIAN_POINT ( 'NONE',  ( -70.55499999999999261, 0.000000000000000000, 8.024999999999991473 ) ) ;
#14177 = ADVANCED_FACE ( 'NONE', ( #2204 ), #51176, .F. ) ;
#14178 = CARTESIAN_POINT ( 'NONE',  ( -40.78947368421051323, 108.1536491499103505, -3.000000000000005773 ) ) ;
#14179 = VERTEX_POINT ( 'NONE', #14229 ) ;
#14180 = CARTESIAN_POINT ( 'NONE',  ( -8.102448949553181734, 141.0049999999999386, -5.886773742842749790 ) ) ;
#14181 = DIRECTION ( 'NONE',  ( 0.000000000000000000, 0.000000000000000000, 1.000000000000000000 ) ) ;
#14182 = AXIS2_PLACEMENT_3D ( 'NONE', #22398, #27302, #65312 ) ;
#14183 =( NAMED_UNIT ( * ) SI_UNIT ( $, .STERADIAN. ) SOLID_ANGLE_UNIT ( ) );
#14184 = CIRCLE ( 'NONE', #5214, 1.000000000000000888 ) ;
#14185 = EDGE_LOOP ( 'NONE', ( #58156, #37787, #58043, #51362 ) ) ;
#14186 = SURFACE_STYLE_FILL_AREA ( #8567 ) ;
#14187 = LINE ( 'NONE', #63412, #42949 ) ;
#14188 = CARTESIAN_POINT ( 'NONE',  ( -57.44499999999999318, 0.000000000000000000, 8.024999999999991473 ) ) ;
#14189 = ORIENTED_EDGE ( 'NONE', *, *, #50517, .T. ) ;
#14190 = CARTESIAN_POINT ( 'NONE',  ( 6.240333192270946405, 111.1483426130140515, 6.318785644388214884 ) ) ;
#14191 = CARTESIAN_POINT ( 'NONE',  ( 6.767634268437461742, 2.367558512213881805, -2.278113600022080298 ) ) ;
#14192 = DIRECTION ( 'NONE',  ( 1.156482317317873451E-16, -1.000000000000000000, -0.000000000000000000 ) ) ;
#14193 = DIRECTION ( 'NONE',  ( 0.000000000000000000, 0.000000000000000000, -1.000000000000000000 ) ) ;
#14194 = ORIENTED_EDGE ( 'NONE', *, *, #35912, .T. ) ;
#14195 = FILL_AREA_STYLE ('',( #34948 ) ) ;
#14196 = ORIENTED_EDGE ( 'NONE', *, *, #64155, .T. ) ;
#14197 = CARTESIAN_POINT ( 'NONE',  ( -106.8549999999999898, 4.716976649647094177, 6.492361379858945902 ) ) ;
#14198 = ORIENTED_EDGE ( 'NONE', *, *, #4801, .F. ) ;
#14199 = DIRECTION ( 'NONE',  ( -1.982541115402069054E-16, -0.000000000000000000, 1.000000000000000000 ) ) ;
#14200 = CYLINDRICAL_SURFACE ( 'NONE', #35909, 0.2500000000000002220 ) ;
#14201 = AXIS2_PLACEMENT_3D ( 'NONE', #67305, #19092, #7182 ) ;
#14202 = CARTESIAN_POINT ( 'NONE',  ( -139.7070736234661865, -3.094860106618431139, -9.524999999999991473 ) ) ;
#14203 = CARTESIAN_POINT ( 'NONE',  ( 9.058813317711338797, 144.8449999999999989, -2.943386871421372675 ) ) ;
#14204 = CARTESIAN_POINT ( 'NONE',  ( -79.55707362346616662, -1.166476076187852838E-15, -9.524999999999991473 ) ) ;
#14205 = EDGE_CURVE ( 'NONE', #16875, #9166, #36955, .T. ) ;
#14206 = CARTESIAN_POINT ( 'NONE',  ( -4.750000000000002665, 24.74999999999998579, -3.750000000000000000 ) ) ;
#14207 = ORIENTED_EDGE ( 'NONE', *, *, #7292, .T. ) ;
#14208 = DIRECTION ( 'NONE',  ( 0.000000000000000000, 0.000000000000000000, -1.000000000000000000 ) ) ;
#14209 = B_SPLINE_CURVE_WITH_KNOTS ( 'NONE', 3,
 ( #64289, #30892, #52718, #5194, #26636, #4857 ),
 .UNSPECIFIED., .F., .F.,
 ( 4, 2, 4 ),
 ( 0.005386537104126985082, 0.008060814333094825507, 0.01073509156206266767 ),
 .UNSPECIFIED. ) ;
#14210 = CARTESIAN_POINT ( 'NONE',  ( -18.76557388412283345, -11.53827662439787005, -3.305441448926072390 ) ) ;
#14211 = CARTESIAN_POINT ( 'NONE',  ( 2.607480562269107072, 120.9070736234661609, -8.024999999999979039 ) ) ;
#14212 = CARTESIAN_POINT ( 'NONE',  ( -124.2549999999999955, -4.716976649647092401, 6.492361379858946790 ) ) ;
#14213 = SURFACE_STYLE_USAGE ( .BOTH. , #62032 ) ;
#14214 = CARTESIAN_POINT ( 'NONE',  ( -8.102448949553181734, 112.8949999999999818, -5.886773742842749790 ) ) ;
#14215 = CARTESIAN_POINT ( 'NONE',  ( -121.7949999999999875, 2.607480562269068880, -8.024999999999993250 ) ) ;
#14216 = CARTESIAN_POINT ( 'NONE',  ( -118.1949999999999790, 8.437984349512086979, -1.550032578732815448E-15 ) ) ;
#14217 = CARTESIAN_POINT ( 'NONE',  ( 48.50000000000000000, 14.49137674618942562, -9.500000000000000000 ) ) ;
#14218 = ORIENTED_EDGE ( 'NONE', *, *, #6667, .T. ) ;
#14219 =( LENGTH_UNIT ( ) NAMED_UNIT ( * ) SI_UNIT ( .MILLI., .METRE. ) );
#14220 = EDGE_CURVE ( 'NONE', #13679, #50952, #67007, .T. ) ;
#14221 = LINE ( 'NONE', #31073, #50745 ) ;
#14222 = CARTESIAN_POINT ( 'NONE',  ( -170.2429263765338305, 5.598654528085804216, 7.705886871421366635 ) ) ;
#14223 = EDGE_CURVE ( 'NONE', #18076, #62248, #66076, .T. ) ;
#14224 = MECHANICAL_DESIGN_GEOMETRIC_PRESENTATION_REPRESENTATION (  '', ( #9766 ), #32197 ) ;
#14225 = EDGE_CURVE ( 'NONE', #41529, #30954, #29345, .T. ) ;
#14226 = EDGE_CURVE ( 'NONE', #13735, #9516, #42534, .T. ) ;
#14227 =( GEOMETRIC_REPRESENTATION_CONTEXT ( 3 ) GLOBAL_UNCERTAINTY_ASSIGNED_CONTEXT ( ( #24795 ) ) GLOBAL_UNIT_ASSIGNED_CONTEXT ( ( #24519, #19247, #63568 ) ) REPRESENTATION_CONTEXT ( 'NONE', 'WORKASPACE' ) );
#14228 = CARTESIAN_POINT ( 'NONE',  ( 98.00000000000000000, 16.00000000000000000, 0.000000000000000000 ) ) ;
#14229 = CARTESIAN_POINT ( 'NONE',  ( 66.24999999999998579, 33.74999999999999289, 4.000000000000000000 ) ) ;
#14230 = CARTESIAN_POINT ( 'NONE',  ( 0.000000000000000000, 30.74999999999999289, 4.000000000000000000 ) ) ;
#14231 = ORIENTED_EDGE ( 'NONE', *, *, #64564, .T. ) ;
#14232 = CARTESIAN_POINT ( 'NONE',  ( -89.24292637653380211, 5.598654528085804216, 7.705886871421366635 ) ) ;
#14233 =( NAMED_UNIT ( * ) PLANE_ANGLE_UNIT ( ) SI_UNIT ( $, .RADIAN. ) );
#14234 = DIRECTION ( 'NONE',  ( -0.000000000000000000, -1.000000000000000000, -0.000000000000000000 ) ) ;
#14235 = CARTESIAN_POINT ( 'NONE',  ( -178.9429263765338192, 0.000000000000000000, 9.524999999999991473 ) ) ;
#14237 = FACE_OUTER_BOUND ( 'NONE', #5427, .T. ) ;
#14236 =( BOUNDED_CURVE ( )  B_SPLINE_CURVE ( 2, ( #44025, #38747, #60154, #65782, #39084, #44716, #17936, #18291, #50641, #8073, #58555 ),
 .UNSPECIFIED., .F., .F. ) 
 B_SPLINE_CURVE_WITH_KNOTS ( ( 3, 2, 2, 2, 2, 3 ),
 ( 0.5882352941176473005, 0.5941176470588237502, 0.6000000000000001998, 0.6058823529411767606, 0.6117647058823533213, 0.6176470588235297710 ),
 .UNSPECIFIED. ) 
 CURVE ( )  GEOMETRIC_REPRESENTATION_ITEM ( )  RATIONAL_B_SPLINE_CURVE ( ( 0.9999999999999981126, 0.9510565162951554186, 1.000000000000000000, 0.9510565162951535312, 1.000000000000000000, 0.9510565162951535312, 1.000000000000000000, 0.9510565162951535312, 1.000000000000000000, 0.9510565162951507556, 1.000000000000002665 ) ) 
 REPRESENTATION_ITEM ( '' )  );
#14238 = DIRECTION ( 'NONE',  ( 0.000000000000000000, 0.000000000000000000, -1.000000000000000000 ) ) ;
#14239 = ADVANCED_FACE ( 'NONE', ( #67339 ), #28987, .F. ) ;
#14240 = ORIENTED_EDGE ( 'NONE', *, *, #20051, .T. ) ;
#14241 = CARTESIAN_POINT ( 'NONE',  ( 3.000000000000002665, 43.00000000000000000, -90.00000000000000000 ) ) ;
#14242 = FACE_OUTER_BOUND ( 'NONE', #43470, .T. ) ;
#14243 = ORIENTED_EDGE ( 'NONE', *, *, #45130, .F. ) ;
#14244 = DIRECTION ( 'NONE',  ( 0.000000000000000000, 0.000000000000000000, 1.000000000000000000 ) ) ;
#14245 = CARTESIAN_POINT ( 'NONE',  ( -6.826472737025120807, 136.5070736234661410, -4.959722759717907437 ) ) ;
#14246 = DIRECTION ( 'NONE',  ( 1.000000000000000000, 0.000000000000000000, 0.000000000000000000 ) ) ;
#14247 = EDGE_LOOP ( 'NONE', ( #69529, #11152, #30136, #11030, #65413, #16880, #22777 ) ) ;
#14248 =( NAMED_UNIT ( * ) PLANE_ANGLE_UNIT ( ) SI_UNIT ( $, .RADIAN. ) );
#14249 = CARTESIAN_POINT ( 'NONE',  ( -107.0049999999999955, 6.826472737025115478, 4.959722759717899443 ) ) ;
#14250 = CIRCLE ( 'NONE', #44627, 17.50000000000000000 ) ;
#14251 = ORIENTED_EDGE ( 'NONE', *, *, #25060, .F. ) ;
#14252 =( LENGTH_UNIT ( ) NAMED_UNIT ( * ) SI_UNIT ( .MILLI., .METRE. ) );
#14253 = CARTESIAN_POINT ( 'NONE',  ( -4.041451884327380562, -1.417096231345237545, -7.000000000000003553 ) ) ;
#14254 = CARTESIAN_POINT ( 'NONE',  ( 0.000000000000000000, 151.0570736234661524, -8.025000000000000355 ) ) ;
#14255 = EDGE_CURVE ( 'NONE', #15573, #50024, #8267, .T. ) ;
#14256 = CARTESIAN_POINT ( 'NONE',  ( -30.38025804287905629, -8.499999999999996447, 8.000000000000000000 ) ) ;
#14257 = ADVANCED_FACE ( 'NONE', ( #30044 ), #51504, .F. ) ;
#14258 = CARTESIAN_POINT ( 'NONE',  ( -80.69499999999999318, -8.437984349512085203, 5.166775262442717831E-16 ) ) ;
#14259 = ORIENTED_EDGE ( 'NONE', *, *, #21567, .T. ) ;
#14260 = DIRECTION ( 'NONE',  ( 1.000000000000000000, 0.000000000000000000, 0.000000000000000000 ) ) ;
#14261 =( LENGTH_UNIT ( ) NAMED_UNIT ( * ) SI_UNIT ( .MILLI., .METRE. ) );
#14262 = UNCERTAINTY_MEASURE_WITH_UNIT (LENGTH_MEASURE( 1.000000000000000082E-05 ), #2712, 'distance_accuracy_value', 'NONE');
#14263 = EDGE_LOOP ( 'NONE', ( #63314, #60583, #16993, #57720 ) ) ;
#14264 = PRESENTATION_STYLE_ASSIGNMENT (( #56119 ) ) ;
#14265 = AXIS2_PLACEMENT_3D ( 'NONE', #39226, #40523, #61936 ) ;
#14266 = DIRECTION ( 'NONE',  ( 0.000000000000000000, 0.000000000000000000, 1.000000000000000000 ) ) ;
#14267 = CARTESIAN_POINT ( 'NONE',  ( -47.75499999999999545, 4.716976649647091513, -6.492361379858946790 ) ) ;
#14268 = ORIENTED_EDGE ( 'NONE', *, *, #14255, .F. ) ;
#14269 = AXIS2_PLACEMENT_3D ( 'NONE', #42355, #10301, #21174 ) ;
#14270 = SURFACE_STYLE_USAGE ( .BOTH. , #24454 ) ;
#14271 = VERTEX_POINT ( 'NONE', #44887 ) ;
#14272 = MECHANICAL_DESIGN_GEOMETRIC_PRESENTATION_REPRESENTATION (  '', ( #5272 ), #62563 ) ;
#14273 = DIRECTION ( 'NONE',  ( -1.000000000000000000, 0.000000000000000000, 0.000000000000000000 ) ) ;
#14274 = CARTESIAN_POINT ( 'NONE',  ( 4.041451884327377897, -1.417096231345241097, 7.000000000000000888 ) ) ;
#14275 = CARTESIAN_POINT ( 'NONE',  ( -171.6570736234661751, 9.058813317711329915, 2.943386871421369566 ) ) ;
#14276 = CARTESIAN_POINT ( 'NONE',  ( -8.102448949553179958, 115.8949999999999818, -5.886773742842749790 ) ) ;
#14277 = CARTESIAN_POINT ( 'NONE',  ( -108.5070736234661695, 8.102448949553176405, 5.886773742842740909 ) ) ;
#14278 = CARTESIAN_POINT ( 'NONE',  ( -65.15707362346617515, -9.058813317711329915, -2.943386871421370898 ) ) ;
#14279 = ORIENTED_EDGE ( 'NONE', *, *, #41816, .F. ) ;
#14280 = CARTESIAN_POINT ( 'NONE',  ( -108.1429263765338078, 5.598654528085800663, -7.705886871421367523 ) ) ;
#14281 = CARTESIAN_POINT ( 'NONE',  ( -82.94292637653380496, 0.000000000000000000, 9.524999999999991473 ) ) ;
#14283 = CARTESIAN_POINT ( 'NONE',  ( 1.224646799147353256E-15, 0.000000000000000000, 10.00000000000000000 ) ) ;
#14282 = SPHERICAL_SURFACE ( 'NONE', #66024, 0.2500000000000000000 ) ;
#14284 = FILL_AREA_STYLE ('',( #31138 ) ) ;
#14285 = CIRCLE ( 'NONE', #49120, 5.000000000000000888 ) ;
#14286 = CARTESIAN_POINT ( 'NONE',  ( -150.2049999999999841, -2.607480562269071545, -8.024999999999991473 ) ) ;
#14287 = CARTESIAN_POINT ( 'NONE',  ( -148.0429263765338135, -9.058813317711329915, -2.943386871421370898 ) ) ;
#14288 = EDGE_CURVE ( 'NONE', #30516, #31691, #55991, .T. ) ;
#14289 = CARTESIAN_POINT ( 'NONE',  ( -152.3950000000000102, -6.826472737025115478, -4.959722759717899443 ) ) ;
#14290 = CARTESIAN_POINT ( 'NONE',  ( -148.1949999999999932, 8.437984349512086979, -1.550032578732815448E-15 ) ) ;
#14291 = ORIENTED_EDGE ( 'NONE', *, *, #39509, .T. ) ;
#14292 = LINE ( 'NONE', #42128, #12268 ) ;
#14293 = DIRECTION ( 'NONE',  ( 0.000000000000000000, 0.000000000000000000, 1.000000000000000000 ) ) ;
#14294 = EDGE_CURVE ( 'NONE', #4798, #21468, #36910, .T. ) ;
#14295 = LINE ( 'NONE', #35057, #55195 ) ;
#14296 = UNCERTAINTY_MEASURE_WITH_UNIT (LENGTH_MEASURE( 1.000000000000000082E-05 ), #11571, 'distance_accuracy_value', 'NONE');
#14297 = CARTESIAN_POINT ( 'NONE',  ( -60.80499999999998550, -8.437984349512085203, 5.166775262442717831E-16 ) ) ;
#14298 = CARTESIAN_POINT ( 'NONE',  ( -34.99999999999999289, 99.99999999999998579, -3.500000000000000000 ) ) ;
#14299 = EDGE_CURVE ( 'NONE', #34430, #5028, #9972, .T. ) ;
#14300 = CARTESIAN_POINT ( 'NONE',  ( -63.29499999999998749, -2.607480562269069768, 8.024999999999991473 ) ) ;
#14301 = CARTESIAN_POINT ( 'NONE',  ( -8.102448949553181734, 156.6049999999999329, 5.886773742842747126 ) ) ;
#14302 = LINE ( 'NONE', #25204, #39897 ) ;
#14303 = LINE ( 'NONE', #50904, #48107 ) ;
#14304 = UNCERTAINTY_MEASURE_WITH_UNIT (LENGTH_MEASURE( 1.000000000000000082E-05 ), #23991, 'distance_accuracy_value', 'NONE');
#14305 = DIRECTION ( 'NONE',  ( 1.143371202829814718E-15, -0.9999999999999998890, 5.551115123125782702E-17 ) ) ;
#14306 = DIRECTION ( 'NONE',  ( 0.000000000000000000, -1.000000000000000000, 0.000000000000000000 ) ) ;
#14307 = CARTESIAN_POINT ( 'NONE',  ( 1.000000000000000000, 36.74999999999999289, 4.000000000000000000 ) ) ;
#14308 =( NAMED_UNIT ( * ) PLANE_ANGLE_UNIT ( ) SI_UNIT ( $, .RADIAN. ) );
#14309 = VECTOR ( 'NONE', #36182, 1000.000000000000114 ) ;
#14310 = CIRCLE ( 'NONE', #64868, 0.5000000000000004441 ) ;
#14311 = EDGE_CURVE ( 'NONE', #34405, #54990, #44793, .T. ) ;
#14312 = SURFACE_SIDE_STYLE ('',( #46365 ) ) ;
#14313 = VECTOR ( 'NONE', #9540, 1000.000000000000000 ) ;
#14314 = CARTESIAN_POINT ( 'NONE',  ( 0.000000000000000000, 154.9999999999999716, 0.000000000000000000 ) ) ;
#14315 = LINE ( 'NONE', #20279, #8166 ) ;
#14316 = ORIENTED_EDGE ( 'NONE', *, *, #6491, .F. ) ;
#14317 = VERTEX_POINT ( 'NONE', #25123 ) ;
#14318 = CARTESIAN_POINT ( 'NONE',  ( 32.00000000000000000, 50.00000000000000000, -60.00000000000000711 ) ) ;
#14319 = CARTESIAN_POINT ( 'NONE',  ( -4.716976649647097730, 109.3570736234661496, -6.492361379858953896 ) ) ;
#14320 = DIRECTION ( 'NONE',  ( 1.000000000000000000, 0.000000000000000000, 0.000000000000000000 ) ) ;
#14321 = ORIENTED_EDGE ( 'NONE', *, *, #53226, .F. ) ;
#14322 = ORIENTED_EDGE ( 'NONE', *, *, #37380, .T. ) ;
#14323 = CIRCLE ( 'NONE', #54727, 0.5000000000000004441 ) ;
#14324 = DIRECTION ( 'NONE',  ( 1.000000000000000000, -0.000000000000000000, 0.000000000000000000 ) ) ;
#14325 = ORIENTED_EDGE ( 'NONE', *, *, #64658, .T. ) ;
#14326 = DIRECTION ( 'NONE',  ( -0.000000000000000000, -0.000000000000000000, -1.000000000000000000 ) ) ;
#14327 = CARTESIAN_POINT ( 'NONE',  ( 22.00000000000002132, 43.00000000000000000, 90.00000000000000000 ) ) ;
#14328 = ORIENTED_EDGE ( 'NONE', *, *, #68478, .T. ) ;
#14329 = DIRECTION ( 'NONE',  ( 0.000000000000000000, 0.000000000000000000, 1.000000000000000000 ) ) ;
#14330 = CARTESIAN_POINT ( 'NONE',  ( -111.5949999999999704, 2.607480562269073321, 8.024999999999991473 ) ) ;
#14331 = ORIENTED_EDGE ( 'NONE', *, *, #13254, .F. ) ;
#14332 = LINE ( 'NONE', #51283, #38967 ) ;
#14333 = DIRECTION ( 'NONE',  ( 1.000000000000000000, 0.000000000000000000, 0.000000000000000000 ) ) ;
#14334 = ORIENTED_EDGE ( 'NONE', *, *, #46016, .T. ) ;
#14335 = CARTESIAN_POINT ( 'NONE',  ( 0.000000000000000000, 149.9429263765338476, -8.025000000000000355 ) ) ;
#14336 = PRESENTATION_STYLE_ASSIGNMENT (( #3032 ) ) ;
#14337 =( LENGTH_UNIT ( ) NAMED_UNIT ( * ) SI_UNIT ( .MILLI., .METRE. ) );
#14338 = CARTESIAN_POINT ( 'NONE',  ( 0.000000000000000000, 0.000000000000000000, 32.50000000000000000 ) ) ;
#14339 = FACE_OUTER_BOUND ( 'NONE', #62496, .T. ) ;
#14340 = EDGE_LOOP ( 'NONE', ( #38261, #49779, #55542, #30168 ) ) ;
#14341 = FILL_AREA_STYLE ('',( #25246 ) ) ;
#14342 = ORIENTED_EDGE ( 'NONE', *, *, #43114, .F. ) ;
#14343 = CARTESIAN_POINT ( 'NONE',  ( 1.000000000000000000, 36.74999999999999289, 3.000000000000000000 ) ) ;
#14344 =( NAMED_UNIT ( * ) SI_UNIT ( $, .STERADIAN. ) SOLID_ANGLE_UNIT ( ) );
#14345 = CARTESIAN_POINT ( 'NONE',  ( -157.8570736234661922, -5.598654528085803328, -7.705886871421366635 ) ) ;
#14346 = CARTESIAN_POINT ( 'NONE',  ( -119.9049999999999869, 2.607480562269068880, -8.024999999999993250 ) ) ;
#14347 = FILL_AREA_STYLE_COLOUR ( '', #69069 ) ;
#14348 = DIRECTION ( 'NONE',  ( 1.000000000000000000, 0.000000000000000000, 0.000000000000000000 ) ) ;
#14349 = MECHANICAL_DESIGN_GEOMETRIC_PRESENTATION_REPRESENTATION (  '', ( #3047 ), #44733 ) ;
#14350 = CARTESIAN_POINT ( 'NONE',  ( -125.2429263765338021, 5.598654528085804216, 7.705886871421366635 ) ) ;
#14351 = LINE ( 'NONE', #3406, #47451 ) ;
#14352 = ORIENTED_EDGE ( 'NONE', *, *, #41502, .T. ) ;
#14353 = VECTOR ( 'NONE', #16378, 1000.000000000000000 ) ;
#14354 = ORIENTED_EDGE ( 'NONE', *, *, #44675, .F. ) ;
#14355 = CARTESIAN_POINT ( 'NONE',  ( 30.99999999999999289, 5.000000000000000000, 24.00402776293822171 ) ) ;
#14356 = CARTESIAN_POINT ( 'NONE',  ( 52.75000000000000000, 25.24999999999998579, 4.000000000000000000 ) ) ;
#14357 = DIRECTION ( 'NONE',  ( -1.000000000000000000, 0.000000000000000000, 0.000000000000000000 ) ) ;
#14358 = ORIENTED_EDGE ( 'NONE', *, *, #21882, .T. ) ;
#14359 = CARTESIAN_POINT ( 'NONE',  ( -175.8549999999999898, 4.716976649647094177, 6.492361379858945902 ) ) ;
#14360 =( LENGTH_UNIT ( ) NAMED_UNIT ( * ) SI_UNIT ( .MILLI., .METRE. ) );
#14361 = FACE_OUTER_BOUND ( 'NONE', #16868, .T. ) ;
#14362 = EDGE_CURVE ( 'NONE', #31626, #31846, #18913, .T. ) ;
#14363 = CARTESIAN_POINT ( 'NONE',  ( -53.75707362346618368, -5.598654528085801552, 7.705886871421367523 ) ) ;
#14364 = AXIS2_PLACEMENT_3D ( 'NONE', #64215, #33262, #5809 ) ;
#14365 = CARTESIAN_POINT ( 'NONE',  ( -181.4949999999999761, 6.826472737025113702, -4.959722759717902107 ) ) ;
#14366 = DIRECTION ( 'NONE',  ( -0.7071067811865549002, 8.659560562355022838E-17, 0.7071067811865401342 ) ) ;
#14367 = ORIENTED_EDGE ( 'NONE', *, *, #32546, .T. ) ;
#14368 =( NAMED_UNIT ( * ) SI_UNIT ( $, .STERADIAN. ) SOLID_ANGLE_UNIT ( ) );
#14369 = PLANE ( 'NONE',  #65036 ) ;
#14370 = CARTESIAN_POINT ( 'NONE',  ( -91.25499999999999545, -4.716976649647092401, 6.492361379858946790 ) ) ;
#14371 = CARTESIAN_POINT ( 'NONE',  ( 7.647808743684392674, 154.4999999999999432, 5.677732506910178500 ) ) ;
#14372 = LINE ( 'NONE', #3794, #20234 ) ;
#14373 = AXIS2_PLACEMENT_3D ( 'NONE', #7562, #28992, #61018 ) ;
#14374 = EDGE_CURVE ( 'NONE', #65002, #61213, #31266, .T. ) ;
#14375 = CARTESIAN_POINT ( 'NONE',  ( -87.14499999999998181, -4.716976649647092401, 6.492361379858946790 ) ) ;
#14376 = CARTESIAN_POINT ( 'NONE',  ( -8.102448949553181734, 126.0049999999999812, -5.886773742842749790 ) ) ;
#14377 = CARTESIAN_POINT ( 'NONE',  ( -71.39499999999998181, -6.826472737025115478, -4.959722759717899443 ) ) ;
#14378 = EDGE_CURVE ( 'NONE', #24720, #20026, #31779, .T. ) ;
#14379 = CARTESIAN_POINT ( 'NONE',  ( 23.50000000000001776, 43.00000000000000000, 29.68999999999999417 ) ) ;
#14380 = CARTESIAN_POINT ( 'NONE',  ( -55.85707362346617799, -5.598654528085803328, -7.705886871421366635 ) ) ;
#14381 = EDGE_CURVE ( 'NONE', #24594, #34584, #47682, .T. ) ;
#14382 = UNCERTAINTY_MEASURE_WITH_UNIT (LENGTH_MEASURE( 1.000000000000000082E-05 ), #20916, 'distance_accuracy_value', 'NONE');
#14383 = FILL_AREA_STYLE_COLOUR ( '', #37179 ) ;
#14384 = ORIENTED_EDGE ( 'NONE', *, *, #26530, .T. ) ;
#14385 = EDGE_CURVE ( 'NONE', #51271, #51980, #26150, .T. ) ;
#14386 = CARTESIAN_POINT ( 'NONE',  ( -119.2429263765338021, 5.598654528085804216, 7.705886871421366635 ) ) ;
#14387 = CARTESIAN_POINT ( 'NONE',  ( -127.1949999999999932, 8.437984349512085203, -1.550032578732815448E-15 ) ) ;
#14388 = DIRECTION ( 'NONE',  ( -1.000000000000000000, 0.000000000000000000, 0.000000000000000000 ) ) ;
#14389 =( NAMED_UNIT ( * ) SI_UNIT ( $, .STERADIAN. ) SOLID_ANGLE_UNIT ( ) );
#14390 = EDGE_LOOP ( 'NONE', ( #27952, #32551, #19073, #30085 ) ) ;
#14391 = STYLED_ITEM ( 'NONE', ( #19060 ), #9712 ) ;
#14392 = EDGE_LOOP ( 'NONE', ( #29974, #56544 ) ) ;
#14393 = CARTESIAN_POINT ( 'NONE',  ( -61.94292637653379785, 0.000000000000000000, 9.524999999999991473 ) ) ;
#14394 = UNCERTAINTY_MEASURE_WITH_UNIT (LENGTH_MEASURE( 1.000000000000000082E-05 ), #25620, 'distance_accuracy_value', 'NONE');
#14395 = DIRECTION ( 'NONE',  ( 0.000000000000000000, 0.000000000000000000, 1.000000000000000000 ) ) ;
#14396 = LINE ( 'NONE', #14772, #2174 ) ;
#14397 = TOROIDAL_SURFACE ( 'NONE', #22292, 1.000000000000000000, 0.5000000000000000000 ) ;
#14398 = SURFACE_SIDE_STYLE ('',( #19684 ) ) ;
#14400 = CARTESIAN_POINT ( 'NONE',  ( -14.98999599679679662, 146.4999999999999716, 10.00000000000000000 ) ) ;
#14399 = AXIS2_PLACEMENT_3D ( 'NONE', #42117, #16050, #48416 ) ;
#14401 = ORIENTED_EDGE ( 'NONE', *, *, #28329, .T. ) ;
#14402 = CARTESIAN_POINT ( 'NONE',  ( -126.9549999999999841, -7.632228543268599452, 2.479861379858951054 ) ) ;
#14403 = VERTEX_POINT ( 'NONE', #46636 ) ;
#14404 = CARTESIAN_POINT ( 'NONE',  ( -124.7070736234661723, -3.094860106618431139, -9.524999999999991473 ) ) ;
#14405 = ORIENTED_EDGE ( 'NONE', *, *, #12377, .F. ) ;
#14406 = CARTESIAN_POINT ( 'NONE',  ( -4.041451884327381450, 7.000000000000006217, 7.500000000000000000 ) ) ;
#14407 = EDGE_LOOP ( 'NONE', ( #42689, #55624, #25481, #67073 ) ) ;
#14408 = AXIS2_PLACEMENT_3D ( 'NONE', #51872, #13168, #34627 ) ;
#14409 = DIRECTION ( 'NONE',  ( 0.000000000000000000, 1.000000000000000000, -0.000000000000000000 ) ) ;
#14410 = CARTESIAN_POINT ( 'NONE',  ( 8.102448949553181734, 141.3949999999999818, 5.886773742842750679 ) ) ;
#14411 = CARTESIAN_POINT ( 'NONE',  ( -22.75000000000000711, 0.000000000000000000, 4.000000000000000000 ) ) ;
#14412 = ORIENTED_EDGE ( 'NONE', *, *, #42787, .F. ) ;
#14413 = FILL_AREA_STYLE_COLOUR ( '', #30767 ) ;
#14414 = CARTESIAN_POINT ( 'NONE',  ( 5.598654528085805993, 145.3549999999999898, 7.705886871421374629 ) ) ;
#14415 = LINE ( 'NONE', #46126, #56366 ) ;
#14416 = CARTESIAN_POINT ( 'NONE',  ( -22.25000000000000711, 34.24999999999999289, -3.750000000000000000 ) ) ;
#14417 = VERTEX_POINT ( 'NONE', #41335 ) ;
#14418 = CARTESIAN_POINT ( 'NONE',  ( -6.826472737025120807, 120.9929263765338021, 4.959722759717906548 ) ) ;
#14419 =( LENGTH_UNIT ( ) NAMED_UNIT ( * ) SI_UNIT ( .MILLI., .METRE. ) );
#14420 = UNCERTAINTY_MEASURE_WITH_UNIT (LENGTH_MEASURE( 1.000000000000000082E-05 ), #12066, 'distance_accuracy_value', 'NONE');
#14421 = CYLINDRICAL_SURFACE ( 'NONE', #12105, 30.00000000000000000 ) ;
#14422 = VECTOR ( 'NONE', #48593, 1000.000000000000000 ) ;
#14423 = CARTESIAN_POINT ( 'NONE',  ( -15.48999599679679662, 146.4999999999999716, -7.500000000000000000 ) ) ;
#14424 = DIRECTION ( 'NONE',  ( -0.7833176619561891263, -0.6216216216216174928, -0.000000000000000000 ) ) ;
#14425 = ORIENTED_EDGE ( 'NONE', *, *, #42722, .T. ) ;
#14426 = CARTESIAN_POINT ( 'NONE',  ( -0.9113929259990886100, -9.000000000000001776, 0.04319542563019202613 ) ) ;
#14427 = EDGE_LOOP ( 'NONE', ( #19653, #25852 ) ) ;
#14428 = CARTESIAN_POINT ( 'NONE',  ( -54.89292637653381490, -8.102448949553172852, -5.886773742842741797 ) ) ;
#14429 = DIRECTION ( 'NONE',  ( 1.000000000000000000, -0.000000000000000000, 0.000000000000000000 ) ) ;
#14430 = CARTESIAN_POINT ( 'NONE',  ( -148.5550000000000068, 0.000000000000000000, 8.024999999999991473 ) ) ;
#14431 = VERTEX_POINT ( 'NONE', #15307 ) ;
#14432 = SURFACE_STYLE_USAGE ( .BOTH. , #31295 ) ;
#14433 = UNCERTAINTY_MEASURE_WITH_UNIT (LENGTH_MEASURE( 1.000000000000000082E-05 ), #48150, 'distance_accuracy_value', 'NONE');
#14434 = STYLED_ITEM ( 'NONE', ( #30623 ), #43263 ) ;
#14435 = SURFACE_SIDE_STYLE ('',( #57010 ) ) ;
#14436 = CARTESIAN_POINT ( 'NONE',  ( -2.607480562269032021, 151.2070736234661581, -8.025000000000032330 ) ) ;
#14437 = FACE_OUTER_BOUND ( 'NONE', #35391, .T. ) ;
#14438 = CARTESIAN_POINT ( 'NONE',  ( -9.827790563157511022E-16, 145.4429263765338192, 8.025000000000000355 ) ) ;
#14439 = ORIENTED_EDGE ( 'NONE', *, *, #21126, .F. ) ;
#14440 = CARTESIAN_POINT ( 'NONE',  ( 27.00000000000001776, 42.00000000000000000, -36.50000000000000000 ) ) ;
#14441 = ORIENTED_EDGE ( 'NONE', *, *, #22431, .T. ) ;
#14442 = DIRECTION ( 'NONE',  ( 0.000000000000000000, 0.000000000000000000, 1.000000000000000000 ) ) ;
#14443 = CIRCLE ( 'NONE', #42556, 0.2500000000000002220 ) ;
#14444 = DIRECTION ( 'NONE',  ( 1.000000000000000000, 0.000000000000000000, 0.000000000000000000 ) ) ;
#14445 = CARTESIAN_POINT ( 'NONE',  ( -62.60499999999998266, 6.826472737025113702, -4.959722759717902107 ) ) ;
#14446 = ORIENTED_EDGE ( 'NONE', *, *, #40871, .F. ) ;
#14447 = DIRECTION ( 'NONE',  ( 0.000000000000000000, 0.000000000000000000, 1.000000000000000000 ) ) ;
#14448 = ADVANCED_BREP_SHAPE_REPRESENTATION ( '', ( #3964, #42840 ), #2244 ) ;
#14449 = EDGE_CURVE ( 'NONE', #45721, #57515, #15990, .T. ) ;
#14450 = VECTOR ( 'NONE', #26082, 1000.000000000000000 ) ;
#14451 = SURFACE_STYLE_FILL_AREA ( #42298 ) ;
#14452 = CARTESIAN_POINT ( 'NONE',  ( -74.75000000000000000, -0.9999999999999995559, 7.000000000000001776 ) ) ;
#14453 = VECTOR ( 'NONE', #21017, 1000.000000000000000 ) ;
#14455 = EDGE_CURVE ( 'NONE', #59005, #22530, #27888, .T. ) ;
#14454 = ORIENTED_EDGE ( 'NONE', *, *, #48019, .F. ) ;
#14456 = CARTESIAN_POINT ( 'NONE',  ( -75.00000000000000000, 9.609776836748626039, -6.329322064279367943 ) ) ;
#14457 = DIRECTION ( 'NONE',  ( 8.391040747885011388E-17, 0.7641995406119433953, 0.6449798928094538919 ) ) ;
#14458 = SURFACE_STYLE_FILL_AREA ( #53156 ) ;
#14459 = COLOUR_RGB ( '', 0.40784314, 0.44705882, 0.49803922) ;
#14460 = CARTESIAN_POINT ( 'NONE',  ( 0.000000000000000000, 8.270287287112621792E-15, 12.50000000000000000 ) ) ;
#14461 = CARTESIAN_POINT ( 'NONE',  ( 9.058813317711338797, 144.8449999999999989, -2.943386871421372675 ) ) ;
#14462 = CARTESIAN_POINT ( 'NONE',  ( -99.29499999999997328, -2.607480562269069768, 8.024999999999991473 ) ) ;
#14463 = EDGE_CURVE ( 'NONE', #22460, #54909, #3992, .T. ) ;
#14464 = DIRECTION ( 'NONE',  ( 0.000000000000000000, 0.000000000000000000, 1.000000000000000000 ) ) ;
#14465 = VECTOR ( 'NONE', #25865, 1000.000000000000000 ) ;
#14466 = DIRECTION ( 'NONE',  ( 0.000000000000000000, -1.000000000000000000, -0.000000000000000000 ) ) ;
#14467 = UNCERTAINTY_MEASURE_WITH_UNIT (LENGTH_MEASURE( 1.000000000000000082E-05 ), #11371, 'distance_accuracy_value', 'NONE');
#14468 = ORIENTED_EDGE ( 'NONE', *, *, #52842, .T. ) ;
#14469 = EDGE_CURVE ( 'NONE', #36379, #65996, #36767, .T. ) ;
#14470 = CARTESIAN_POINT ( 'NONE',  ( -143.0929263765338249, 3.094860106618433360, 9.524999999999991473 ) ) ;
#14471 = SURFACE_STYLE_USAGE ( .BOTH. , #51780 ) ;
#14472 =( NAMED_UNIT ( * ) PLANE_ANGLE_UNIT ( ) SI_UNIT ( $, .RADIAN. ) );
#14473 = CARTESIAN_POINT ( 'NONE',  ( -159.4449999999999932, 0.000000000000000000, 8.024999999999991473 ) ) ;
#14474 = AXIS2_PLACEMENT_3D ( 'NONE', #69237, #32604, #5188 ) ;
#14475 = FACE_OUTER_BOUND ( 'NONE', #37484, .T. ) ;
#14476 = DIRECTION ( 'NONE',  ( 0.000000000000000000, 1.000000000000000000, 0.000000000000000000 ) ) ;
#14477 = DIRECTION ( 'NONE',  ( 0.000000000000000000, 0.000000000000000000, 1.000000000000000000 ) ) ;
#14478 = EDGE_LOOP ( 'NONE', ( #40305, #10120, #43944 ) ) ;
#14479 = DIRECTION ( 'NONE',  ( -9.376883653928687363E-17, -1.000000000000000000, -0.000000000000000000 ) ) ;
#14480 = ORIENTED_EDGE ( 'NONE', *, *, #45154, .F. ) ;
#14481 = DIRECTION ( 'NONE',  ( 0.000000000000000000, 0.000000000000000000, -1.000000000000000000 ) ) ;
#14482 = CIRCLE ( 'NONE', #53796, 0.2500000000000002220 ) ;
#14483 = SURFACE_SIDE_STYLE ('',( #51794 ) ) ;
#14484 = FACE_OUTER_BOUND ( 'NONE', #49891, .T. ) ;
#14485 = CARTESIAN_POINT ( 'NONE',  ( -109.5570736234661666, -1.166476076187852838E-15, -9.524999999999991473 ) ) ;
#14486 = PRESENTATION_STYLE_ASSIGNMENT (( #19769 ) ) ;
#14487 = VECTOR ( 'NONE', #58932, 1000.000000000000000 ) ;
#14488 = ORIENTED_EDGE ( 'NONE', *, *, #64613, .F. ) ;
#14489 = CARTESIAN_POINT ( 'NONE',  ( -156.0550000000000068, -9.827790563157499189E-16, -8.024999999999991473 ) ) ;
#14490 = ORIENTED_EDGE ( 'NONE', *, *, #44972, .T. ) ;
#14491 = DIRECTION ( 'NONE',  ( 0.000000000000000000, 0.000000000000000000, 1.000000000000000000 ) ) ;
#14492 = CARTESIAN_POINT ( 'NONE',  ( -22.25000000000000711, 33.99999999999999289, -3.750000000000000000 ) ) ;
#14493 = ORIENTED_EDGE ( 'NONE', *, *, #48720, .T. ) ;
#14494 = STYLED_ITEM ( 'NONE', ( #10498 ), #19930 ) ;
#14495 = MECHANICAL_DESIGN_GEOMETRIC_PRESENTATION_REPRESENTATION (  '', ( #15630 ), #30193 ) ;
#14496 = SURFACE_STYLE_FILL_AREA ( #4630 ) ;
#14497 = CARTESIAN_POINT ( 'NONE',  ( -23.21231517720797655, 113.4999999999999858, 9.500000000000000000 ) ) ;
#14498 = CARTESIAN_POINT ( 'NONE',  ( -1.166476076187854022E-15, 113.9449999999999932, 9.525000000000000355 ) ) ;
#14499 = VECTOR ( 'NONE', #59593, 1000.000000000000000 ) ;
#14500 = ADVANCED_FACE ( 'NONE', ( #57480 ), #68360, .T. ) ;
#14501 = EDGE_LOOP ( 'NONE', ( #45522, #40831, #23448, #64003 ) ) ;
#14502 = DIRECTION ( 'NONE',  ( 0.000000000000000000, -1.000000000000000000, 0.000000000000000000 ) ) ;
#14503 = CARTESIAN_POINT ( 'NONE',  ( -5.598654528085806881, 122.8549999999999898, -7.705886871421374629 ) ) ;
#14504 = CARTESIAN_POINT ( 'NONE',  ( -72.80499999999997840, -8.437984349512086979, 5.166775262442717831E-16 ) ) ;
#14505 = CYLINDRICAL_SURFACE ( 'NONE', #2555, 0.2500000000000002220 ) ;
#14506 = EDGE_LOOP ( 'NONE', ( #7431, #49272, #55222, #18216 ) ) ;
#14507 = CARTESIAN_POINT ( 'NONE',  ( 8.102448949553183510, 137.1049999999999898, -5.886773742842746238 ) ) ;
#14508 = UNCERTAINTY_MEASURE_WITH_UNIT (LENGTH_MEASURE( 1.000000000000000082E-05 ), #22104, 'distance_accuracy_value', 'NONE');
#14509 = PRESENTATION_LAYER_ASSIGNMENT (  '', '', ( #4387 ) ) ;
#14510 = CYLINDRICAL_SURFACE ( 'NONE', #23222, 0.2500000000000002220 ) ;
#14511 = LINE ( 'NONE', #63407, #41039 ) ;
#14512 = ORIENTED_EDGE ( 'NONE', *, *, #15800, .T. ) ;
#14513 = CARTESIAN_POINT ( 'NONE',  ( 51.49999999999998579, 2.837994680254535968E-15, 10.00000000000000000 ) ) ;
#14514 = CARTESIAN_POINT ( 'NONE',  ( 60.00000000000000000, 1.797044900979284448E-15, -12.00000000000000000 ) ) ;
#14515 = CARTESIAN_POINT ( 'NONE',  ( -182.9050000000000011, 2.607480562269068880, -8.024999999999993250 ) ) ;
#14516 = ORIENTED_EDGE ( 'NONE', *, *, #9176, .T. ) ;
#14517 = CARTESIAN_POINT ( 'NONE',  ( 8.325601791849228661, 111.5275746901607619, -1.721597945495230819 ) ) ;
#14518 = SURFACE_STYLE_USAGE ( .BOTH. , #4283 ) ;
#14519 = CARTESIAN_POINT ( 'NONE',  ( -86.24292637653380211, 5.598654528085804216, 7.705886871421366635 ) ) ;
#14520 = ORIENTED_EDGE ( 'NONE', *, *, #49330, .T. ) ;
#14521 = CARTESIAN_POINT ( 'NONE',  ( -69.49999999999997158, 50.00000000000000000, -6.500000000000000000 ) ) ;
#14522 = DIRECTION ( 'NONE',  ( 0.000000000000000000, 0.000000000000000000, -1.000000000000000000 ) ) ;
#14523 = VERTEX_POINT ( 'NONE', #14943 ) ;
#14524 = AXIS2_PLACEMENT_3D ( 'NONE', #51490, #46623, #2559 ) ;
#14525 = DIRECTION ( 'NONE',  ( -1.000000000000000000, -0.000000000000000000, -0.000000000000000000 ) ) ;
#14526 = ADVANCED_FACE ( 'NONE', ( #52235 ), #43689, .T. ) ;
#14527 =( LENGTH_UNIT ( ) NAMED_UNIT ( * ) SI_UNIT ( .MILLI., .METRE. ) );
#14528 = CARTESIAN_POINT ( 'NONE',  ( -93.65499999999998693, -7.632228543268600340, -2.479861379858950166 ) ) ;
#14529 = ORIENTED_EDGE ( 'NONE', *, *, #27893, .F. ) ;
#14530 = EDGE_CURVE ( 'NONE', #20740, #57439, #10683, .T. ) ;
#14531 = DIRECTION ( 'NONE',  ( 1.000000000000000000, 0.000000000000000000, 0.000000000000000000 ) ) ;
#14532 = CARTESIAN_POINT ( 'NONE',  ( -137.0070736234661410, -8.102448949553172852, -5.886773742842741797 ) ) ;
#14533 = PRESENTATION_LAYER_ASSIGNMENT (  '', '', ( #31391 ) ) ;
#14534 = CIRCLE ( 'NONE', #25778, 0.5000000000000004441 ) ;
#14535 =( NAMED_UNIT ( * ) SI_UNIT ( $, .STERADIAN. ) SOLID_ANGLE_UNIT ( ) );
#14536 = CARTESIAN_POINT ( 'NONE',  ( -1.166476076187854022E-15, 152.9449999999999932, 9.525000000000000355 ) ) ;
#14537 = CARTESIAN_POINT ( 'NONE',  ( -75.65707362346617515, 9.058813317711329915, 2.943386871421369566 ) ) ;
#14538 = EDGE_CURVE ( 'NONE', #26431, #57943, #27168, .T. ) ;
#14539 = VECTOR ( 'NONE', #54256, 1000.000000000000000 ) ;
#14540 = PRESENTATION_STYLE_ASSIGNMENT (( #24390 ) ) ;
#14541 = ORIENTED_EDGE ( 'NONE', *, *, #57522, .F. ) ;
#14542 = B_SPLINE_CURVE_WITH_KNOTS ( 'NONE', 3,
 ( #4940, #32021, #65420, #21117, #6315, #26717, #15871, #53147 ),
 .UNSPECIFIED., .F., .F.,
 ( 4, 2, 2, 4 ),
 ( 1.425583368063878336E-15, 0.0009391389479451172110, 0.001878277895888808696, 0.003756555791776202725 ),
 .UNSPECIFIED. ) ;
#14543 = DIRECTION ( 'NONE',  ( 0.000000000000000000, 1.000000000000000000, 0.000000000000000000 ) ) ;
#14544 = CARTESIAN_POINT ( 'NONE',  ( -20.00036572459219997, -12.00015238516981952, -0.3288021958098223396 ) ) ;
#14546 = FILL_AREA_STYLE ('',( #62716 ) ) ;
#14545 = DIRECTION ( 'NONE',  ( 0.000000000000000000, 0.000000000000000000, -1.000000000000000000 ) ) ;
#14547 = CIRCLE ( 'NONE', #23521, 0.2500000000000002220 ) ;
#14548 = CARTESIAN_POINT ( 'NONE',  ( -121.4049999999999869, -2.607480562269069768, 8.024999999999991473 ) ) ;
#14549 = CARTESIAN_POINT ( 'NONE',  ( 24.70577775730028236, 25.82240647180052662, -27.50000000000001421 ) ) ;
#14550 = CARTESIAN_POINT ( 'NONE',  ( 3.094860106618435136, 124.2949999999999733, -9.525000000000000355 ) ) ;
#14551 = CARTESIAN_POINT ( 'NONE',  ( -124.0449999999999875, 7.632228543268600340, 2.479861379858949277 ) ) ;
#14552 = AXIS2_PLACEMENT_3D ( 'NONE', #46711, #4063, #62809 ) ;
#14553 = EDGE_CURVE ( 'NONE', #29454, #10808, #34690, .T. ) ;
#14554 = DIRECTION ( 'NONE',  ( -1.000000000000000000, -0.000000000000000000, -0.000000000000000000 ) ) ;
#14555 = PRESENTATION_LAYER_ASSIGNMENT (  '', '', ( #25794 ) ) ;
#14556 = EDGE_LOOP ( 'NONE', ( #68097, #41648, #55175 ) ) ;
#14557 = VECTOR ( 'NONE', #59165, 1000.000000000000000 ) ;
#14558 = SHAPE_REPRESENTATION ( '5. Handle', ( #42840 ), #37272 ) ;
#14559 = PRESENTATION_LAYER_ASSIGNMENT (  '', '', ( #29142 ) ) ;
#14560 = SURFACE_STYLE_USAGE ( .BOTH. , #26489 ) ;
#14561 = ORIENTED_EDGE ( 'NONE', *, *, #3890, .F. ) ;
#14562 = CARTESIAN_POINT ( 'NONE',  ( 60.00000000000000000, 1.797044900979284448E-15, 12.00000000000000000 ) ) ;
#14563 = EDGE_CURVE ( 'NONE', #23940, #60504, #6559, .T. ) ;
#14564 = CARTESIAN_POINT ( 'NONE',  ( -167.8429263765337964, 9.058813317711329915, -2.943386871421373119 ) ) ;
#14565 = SURFACE_STYLE_USAGE ( .BOTH. , #14937 ) ;
#14566 = CARTESIAN_POINT ( 'NONE',  ( -181.7949999999999875, 2.607480562269068880, -8.024999999999993250 ) ) ;
#14567 = AXIS2_PLACEMENT_3D ( 'NONE', #58342, #48525, #42912 ) ;
#14568 = B_SPLINE_CURVE_WITH_KNOTS ( 'NONE', 3,
 ( #1678, #23872, #28076, #17259, #12969, #7364, #2351, #38721, #33395, #34429, #7008, #54824, #49590, #1321 ),
 .UNSPECIFIED., .F., .F.,
 ( 4, 2, 2, 2, 2, 2, 4 ),
 ( 0.000000000000000000, 0.0005917671672764528764, 0.001183534334552905753, 0.001479417918191132733, 0.001775301501829359713, 0.002071185085467586694, 0.002367068669105813674 ),
 .UNSPECIFIED. ) ;
#14569 = CARTESIAN_POINT ( 'NONE',  ( -6.826472737025120807, 125.1070736234661496, 4.959722759717906548 ) ) ;
#14570 = PRESENTATION_LAYER_ASSIGNMENT (  '', '', ( #33643 ) ) ;
#14571 = DIRECTION ( 'NONE',  ( 0.000000000000000000, 0.000000000000000000, 1.000000000000000000 ) ) ;
#14572 = DIRECTION ( 'NONE',  ( 7.709882115452468306E-16, -1.000000000000000000, 0.000000000000000000 ) ) ;
#14573 = EDGE_LOOP ( 'NONE', ( #3016, #1756, #34818, #3144 ) ) ;
#14574 = CARTESIAN_POINT ( 'NONE',  ( -85.49292637653380211, -8.102448949553172852, 5.886773742842742685 ) ) ;
#14575 = ITEM_DEFINED_TRANSFORMATION ( 'NONE', 'NONE', #47312,  #42840 ) ;
#14576 = AXIS2_PLACEMENT_3D ( 'NONE', #26490, #43755, #21568 ) ;
#14577 = CARTESIAN_POINT ( 'NONE',  ( 32.00000000000000000, 43.00000000000000000, -80.00402776293826435 ) ) ;
#14578 = SURFACE_STYLE_FILL_AREA ( #57128 ) ;
#14579 = FACE_OUTER_BOUND ( 'NONE', #22841, .T. ) ;
#14580 = CARTESIAN_POINT ( 'NONE',  ( 7.632228543268607446, 123.1570736234661609, 2.479861379858954606 ) ) ;
#14581 = CARTESIAN_POINT ( 'NONE',  ( 3.999798566743339556, 8.867945265733707672, 2.000000000000000000 ) ) ;
#14582 = TOROIDAL_SURFACE ( 'NONE', #19075, 111.0000000000000142, 1.000000000000000000 ) ;
#14583 = FACE_OUTER_BOUND ( 'NONE', #31004, .T. ) ;
#14584 = VERTEX_POINT ( 'NONE', #54614 ) ;
#14585 = CARTESIAN_POINT ( 'NONE',  ( 39.24999999999999289, 16.24999999999997513, -3.750000000000000000 ) ) ;
#14586 = PLANE ( 'NONE',  #43268 ) ;
#14587 = SURFACE_STYLE_USAGE ( .BOTH. , #67710 ) ;
#14588 = EDGE_LOOP ( 'NONE', ( #9900, #31925, #55629, #13319 ) ) ;
#14589 = DIRECTION ( 'NONE',  ( -1.000000000000000000, 0.000000000000000000, 0.000000000000000000 ) ) ;
#14590 = PRESENTATION_LAYER_ASSIGNMENT (  '', '', ( #22467 ) ) ;
#14591 = DIRECTION ( 'NONE',  ( -0.000000000000000000, -1.000000000000000000, -0.000000000000000000 ) ) ;
#14592 = CARTESIAN_POINT ( 'NONE',  ( -8.437984349512095861, 130.8070736234661524, -5.166775262442723748E-16 ) ) ;
#14593 = EDGE_CURVE ( 'NONE', #34471, #40156, #39205, .T. ) ;
#14594 = EDGE_LOOP ( 'NONE', ( #53526, #23578, #65693, #5011 ) ) ;
#14595 = PRESENTATION_LAYER_ASSIGNMENT (  '', '', ( #44957 ) ) ;
#14596 = FILL_AREA_STYLE_COLOUR ( '', #54056 ) ;
#14597 = CARTESIAN_POINT ( 'NONE',  ( -100.8549999999999898, 4.716976649647094177, 6.492361379858945902 ) ) ;
#14598 = LINE ( 'NONE', #4017, #45510 ) ;
#14599 = ORIENTED_EDGE ( 'NONE', *, *, #26752, .T. ) ;
#14600 = CARTESIAN_POINT ( 'NONE',  ( 4.383776131304275125, -1.496531397472843361, -9.000000000000007105 ) ) ;
#14601 = SPHERICAL_SURFACE ( 'NONE', #60812, 0.2500000000000000000 ) ;
#14602 = CARTESIAN_POINT ( 'NONE',  ( 4.750000000000002665, 24.74999999999998579, -3.750000000000000000 ) ) ;
#14603 = PRESENTATION_STYLE_ASSIGNMENT (( #25153 ) ) ;
#14604 = AXIS2_PLACEMENT_3D ( 'NONE', #46097, #18304, #61201 ) ;
#14605 = CIRCLE ( 'NONE', #19042, 0.2500000000000002220 ) ;
#14606 = ORIENTED_EDGE ( 'NONE', *, *, #61684, .T. ) ;
#14607 = SURFACE_STYLE_USAGE ( .BOTH. , #63139 ) ;
#14608 = CARTESIAN_POINT ( 'NONE',  ( -68.69500000000000739, -8.437984349512085203, 5.166775262442717831E-16 ) ) ;
#14610 = EDGE_LOOP ( 'NONE', ( #25393, #37395, #14866, #33039 ) ) ;
#14609 = CIRCLE ( 'NONE', #21313, 0.5000000000000004441 ) ;
#14611 = FACE_OUTER_BOUND ( 'NONE', #65876, .T. ) ;
#14612 = ADVANCED_FACE ( 'NONE', ( #49359 ), #33513, .T. ) ;
#14613 = FILL_AREA_STYLE_COLOUR ( '', #61529 ) ;
#14614 = FILL_AREA_STYLE ('',( #62447 ) ) ;
#14615 = AXIS2_PLACEMENT_3D ( 'NONE', #67973, #18720, #68307 ) ;
#14616 = ORIENTED_EDGE ( 'NONE', *, *, #485, .F. ) ;
#14617 = DIRECTION ( 'NONE',  ( 0.000000000000000000, -1.000000000000000000, 0.000000000000000000 ) ) ;
#14618 = LINE ( 'NONE', #64176, #42710 ) ;
#14619 = VECTOR ( 'NONE', #37562, 1000.000000000000000 ) ;
#14620 = ADVANCED_FACE ( 'NONE', ( #38838 ), #12047, .T. ) ;
#14621 =( NAMED_UNIT ( * ) PLANE_ANGLE_UNIT ( ) SI_UNIT ( $, .RADIAN. ) );
#14622 = EDGE_LOOP ( 'NONE', ( #31263, #17245, #59358, #23948 ) ) ;
#14623 = EDGE_CURVE ( 'NONE', #62586, #67110, #66124, .T. ) ;
#14624 = CYLINDRICAL_SURFACE ( 'NONE', #53278, 1.000000000000000888 ) ;
#14625 = COLOUR_RGB ( '', 0.66274510, 0.83137255, 0.94901961) ;
#14626 = ORIENTED_EDGE ( 'NONE', *, *, #61683, .T. ) ;
#14627 = CARTESIAN_POINT ( 'NONE',  ( 15.48999599679679662, 146.4999999999999716, -7.000000000000000000 ) ) ;
#14628 = CARTESIAN_POINT ( 'NONE',  ( -150.2929263765342114, 3.094860106611235562, -9.525000000005221068 ) ) ;
#14630 = AXIS2_PLACEMENT_3D ( 'NONE', #18281, #17276, #11611 ) ;
#14629 =( NAMED_UNIT ( * ) SI_UNIT ( $, .STERADIAN. ) SOLID_ANGLE_UNIT ( ) );
#14631 = CARTESIAN_POINT ( 'NONE',  ( -173.9070736234662036, -3.094860106618429807, 9.524999999999991473 ) ) ;
#14632 = MECHANICAL_DESIGN_GEOMETRIC_PRESENTATION_REPRESENTATION (  '', ( #12346 ), #32576 ) ;
#14633 = CARTESIAN_POINT ( 'NONE',  ( -3.094860106618434248, 125.7949999999999591, 9.525000000000000355 ) ) ;
#14634 = CARTESIAN_POINT ( 'NONE',  ( -108.6570736234661751, 9.058813317711329915, 2.943386871421369566 ) ) ;
#14635 = CYLINDRICAL_SURFACE ( 'NONE', #44830, 9.524999999999991473 ) ;
#14636 = EDGE_CURVE ( 'NONE', #36632, #67977, #25141, .T. ) ;
#14637 = CARTESIAN_POINT ( 'NONE',  ( -64.85707362346616378, -5.598654528085803328, -7.705886871421366635 ) ) ;
#14638 = VERTEX_POINT ( 'NONE', #68115 ) ;
#14639 = CIRCLE ( 'NONE', #25863, 13.49999999999999822 ) ;
#14640 = CARTESIAN_POINT ( 'NONE',  ( -107.8429263765338106, 9.058813317711329915, -2.943386871421373119 ) ) ;
#14641 = CARTESIAN_POINT ( 'NONE',  ( -81.74292637653380211, -5.598654528085803328, -7.705886871421366635 ) ) ;
#14642 = EDGE_CURVE ( 'NONE', #35085, #68501, #57186, .T. ) ;
#14644 = FACE_OUTER_BOUND ( 'NONE', #54566, .T. ) ;
#14643 = LINE ( 'NONE', #41392, #69498 ) ;
#14645 = CARTESIAN_POINT ( 'NONE',  ( -145.4050000000000296, -2.607480562269069768, 8.024999999999991473 ) ) ;
#14646 = DIRECTION ( 'NONE',  ( -1.000000000000000000, 0.000000000000000000, 0.000000000000000000 ) ) ;
#14647 = CARTESIAN_POINT ( 'NONE',  ( -148.3429263765338249, -9.058813317711329915, 2.943386871421371787 ) ) ;
#14648 = CARTESIAN_POINT ( 'NONE',  ( -158.3949999999999818, -6.826472737025115478, -4.959722759717899443 ) ) ;
#14649 = CARTESIAN_POINT ( 'NONE',  ( -147.7449999999999761, 4.716976649647094177, 6.492361379858945902 ) ) ;
#14650 = VERTEX_POINT ( 'NONE', #58237 ) ;
#14651 = CARTESIAN_POINT ( 'NONE',  ( -75.00000000000000000, 33.00000000000000000, 6.500000000000000000 ) ) ;
#14652 = SURFACE_SIDE_STYLE ('',( #68126 ) ) ;
#14653 = AXIS2_PLACEMENT_3D ( 'NONE', #19991, #67872, #30194 ) ;
#14654 = DIRECTION ( 'NONE',  ( 0.000000000000000000, 0.000000000000000000, 1.000000000000000000 ) ) ;
#14655 = CARTESIAN_POINT ( 'NONE',  ( -59.60499999999998977, 6.826472737025113702, -4.959722759717902107 ) ) ;
#14656 = FILL_AREA_STYLE ('',( #51947 ) ) ;
#14657 = CARTESIAN_POINT ( 'NONE',  ( -59.84499999999998465, -7.632228543268599452, 2.479861379858951054 ) ) ;
#14658 = CARTESIAN_POINT ( 'NONE',  ( -1.166476076187854022E-15, 160.0550000000000068, 9.525000000000000355 ) ) ;
#14659 = LINE ( 'NONE', #56876, #26397 ) ;
#14660 = STYLED_ITEM ( 'NONE', ( #30741 ), #21188 ) ;
#14661 = CIRCLE ( 'NONE', #22488, 0.9999999999999997780 ) ;
#14662 = CARTESIAN_POINT ( 'NONE',  ( -155.4570736234661581, -9.058813317711329915, 2.943386871421371787 ) ) ;
#14663 = EDGE_CURVE ( 'NONE', #39204, #43611, #41393, .T. ) ;
#14664 = SURFACE_STYLE_FILL_AREA ( #36133 ) ;
#14665 = CARTESIAN_POINT ( 'NONE',  ( 0.8561458320465512584, 43.00000000000000711, -45.61250543006185154 ) ) ;
#14666 = CIRCLE ( 'NONE', #60678, 1.000000000000000888 ) ;
#14667 = DIRECTION ( 'NONE',  ( 0.000000000000000000, 0.000000000000000000, -1.000000000000000000 ) ) ;
#14668 = FACE_OUTER_BOUND ( 'NONE', #23712, .T. ) ;
#14669 =( GEOMETRIC_REPRESENTATION_CONTEXT ( 3 ) GLOBAL_UNCERTAINTY_ASSIGNED_CONTEXT ( ( #21482 ) ) GLOBAL_UNIT_ASSIGNED_CONTEXT ( ( #26503, #64503, #26158 ) ) REPRESENTATION_CONTEXT ( 'NONE', 'WORKASPACE' ) );
#14670 = CARTESIAN_POINT ( 'NONE',  ( -43.99999999999998579, 0.000000000000000000, 0.000000000000000000 ) ) ;
#14671 = CIRCLE ( 'NONE', #11254, 0.5000000000000004441 ) ;
#14672 = DIRECTION ( 'NONE',  ( -0.000000000000000000, 1.000000000000000000, -0.000000000000000000 ) ) ;
#14673 = CARTESIAN_POINT ( 'NONE',  ( 26.00000000000001776, 42.00000000000000000, -29.68999999999999417 ) ) ;
#14674 = SURFACE_STYLE_USAGE ( .BOTH. , #15044 ) ;
#14675 = ORIENTED_EDGE ( 'NONE', *, *, #47560, .F. ) ;
#14676 = AXIS2_PLACEMENT_3D ( 'NONE', #33669, #6939, #64978 ) ;
#14677 = VERTEX_POINT ( 'NONE', #35749 ) ;
#14678 = COLOUR_RGB ( '', 0.40784314, 0.44705882, 0.49803922) ;
#14679 = FACE_OUTER_BOUND ( 'NONE', #37291, .T. ) ;
#14680 = PRODUCT_DEFINITION_FORMATION_WITH_SPECIFIED_SOURCE ( 'ANY', '', #54094, .NOT_KNOWN. ) ;
#14681 = CARTESIAN_POINT ( 'NONE',  ( -20.71462254620879762, 114.5909367637873402, 9.999999999998797406 ) ) ;
#14682 = DIRECTION ( 'NONE',  ( 0.000000000000000000, 1.000000000000000000, -0.000000000000000000 ) ) ;
#14683 = CARTESIAN_POINT ( 'NONE',  ( -77.90707362346617515, -3.094860106618429807, 9.524999999999991473 ) ) ;
#14684 = ORIENTED_EDGE ( 'NONE', *, *, #62802, .F. ) ;
#14685 = ORIENTED_EDGE ( 'NONE', *, *, #28671, .T. ) ;
#14686 = CARTESIAN_POINT ( 'NONE',  ( -108.6570736234661751, 9.058813317711329915, 2.943386871421369566 ) ) ;
#14687 = DIRECTION ( 'NONE',  ( 0.000000000000000000, 0.000000000000000000, 1.000000000000000000 ) ) ;
#14688 = FILL_AREA_STYLE ('',( #51026 ) ) ;
#14689 = ORIENTED_EDGE ( 'NONE', *, *, #38372, .F. ) ;
#14690 = CARTESIAN_POINT ( 'NONE',  ( -9.058813317711337021, 117.1549999999999869, -2.943386871421374895 ) ) ;
#14691 = ORIENTED_EDGE ( 'NONE', *, *, #17368, .T. ) ;
#14692 = EDGE_CURVE ( 'NONE', #49243, #41309, #13938, .T. ) ;
#14693 = VECTOR ( 'NONE', #69090, 1000.000000000000000 ) ;
#14694 = CARTESIAN_POINT ( 'NONE',  ( -13.50000000000000533, 30.99999999999999289, 3.750000000000000000 ) ) ;
#14695 = CARTESIAN_POINT ( 'NONE',  ( -107.3949999999999960, -6.826472737025115478, -4.959722759717899443 ) ) ;
#14696 = ORIENTED_EDGE ( 'NONE', *, *, #45785, .T. ) ;
#14697 =( LENGTH_UNIT ( ) NAMED_UNIT ( * ) SI_UNIT ( .MILLI., .METRE. ) );
#14698 = SURFACE_STYLE_FILL_AREA ( #4099 ) ;
#14699 = AXIS2_PLACEMENT_3D ( 'NONE', #15061, #7426, #23930 ) ;
#14700 = ADVANCED_FACE ( 'NONE', ( #14644 ), #19555, .F. ) ;
#14701 = STYLED_ITEM ( 'NONE', ( #28448 ), #12291 ) ;
#14702 = ORIENTED_EDGE ( 'NONE', *, *, #32467, .F. ) ;
#14703 = CARTESIAN_POINT ( 'NONE',  ( -6.826472737025120807, 153.3929263765338078, -4.959722759717907437 ) ) ;
#14704 = CARTESIAN_POINT ( 'NONE',  ( 54.99999999999999289, 2.409368300552961372E-15, 11.50000000000003730 ) ) ;
#14705 = DIRECTION ( 'NONE',  ( -1.274184670190250597E-16, 1.000000000000000000, 2.430666987507993885E-16 ) ) ;
#14706 = EDGE_CURVE ( 'NONE', #62143, #39909, #15608, .T. ) ;
#14707 = CARTESIAN_POINT ( 'NONE',  ( 60.00000000000000000, 1.797044900979284448E-15, 10.50000000000000000 ) ) ;
#14708 = VERTEX_POINT ( 'NONE', #4054 ) ;
#14709 = AXIS2_PLACEMENT_3D ( 'NONE', #1088, #38847, #65534 ) ;
#14710 =( NAMED_UNIT ( * ) SI_UNIT ( $, .STERADIAN. ) SOLID_ANGLE_UNIT ( ) );
#14711 = ORIENTED_EDGE ( 'NONE', *, *, #1698, .T. ) ;
#14712 = SURFACE_STYLE_FILL_AREA ( #41459 ) ;
#14713 = FILL_AREA_STYLE ('',( #42873 ) ) ;
#14714 = CARTESIAN_POINT ( 'NONE',  ( -122.1549999999999869, 7.632228543268600340, 2.479861379858949277 ) ) ;
#14715 = CARTESIAN_POINT ( 'NONE',  ( -183.9999999999999716, -5.054410645616873587, 6.281779722895938889 ) ) ;
#14716 = CARTESIAN_POINT ( 'NONE',  ( -9.827790563157511022E-16, 140.5570736234661524, 8.025000000000000355 ) ) ;
#14717 =( NAMED_UNIT ( * ) PLANE_ANGLE_UNIT ( ) SI_UNIT ( $, .RADIAN. ) );
#14718 = AXIS2_PLACEMENT_3D ( 'NONE', #54444, #32298, #64990 ) ;
#14719 = CARTESIAN_POINT ( 'NONE',  ( -74.35421852510367557, 8.378235220106981629, 6.482771786488847887 ) ) ;
#14720 = CARTESIAN_POINT ( 'NONE',  ( -75.50000000000000000, -8.499999999999991118, 21.00000000000000000 ) ) ;
#14721 = CARTESIAN_POINT ( 'NONE',  ( -6.898093598910799429, 6.052151411320864760, 0.1381979515792698954 ) ) ;
#14722 = CARTESIAN_POINT ( 'NONE',  ( -35.25000000000000000, 4.336808689942018722E-16, -5.099999999999999645 ) ) ;
#14723 = ORIENTED_EDGE ( 'NONE', *, *, #62566, .F. ) ;
#14724 = AXIS2_PLACEMENT_3D ( 'NONE', #9592, #52502, #4245 ) ;
#14725 = ORIENTED_EDGE ( 'NONE', *, *, #55183, .F. ) ;
#14726 = SURFACE_STYLE_FILL_AREA ( #36569 ) ;
#14727 = FACE_BOUND ( 'NONE', #67648, .T. ) ;
#14728 = EDGE_CURVE ( 'NONE', #23874, #47647, #10369, .T. ) ;
#14729 = DIRECTION ( 'NONE',  ( 1.000000000000000000, 0.000000000000000000, 0.000000000000000000 ) ) ;
#14730 = ORIENTED_EDGE ( 'NONE', *, *, #56521, .T. ) ;
#14731 = CARTESIAN_POINT ( 'NONE',  ( 15.48999599679679662, 117.9999999999999716, -7.000000000000000000 ) ) ;
#14732 = CARTESIAN_POINT ( 'NONE',  ( -174.6550000000000011, -7.632228543268600340, -2.479861379858950166 ) ) ;
#14733 = CARTESIAN_POINT ( 'NONE',  ( -8.701243704650556410, 2.329718218673040298, 2.929003814506404790 ) ) ;
#14734 = DIRECTION ( 'NONE',  ( 1.000000000000000000, 0.000000000000000000, 0.000000000000000000 ) ) ;
#14735 = CARTESIAN_POINT ( 'NONE',  ( -47.75707362346617657, -5.598654528085801552, 7.705886871421367523 ) ) ;
#14736 = CARTESIAN_POINT ( 'NONE',  ( -175.0450000000000159, 7.632228543268600340, 2.479861379858949277 ) ) ;
#14737 = FACE_OUTER_BOUND ( 'NONE', #18592, .T. ) ;
#14738 = AXIS2_PLACEMENT_3D ( 'NONE', #21304, #36843, #42825 ) ;
#14739 = ORIENTED_EDGE ( 'NONE', *, *, #18275, .F. ) ;
#14740 = CARTESIAN_POINT ( 'NONE',  ( 34.99999999999992895, 112.4999999999999858, 9.500000000000000000 ) ) ;
#14741 = LINE ( 'NONE', #46800, #50449 ) ;
#14742 = CYLINDRICAL_SURFACE ( 'NONE', #48524, 16.00000000000000000 ) ;
#14743 = CARTESIAN_POINT ( 'NONE',  ( -90.65499999999998693, -7.632228543268600340, -2.479861379858950166 ) ) ;
#14744 = CARTESIAN_POINT ( 'NONE',  ( 8.876997378076488587, 154.5000000000000284, -3.480709456473927599 ) ) ;
#14745 = SURFACE_STYLE_USAGE ( .BOTH. , #62900 ) ;
#14746 = FILL_AREA_STYLE_COLOUR ( '', #17988 ) ;
#14747 = CARTESIAN_POINT ( 'NONE',  ( -86.54499999999998749, -7.632228543268600340, -2.479861379858950166 ) ) ;
#14748 = CARTESIAN_POINT ( 'NONE',  ( 8.102448949553181734, 124.5049999999999812, 5.886773742842750679 ) ) ;
#14749 = CARTESIAN_POINT ( 'NONE',  ( -69.29499999999995907, -2.607480562269069768, 8.024999999999991473 ) ) ;
#14750 = CARTESIAN_POINT ( 'NONE',  ( -75.00000000000001421, 9.585601099689363025, -6.373959028214384759 ) ) ;
#14751 =( NAMED_UNIT ( * ) SI_UNIT ( $, .STERADIAN. ) SOLID_ANGLE_UNIT ( ) );
#14752 = ADVANCED_FACE ( 'NONE', ( #19190 ), #52634, .F. ) ;
#14753 = DIRECTION ( 'NONE',  ( 1.000000000000000000, 0.000000000000000000, 0.000000000000000000 ) ) ;
#14754 = DIRECTION ( 'NONE',  ( -1.000000000000000000, 0.000000000000000000, 0.000000000000000000 ) ) ;
#14756 = VERTEX_POINT ( 'NONE', #14283 ) ;
#14755 = PRESENTATION_LAYER_ASSIGNMENT (  '', '', ( #42859 ) ) ;
#14757 = CARTESIAN_POINT ( 'NONE',  ( -104.9929263765337879, 8.102448949553171076, -5.886773742842744461 ) ) ;
#14758 = AXIS2_PLACEMENT_3D ( 'NONE', #42129, #31149, #52644 ) ;
#14759 = PRODUCT_DEFINITION_SHAPE ( 'NONE', 'NONE',  #32611 ) ;
#14760 = CARTESIAN_POINT ( 'NONE',  ( -126.5949999999999847, 2.607480562269073321, 8.024999999999991473 ) ) ;
#14761 =( LENGTH_UNIT ( ) NAMED_UNIT ( * ) SI_UNIT ( .MILLI., .METRE. ) );
#14762 = AXIS2_PLACEMENT_3D ( 'NONE', #11979, #33438, #49631 ) ;
#14764 = DIRECTION ( 'NONE',  ( -1.000000000000000000, -0.000000000000000000, -0.000000000000000000 ) ) ;
#14763 = CARTESIAN_POINT ( 'NONE',  ( 6.826472737025121695, 135.6070736234661638, -4.959722759717905660 ) ) ;
#14765 = DIRECTION ( 'NONE',  ( 0.2413793103448194644, -0.9704308468600220117, 0.000000000000000000 ) ) ;
#14766 = EDGE_LOOP ( 'NONE', ( #12432, #41926, #7662, #55234, #54302 ) ) ;
#14767 = ORIENTED_EDGE ( 'NONE', *, *, #31288, .F. ) ;
#14768 = FACE_OUTER_BOUND ( 'NONE', #29749, .T. ) ;
#14769 = MECHANICAL_DESIGN_GEOMETRIC_PRESENTATION_REPRESENTATION (  '', ( #3452 ), #20370 ) ;
#14770 = DIRECTION ( 'NONE',  ( 6.938893903907233900E-15, -0.4705882352941119229, 0.8823529411764736707 ) ) ;
#14771 =( NAMED_UNIT ( * ) PLANE_ANGLE_UNIT ( ) SI_UNIT ( $, .RADIAN. ) );
#14772 = CARTESIAN_POINT ( 'NONE',  ( 3.999798566743339556, 49.09558629977726696, -2.000000000000000000 ) ) ;
#14773 = AXIS2_PLACEMENT_3D ( 'NONE', #50147, #66294, #17783 ) ;
#14774 = DIRECTION ( 'NONE',  ( -1.000000000000000000, 0.000000000000000000, 0.000000000000000000 ) ) ;
#14775 = ORIENTED_EDGE ( 'NONE', *, *, #15074, .F. ) ;
#14776 = CARTESIAN_POINT ( 'NONE',  ( -122.7549999999999955, 4.716976649647091513, -6.492361379858946790 ) ) ;
#14777 = ORIENTED_EDGE ( 'NONE', *, *, #69029, .T. ) ;
#14778 = CARTESIAN_POINT ( 'NONE',  ( 22.50000000000000711, 36.75000000000000000, 4.000000000000000000 ) ) ;
#14779 = CARTESIAN_POINT ( 'NONE',  ( -123.0570736234661808, 0.000000000000000000, 9.524999999999991473 ) ) ;
#14780 = EDGE_LOOP ( 'NONE', ( #5959, #50891, #429, #28490 ) ) ;
#14781 = PLANE ( 'NONE',  #27923 ) ;
#14782 = DIRECTION ( 'NONE',  ( -1.000000000000000000, 0.000000000000000000, 0.000000000000000000 ) ) ;
#14783 = EDGE_LOOP ( 'NONE', ( #18496, #33715, #53768, #19478 ) ) ;
#14784 = CIRCLE ( 'NONE', #25949, 1.000000000000000000 ) ;
#14785 = ADVANCED_FACE ( 'NONE', ( #27229 ), #47754, .F. ) ;
#14786 = CARTESIAN_POINT ( 'NONE',  ( -74.99999999999998579, 50.00000000000000000, -12.00000000000000000 ) ) ;
#14787 = CARTESIAN_POINT ( 'NONE',  ( -9.058813317711337021, 152.0449999999999875, -2.943386871421374895 ) ) ;
#14788 = STYLED_ITEM ( 'NONE', ( #8957 ), #17106 ) ;
#14789 = ORIENTED_EDGE ( 'NONE', *, *, #26039, .F. ) ;
#14790 = CIRCLE ( 'NONE', #47585, 0.5000000000000004441 ) ;
#14791 =( NAMED_UNIT ( * ) PLANE_ANGLE_UNIT ( ) SI_UNIT ( $, .RADIAN. ) );
#14792 = CARTESIAN_POINT ( 'NONE',  ( 5.598654528085805993, 154.3549999999999898, 7.705886871421374629 ) ) ;
#14793 = CARTESIAN_POINT ( 'NONE',  ( 2.000000000000022204, 50.00000000000000000, 55.00000000000000711 ) ) ;
#14794 =( LENGTH_UNIT ( ) NAMED_UNIT ( * ) SI_UNIT ( .MILLI., .METRE. ) );
#14795 = ORIENTED_EDGE ( 'NONE', *, *, #36154, .T. ) ;
#14796 = CARTESIAN_POINT ( 'NONE',  ( 6.826472737025119919, 112.8929263765338078, 4.959722759717908325 ) ) ;
#14797 = SURFACE_STYLE_USAGE ( .BOTH. , #30233 ) ;
#14798 = EDGE_CURVE ( 'NONE', #42205, #39971, #59961, .T. ) ;
#14799 = CARTESIAN_POINT ( 'NONE',  ( 45.65811388300840434, 10.21937129433612057, -6.292893218813452982 ) ) ;
#14800 = ORIENTED_EDGE ( 'NONE', *, *, #53837, .T. ) ;
#14801 = DIRECTION ( 'NONE',  ( -0.000000000000000000, -1.000000000000000000, -0.000000000000000000 ) ) ;
#14802 = ORIENTED_EDGE ( 'NONE', *, *, #30032, .F. ) ;
#14803 = CARTESIAN_POINT ( 'NONE',  ( -59.39292637653377938, 8.102448949553176405, 5.886773742842740909 ) ) ;
#14804 = CARTESIAN_POINT ( 'NONE',  ( 34.99999999999999289, 99.99999999999998579, -7.000000000000000000 ) ) ;
#14805 =( NAMED_UNIT ( * ) SI_UNIT ( $, .STERADIAN. ) SOLID_ANGLE_UNIT ( ) );
#14807 = CARTESIAN_POINT ( 'NONE',  ( -151.1049999999999613, -6.826472737025115478, 4.959722759717900331 ) ) ;
#14806 = COLOUR_RGB ( '', 0.31764706, 0.68627451, 0.89019608) ;
#14809 = ORIENTED_EDGE ( 'NONE', *, *, #55673, .F. ) ;
#14808 = ADVANCED_FACE ( 'NONE', ( #32898, #53325, #17087, #16404, #27585, #11777, #26555 ), #49102, .T. ) ;
#14810 =( NAMED_UNIT ( * ) SI_UNIT ( $, .STERADIAN. ) SOLID_ANGLE_UNIT ( ) );
#14811 =( GEOMETRIC_REPRESENTATION_CONTEXT ( 3 ) GLOBAL_UNCERTAINTY_ASSIGNED_CONTEXT ( ( #37548 ) ) GLOBAL_UNIT_ASSIGNED_CONTEXT ( ( #59572, #32857, #759 ) ) REPRESENTATION_CONTEXT ( 'NONE', 'WORKASPACE' ) );
#14812 = ADVANCED_FACE ( 'NONE', ( #26877 ), #28631, .F. ) ;
#14813 = AXIS2_PLACEMENT_3D ( 'NONE', #26891, #53998, #54346 ) ;
#14814 = DIRECTION ( 'NONE',  ( 0.000000000000000000, 0.000000000000000000, -1.000000000000000000 ) ) ;
#14815 = DIRECTION ( 'NONE',  ( -1.000000000000000000, 0.000000000000000000, -0.000000000000000000 ) ) ;
#14816 = CARTESIAN_POINT ( 'NONE',  ( -70.64292637653379359, -5.598654528085801552, 7.705886871421367523 ) ) ;
#14817 = DIRECTION ( 'NONE',  ( -0.000000000000000000, -0.000000000000000000, -1.000000000000000000 ) ) ;
#14818 = ORIENTED_EDGE ( 'NONE', *, *, #62637, .T. ) ;
#14819 = VERTEX_POINT ( 'NONE', #11069 ) ;
#14820 = CARTESIAN_POINT ( 'NONE',  ( 23.06857045728888522, 24.64236968870869404, 27.22624481166502264 ) ) ;
#14821 = AXIS2_PLACEMENT_3D ( 'NONE', #39934, #55728, #26961 ) ;
#14822 = ADVANCED_FACE ( 'NONE', ( #23715 ), #12111, .T. ) ;
#14823 = CARTESIAN_POINT ( 'NONE',  ( -65.45499999999998408, 7.632228543268599452, -2.479861379858951942 ) ) ;
#14824 = VERTEX_POINT ( 'NONE', #18452 ) ;
#14825 = DIRECTION ( 'NONE',  ( 0.000000000000000000, 0.000000000000000000, -1.000000000000000000 ) ) ;
#14826 = DIRECTION ( 'NONE',  ( 1.000000000000000000, 0.000000000000000000, 0.000000000000000000 ) ) ;
#14827 = CIRCLE ( 'NONE', #12561, 0.5000000000000004441 ) ;
#14828 = MECHANICAL_DESIGN_GEOMETRIC_PRESENTATION_REPRESENTATION (  '', ( #57483 ), #27130 ) ;
#14829 = CARTESIAN_POINT ( 'NONE',  ( -91.40707362346728360, 3.094860106599739868, -9.525000000013571722 ) ) ;
#14830 = DIRECTION ( 'NONE',  ( 0.000000000000000000, 0.000000000000000000, 1.000000000000000000 ) ) ;
#14831 = ORIENTED_EDGE ( 'NONE', *, *, #25060, .T. ) ;
#14832 = MECHANICAL_DESIGN_GEOMETRIC_PRESENTATION_REPRESENTATION (  '', ( #11435 ), #48536 ) ;
#14833 = LINE ( 'NONE', #35934, #60616 ) ;
#14834 =( LENGTH_UNIT ( ) NAMED_UNIT ( * ) SI_UNIT ( .MILLI., .METRE. ) );
#14835 = AXIS2_PLACEMENT_3D ( 'NONE', #33845, #65875, #27855 ) ;
#14836 = DIRECTION ( 'NONE',  ( 0.000000000000000000, -1.000000000000000000, 0.000000000000000000 ) ) ;
#14837 = CIRCLE ( 'NONE', #17105, 0.2500000000000002220 ) ;
#14838 = CARTESIAN_POINT ( 'NONE',  ( -9.058813317711337021, 152.0449999999999875, -2.943386871421374895 ) ) ;
#14839 = CARTESIAN_POINT ( 'NONE',  ( -93.14499999999999602, -4.716976649647092401, 6.492361379858946790 ) ) ;
#14840 = TOROIDAL_SURFACE ( 'NONE', #15961, 24.00000000000001421, 1.000000000000000000 ) ;
#14841 = CARTESIAN_POINT ( 'NONE',  ( 21.25000000000001066, 24.99999999999998579, -3.750000000000000000 ) ) ;
#14842 = DIRECTION ( 'NONE',  ( -1.000000000000000000, 1.156482317317870344E-15, 0.000000000000000000 ) ) ;
#14843 = VECTOR ( 'NONE', #48928, 1000.000000000000000 ) ;
#14844 = DIRECTION ( 'NONE',  ( 0.000000000000000000, 1.000000000000000000, -0.000000000000000000 ) ) ;
#14845 = ORIENTED_EDGE ( 'NONE', *, *, #22172, .T. ) ;
#14846 = CARTESIAN_POINT ( 'NONE',  ( -137.3929263765337510, 8.102448949553176405, 5.886773742842740909 ) ) ;
#14847 = CARTESIAN_POINT ( 'NONE',  ( 5.196152422706628471, 2.500000000000000000, -9.000000000000005329 ) ) ;
#14848 = CARTESIAN_POINT ( 'NONE',  ( -160.3449999999999989, 7.632228543268599452, -2.479861379858951942 ) ) ;
#14849 =( GEOMETRIC_REPRESENTATION_CONTEXT ( 3 ) GLOBAL_UNCERTAINTY_ASSIGNED_CONTEXT ( ( #26522 ) ) GLOBAL_UNIT_ASSIGNED_CONTEXT ( ( #42779, #22657, #33553 ) ) REPRESENTATION_CONTEXT ( 'NONE', 'WORKASPACE' ) );
#14850 = CARTESIAN_POINT ( 'NONE',  ( 71.99999999999998579, 119.9999999999997868, 9.500000000000000000 ) ) ;
#14851 =( LENGTH_UNIT ( ) NAMED_UNIT ( * ) SI_UNIT ( .MILLI., .METRE. ) );
#14852 = DIRECTION ( 'NONE',  ( 0.000000000000000000, -1.000000000000000000, 0.000000000000000000 ) ) ;
#14853 = EDGE_LOOP ( 'NONE', ( #65654, #19010, #50249, #20122 ) ) ;
#14854 = ORIENTED_EDGE ( 'NONE', *, *, #65403, .F. ) ;
#14855 = MECHANICAL_DESIGN_GEOMETRIC_PRESENTATION_REPRESENTATION (  '', ( #26019 ), #1258 ) ;
#14856 = CARTESIAN_POINT ( 'NONE',  ( 8.000000000000001776, 30.74999999999998579, -3.750000000000000000 ) ) ;
#14857 = AXIS2_PLACEMENT_3D ( 'NONE', #5332, #33805, #27122 ) ;
#14858 = CIRCLE ( 'NONE', #32820, 0.5000000000000004441 ) ;
#14859 = CARTESIAN_POINT ( 'NONE',  ( -24.21231517720798010, 113.4999999999999858, 7.500000000000000000 ) ) ;
#14860 = CARTESIAN_POINT ( 'NONE',  ( 0.000000000000000000, 119.9429263765338050, -8.025000000000000355 ) ) ;
#14861 = DIRECTION ( 'NONE',  ( 0.000000000000000000, 0.000000000000000000, 1.000000000000000000 ) ) ;
#14862 = VECTOR ( 'NONE', #5478, 1000.000000000000000 ) ;
#14863 =( NAMED_UNIT ( * ) SI_UNIT ( $, .STERADIAN. ) SOLID_ANGLE_UNIT ( ) );
#14864 = ORIENTED_EDGE ( 'NONE', *, *, #29228, .F. ) ;
#14865 = CARTESIAN_POINT ( 'NONE',  ( -153.3549999999999898, -4.716976649647093289, -6.492361379858945902 ) ) ;
#14866 = ORIENTED_EDGE ( 'NONE', *, *, #13559, .F. ) ;
#14867 = DIRECTION ( 'NONE',  ( 0.000000000000000000, 1.000000000000000000, -0.000000000000000000 ) ) ;
#14868 = DIRECTION ( 'NONE',  ( 0.000000000000000000, 1.224646799147353207E-16, -1.000000000000000000 ) ) ;
#14869 = ORIENTED_EDGE ( 'NONE', *, *, #15850, .T. ) ;
#14870 = EDGE_CURVE ( 'NONE', #46789, #55490, #51523, .T. ) ;
#14871 = LINE ( 'NONE', #25738, #49543 ) ;
#14872 = PRESENTATION_LAYER_ASSIGNMENT (  '', '', ( #5840 ) ) ;
#14873 = CARTESIAN_POINT ( 'NONE',  ( -57.50707362346616236, 8.102448949553176405, 5.886773742842740909 ) ) ;
#14874 = CARTESIAN_POINT ( 'NONE',  ( -9.058813317711338797, 125.3449999999999847, 2.943386871421373563 ) ) ;
#14875 = ADVANCED_FACE ( 'NONE', ( #29326 ), #33596, .T. ) ;
#14876 = AXIS2_PLACEMENT_3D ( 'NONE', #9428, #69455, #58905 ) ;
#14877 = EDGE_LOOP ( 'NONE', ( #60090, #28299 ) ) ;
#14878 = ADVANCED_FACE ( 'NONE', ( #34275 ), #56777, .T. ) ;
#14879 = CARTESIAN_POINT ( 'NONE',  ( -57.44292637653381206, -1.166476076187852838E-15, -9.524999999999991473 ) ) ;
#14880 = CARTESIAN_POINT ( 'NONE',  ( -3.094860106618434248, 120.9049999999999869, 9.525000000000000355 ) ) ;
#14881 = CARTESIAN_POINT ( 'NONE',  ( -71.15499999999998693, 7.632228543268600340, 2.479861379858949277 ) ) ;
#14882 = CARTESIAN_POINT ( 'NONE',  ( 3.249999999999998668, 36.99999999999999289, 3.750000000000000000 ) ) ;
#14883 = ORIENTED_EDGE ( 'NONE', *, *, #6342, .F. ) ;
#14884 = CARTESIAN_POINT ( 'NONE',  ( 9.058813317711337021, 142.6549999999999727, 2.943386871421375783 ) ) ;
#14885 = EDGE_CURVE ( 'NONE', #6197, #41879, #33240, .T. ) ;
#14886 = DIRECTION ( 'NONE',  ( -0.000000000000000000, -1.000000000000000000, -0.000000000000000000 ) ) ;
#14887 = LINE ( 'NONE', #36370, #30531 ) ;
#14888 = EDGE_CURVE ( 'NONE', #51313, #67895, #61052, .T. ) ;
#14889 = CARTESIAN_POINT ( 'NONE',  ( -41.16151714082912605, 107.5071857241661348, 3.372843186988513597 ) ) ;
#14890 = AXIS2_PLACEMENT_3D ( 'NONE', #35921, #48231, #30613 ) ;
#14891 = EDGE_CURVE ( 'NONE', #60007, #3926, #10066, .T. ) ;
#14892 = FACE_OUTER_BOUND ( 'NONE', #66873, .T. ) ;
#14893 = ORIENTED_EDGE ( 'NONE', *, *, #40760, .T. ) ;
#14894 = DIRECTION ( 'NONE',  ( -0.000000000000000000, -0.000000000000000000, 1.000000000000000000 ) ) ;
#14895 = FILL_AREA_STYLE_COLOUR ( '', #19414 ) ;
#14896 = CARTESIAN_POINT ( 'NONE',  ( 2.999999999999990230, 0.000000000000000000, 37.00402776293829277 ) ) ;
#14897 = CARTESIAN_POINT ( 'NONE',  ( -182.3049999999999500, 8.437984349512085203, -1.550032578732815448E-15 ) ) ;
#14898 = ORIENTED_EDGE ( 'NONE', *, *, #43266, .T. ) ;
#14899 =( BOUNDED_CURVE ( )  B_SPLINE_CURVE ( 2, ( #31135, #62464, #14280, #8667, #14640, #36817, #30095, #4052, #35746, #4388, #58235 ),
 .UNSPECIFIED., .F., .F. ) 
 B_SPLINE_CURVE_WITH_KNOTS ( ( 3, 2, 2, 2, 2, 3 ),
 ( 0.5543478260869434404, 0.5565217391304216887, 0.5586956521738998260, 0.5608695652173780744, 0.5630434782608562116, 0.5652173913043344600 ),
 .UNSPECIFIED. ) 
 CURVE ( )  GEOMETRIC_REPRESENTATION_ITEM ( )  RATIONAL_B_SPLINE_CURVE ( ( 1.000000000000294875, 0.9510565162948585449, 1.000000000000000000, 0.9510565162951535312, 1.000000000000000000, 0.9510565162951535312, 1.000000000000000000, 0.9510565162951535312, 1.000000000000000000, 0.9510565162954535134, 0.9999999999997000177 ) ) 
 REPRESENTATION_ITEM ( '' )  );
#14900 = CARTESIAN_POINT ( 'NONE',  ( 32.00000000000001421, 42.00000000000000711, 44.99999999999998579 ) ) ;
#14901 = PRESENTATION_STYLE_ASSIGNMENT (( #14518 ) ) ;
#14902 = EDGE_CURVE ( 'NONE', #57697, #54371, #17564, .T. ) ;
#14903 = DIRECTION ( 'NONE',  ( 1.000000000000000000, 0.000000000000000000, 0.000000000000000000 ) ) ;
#14904 = ORIENTED_EDGE ( 'NONE', *, *, #43370, .F. ) ;
#14905 = DIRECTION ( 'NONE',  ( 0.8660254037844385966, -0.5000000000000002220, 0.000000000000000000 ) ) ;
#14906 = ORIENTED_EDGE ( 'NONE', *, *, #63838, .T. ) ;
#14907 = CARTESIAN_POINT ( 'NONE',  ( -128.1570736234661751, -9.058813317711329915, -2.943386871421370898 ) ) ;
#14908 = SPHERICAL_SURFACE ( 'NONE', #48293, 0.2500000000000000000 ) ;
#14909 = CARTESIAN_POINT ( 'NONE',  ( -98.75499999999999545, 4.716976649647091513, -6.492361379858946790 ) ) ;
#14910 = ORIENTED_EDGE ( 'NONE', *, *, #12624, .F. ) ;
#14911 = DIRECTION ( 'NONE',  ( 0.000000000000000000, 0.000000000000000000, 1.000000000000000000 ) ) ;
#14912 = CARTESIAN_POINT ( 'NONE',  ( -130.4070736234661751, 3.094860106618428031, -9.524999999999993250 ) ) ;
#14913 = AXIS2_PLACEMENT_3D ( 'NONE', #7641, #2295, #29442 ) ;
#14914 = CARTESIAN_POINT ( 'NONE',  ( 10.01517768586949408, 153.6949999999999932, 1.839758294383810543E-15 ) ) ;
#14915 = CARTESIAN_POINT ( 'NONE',  ( -74.60707362346617799, -8.102448949553172852, 5.886773742842742685 ) ) ;
#14916 = DIRECTION ( 'NONE',  ( 0.000000000000000000, 0.000000000000000000, 1.000000000000000000 ) ) ;
#14917 = ORIENTED_EDGE ( 'NONE', *, *, #61758, .F. ) ;
#14918 = SURFACE_STYLE_USAGE ( .BOTH. , #24731 ) ;
#14920 = CARTESIAN_POINT ( 'NONE',  ( -19.48783162866786611, -11.79520720594569738, -2.229038028308376607 ) ) ;
#14919 = AXIS2_PLACEMENT_3D ( 'NONE', #6523, #16787, #22380 ) ;
#14921 = SURFACE_STYLE_USAGE ( .BOTH. , #42033 ) ;
#14922 = CARTESIAN_POINT ( 'NONE',  ( -116.0049999999999955, 6.826472737025116366, 4.959722759717898555 ) ) ;
#14923 = CLOSED_SHELL ( 'NONE', ( #28952, #60140, #58083, #64777, #41995, #50849, #5939, #39263, #42582, #27762, #31837, #55988, #62658, #6790, #5072, #59971, #45411, #17725, #6746, #56080, #15442, #62192, #11681, #61443, #51663 ) ) ;
#14924 = FILL_AREA_STYLE_COLOUR ( '', #65135 ) ;
#14925 = CARTESIAN_POINT ( 'NONE',  ( -5.598654528085806881, 121.7449999999999903, -7.705886871421374629 ) ) ;
#14926 = MECHANICAL_DESIGN_GEOMETRIC_PRESENTATION_REPRESENTATION (  '', ( #38551 ), #22735 ) ;
#14927 = CARTESIAN_POINT ( 'NONE',  ( -123.4449999999999932, 0.000000000000000000, 8.024999999999991473 ) ) ;
#14928 = PRESENTATION_LAYER_ASSIGNMENT (  '', '', ( #25045 ) ) ;
#14929 = CARTESIAN_POINT ( 'NONE',  ( -112.2570736234661837, 5.598654528085800663, -7.705886871421367523 ) ) ;
#14930 = EDGE_CURVE ( 'NONE', #3143, #41012, #2906, .T. ) ;
#14931 = AXIS2_PLACEMENT_3D ( 'NONE', #8214, #68340, #3214 ) ;
#14932 = FILL_AREA_STYLE_COLOUR ( '', #59469 ) ;
#14933 = CARTESIAN_POINT ( 'NONE',  ( 28.58578643762690419, 42.99999999999999289, -79.58981420056515788 ) ) ;
#14934 = ORIENTED_EDGE ( 'NONE', *, *, #27307, .F. ) ;
#14935 = DIRECTION ( 'NONE',  ( -0.000000000000000000, -0.000000000000000000, -1.000000000000000000 ) ) ;
#14936 = CARTESIAN_POINT ( 'NONE',  ( -175.3429263765338249, -9.058813317711329915, 2.943386871421371787 ) ) ;
#14937 = SURFACE_SIDE_STYLE ('',( #68380 ) ) ;
#14938 = LINE ( 'NONE', #48016, #18543 ) ;
#14939 = AXIS2_PLACEMENT_3D ( 'NONE', #40673, #52273, #3666 ) ;
#14940 = AXIS2_PLACEMENT_3D ( 'NONE', #13770, #44447, #12360 ) ;
#14941 = DIRECTION ( 'NONE',  ( 0.000000000000000000, 0.000000000000000000, -1.000000000000000000 ) ) ;
#14942 = CARTESIAN_POINT ( 'NONE',  ( 6.020204320972965206, 7.572700244129134894, 0.6386920474458019914 ) ) ;
#14943 = CARTESIAN_POINT ( 'NONE',  ( -1.011095968855053334E-15, -8.500000000000000000, 3.000000000000000000 ) ) ;
#14944 = LINE ( 'NONE', #68749, #20375 ) ;
#14945 = VERTEX_POINT ( 'NONE', #4305 ) ;
#14946 = CARTESIAN_POINT ( 'NONE',  ( -83.39292637653379359, 8.102448949553176405, 5.886773742842740909 ) ) ;
#14947 = APPLICATION_PROTOCOL_DEFINITION ( 'draft international standard', 'automotive_design', 1998, #5990 ) ;
#14948 = PRESENTATION_STYLE_ASSIGNMENT (( #63107 ) ) ;
#14949 = CONICAL_SURFACE ( 'NONE', #43049, 7.000000000000000888, 0.7853981633974500554 ) ;
#14950 = SURFACE_STYLE_USAGE ( .BOTH. , #31087 ) ;
#14951 = CARTESIAN_POINT ( 'NONE',  ( 0.000000000000000000, -2.500000000000000000, 0.000000000000000000 ) ) ;
#14952 = CARTESIAN_POINT ( 'NONE',  ( -162.4429263765338192, -1.166476076187852838E-15, -9.524999999999991473 ) ) ;
#14953 = EDGE_CURVE ( 'NONE', #37155, #19696, #66180, .T. ) ;
#14954 = ORIENTED_EDGE ( 'NONE', *, *, #42310, .F. ) ;
#14955 = CARTESIAN_POINT ( 'NONE',  ( -136.9429263765338192, 0.000000000000000000, 9.524999999999991473 ) ) ;
#14956 = SURFACE_STYLE_USAGE ( .BOTH. , #56447 ) ;
#14957 = ORIENTED_EDGE ( 'NONE', *, *, #51549, .F. ) ;
#14958 = CARTESIAN_POINT ( 'NONE',  ( -103.3429263765338106, -9.058813317711329915, 2.943386871421371787 ) ) ;
#14959 = VECTOR ( 'NONE', #67838, 1000.000000000000000 ) ;
#14960 = VECTOR ( 'NONE', #46290, 1000.000000000000000 ) ;
#14961 = CARTESIAN_POINT ( 'NONE',  ( 22.99999999999995026, 5.000000000000000000, 77.00402776293825013 ) ) ;
#14962 = CARTESIAN_POINT ( 'NONE',  ( 7.632228543268608334, 135.4570736234661581, -2.479861379858951942 ) ) ;
#14963 = SURFACE_STYLE_FILL_AREA ( #27448 ) ;
#14964 = ADVANCED_FACE ( 'NONE', ( #51855 ), #57821, .F. ) ;
#14965 = PRESENTATION_LAYER_ASSIGNMENT (  '', '', ( #23919 ) ) ;
#14966 = ORIENTED_EDGE ( 'NONE', *, *, #69037, .T. ) ;
#14967 = LINE ( 'NONE', #64517, #15886 ) ;
#14968 = CARTESIAN_POINT ( 'NONE',  ( -99.35499999999998977, -4.716976649647093289, -6.492361379858945902 ) ) ;
#14969 = CARTESIAN_POINT ( 'NONE',  ( 27.00000000000001776, 15.00000000000000000, 34.49999999999999289 ) ) ;
#14970 = ORIENTED_EDGE ( 'NONE', *, *, #46279, .T. ) ;
#14971 = CARTESIAN_POINT ( 'NONE',  ( -34.28383209646202801, -10.32887243014199363, 2.406038820785245225 ) ) ;
#14972 = CARTESIAN_POINT ( 'NONE',  ( 7.632228543268607446, 143.0429263765338135, 2.479861379858954606 ) ) ;
#14973 = DIRECTION ( 'NONE',  ( 1.000000000000000000, 0.000000000000000000, 0.000000000000000000 ) ) ;
#14974 =( NAMED_UNIT ( * ) PLANE_ANGLE_UNIT ( ) SI_UNIT ( $, .RADIAN. ) );
#14975 = COLOUR_RGB ( '', 0.66274510, 0.83137255, 0.94901961) ;
#14976 = EDGE_CURVE ( 'NONE', #56887, #65467, #41313, .T. ) ;
#14977 = VERTEX_POINT ( 'NONE', #6069 ) ;
#14978 = AXIS2_PLACEMENT_3D ( 'NONE', #8493, #57006, #56668 ) ;
#14979 =( LENGTH_UNIT ( ) NAMED_UNIT ( * ) SI_UNIT ( .MILLI., .METRE. ) );
#14980 = CARTESIAN_POINT ( 'NONE',  ( -76.34499999999998465, 7.632228543268599452, -2.479861379858951942 ) ) ;
#14981 = EDGE_LOOP ( 'NONE', ( #13918, #17624, #24550, #43874 ) ) ;
#14982 = CIRCLE ( 'NONE', #56513, 6.999999999999997335 ) ;
#14983 = CARTESIAN_POINT ( 'NONE',  ( -121.4070736234669283, 3.094860106605790140, -9.525000000009175238 ) ) ;
#14984 = CARTESIAN_POINT ( 'NONE',  ( -124.8570736234661780, -5.598654528085803328, -7.705886871421366635 ) ) ;
#14985 = ADVANCED_FACE ( 'NONE', ( #26483 ), #719, .F. ) ;
#14986 = VECTOR ( 'NONE', #52069, 1000.000000000000000 ) ;
#14987 = UNCERTAINTY_MEASURE_WITH_UNIT (LENGTH_MEASURE( 1.000000000000000082E-05 ), #62540, 'distance_accuracy_value', 'NONE');
#14988 = ORIENTED_EDGE ( 'NONE', *, *, #30509, .F. ) ;
#14989 = FACE_OUTER_BOUND ( 'NONE', #47079, .T. ) ;
#14990 = CARTESIAN_POINT ( 'NONE',  ( 25.00000000000001421, 43.00000000000000000, 34.49999999999999289 ) ) ;
#14991 = FILL_AREA_STYLE ('',( #48395 ) ) ;
#14992 = CARTESIAN_POINT ( 'NONE',  ( 71.50000000000000000, 14.49137674618942562, 7.500000000000000000 ) ) ;
#14993 = ORIENTED_EDGE ( 'NONE', *, *, #13658, .T. ) ;
#14994 = PLANE ( 'NONE',  #21785 ) ;
#14995 = ORIENTED_EDGE ( 'NONE', *, *, #40551, .T. ) ;
#14996 =( NAMED_UNIT ( * ) PLANE_ANGLE_UNIT ( ) SI_UNIT ( $, .RADIAN. ) );
#14997 = FACE_OUTER_BOUND ( 'NONE', #28350, .T. ) ;
#14998 = CARTESIAN_POINT ( 'NONE',  ( -169.4070736234661751, 3.094860106618428031, -9.524999999999993250 ) ) ;
#14999 = B_SPLINE_CURVE_WITH_KNOTS ( 'NONE', 3,
 ( #9479, #53075, #63947, #57653, #8770, #30543, #47129, #26311 ),
 .UNSPECIFIED., .F., .F.,
 ( 4, 2, 2, 4 ),
 ( 0.000000000000000000, 0.0004792974172913012877, 0.0007189461259369623941, 0.0009585948345826236089 ),
 .UNSPECIFIED. ) ;
#15000 = CARTESIAN_POINT ( 'NONE',  ( -8.102448949553179958, 127.8949999999999534, -5.886773742842749790 ) ) ;
#15001 = SHAPE_REPRESENTATION ( '7. Upper Jaw', ( #42840 ), #18040 ) ;
#15002 = CARTESIAN_POINT ( 'NONE',  ( -101.7570736234661695, -5.598654528085801552, 7.705886871421367523 ) ) ;
#15003 = AXIS2_PLACEMENT_3D ( 'NONE', #69650, #38388, #21462 ) ;
#15004 = CARTESIAN_POINT ( 'NONE',  ( 12.25000000000000355, 30.74999999999998579, -3.750000000000000000 ) ) ;
#15005 = DIRECTION ( 'NONE',  ( 1.000000000000000000, 0.000000000000000000, 0.000000000000000000 ) ) ;
#15006 = ORIENTED_EDGE ( 'NONE', *, *, #49184, .F. ) ;
#15008 = CARTESIAN_POINT ( 'NONE',  ( -61.19292637653379074, -10.01517768586948698, 6.132527647946031529E-16 ) ) ;
#15007 = DIRECTION ( 'NONE',  ( -0.000000000000000000, -1.000000000000000000, -0.000000000000000000 ) ) ;
#15009 = CARTESIAN_POINT ( 'NONE',  ( 22.99999999999999645, 5.000000000000000000, -72.00402776293825013 ) ) ;
#15010 = CARTESIAN_POINT ( 'NONE',  ( -141.9549999999999841, -7.632228543268599452, 2.479861379858951054 ) ) ;
#15011 =( NAMED_UNIT ( * ) PLANE_ANGLE_UNIT ( ) SI_UNIT ( $, .RADIAN. ) );
#15012 = CARTESIAN_POINT ( 'NONE',  ( -152.5449999999999875, -7.632228543268600340, -2.479861379858950166 ) ) ;
#15013 = AXIS2_PLACEMENT_3D ( 'NONE', #5554, #36616, #48533 ) ;
#15015 = CIRCLE ( 'NONE', #2577, 1.000000000000000888 ) ;
#15014 =( GEOMETRIC_REPRESENTATION_CONTEXT ( 3 ) GLOBAL_UNCERTAINTY_ASSIGNED_CONTEXT ( ( #43259 ) ) GLOBAL_UNIT_ASSIGNED_CONTEXT ( ( #62247, #40139, #50325 ) ) REPRESENTATION_CONTEXT ( 'NONE', 'WORKASPACE' ) );
#15016 = CARTESIAN_POINT ( 'NONE',  ( -150.2949999999999875, -2.607480562269069768, 8.024999999999991473 ) ) ;
#15017 = ORIENTED_EDGE ( 'NONE', *, *, #1471, .F. ) ;
#15018 = EDGE_CURVE ( 'NONE', #10014, #9623, #9981, .T. ) ;
#15019 = CARTESIAN_POINT ( 'NONE',  ( -44.50000000000000000, 10.49999999999998224, -3.500000000000000000 ) ) ;
#15020 = CIRCLE ( 'NONE', #34058, 0.2500000000000002220 ) ;
#15021 =( NAMED_UNIT ( * ) PLANE_ANGLE_UNIT ( ) SI_UNIT ( $, .RADIAN. ) );
#15022 = CARTESIAN_POINT ( 'NONE',  ( -195.0000000000000000, 0.000000000000000000, 0.000000000000000000 ) ) ;
#15023 = UNCERTAINTY_MEASURE_WITH_UNIT (LENGTH_MEASURE( 1.000000000000000082E-05 ), #594, 'distance_accuracy_value', 'NONE');
#15024 = CARTESIAN_POINT ( 'NONE',  ( -65.15499999999998693, 7.632228543268600340, 2.479861379858949277 ) ) ;
#15025 = B_SPLINE_CURVE_WITH_KNOTS ( 'NONE', 1,
 ( #2962, #14267 ),
 .UNSPECIFIED., .F., .F.,
 ( 2, 2 ),
 ( 0.000000000000000000, 1.000000000000000000 ),
 .UNSPECIFIED. ) ;
#15026 = DIRECTION ( 'NONE',  ( 1.000000000000000000, 0.000000000000000000, 0.000000000000000000 ) ) ;
#15027 = CARTESIAN_POINT ( 'NONE',  ( -61.64499999999998892, 4.716976649647091513, -6.492361379858946790 ) ) ;
#15028 = STYLED_ITEM ( 'NONE', ( #14948 ), #37626 ) ;
#15029 = CARTESIAN_POINT ( 'NONE',  ( 8.102448949553181734, 157.5050000000000239, 5.886773742842750679 ) ) ;
#15030 = SURFACE_STYLE_FILL_AREA ( #48436 ) ;
#15031 = CARTESIAN_POINT ( 'NONE',  ( 3.499999999999998668, 36.74999999999999289, -3.750000000000000000 ) ) ;
#15032 = TOROIDAL_SURFACE ( 'NONE', #45373, 26.49999999999999645, 0.5000000000000000000 ) ;
#15033 = CARTESIAN_POINT ( 'NONE',  ( -69.49999999999997158, 50.00000000000000000, 6.500000000000000000 ) ) ;
#15034 = UNCERTAINTY_MEASURE_WITH_UNIT (LENGTH_MEASURE( 1.000000000000000082E-05 ), #28009, 'distance_accuracy_value', 'NONE');
#15035 = CARTESIAN_POINT ( 'NONE',  ( 16.00000000000007105, 50.00000000000002842, 1.214306433183764966E-14 ) ) ;
#15036 = PRESENTATION_LAYER_ASSIGNMENT (  '', '', ( #45376 ) ) ;
#15037 =( LENGTH_UNIT ( ) NAMED_UNIT ( * ) SI_UNIT ( .MILLI., .METRE. ) );
#15038 = ADVANCED_FACE ( 'NONE', ( #53900 ), #59174, .T. ) ;
#15039 = DIRECTION ( 'NONE',  ( -0.000000000000000000, -1.000000000000000000, -0.000000000000000000 ) ) ;
#15040 = LINE ( 'NONE', #9753, #26975 ) ;
#15041 = EDGE_CURVE ( 'NONE', #20378, #15573, #48251, .T. ) ;
#15042 = COLOUR_RGB ( '', 0.09019608, 0.27058824, 0.51372549) ;
#15043 = EDGE_CURVE ( 'NONE', #60504, #51066, #63912, .T. ) ;
#15044 = SURFACE_SIDE_STYLE ('',( #67789 ) ) ;
#15045 = EDGE_LOOP ( 'NONE', ( #19642, #5183, #55729, #18262 ) ) ;
#15046 = ORIENTED_EDGE ( 'NONE', *, *, #24077, .T. ) ;
#15047 = SURFACE_STYLE_USAGE ( .BOTH. , #52657 ) ;
#15048 = MECHANICAL_DESIGN_GEOMETRIC_PRESENTATION_REPRESENTATION (  '', ( #8301 ), #9460 ) ;
#15049 = DIRECTION ( 'NONE',  ( 0.000000000000000000, 1.000000000000000000, 0.000000000000000000 ) ) ;
#15050 = B_SPLINE_CURVE_WITH_KNOTS ( 'NONE', 3,
 ( #39632, #6527, #65295, #17811, #1568, #29017, #44240, #66329 ),
 .UNSPECIFIED., .F., .F.,
 ( 4, 2, 2, 4 ),
 ( 0.000000000000000000, 0.0004782788118992547534, 0.0007174182178488821031, 0.0009565576237985095069 ),
 .UNSPECIFIED. ) ;
#15051 = CIRCLE ( 'NONE', #38668, 4.999999999999997335 ) ;
#15052 = EDGE_CURVE ( 'NONE', #36322, #69269, #32810, .T. ) ;
#15053 = CARTESIAN_POINT ( 'NONE',  ( 0.000000000000000000, -7.000000000000000888, 0.000000000000000000 ) ) ;
#15054 = DIRECTION ( 'NONE',  ( 0.000000000000000000, 0.000000000000000000, 1.000000000000000000 ) ) ;
#15055 = DIRECTION ( 'NONE',  ( 1.000000000000000000, 1.156482317317866302E-16, 0.000000000000000000 ) ) ;
#15056 = ADVANCED_FACE ( 'NONE', ( #6752 ), #8899, .T. ) ;
#15057 = ORIENTED_EDGE ( 'NONE', *, *, #27021, .F. ) ;
#15058 = ORIENTED_EDGE ( 'NONE', *, *, #46532, .F. ) ;
#15059 = CARTESIAN_POINT ( 'NONE',  ( -109.4070736234670704, 3.094860106603370298, -9.525000000010933832 ) ) ;
#15060 = CARTESIAN_POINT ( 'NONE',  ( 68.99999999999998579, 37.00000000000000000, 3.000000000000000000 ) ) ;
#15061 = CARTESIAN_POINT ( 'NONE',  ( 17.75000000000000711, 31.24999999999999289, 3.750000000000000000 ) ) ;
#15062 = EDGE_LOOP ( 'NONE', ( #53841, #65548, #38839, #27181, #40520 ) ) ;
#15063 = CARTESIAN_POINT ( 'NONE',  ( -8.102448949553181734, 117.6049999999999898, 5.886773742842747126 ) ) ;
#15064 = CARTESIAN_POINT ( 'NONE',  ( 4.793834890952473948, 1.308853920463818987, -9.000000000000007105 ) ) ;
#15065 = ORIENTED_EDGE ( 'NONE', *, *, #7692, .T. ) ;
#15066 = ADVANCED_FACE ( 'NONE', ( #54601 ), #38487, .F. ) ;
#15067 = VECTOR ( 'NONE', #9051, 1000.000000000000000 ) ;
#15068 = DIRECTION ( 'NONE',  ( -1.000000000000000000, 0.000000000000000000, 0.000000000000000000 ) ) ;
#15069 = CARTESIAN_POINT ( 'NONE',  ( -99.89499999999998181, 6.826472737025116366, 4.959722759717898555 ) ) ;
#15070 = ORIENTED_EDGE ( 'NONE', *, *, #37464, .F. ) ;
#15071 = PRESENTATION_LAYER_ASSIGNMENT (  '', '', ( #26123 ) ) ;
#15072 = LINE ( 'NONE', #52349, #45687 ) ;
#15073 = SURFACE_STYLE_FILL_AREA ( #25238 ) ;
#15074 = EDGE_CURVE ( 'NONE', #13744, #12261, #59878, .T. ) ;
#15075 = EDGE_LOOP ( 'NONE', ( #56277, #3463, #49011 ) ) ;
#15076 = CARTESIAN_POINT ( 'NONE',  ( -2.607480562269073765, 156.0929263765337964, -8.025000000000000355 ) ) ;
#15077 = LINE ( 'NONE', #4821, #879 ) ;
#15078 = CARTESIAN_POINT ( 'NONE',  ( 0.000000000000000000, 128.9429263765338192, -8.025000000000000355 ) ) ;
#15079 = CARTESIAN_POINT ( 'NONE',  ( 26.00000000000001776, 15.00000000000000000, 35.50000000000000000 ) ) ;
#15080 = PRESENTATION_LAYER_ASSIGNMENT (  '', '', ( #1526 ) ) ;
#15081 = ORIENTED_EDGE ( 'NONE', *, *, #65990, .T. ) ;
#15082 = ORIENTED_EDGE ( 'NONE', *, *, #36084, .F. ) ;
#15083 = CARTESIAN_POINT ( 'NONE',  ( 4.716976649647096842, 127.7429263765338163, 6.492361379858953896 ) ) ;
#15084 = CARTESIAN_POINT ( 'NONE',  ( 62.24999999999998579, 33.99999999999999289, 3.750000000000000000 ) ) ;
#15085 = CARTESIAN_POINT ( 'NONE',  ( -33.89861118948982721, -9.947368421052631859, 2.722470280083840066 ) ) ;
#15086 = VECTOR ( 'NONE', #11141, 1000.000000000000000 ) ;
#15087 = SURFACE_STYLE_USAGE ( .BOTH. , #20319 ) ;
#15088 = CARTESIAN_POINT ( 'NONE',  ( 6.826472737025121695, 141.6070736234661354, -4.959722759717905660 ) ) ;
#15089 = PLANE ( 'NONE',  #43203 ) ;
#15090 = TOROIDAL_SURFACE ( 'NONE', #8337, 8.499999999999994671, 0.5000000000000000000 ) ;
#15092 = CARTESIAN_POINT ( 'NONE',  ( 107.0858988931383777, 5.000000000000000000, -16.89933289725613363 ) ) ;
#15091 = PRESENTATION_LAYER_ASSIGNMENT (  '', '', ( #43180 ) ) ;
#15093 = DIRECTION ( 'NONE',  ( 0.000000000000000000, 0.000000000000000000, -1.000000000000000000 ) ) ;
#15094 = CARTESIAN_POINT ( 'NONE',  ( 36.00000000000002842, 5.000000000000000000, -32.00402776293825724 ) ) ;
#15095 = ORIENTED_EDGE ( 'NONE', *, *, #1927, .T. ) ;
#15096 = ORIENTED_EDGE ( 'NONE', *, *, #6486, .F. ) ;
#15097 = DIRECTION ( 'NONE',  ( 0.000000000000000000, 0.000000000000000000, -1.000000000000000000 ) ) ;
#15098 = CARTESIAN_POINT ( 'NONE',  ( -182.8429263765338249, 9.058813317711329915, -2.943386871421373119 ) ) ;
#15099 = AXIS2_PLACEMENT_3D ( 'NONE', #28914, #67618, #66214 ) ;
#15100 = SURFACE_STYLE_FILL_AREA ( #19641 ) ;
#15101 = ORIENTED_EDGE ( 'NONE', *, *, #61932, .T. ) ;
#15102 = CARTESIAN_POINT ( 'NONE',  ( -153.7429263765338021, -5.598654528085803328, -7.705886871421366635 ) ) ;
#15103 = CARTESIAN_POINT ( 'NONE',  ( -177.3549999999999898, -4.716976649647093289, -6.492361379858945902 ) ) ;
#15104 = CARTESIAN_POINT ( 'NONE',  ( 45.65811388300841855, 10.21937129433612235, 6.000000000000000888 ) ) ;
#15105 = CARTESIAN_POINT ( 'NONE',  ( 47.50000000000000000, 99.99999999999992895, 9.500000000000000000 ) ) ;
#15106 = CARTESIAN_POINT ( 'NONE',  ( -180.7449999999999761, 4.716976649647094177, 6.492361379858945902 ) ) ;
#15107 = CARTESIAN_POINT ( 'NONE',  ( -180.4449999999999932, 0.000000000000000000, 8.024999999999991473 ) ) ;
#15108 = ORIENTED_EDGE ( 'NONE', *, *, #63256, .T. ) ;
#15109 = STYLED_ITEM ( 'NONE', ( #42811 ), #26993 ) ;
#15110 = FILL_AREA_STYLE ('',( #53414 ) ) ;
#15111 = CIRCLE ( 'NONE', #53256, 0.5000000000000004441 ) ;
#15112 = CARTESIAN_POINT ( 'NONE',  ( -38.44653593450800599, -11.31074412437664378, 3.500884832118608792 ) ) ;
#15113 = CARTESIAN_POINT ( 'NONE',  ( -10.00004746342556317, 11.99998022357284810, -0.3303491890816930843 ) ) ;
#15114 = CARTESIAN_POINT ( 'NONE',  ( -93.95499999999998408, -7.632228543268599452, 2.479861379858951054 ) ) ;
#15115 =( LENGTH_UNIT ( ) NAMED_UNIT ( * ) SI_UNIT ( .MILLI., .METRE. ) );
#15116 =( GEOMETRIC_REPRESENTATION_CONTEXT ( 3 ) GLOBAL_UNCERTAINTY_ASSIGNED_CONTEXT ( ( #53080 ) ) GLOBAL_UNIT_ASSIGNED_CONTEXT ( ( #16989, #21909, #49688 ) ) REPRESENTATION_CONTEXT ( 'NONE', 'WORKASPACE' ) );
#15117 = CARTESIAN_POINT ( 'NONE',  ( -90.44499999999997897, 0.000000000000000000, 8.024999999999991473 ) ) ;
#15118 = CARTESIAN_POINT ( 'NONE',  ( 9.058813317711337021, 124.6549999999999869, 2.943386871421375783 ) ) ;
#15119 = CARTESIAN_POINT ( 'NONE',  ( -70.34499999999998465, 7.632228543268599452, -2.479861379858951942 ) ) ;
#15120 = DIRECTION ( 'NONE',  ( -0.000000000000000000, -0.000000000000000000, 1.000000000000000000 ) ) ;
#15121 = AXIS2_PLACEMENT_3D ( 'NONE', #39273, #59995, #1187 ) ;
#15122 = TOROIDAL_SURFACE ( 'NONE', #8319, 13.50000000000000178, 0.5000000000000000000 ) ;
#15123 = CARTESIAN_POINT ( 'NONE',  ( -20.57648123223228254, 114.4999999999999574, 10.27659574468085069 ) ) ;
#15124 = PLANE ( 'NONE',  #29291 ) ;
#15125 = UNCERTAINTY_MEASURE_WITH_UNIT (LENGTH_MEASURE( 1.000000000000000082E-05 ), #41508, 'distance_accuracy_value', 'NONE');
#15126 = CARTESIAN_POINT ( 'NONE',  ( -74.84292637653381064, 9.058813317711329915, -2.943386871421373119 ) ) ;
#15127 = ORIENTED_EDGE ( 'NONE', *, *, #32272, .F. ) ;
#15128 = EDGE_CURVE ( 'NONE', #43530, #44582, #28033, .T. ) ;
#15129 = CARTESIAN_POINT ( 'NONE',  ( -129.1449999999999818, -4.716976649647092401, 6.492361379858946790 ) ) ;
#15130 = CARTESIAN_POINT ( 'NONE',  ( -8.437984349512095861, 145.8070736234661808, -5.166775262442723748E-16 ) ) ;
#15131 = EDGE_CURVE ( 'NONE', #34861, #60166, #61737, .T. ) ;
#15132 = ADVANCED_FACE ( 'NONE', ( #33166 ), #60551, .F. ) ;
#15134 = CYLINDRICAL_SURFACE ( 'NONE', #13498, 9.524999999999991473 ) ;
#15133 = CARTESIAN_POINT ( 'NONE',  ( 62.24999999999998579, 33.74999999999999289, 3.750000000000000000 ) ) ;
#15135 = CARTESIAN_POINT ( 'NONE',  ( -23.21231517720797655, 117.4999999999999716, -7.500000000000000000 ) ) ;
#15136 = ORIENTED_EDGE ( 'NONE', *, *, #4689, .T. ) ;
#15137 = ORIENTED_EDGE ( 'NONE', *, *, #62014, .T. ) ;
#15138 = VECTOR ( 'NONE', #43140, 1000.000000000000000 ) ;
#15139 = DIRECTION ( 'NONE',  ( 0.000000000000000000, -1.000000000000000000, 0.000000000000000000 ) ) ;
#15140 = PRESENTATION_LAYER_ASSIGNMENT (  '', '', ( #3883 ) ) ;
#15141 = MECHANICAL_DESIGN_GEOMETRIC_PRESENTATION_REPRESENTATION (  '', ( #14001 ), #65660 ) ;
#15142 = PRESENTATION_STYLE_ASSIGNMENT (( #41875 ) ) ;
#15143 = CARTESIAN_POINT ( 'NONE',  ( 24.21231517720798010, 112.4999999999999858, 10.00000000000000000 ) ) ;
#15144 = ADVANCED_FACE ( 'NONE', ( #49341 ), #39500, .T. ) ;
#15145 = ORIENTED_EDGE ( 'NONE', *, *, #59538, .T. ) ;
#15146 = CARTESIAN_POINT ( 'NONE',  ( -124.4049999999999869, -2.607480562269069768, 8.024999999999991473 ) ) ;
#15147 = EDGE_LOOP ( 'NONE', ( #29169, #45727, #28111, #56989 ) ) ;
#15148 = PRESENTATION_LAYER_ASSIGNMENT (  '', '', ( #56516 ) ) ;
#15149 = DIRECTION ( 'NONE',  ( -0.7071067811865345831, 0.000000000000000000, -0.7071067811865603403 ) ) ;
#15150 = CARTESIAN_POINT ( 'NONE',  ( -105.0570736234661666, 0.000000000000000000, 9.524999999999991473 ) ) ;
#15151 = VERTEX_POINT ( 'NONE', #7465 ) ;
#15152 = CARTESIAN_POINT ( 'NONE',  ( 8.082903768654762899, -1.105959442090949618E-15, 7.500000000000000000 ) ) ;
#15153 = DIRECTION ( 'NONE',  ( 0.000000000000000000, 0.000000000000000000, -1.000000000000000000 ) ) ;
#15154 = VERTEX_POINT ( 'NONE', #23292 ) ;
#15155 = CARTESIAN_POINT ( 'NONE',  ( -74.99999999999998579, 50.00000000000000000, -10.49999999999999822 ) ) ;
#15156 = CARTESIAN_POINT ( 'NONE',  ( 0.000000000000000000, 145.4449999999999932, -9.525000000000000355 ) ) ;
#15157 = CARTESIAN_POINT ( 'NONE',  ( 39.49999999999999289, 18.74999999999997868, 3.750000000000000000 ) ) ;
#15158 =( GEOMETRIC_REPRESENTATION_CONTEXT ( 3 ) GLOBAL_UNCERTAINTY_ASSIGNED_CONTEXT ( ( #68689 ) ) GLOBAL_UNIT_ASSIGNED_CONTEXT ( ( #14834, #52816, #44367 ) ) REPRESENTATION_CONTEXT ( 'NONE', 'WORKASPACE' ) );
#15159 = VERTEX_POINT ( 'NONE', #17691 ) ;
#15160 = VECTOR ( 'NONE', #69221, 1000.000000000000000 ) ;
#15161 = CARTESIAN_POINT ( 'NONE',  ( 48.25000000000000000, 22.24999999999998579, 4.000000000000000000 ) ) ;
#15162 = CARTESIAN_POINT ( 'NONE',  ( 10.01517768586949408, 145.8050000000000068, 1.839758294383810543E-15 ) ) ;
#15163 = PRESENTATION_STYLE_ASSIGNMENT (( #31276 ) ) ;
#15164 = ORIENTED_EDGE ( 'NONE', *, *, #45859, .T. ) ;
#15165 = CARTESIAN_POINT ( 'NONE',  ( -7.632228543268607446, 126.5429263765337993, -2.479861379858953718 ) ) ;
#15166 = CARTESIAN_POINT ( 'NONE',  ( 0.000000000000000000, 114.9999999999999574, -10.50000000000000000 ) ) ;
#15167 = UNCERTAINTY_MEASURE_WITH_UNIT (LENGTH_MEASURE( 1.000000000000000082E-05 ), #34951, 'distance_accuracy_value', 'NONE');
#15168 = PRESENTATION_STYLE_ASSIGNMENT (( #4909 ) ) ;
#15169 =( LENGTH_UNIT ( ) NAMED_UNIT ( * ) SI_UNIT ( .MILLI., .METRE. ) );
#15170 =( GEOMETRIC_REPRESENTATION_CONTEXT ( 3 ) GLOBAL_UNCERTAINTY_ASSIGNED_CONTEXT ( ( #5897 ) ) GLOBAL_UNIT_ASSIGNED_CONTEXT ( ( #23210, #7700, #24229 ) ) REPRESENTATION_CONTEXT ( 'NONE', 'WORKASPACE' ) );
#15171 =( NAMED_UNIT ( * ) SI_UNIT ( $, .STERADIAN. ) SOLID_ANGLE_UNIT ( ) );
#15172 = SURFACE_STYLE_FILL_AREA ( #52449 ) ;
#15173 = ADVANCED_FACE ( 'NONE', ( #39861, #55294 ), #7115, .F. ) ;
#15174 = ORIENTED_EDGE ( 'NONE', *, *, #59374, .F. ) ;
#15175 = ORIENTED_EDGE ( 'NONE', *, *, #27124, .T. ) ;
#15176 = CARTESIAN_POINT ( 'NONE',  ( -55.64292637653381490, -5.598654528085801552, 7.705886871421367523 ) ) ;
#15177 = MECHANICAL_DESIGN_GEOMETRIC_PRESENTATION_REPRESENTATION (  '', ( #41021 ), #18501 ) ;
#15178 = PRESENTATION_LAYER_ASSIGNMENT (  '', '', ( #60063 ) ) ;
#15179 = SURFACE_SIDE_STYLE ('',( #39831 ) ) ;
#15180 = FILL_AREA_STYLE_COLOUR ( '', #2545 ) ;
#15181 = CARTESIAN_POINT ( 'NONE',  ( -149.9050000000000296, 2.607480562269068880, -8.024999999999993250 ) ) ;
#15182 = ORIENTED_EDGE ( 'NONE', *, *, #38171, .T. ) ;
#15183 = EDGE_CURVE ( 'NONE', #65559, #62752, #56327, .T. ) ;
#15184 = UNCERTAINTY_MEASURE_WITH_UNIT (LENGTH_MEASURE( 1.000000000000000082E-05 ), #8547, 'distance_accuracy_value', 'NONE');
#15185 = CARTESIAN_POINT ( 'NONE',  ( -11.99999999999999822, -6.499999999999999112, 21.00000000000000000 ) ) ;
#15186 = FACE_OUTER_BOUND ( 'NONE', #5347, .T. ) ;
#15187 = CARTESIAN_POINT ( 'NONE',  ( 75.00000000000000000, 19.62820054891024668, 6.498343828034905734 ) ) ;
#15188 = EDGE_LOOP ( 'NONE', ( #18733, #3157, #16944, #30400 ) ) ;
#15189 = AXIS2_PLACEMENT_3D ( 'NONE', #64369, #32008, #49497 ) ;
#15190 = VERTEX_POINT ( 'NONE', #19392 ) ;
#15191 = DIRECTION ( 'NONE',  ( 1.000000000000000000, -7.709882115452468306E-16, 0.000000000000000000 ) ) ;
#15192 = CARTESIAN_POINT ( 'NONE',  ( 45.00000000000000000, 10.69371294336137979, -4.000000000000000000 ) ) ;
#15193 = CARTESIAN_POINT ( 'NONE',  ( -69.50499999999996703, -6.826472737025115478, -4.959722759717899443 ) ) ;
#15195 = ORIENTED_EDGE ( 'NONE', *, *, #54223, .T. ) ;
#15194 = STYLED_ITEM ( 'NONE', ( #62060 ), #38719 ) ;
#15196 = DIRECTION ( 'NONE',  ( 0.000000000000000000, 0.000000000000000000, -1.000000000000000000 ) ) ;
#15197 = AXIS2_PLACEMENT_3D ( 'NONE', #5076, #32486, #64527 ) ;
#15198 = CARTESIAN_POINT ( 'NONE',  ( -195.0000000000000000, 0.000000000000000000, 0.000000000000000000 ) ) ;
#15199 = DIRECTION ( 'NONE',  ( 0.000000000000000000, 1.000000000000000000, 0.000000000000000000 ) ) ;
#15200 = AXIS2_PLACEMENT_3D ( 'NONE', #10955, #59132, #64429 ) ;
#15201 = ORIENTED_EDGE ( 'NONE', *, *, #1733, .F. ) ;
#15202 = CARTESIAN_POINT ( 'NONE',  ( -75.75000000000000000, -3.000000000000000000, 6.000000000000001776 ) ) ;
#15203 = CIRCLE ( 'NONE', #67956, 1.000000000000000888 ) ;
#15204 = CARTESIAN_POINT ( 'NONE',  ( -169.9429263765337907, 0.000000000000000000, 9.524999999999991473 ) ) ;
#15205 = CARTESIAN_POINT ( 'NONE',  ( 65.49999999999997158, 2.470600640510325396E-15, -12.00000000000000000 ) ) ;
#15206 =( NAMED_UNIT ( * ) SI_UNIT ( $, .STERADIAN. ) SOLID_ANGLE_UNIT ( ) );
#15207 = CARTESIAN_POINT ( 'NONE',  ( -8.102448949553181734, 146.4950000000000045, 5.886773742842747126 ) ) ;
#15208 = CARTESIAN_POINT ( 'NONE',  ( -98.09499999999997044, -2.607480562269071545, -8.024999999999991473 ) ) ;
#15209 = ADVANCED_FACE ( 'NONE', ( #24323 ), #62996, .F. ) ;
#15210 = DIRECTION ( 'NONE',  ( -1.000000000000000000, -0.000000000000000000, -0.000000000000000000 ) ) ;
#15211 = LINE ( 'NONE', #62999, #47228 ) ;
#15212 = UNCERTAINTY_MEASURE_WITH_UNIT (LENGTH_MEASURE( 1.000000000000000082E-05 ), #29633, 'distance_accuracy_value', 'NONE');
#15213 = AXIS2_PLACEMENT_3D ( 'NONE', #58149, #52540, #9962 ) ;
#15214 = CARTESIAN_POINT ( 'NONE',  ( -41.05151532188900632, 107.6719357445258680, -3.224518739502661990 ) ) ;
#15215 = ORIENTED_EDGE ( 'NONE', *, *, #12209, .F. ) ;
#15216 = CARTESIAN_POINT ( 'NONE',  ( -131.3929263765338078, 8.102448949553176405, 5.886773742842740909 ) ) ;
#15217 = FILL_AREA_STYLE ('',( #48618 ) ) ;
#15218 = LINE ( 'NONE', #42317, #25366 ) ;
#15219 = CARTESIAN_POINT ( 'NONE',  ( -157.6449999999999818, 4.716976649647091513, -6.492361379858946790 ) ) ;
#15220 = SURFACE_STYLE_FILL_AREA ( #41589 ) ;
#15221 = ADVANCED_FACE ( 'NONE', ( #51075 ), #43835, .T. ) ;
#15222 = CARTESIAN_POINT ( 'NONE',  ( 0.000000000000000000, 2.500000000000000000, 0.000000000000000000 ) ) ;
#15223 = LINE ( 'NONE', #21139, #64415 ) ;
#15224 = LINE ( 'NONE', #3534, #32702 ) ;
#15225 = ORIENTED_EDGE ( 'NONE', *, *, #63207, .T. ) ;
#15226 = ORIENTED_EDGE ( 'NONE', *, *, #5978, .T. ) ;
#15227 = PRESENTATION_LAYER_ASSIGNMENT (  '', '', ( #7305 ) ) ;
#15228 = DIRECTION ( 'NONE',  ( 0.000000000000000000, 0.000000000000000000, -1.000000000000000000 ) ) ;
#15229 = CARTESIAN_POINT ( 'NONE',  ( -143.5429263765338135, 9.058813317711329915, 2.943386871421369566 ) ) ;
#15230 = DIRECTION ( 'NONE',  ( 1.000000000000000000, -1.084202172485504434E-16, -0.000000000000000000 ) ) ;
#15231 = CARTESIAN_POINT ( 'NONE',  ( -174.0570736234661808, 0.000000000000000000, 9.524999999999991473 ) ) ;
#15232 = EDGE_CURVE ( 'NONE', #13259, #23198, #57032, .T. ) ;
#15233 = VERTEX_POINT ( 'NONE', #51769 ) ;
#15234 = CARTESIAN_POINT ( 'NONE',  ( -146.1549999999999727, 7.632228543268600340, 2.479861379858949277 ) ) ;
#15235 = VECTOR ( 'NONE', #19061, 1000.000000000000000 ) ;
#15236 = ORIENTED_EDGE ( 'NONE', *, *, #31614, .T. ) ;
#15237 = DIRECTION ( 'NONE',  ( 1.000000000000000000, -0.000000000000000000, -0.000000000000000000 ) ) ;
#15238 = ORIENTED_EDGE ( 'NONE', *, *, #53837, .F. ) ;
#15239 = FACE_OUTER_BOUND ( 'NONE', #49577, .T. ) ;
#15240 = FILL_AREA_STYLE ('',( #8549 ) ) ;
#15241 = CARTESIAN_POINT ( 'NONE',  ( -3.094860106618434248, 122.7949999999999875, 9.525000000000000355 ) ) ;
#15242 = DIRECTION ( 'NONE',  ( 0.000000000000000000, 1.000000000000000000, -0.000000000000000000 ) ) ;
#15243 = VERTEX_POINT ( 'NONE', #3516 ) ;
#15244 = CARTESIAN_POINT ( 'NONE',  ( -57.59292637653379643, -3.094860106618431139, -9.524999999999991473 ) ) ;
#15245 = CARTESIAN_POINT ( 'NONE',  ( -8.102448949553179958, 117.0049999999999670, -5.886773742842749790 ) ) ;
#15246 = CARTESIAN_POINT ( 'NONE',  ( -60.35499999999998977, -4.716976649647093289, -6.492361379858945902 ) ) ;
#15247 = VECTOR ( 'NONE', #65953, 1000.000000000000000 ) ;
#15248 = DIRECTION ( 'NONE',  ( -0.000000000000000000, 0.3420201433256694346, 0.9396926207859082059 ) ) ;
#15249 = ORIENTED_EDGE ( 'NONE', *, *, #10042, .F. ) ;
#15250 = CARTESIAN_POINT ( 'NONE',  ( -3.094860106618434248, 147.9049999999999727, 9.525000000000000355 ) ) ;
#15251 = UNCERTAINTY_MEASURE_WITH_UNIT (LENGTH_MEASURE( 1.000000000000000082E-05 ), #14851, 'distance_accuracy_value', 'NONE');
#15252 = FILL_AREA_STYLE_COLOUR ( '', #11964 ) ;
#15253 = SPHERICAL_SURFACE ( 'NONE', #144, 0.2500000000000000000 ) ;
#15254 = DIRECTION ( 'NONE',  ( -1.000000000000000000, 0.000000000000000000, 0.000000000000000000 ) ) ;
#15255 = VERTEX_POINT ( 'NONE', #41238 ) ;
#15256 = SURFACE_SIDE_STYLE ('',( #42004 ) ) ;
#15257 = DIRECTION ( 'NONE',  ( -1.000000000000000000, -0.000000000000000000, -0.000000000000000000 ) ) ;
#15258 = CARTESIAN_POINT ( 'NONE',  ( -47.84499999999997044, -7.632228543268599452, 2.479861379858951054 ) ) ;
#15259 = EDGE_LOOP ( 'NONE', ( #37149, #57746, #62306, #46864 ) ) ;
#15260 = CARTESIAN_POINT ( 'NONE',  ( 3.607123150363803710, 111.8710042735134209, -7.332553890433502808 ) ) ;
#15261 = MECHANICAL_DESIGN_GEOMETRIC_PRESENTATION_REPRESENTATION (  '', ( #53391 ), #19680 ) ;
#15262 = CIRCLE ( 'NONE', #54528, 1.000000000000000000 ) ;
#15263 = DIRECTION ( 'NONE',  ( 0.000000000000000000, 0.000000000000000000, 1.000000000000000000 ) ) ;
#15264 = EDGE_LOOP ( 'NONE', ( #29735, #27497, #8046, #33633, #22213 ) ) ;
#15265 = FACE_OUTER_BOUND ( 'NONE', #33067, .T. ) ;
#15266 = SURFACE_STYLE_FILL_AREA ( #63421 ) ;
#15267 = ORIENTED_EDGE ( 'NONE', *, *, #66636, .F. ) ;
#15268 = CARTESIAN_POINT ( 'NONE',  ( -128.6070736234661922, -8.102448949553174629, 5.886773742842742685 ) ) ;
#15269 = PRESENTATION_LAYER_ASSIGNMENT (  '', '', ( #44457 ) ) ;
#15270 = SURFACE_STYLE_FILL_AREA ( #47996 ) ;
#15271 = CARTESIAN_POINT ( 'NONE',  ( -97.10499999999998977, -6.826472737025115478, 4.959722759717900331 ) ) ;
#15272 = EDGE_LOOP ( 'NONE', ( #53429, #1019, #29915, #1336 ) ) ;
#15273 = FILL_AREA_STYLE_COLOUR ( '', #49689 ) ;
#15274 = AXIS2_PLACEMENT_3D ( 'NONE', #61035, #29010, #67031 ) ;
#15275 = CARTESIAN_POINT ( 'NONE',  ( -133.8570736234661638, -5.598654528085803328, -7.705886871421366635 ) ) ;
#15276 = AXIS2_PLACEMENT_3D ( 'NONE', #19969, #41469, #60041 ) ;
#15277 = PLANE ( 'NONE',  #13765 ) ;
#15278 = CARTESIAN_POINT ( 'NONE',  ( 3.094860106618435136, 154.2949999999999875, -9.525000000000000355 ) ) ;
#15279 = CARTESIAN_POINT ( 'NONE',  ( -72.35707362346617799, 5.598654528085804216, 7.705886871421366635 ) ) ;
#15280 = FILL_AREA_STYLE_COLOUR ( '', #998 ) ;
#15281 = ORIENTED_EDGE ( 'NONE', *, *, #33593, .F. ) ;
#15282 = DIRECTION ( 'NONE',  ( -1.000000000000000000, 0.000000000000000000, 0.000000000000000000 ) ) ;
#15283 =( NAMED_UNIT ( * ) SI_UNIT ( $, .STERADIAN. ) SOLID_ANGLE_UNIT ( ) );
#15285 = SURFACE_STYLE_FILL_AREA ( #43073 ) ;
#15284 = CARTESIAN_POINT ( 'NONE',  ( -44.99999999999998579, 119.9999999999999716, -7.500000000000000000 ) ) ;
#15286 = AXIS2_PLACEMENT_3D ( 'NONE', #34140, #17967, #44054 ) ;
#15287 = CARTESIAN_POINT ( 'NONE',  ( -114.5050000000000097, -6.826472737025115478, -4.959722759717899443 ) ) ;
#15288 = CARTESIAN_POINT ( 'NONE',  ( 0.000000000000000000, 33.74999999999998579, 4.000000000000000000 ) ) ;
#15289 = CARTESIAN_POINT ( 'NONE',  ( -8.102448949553181734, 115.8949999999999960, -5.886773742842749790 ) ) ;
#15290 = CARTESIAN_POINT ( 'NONE',  ( -127.6450000000000102, 4.716976649647091513, -6.492361379858946790 ) ) ;
#15291 = AXIS2_PLACEMENT_3D ( 'NONE', #20403, #14424, #46495 ) ;
#15292 = EDGE_CURVE ( 'NONE', #10407, #6631, #46531, .T. ) ;
#15293 = FILL_AREA_STYLE_COLOUR ( '', #35888 ) ;
#15294 = COLOUR_RGB ( '', 0.40784314, 0.44705882, 0.49803922) ;
#15295 = EDGE_CURVE ( 'NONE', #27359, #12327, #68289, .T. ) ;
#15296 = CARTESIAN_POINT ( 'NONE',  ( 23.71231517720798010, 117.4999999999999716, 9.500000000000000000 ) ) ;
#15297 = VERTEX_POINT ( 'NONE', #61951 ) ;
#15298 = COLOUR_RGB ( '', 0.09019608, 0.27058824, 0.51372549) ;
#15299 = CARTESIAN_POINT ( 'NONE',  ( -166.7929263765337851, -3.094860106618429807, 9.524999999999991473 ) ) ;
#15300 = FILL_AREA_STYLE_COLOUR ( '', #19218 ) ;
#15301 = LINE ( 'NONE', #63096, #30873 ) ;
#15302 = EDGE_CURVE ( 'NONE', #29672, #14179, #52809, .T. ) ;
#15303 = ADVANCED_FACE ( 'NONE', ( #29950 ), #35939, .F. ) ;
#15304 =( LENGTH_UNIT ( ) NAMED_UNIT ( * ) SI_UNIT ( .MILLI., .METRE. ) );
#15305 = ADVANCED_FACE ( 'NONE', ( #3889, #53495 ), #48605, .T. ) ;
#15306 = CARTESIAN_POINT ( 'NONE',  ( -21.02379605245189964, 114.6413612702713465, -10.00000000000000000 ) ) ;
#15307 = CARTESIAN_POINT ( 'NONE',  ( 3.749999999999999556, 33.74999999999998579, -4.000000000000000000 ) ) ;
#15308 = VERTEX_POINT ( 'NONE', #4223 ) ;
#15309 = EDGE_CURVE ( 'NONE', #6894, #46319, #56568, .T. ) ;
#15310 = CARTESIAN_POINT ( 'NONE',  ( -73.64292637653380780, -5.598654528085801552, 7.705886871421367523 ) ) ;
#15311 = DIRECTION ( 'NONE',  ( -1.000000000000000000, -1.156482317317878627E-15, 0.000000000000000000 ) ) ;
#15312 = CARTESIAN_POINT ( 'NONE',  ( 0.000000000000000000, 0.000000000000000000, 0.7500000000000000000 ) ) ;
#15313 = MECHANICAL_DESIGN_GEOMETRIC_PRESENTATION_REPRESENTATION (  '', ( #27594 ), #22007 ) ;
#15314 = ADVANCED_FACE ( 'NONE', ( #4591 ), #10923, .T. ) ;
#15315 =( NAMED_UNIT ( * ) PLANE_ANGLE_UNIT ( ) SI_UNIT ( $, .RADIAN. ) );
#15316 = DIRECTION ( 'NONE',  ( -0.000000000000000000, -1.000000000000000000, -0.000000000000000000 ) ) ;
#15317 = STYLED_ITEM ( 'NONE', ( #67129 ), #64439 ) ;
#15318 = CARTESIAN_POINT ( 'NONE',  ( -184.0000000000000000, -7.358988424933670558, 3.200923985616050071 ) ) ;
#15319 = ORIENTED_EDGE ( 'NONE', *, *, #60488, .F. ) ;
#15320 = CARTESIAN_POINT ( 'NONE',  ( 71.50000000000000000, 35.92875272052971525, -9.500000000000000000 ) ) ;
#15321 = VERTEX_POINT ( 'NONE', #58419 ) ;
#15322 = CARTESIAN_POINT ( 'NONE',  ( -110.8429263765337964, 9.058813317711329915, -2.943386871421373119 ) ) ;
#15323 = AXIS2_PLACEMENT_3D ( 'NONE', #49854, #7608, #1592 ) ;
#15324 =( BOUNDED_CURVE ( )  B_SPLINE_CURVE ( 2, ( #42526, #68893, #19970, #9805, #24907, #51659, #9104, #47111, #52020, #69232, #25595 ),
 .UNSPECIFIED., .F., .F. ) 
 B_SPLINE_CURVE_WITH_KNOTS ( ( 3, 2, 2, 2, 2, 3 ),
 ( 0.08823529411764713393, 0.09411764705882361137, 0.1000000000000000888, 0.1058823529411765663, 0.1117647058823530437, 0.1176470588235295212 ),
 .UNSPECIFIED. ) 
 CURVE ( )  GEOMETRIC_REPRESENTATION_ITEM ( )  RATIONAL_B_SPLINE_CURVE ( ( 0.9999999999999994449, 0.9510565162951540863, 1.000000000000000000, 0.9510565162951535312, 1.000000000000000000, 0.9510565162951535312, 1.000000000000000000, 0.9510565162951535312, 1.000000000000000000, 0.9510565162951526430, 1.000000000000000888 ) ) 
 REPRESENTATION_ITEM ( '' )  );
#15325 = CARTESIAN_POINT ( 'NONE',  ( -74.99999999999998579, 50.00000000000000000, -12.00000000000000000 ) ) ;
#15326 = CARTESIAN_POINT ( 'NONE',  ( 4.716976649647096842, 146.8570736234661638, 6.492361379858953896 ) ) ;
#15327 = ORIENTED_EDGE ( 'NONE', *, *, #60829, .F. ) ;
#15328 = DIRECTION ( 'NONE',  ( -0.000000000000000000, -0.000000000000000000, -1.000000000000000000 ) ) ;
#15329 = CARTESIAN_POINT ( 'NONE',  ( -91.25499999999999545, -4.716976649647092401, 6.492361379858946790 ) ) ;
#15330 = UNCERTAINTY_MEASURE_WITH_UNIT (LENGTH_MEASURE( 1.000000000000000082E-05 ), #37642, 'distance_accuracy_value', 'NONE');
#15331 = ORIENTED_EDGE ( 'NONE', *, *, #21342, .F. ) ;
#15332 = DIRECTION ( 'NONE',  ( 0.000000000000000000, 0.3420201433256629953, -0.9396926207859104263 ) ) ;
#15333 = AXIS2_PLACEMENT_3D ( 'NONE', #22821, #44319, #49554 ) ;
#15334 = DIRECTION ( 'NONE',  ( -1.000000000000000000, 0.000000000000000000, 0.000000000000000000 ) ) ;
#15335 = CARTESIAN_POINT ( 'NONE',  ( -83.75707362346616947, -5.598654528085801552, 7.705886871421367523 ) ) ;
#15336 = CARTESIAN_POINT ( 'NONE',  ( -58.57094193006191318, -7.669019089512441489, -0.3330098372451437139 ) ) ;
#15337 = MECHANICAL_DESIGN_GEOMETRIC_PRESENTATION_REPRESENTATION (  '', ( #17583 ), #19815 ) ;
#15338 = ORIENTED_EDGE ( 'NONE', *, *, #65927, .F. ) ;
#15339 = DIRECTION ( 'NONE',  ( -0.000000000000000000, -0.000000000000000000, -1.000000000000000000 ) ) ;
#15340 = CARTESIAN_POINT ( 'NONE',  ( -72.29499999999998749, -2.607480562269069768, 8.024999999999991473 ) ) ;
#15341 = EDGE_LOOP ( 'NONE', ( #39744, #12932, #42164 ) ) ;
#15342 = MECHANICAL_DESIGN_GEOMETRIC_PRESENTATION_REPRESENTATION (  '', ( #42326 ), #66984 ) ;
#15343 = FACE_OUTER_BOUND ( 'NONE', #41132, .T. ) ;
#15344 = DIRECTION ( 'NONE',  ( -0.000000000000000000, -1.000000000000000000, 0.000000000000000000 ) ) ;
#15345 = DIRECTION ( 'NONE',  ( -0.3403530053317448401, 0.9351121967924955758, 0.09861547125863370789 ) ) ;
#15346 = ORIENTED_EDGE ( 'NONE', *, *, #19128, .T. ) ;
#15347 = CARTESIAN_POINT ( 'NONE',  ( 92.41620014002536720, 5.000000000000000000, 29.00402776293826079 ) ) ;
#15348 = DIRECTION ( 'NONE',  ( -1.000000000000000000, 0.000000000000000000, -0.000000000000000000 ) ) ;
#15349 = CARTESIAN_POINT ( 'NONE',  ( -44.99999999999998579, 119.9999999999999716, 9.500000000000000000 ) ) ;
#15350 = PRESENTATION_STYLE_ASSIGNMENT (( #30779 ) ) ;
#15351 = ORIENTED_EDGE ( 'NONE', *, *, #53071, .T. ) ;
#15352 = CARTESIAN_POINT ( 'NONE',  ( 13.25000000000000355, 28.24999999999998934, 3.750000000000000000 ) ) ;
#15353 = EDGE_LOOP ( 'NONE', ( #32679, #21026, #58909, #11892 ) ) ;
#15354 =( LENGTH_UNIT ( ) NAMED_UNIT ( * ) SI_UNIT ( .MILLI., .METRE. ) );
#15355 = DIRECTION ( 'NONE',  ( 1.073081856240828566E-16, -1.000000000000000000, 0.000000000000000000 ) ) ;
#15356 = CARTESIAN_POINT ( 'NONE',  ( -48.50000000000000000, 50.00000000000000000, 7.500000000000000000 ) ) ;
#15357 = CARTESIAN_POINT ( 'NONE',  ( -162.0570736234661808, 0.000000000000000000, 9.524999999999991473 ) ) ;
#15358 = CARTESIAN_POINT ( 'NONE',  ( 10.01517768586949408, 120.6949999999999790, 1.839758294383810543E-15 ) ) ;
#15359 = CARTESIAN_POINT ( 'NONE',  ( -104.0070736234661695, -8.102448949553172852, -5.886773742842741797 ) ) ;
#15360 = DIRECTION ( 'NONE',  ( 0.000000000000000000, 1.000000000000000000, -0.000000000000000000 ) ) ;
#15361 = PRODUCT_DEFINITION_SHAPE ( 'NONE', 'NONE',  #29610 ) ;
#15362 = ORIENTED_EDGE ( 'NONE', *, *, #26440, .F. ) ;
#15363 = DIRECTION ( 'NONE',  ( 0.000000000000000000, 0.000000000000000000, -1.000000000000000000 ) ) ;
#15365 = DIRECTION ( 'NONE',  ( -0.000000000000000000, -1.000000000000000000, -0.000000000000000000 ) ) ;
#15364 = DIRECTION ( 'NONE',  ( 0.000000000000000000, -1.000000000000000000, 0.000000000000000000 ) ) ;
#15367 = FILL_AREA_STYLE_COLOUR ( '', #65840 ) ;
#15366 = PRESENTATION_LAYER_ASSIGNMENT (  '', '', ( #27642 ) ) ;
#15368 = CARTESIAN_POINT ( 'NONE',  ( -144.8049999999999216, -8.437984349512085203, 5.166775262442717831E-16 ) ) ;
#15369 = EDGE_CURVE ( 'NONE', #37989, #5853, #41945, .T. ) ;
#15370 = PRESENTATION_LAYER_ASSIGNMENT (  '', '', ( #44592 ) ) ;
#15371 = LINE ( 'NONE', #43156, #13413 ) ;
#15372 = CARTESIAN_POINT ( 'NONE',  ( -152.9950000000000045, -6.826472737025115478, 4.959722759717900331 ) ) ;
#15373 = EDGE_CURVE ( 'NONE', #51630, #21322, #31680, .T. ) ;
#15374 = PRESENTATION_LAYER_ASSIGNMENT (  '', '', ( #63629 ) ) ;
#15375 = CARTESIAN_POINT ( 'NONE',  ( -141.8949999999999818, 6.826472737025115478, 4.959722759717899443 ) ) ;
#15376 = ORIENTED_EDGE ( 'NONE', *, *, #67393, .F. ) ;
#15377 = ADVANCED_FACE ( 'NONE', ( #5981 ), #645, .F. ) ;
#15378 = DIRECTION ( 'NONE',  ( -1.000000000000000000, 0.000000000000000000, 0.000000000000000000 ) ) ;
#15379 = CARTESIAN_POINT ( 'NONE',  ( -13.25000000000000355, 28.24999999999998934, 3.750000000000000000 ) ) ;
#15380 = CARTESIAN_POINT ( 'NONE',  ( 20.94636006565341191, 149.9999999999999716, -9.500000000000000000 ) ) ;
#15381 = CARTESIAN_POINT ( 'NONE',  ( -54.95499999999997698, -7.632228543268599452, 2.479861379858951054 ) ) ;
#15382 = CARTESIAN_POINT ( 'NONE',  ( 10.01517768586949231, 151.8049999999999784, 1.839758294383810543E-15 ) ) ;
#15383 = CARTESIAN_POINT ( 'NONE',  ( -52.04292637653379217, -9.058813317711329915, -2.943386871421370898 ) ) ;
#15384 = CARTESIAN_POINT ( 'NONE',  ( -143.4570736234661865, -9.058813317711329915, 2.943386871421371787 ) ) ;
#15385 = EDGE_CURVE ( 'NONE', #31871, #61605, #12994, .T. ) ;
#15386 = FILL_AREA_STYLE_COLOUR ( '', #53675 ) ;
#15387 = EDGE_CURVE ( 'NONE', #52121, #26743, #1075, .T. ) ;
#15388 = LINE ( 'NONE', #16075, #64059 ) ;
#15389 = LINE ( 'NONE', #9043, #56216 ) ;
#15390 = DIRECTION ( 'NONE',  ( 0.000000000000000000, 0.000000000000000000, -1.000000000000000000 ) ) ;
#15391 = CARTESIAN_POINT ( 'NONE',  ( 29.00000000000002842, 0.000000000000000000, 3.902931319921305165E-16 ) ) ;
#15392 = CARTESIAN_POINT ( 'NONE',  ( -17.75000000000000711, 31.24999999999999289, 3.750000000000000000 ) ) ;
#15393 = ORIENTED_EDGE ( 'NONE', *, *, #5096, .T. ) ;
#15394 = VERTEX_POINT ( 'NONE', #11957 ) ;
#15395 =( NAMED_UNIT ( * ) SI_UNIT ( $, .STERADIAN. ) SOLID_ANGLE_UNIT ( ) );
#15396 = CARTESIAN_POINT ( 'NONE',  ( 4.716976649647096842, 116.8570736234661638, 6.492361379858953896 ) ) ;
#15397 = SURFACE_STYLE_FILL_AREA ( #16088 ) ;
#15398 = SURFACE_SIDE_STYLE ('',( #9054 ) ) ;
#15399 = ORIENTED_EDGE ( 'NONE', *, *, #24584, .T. ) ;
#15400 = ORIENTED_EDGE ( 'NONE', *, *, #43665, .T. ) ;
#15401 = VECTOR ( 'NONE', #36471, 1000.000000000000000 ) ;
#15402 = CARTESIAN_POINT ( 'NONE',  ( 27.99999999999999289, 43.00000000000000000, -90.00000000000000000 ) ) ;
#15403 = FILL_AREA_STYLE_COLOUR ( '', #61223 ) ;
#15404 = CARTESIAN_POINT ( 'NONE',  ( -20.71231517720797655, 149.4999999999999716, 10.00000000000000000 ) ) ;
#15405 = VERTEX_POINT ( 'NONE', #60472 ) ;
#15406 = CARTESIAN_POINT ( 'NONE',  ( 9.058813317711338797, 121.9549999999999841, -2.943386871421372675 ) ) ;
#15407 = SURFACE_SIDE_STYLE ('',( #26597 ) ) ;
#15408 = MECHANICAL_DESIGN_GEOMETRIC_PRESENTATION_REPRESENTATION (  '', ( #6381 ), #18732 ) ;
#15409 = FACE_OUTER_BOUND ( 'NONE', #28416, .T. ) ;
#15410 = CARTESIAN_POINT ( 'NONE',  ( -34.99999999999992895, 112.9999999999999858, 7.500000000000000000 ) ) ;
#15411 = CARTESIAN_POINT ( 'NONE',  ( -104.5449999999999875, -7.632228543268600340, -2.479861379858950166 ) ) ;
#15412 = ORIENTED_EDGE ( 'NONE', *, *, #39658, .F. ) ;
#15413 =( BOUNDED_CURVE ( )  B_SPLINE_CURVE ( 2, ( #45348, #25836, #15335, #37140, #40067, #45691, #18893, #40391, #13274, #61799, #35091 ),
 .UNSPECIFIED., .F., .F. ) 
 B_SPLINE_CURVE_WITH_KNOTS ( ( 3, 2, 2, 2, 2, 3 ),
 ( 0.7173913043478260532, 0.7195652173913043015, 0.7217391304347826608, 0.7239130434782609091, 0.7260869565217391575, 0.7282608695652174058 ),
 .UNSPECIFIED. ) 
 CURVE ( )  GEOMETRIC_REPRESENTATION_ITEM ( )  RATIONAL_B_SPLINE_CURVE ( ( 1.000000000000000000, 0.9510565162951535312, 1.000000000000000000, 0.9510565162951535312, 1.000000000000000000, 0.9510565162951535312, 1.000000000000000000, 0.9510565162951535312, 1.000000000000000000, 0.9510565162951535312, 1.000000000000000000 ) ) 
 REPRESENTATION_ITEM ( '' )  );
#15414 = ADVANCED_FACE ( 'NONE', ( #44710 ), #970, .T. ) ;
#15415 = CARTESIAN_POINT ( 'NONE',  ( 8.468573276252547188, 153.4411133142860137, -0.3466697492072565168 ) ) ;
#15416 =( NAMED_UNIT ( * ) PLANE_ANGLE_UNIT ( ) SI_UNIT ( $, .RADIAN. ) );
#15417 = VERTEX_POINT ( 'NONE', #44018 ) ;
#15418 = CARTESIAN_POINT ( 'NONE',  ( 7.632228543268607446, 155.0429263765338419, 2.479861379858954606 ) ) ;
#15419 = CARTESIAN_POINT ( 'NONE',  ( 69.99999999999998579, 36.75000000000000000, 3.000000000000000000 ) ) ;
#15420 = DIRECTION ( 'NONE',  ( -1.000000000000000000, 0.000000000000000000, 0.000000000000000000 ) ) ;
#15421 = AXIS2_PLACEMENT_3D ( 'NONE', #17325, #16965, #65474 ) ;
#15422 = DIRECTION ( 'NONE',  ( -0.000000000000000000, -1.000000000000000000, -0.000000000000000000 ) ) ;
#15423 = EDGE_LOOP ( 'NONE', ( #7336, #60424, #36272 ) ) ;
#15424 = DIRECTION ( 'NONE',  ( -0.000000000000000000, -0.000000000000000000, 1.000000000000000000 ) ) ;
#15425 = DIRECTION ( 'NONE',  ( 0.000000000000000000, 0.000000000000000000, -1.000000000000000000 ) ) ;
#15426 = PRESENTATION_STYLE_ASSIGNMENT (( #19959 ) ) ;
#15427 = CARTESIAN_POINT ( 'NONE',  ( -34.48878133304234694, -10.53184416402257284, 3.891476709836706238 ) ) ;
#15428 =( LENGTH_UNIT ( ) NAMED_UNIT ( * ) SI_UNIT ( .MILLI., .METRE. ) );
#15429 = LINE ( 'NONE', #27305, #64493 ) ;
#15430 = CYLINDRICAL_SURFACE ( 'NONE', #41817, 0.2500000000000002220 ) ;
#15431 = DIRECTION ( 'NONE',  ( 1.000000000000000000, 0.000000000000000000, 0.000000000000000000 ) ) ;
#15432 = FACE_OUTER_BOUND ( 'NONE', #36727, .T. ) ;
#15433 = ORIENTED_EDGE ( 'NONE', *, *, #42612, .F. ) ;
#15434 = EDGE_LOOP ( 'NONE', ( #65022, #55958, #5638 ) ) ;
#15435 =( NAMED_UNIT ( * ) SI_UNIT ( $, .STERADIAN. ) SOLID_ANGLE_UNIT ( ) );
#15436 = FILL_AREA_STYLE ('',( #57269 ) ) ;
#15437 = CARTESIAN_POINT ( 'NONE',  ( -169.7070736234663570, -3.094860106621120988, -9.524999999998039257 ) ) ;
#15438 = EDGE_CURVE ( 'NONE', #59058, #61310, #57294, .T. ) ;
#15439 = EDGE_LOOP ( 'NONE', ( #37217, #52852, #46844, #35159 ) ) ;
#15440 = CARTESIAN_POINT ( 'NONE',  ( -154.0429263765338135, -9.058813317711329915, -2.943386871421370898 ) ) ;
#15441 = CARTESIAN_POINT ( 'NONE',  ( -168.5049999999999955, -6.826472737025115478, -4.959722759717899443 ) ) ;
#15442 = ADVANCED_FACE ( 'NONE', ( #39420, #48948 ), #23216, .F. ) ;
#15443 = DIRECTION ( 'NONE',  ( 0.000000000000000000, 0.000000000000000000, 1.000000000000000000 ) ) ;
#15444 = CARTESIAN_POINT ( 'NONE',  ( -148.2570736234661979, 5.598654528085800663, -7.705886871421367523 ) ) ;
#15445 = CARTESIAN_POINT ( 'NONE',  ( -182.6949999999999648, -8.437984349512085203, 5.166775262442717831E-16 ) ) ;
#15446 = CARTESIAN_POINT ( 'NONE',  ( -169.4949999999999761, 6.826472737025113702, -4.959722759717902107 ) ) ;
#15447 = VERTEX_POINT ( 'NONE', #6326 ) ;
#15448 = EDGE_CURVE ( 'NONE', #65737, #7265, #25857, .T. ) ;
#15449 = PLANE ( 'NONE',  #36983 ) ;
#15450 = CARTESIAN_POINT ( 'NONE',  ( -12.34763874847350529, 11.22577880721510368, -4.241592803799083988 ) ) ;
#15451 = CARTESIAN_POINT ( 'NONE',  ( -83.15499999999998693, 7.632228543268600340, 2.479861379858949277 ) ) ;
#15452 = PRESENTATION_STYLE_ASSIGNMENT (( #56946 ) ) ;
#15453 = CARTESIAN_POINT ( 'NONE',  ( -169.2570736234661695, 5.598654528085800663, -7.705886871421367523 ) ) ;
#15454 = CARTESIAN_POINT ( 'NONE',  ( -74.99999999976296294, 35.99166914554462693, -9.502300335055899438 ) ) ;
#15455 = AXIS2_PLACEMENT_3D ( 'NONE', #46043, #41117, #68175 ) ;
#15456 = ADVANCED_FACE ( 'NONE', ( #7025 ), #6661, .T. ) ;
#15457 = CARTESIAN_POINT ( 'NONE',  ( -91.49499999999997613, 6.826472737025113702, -4.959722759717902107 ) ) ;
#15458 = CARTESIAN_POINT ( 'NONE',  ( -3.094860106618432471, 125.7049999999999841, -9.525000000000000355 ) ) ;
#15459 = CONICAL_SURFACE ( 'NONE', #9824, 9.000000000000000000, 0.7853981633974500554 ) ;
#15460 = CARTESIAN_POINT ( 'NONE',  ( -75.00000000000000000, 8.747703778475438341, -6.883446876413754190 ) ) ;
#15461 = ADVANCED_FACE ( 'NONE', ( #23541 ), #28451, .T. ) ;
#15462 = CARTESIAN_POINT ( 'NONE',  ( -172.5570736234661808, -1.166476076187852838E-15, -9.524999999999991473 ) ) ;
#15463 = DIRECTION ( 'NONE',  ( 0.000000000000000000, 0.000000000000000000, -1.000000000000000000 ) ) ;
#15464 = CARTESIAN_POINT ( 'NONE',  ( -75.44292637653379074, -1.166476076187852838E-15, -9.524999999999991473 ) ) ;
#15465 = FACE_OUTER_BOUND ( 'NONE', #59171, .T. ) ;
#15466 = ORIENTED_EDGE ( 'NONE', *, *, #57141, .F. ) ;
#15467 = EDGE_CURVE ( 'NONE', #7095, #35876, #43669, .T. ) ;
#15468 =( LENGTH_UNIT ( ) NAMED_UNIT ( * ) SI_UNIT ( .MILLI., .METRE. ) );
#15469 = VECTOR ( 'NONE', #33709, 1000.000000000000000 ) ;
#15470 =( LENGTH_UNIT ( ) NAMED_UNIT ( * ) SI_UNIT ( .MILLI., .METRE. ) );
#15471 = CARTESIAN_POINT ( 'NONE',  ( -63.29292637653379927, 3.094860106618428031, -9.524999999999993250 ) ) ;
#15472 = CARTESIAN_POINT ( 'NONE',  ( 48.50000000000000000, 14.49137674618942562, -7.500000000000000000 ) ) ;
#15473 = ORIENTED_EDGE ( 'NONE', *, *, #35689, .F. ) ;
#15474 = EDGE_LOOP ( 'NONE', ( #31815, #52664, #14167, #10881, #7750 ) ) ;
#15475 = LINE ( 'NONE', #20011, #64394 ) ;
#15476 = CARTESIAN_POINT ( 'NONE',  ( -134.0929263765344501, 3.094860106629121699, 9.524999999992225241 ) ) ;
#15477 = APPLICATION_CONTEXT ( 'automotive_design' ) ;
#15478 = CYLINDRICAL_SURFACE ( 'NONE', #68746, 12.50000000000001066 ) ;
#15479 = SURFACE_STYLE_USAGE ( .BOTH. , #5221 ) ;
#15480 = DIRECTION ( 'NONE',  ( 0.000000000000000000, 0.000000000000000000, 1.000000000000000000 ) ) ;
#15481 = EDGE_LOOP ( 'NONE', ( #24989, #5676, #60691, #43199 ) ) ;
#15482 = CARTESIAN_POINT ( 'NONE',  ( -120.6549999999999869, -7.632228543268600340, -2.479861379858950166 ) ) ;
#15483 = ORIENTED_EDGE ( 'NONE', *, *, #38592, .F. ) ;
#15484 = DIRECTION ( 'NONE',  ( 1.000000000000000000, 1.453863484628180989E-14, 0.000000000000000000 ) ) ;
#15485 = CARTESIAN_POINT ( 'NONE',  ( -105.2070736234671386, 3.094860106634298447, 9.524999999988466470 ) ) ;
#15486 = ORIENTED_EDGE ( 'NONE', *, *, #14299, .T. ) ;
#15487 = SURFACE_STYLE_FILL_AREA ( #63305 ) ;
#15488 = ORIENTED_EDGE ( 'NONE', *, *, #31834, .T. ) ;
#15489 = CARTESIAN_POINT ( 'NONE',  ( 9.985360875542987458, 1.514639124457112018, 0.7048476316490990268 ) ) ;
#15490 = CARTESIAN_POINT ( 'NONE',  ( -9.058813317711338797, 152.3449999999999704, 2.943386871421373563 ) ) ;
#15491 = DIRECTION ( 'NONE',  ( 0.000000000000000000, 0.000000000000000000, -1.000000000000000000 ) ) ;
#15492 = EDGE_CURVE ( 'NONE', #29106, #12316, #4501, .T. ) ;
#15493 = ORIENTED_EDGE ( 'NONE', *, *, #57446, .F. ) ;
#15494 = CARTESIAN_POINT ( 'NONE',  ( -54.80707362346617373, 10.01517768586948698, -1.839758294383808966E-15 ) ) ;
#15495 = CARTESIAN_POINT ( 'NONE',  ( -3.094860106618432471, 152.7049999999999841, -9.525000000000000355 ) ) ;
#15496 = CARTESIAN_POINT ( 'NONE',  ( -135.3570736234661638, 5.598654528085804216, 7.705886871421366635 ) ) ;
#15497 = VECTOR ( 'NONE', #45984, 1000.000000000000000 ) ;
#15498 = CARTESIAN_POINT ( 'NONE',  ( 0.000000000000000000, 0.000000000000000000, 0.000000000000000000 ) ) ;
#15499 = ORIENTED_EDGE ( 'NONE', *, *, #31477, .T. ) ;
#15500 = CARTESIAN_POINT ( 'NONE',  ( -7.632228543268608334, 126.8429263765338249, 2.479861379858952830 ) ) ;
#15501 = CIRCLE ( 'NONE', #38053, 3.000000000000000444 ) ;
#15502 = VECTOR ( 'NONE', #69556, 1000.000000000000000 ) ;
#15503 = DIRECTION ( 'NONE',  ( 0.000000000000000000, 0.000000000000000000, -1.000000000000000000 ) ) ;
#15504 =( NAMED_UNIT ( * ) PLANE_ANGLE_UNIT ( ) SI_UNIT ( $, .RADIAN. ) );
#15505 = ORIENTED_EDGE ( 'NONE', *, *, #32174, .F. ) ;
#15506 = CARTESIAN_POINT ( 'NONE',  ( -41.26944598842810308, 107.7917661767790776, -3.849001801206922480 ) ) ;
#15507 = EDGE_LOOP ( 'NONE', ( #48796, #61931 ) ) ;
#15508 = CARTESIAN_POINT ( 'NONE',  ( -60.74292637653380922, -5.598654528085803328, -7.705886871421366635 ) ) ;
#15509 = DIRECTION ( 'NONE',  ( 1.000000000000000000, 0.000000000000000000, 0.000000000000000000 ) ) ;
#15510 = CARTESIAN_POINT ( 'NONE',  ( -6.767634268437469736, 2.278113600022081631, 0.1324414877861203599 ) ) ;
#15511 = STYLED_ITEM ( 'NONE', ( #43848 ), #14160 ) ;
#15512 = CARTESIAN_POINT ( 'NONE',  ( -150.8050000000000068, -8.437984349512085203, 5.166775262442717831E-16 ) ) ;
#15513 = CARTESIAN_POINT ( 'NONE',  ( 17.75000000000000711, 31.24999999999999289, -3.750000000000000000 ) ) ;
#15514 = EDGE_CURVE ( 'NONE', #65971, #40883, #1697, .T. ) ;
#15515 = CARTESIAN_POINT ( 'NONE',  ( 66.74999999999998579, 36.75000000000000000, 4.000000000000000000 ) ) ;
#15516 = CARTESIAN_POINT ( 'NONE',  ( 28.00000000000002842, 43.00000000000000000, 0.000000000000000000 ) ) ;
#15517 = LINE ( 'NONE', #57718, #50013 ) ;
#15518 = ORIENTED_EDGE ( 'NONE', *, *, #66650, .T. ) ;
#15519 = PRESENTATION_LAYER_ASSIGNMENT (  '', '', ( #21059 ) ) ;
#15520 = VERTEX_POINT ( 'NONE', #2015 ) ;
#15521 = CARTESIAN_POINT ( 'NONE',  ( 22.83826606206589815, 27.22759712782712072, 27.27819404924646207 ) ) ;
#15522 = PRESENTATION_LAYER_ASSIGNMENT (  '', '', ( #64927 ) ) ;
#15523 = ADVANCED_FACE ( 'NONE', ( #28102 ), #65062, .F. ) ;
#15524 = CARTESIAN_POINT ( 'NONE',  ( -69.65499999999998693, -7.632228543268600340, -2.479861379858950166 ) ) ;
#15525 = ORIENTED_EDGE ( 'NONE', *, *, #43877, .F. ) ;
#15526 = PRESENTATION_STYLE_ASSIGNMENT (( #10914 ) ) ;
#15527 = ADVANCED_FACE ( 'NONE', ( #19297 ), #7885, .T. ) ;
#15528 = FACE_OUTER_BOUND ( 'NONE', #33584, .T. ) ;
#15529 = DIRECTION ( 'NONE',  ( -0.000000000000000000, -1.000000000000000000, -0.000000000000000000 ) ) ;
#15530 = CARTESIAN_POINT ( 'NONE',  ( -123.8929263765337936, -8.102448949553174629, -5.886773742842741797 ) ) ;
#15531 = CARTESIAN_POINT ( 'NONE',  ( -15.75000000000000000, -3.000000000000000000, 20.00000000000000000 ) ) ;
#15532 = EDGE_LOOP ( 'NONE', ( #39311, #61967, #24964, #59818 ) ) ;
#15533 = EDGE_CURVE ( 'NONE', #15954, #42614, #67157, .T. ) ;
#15534 = LINE ( 'NONE', #38035, #12160 ) ;
#15535 = DIRECTION ( 'NONE',  ( -0.000000000000000000, -0.000000000000000000, 1.000000000000000000 ) ) ;
#15537 =( NAMED_UNIT ( * ) SI_UNIT ( $, .STERADIAN. ) SOLID_ANGLE_UNIT ( ) );
#15536 = DIRECTION ( 'NONE',  ( 0.000000000000000000, 1.000000000000000000, 0.000000000000000000 ) ) ;
#15538 = EDGE_CURVE ( 'NONE', #2689, #29106, #29518, .T. ) ;
#15539 = CARTESIAN_POINT ( 'NONE',  ( -114.5949999999999704, 2.607480562269072433, 8.024999999999991473 ) ) ;
#15540 = CARTESIAN_POINT ( 'NONE',  ( 9.058813317711337021, 150.5449999999999875, 2.943386871421375783 ) ) ;
#15541 = CARTESIAN_POINT ( 'NONE',  ( -85.19500000000000739, 8.437984349512085203, -1.550032578732815448E-15 ) ) ;
#15542 = DIRECTION ( 'NONE',  ( -0.000000000000000000, -0.000000000000000000, -1.000000000000000000 ) ) ;
#15543 = DIRECTION ( 'NONE',  ( 0.000000000000000000, 0.000000000000000000, 1.000000000000000000 ) ) ;
#15544 = PRESENTATION_STYLE_ASSIGNMENT (( #22183 ) ) ;
#15545 = ORIENTED_EDGE ( 'NONE', *, *, #67762, .T. ) ;
#15546 = CARTESIAN_POINT ( 'NONE',  ( -134.5429263765338135, 9.058813317711329915, 2.943386871421369566 ) ) ;
#15547 = DIRECTION ( 'NONE',  ( -1.000000000000000000, -0.000000000000000000, -0.000000000000000000 ) ) ;
#15548 = CARTESIAN_POINT ( 'NONE',  ( -157.3449999999999989, 7.632228543268599452, -2.479861379858951942 ) ) ;
#15549 = CARTESIAN_POINT ( 'NONE',  ( -0.3545099074454313715, 7.000000000000007994, -2.047617446692545640E-14 ) ) ;
#15550 = COLOUR_RGB ( '', 0.08235294, 0.09019608, 0.10196078) ;
#15551 = VECTOR ( 'NONE', #36482, 1000.000000000000000 ) ;
#15552 = EDGE_CURVE ( 'NONE', #24087, #57942, #24927, .T. ) ;
#15553 = DIRECTION ( 'NONE',  ( -0.000000000000000000, -0.000000000000000000, 1.000000000000000000 ) ) ;
#15554 =( NAMED_UNIT ( * ) PLANE_ANGLE_UNIT ( ) SI_UNIT ( $, .RADIAN. ) );
#15555 = ORIENTED_EDGE ( 'NONE', *, *, #63233, .F. ) ;
#15556 =( GEOMETRIC_REPRESENTATION_CONTEXT ( 3 ) GLOBAL_UNCERTAINTY_ASSIGNED_CONTEXT ( ( #32005 ) ) GLOBAL_UNIT_ASSIGNED_CONTEXT ( ( #11715, #43765, #59897 ) ) REPRESENTATION_CONTEXT ( 'NONE', 'WORKASPACE' ) );
#15557 = EDGE_LOOP ( 'NONE', ( #15473, #51617, #14468, #47987 ) ) ;
#15558 = ADVANCED_FACE ( 'NONE', ( #2745 ), #51329, .F. ) ;
#15559 = CARTESIAN_POINT ( 'NONE',  ( 12.75000000000000533, 27.74999999999998224, -4.000000000000000000 ) ) ;
#15560 = CARTESIAN_POINT ( 'NONE',  ( 72.50000000000000000, 13.41640786499872284, 10.00000000000000000 ) ) ;
#15561 = CARTESIAN_POINT ( 'NONE',  ( -45.00000000000000000, 9.708372671849131663, 6.049000248776977173 ) ) ;
#15562 = CARTESIAN_POINT ( 'NONE',  ( 57.00000000000000000, 0.000000000000000000, -65.00402776293825013 ) ) ;
#15563 = VECTOR ( 'NONE', #55299, 1000.000000000000000 ) ;
#15564 = FILL_AREA_STYLE_COLOUR ( '', #13955 ) ;
#15565 = ORIENTED_EDGE ( 'NONE', *, *, #36629, .T. ) ;
#15566 = CARTESIAN_POINT ( 'NONE',  ( -155.3050000000000068, 8.437984349512086979, -1.550032578732815448E-15 ) ) ;
#15567 = ORIENTED_EDGE ( 'NONE', *, *, #40619, .F. ) ;
#15568 = DIRECTION ( 'NONE',  ( -0.000000000000000000, -0.000000000000000000, -1.000000000000000000 ) ) ;
#15569 =( NAMED_UNIT ( * ) SI_UNIT ( $, .STERADIAN. ) SOLID_ANGLE_UNIT ( ) );
#15570 = ORIENTED_EDGE ( 'NONE', *, *, #25115, .F. ) ;
#15571 = CARTESIAN_POINT ( 'NONE',  ( 10.01517768586949231, 120.6949999999999790, 1.839758294383810543E-15 ) ) ;
#15572 = SURFACE_SIDE_STYLE ('',( #42669 ) ) ;
#15573 = VERTEX_POINT ( 'NONE', #19659 ) ;
#15574 = CARTESIAN_POINT ( 'NONE',  ( 9.058813317711338797, 118.9549999999999983, -2.943386871421372675 ) ) ;
#15575 = CARTESIAN_POINT ( 'NONE',  ( -64.85499999999997556, 4.716976649647094177, 6.492361379858945902 ) ) ;
#15576 = STYLED_ITEM ( 'NONE', ( #63689 ), #43323 ) ;
#15577 = CARTESIAN_POINT ( 'NONE',  ( -1.000000000000028644, 0.000000000000000000, 0.000000000000000000 ) ) ;
#15578 = ORIENTED_EDGE ( 'NONE', *, *, #18202, .F. ) ;
#15579 = CARTESIAN_POINT ( 'NONE',  ( 10.01517768586949231, 151.8049999999999784, 1.839758294383810543E-15 ) ) ;
#15580 = COLOUR_RGB ( '', 0.09019608, 0.27058824, 0.51372549) ;
#15581 = CARTESIAN_POINT ( 'NONE',  ( 0.000000000000000000, 0.000000000000000000, -10.00000000000000000 ) ) ;
#15582 = CARTESIAN_POINT ( 'NONE',  ( 24.21231517720798010, 113.4999999999999858, -9.500000000000000000 ) ) ;
#15583 = ADVANCED_FACE ( 'NONE', ( #9121 ), #67497, .T. ) ;
#15584 = DIRECTION ( 'NONE',  ( 0.000000000000000000, 0.000000000000000000, -1.000000000000000000 ) ) ;
#15585 = ORIENTED_EDGE ( 'NONE', *, *, #52304, .F. ) ;
#15586 = COLOUR_RGB ( '', 0.40784314, 0.44705882, 0.49803922) ;
#15587 = FACE_OUTER_BOUND ( 'NONE', #38878, .T. ) ;
#15588 = CARTESIAN_POINT ( 'NONE',  ( -46.40707362346616094, 3.094860106618428031, -9.524999999999993250 ) ) ;
#15589 = CARTESIAN_POINT ( 'NONE',  ( -48.14499999999999602, -4.716976649647092401, 6.492361379858946790 ) ) ;
#15590 = EDGE_LOOP ( 'NONE', ( #33807, #53507, #22157, #25982 ) ) ;
#15591 = CARTESIAN_POINT ( 'NONE',  ( 31.64575758289396745, 42.77450929379339328, 45.47201693779177134 ) ) ;
#15592 = VECTOR ( 'NONE', #39644, 1000.000000000000000 ) ;
#15593 = DIRECTION ( 'NONE',  ( -0.7292845505553197105, 0.6842105263157864936, -0.000000000000000000 ) ) ;
#15594 = EDGE_CURVE ( 'NONE', #65484, #5088, #14372, .T. ) ;
#15595 =( LENGTH_UNIT ( ) NAMED_UNIT ( * ) SI_UNIT ( .MILLI., .METRE. ) );
#15596 = ORIENTED_EDGE ( 'NONE', *, *, #16246, .T. ) ;
#15597 = FACE_OUTER_BOUND ( 'NONE', #33023, .T. ) ;
#15598 = ORIENTED_EDGE ( 'NONE', *, *, #62081, .T. ) ;
#15599 = COLOUR_RGB ( '', 0.40784314, 0.44705882, 0.49803922) ;
#15600 = CIRCLE ( 'NONE', #63864, 1.000000000000001998 ) ;
#15601 = SURFACE_STYLE_FILL_AREA ( #43056 ) ;
#15603 = ADVANCED_FACE ( 'NONE', ( #45404 ), #63758, .F. ) ;
#15602 =( LENGTH_UNIT ( ) NAMED_UNIT ( * ) SI_UNIT ( .MILLI., .METRE. ) );
#15604 = CARTESIAN_POINT ( 'NONE',  ( -93.05499999999997840, -9.827790563157499189E-16, -8.024999999999991473 ) ) ;
#15605 = ORIENTED_EDGE ( 'NONE', *, *, #13511, .T. ) ;
#15606 = DIRECTION ( 'NONE',  ( 0.000000000000000000, 0.000000000000000000, 1.000000000000000000 ) ) ;
#15607 = FILL_AREA_STYLE_COLOUR ( '', #7772 ) ;
#15608 = CIRCLE ( 'NONE', #23446, 16.00000000000000000 ) ;
#15609 = CARTESIAN_POINT ( 'NONE',  ( -131.4570736234661865, -9.058813317711329915, 2.943386871421371787 ) ) ;
#15610 = FILL_AREA_STYLE_COLOUR ( '', #33932 ) ;
#15611 = CARTESIAN_POINT ( 'NONE',  ( 8.102448949553179958, 147.3950000000000102, 5.886773742842750679 ) ) ;
#15612 = CARTESIAN_POINT ( 'NONE',  ( -62.75707362346616236, -5.598654528085801552, 7.705886871421367523 ) ) ;
#15613 = VECTOR ( 'NONE', #55439, 1000.000000000000000 ) ;
#15614 = CARTESIAN_POINT ( 'NONE',  ( -37.75000000000000000, 0.000000000000000000, -6.999999999999999112 ) ) ;
#15615 = VERTEX_POINT ( 'NONE', #16146 ) ;
#15616 = CARTESIAN_POINT ( 'NONE',  ( -184.0000000000000000, 0.000000000000000000, 0.000000000000000000 ) ) ;
#15617 = MECHANICAL_DESIGN_GEOMETRIC_PRESENTATION_REPRESENTATION (  '', ( #20038 ), #21148 ) ;
#15618 = DIRECTION ( 'NONE',  ( 0.000000000000000000, -0.000000000000000000, -1.000000000000000000 ) ) ;
#15619 = ADVANCED_FACE ( 'NONE', ( #52725 ), #53736, .F. ) ;
#15620 = CARTESIAN_POINT ( 'NONE',  ( -109.7049999999999699, 2.607480562269073321, 8.024999999999991473 ) ) ;
#15621 = CARTESIAN_POINT ( 'NONE',  ( 8.102448949553181734, 120.3949999999999960, 5.886773742842750679 ) ) ;
#15622 = CARTESIAN_POINT ( 'NONE',  ( -123.5949999999999704, 2.607480562269073321, 8.024999999999991473 ) ) ;
#15623 =( NAMED_UNIT ( * ) SI_UNIT ( $, .STERADIAN. ) SOLID_ANGLE_UNIT ( ) );
#15624 = CARTESIAN_POINT ( 'NONE',  ( -118.0429263765338135, -9.058813317711329915, -2.943386871421370898 ) ) ;
#15625 = EDGE_LOOP ( 'NONE', ( #58553, #59462, #30679, #68358 ) ) ;
#15626 = STYLED_ITEM ( 'NONE', ( #30533 ), #43534 ) ;
#15627 = CARTESIAN_POINT ( 'NONE',  ( -161.6929263765337907, 10.01517768586948698, -1.839758294383808571E-15 ) ) ;
#15628 = CARTESIAN_POINT ( 'NONE',  ( 1.000000000000000000, 42.00000000000000000, -79.00402776293826435 ) ) ;
#15629 = COLOUR_RGB ( '', 0.40784314, 0.44705882, 0.49803922) ;
#15630 = STYLED_ITEM ( 'NONE', ( #64332 ), #10190 ) ;
#15631 = CARTESIAN_POINT ( 'NONE',  ( -20.86663389611626229, 115.0293260623345475, -10.00000000000000000 ) ) ;
#15632 = PRESENTATION_STYLE_ASSIGNMENT (( #53265 ) ) ;
#15633 = FACE_OUTER_BOUND ( 'NONE', #50494, .T. ) ;
#15634 = VERTEX_POINT ( 'NONE', #60058 ) ;
#15635 = CARTESIAN_POINT ( 'NONE',  ( -77.39292637653380780, 8.102448949553176405, 5.886773742842740909 ) ) ;
#15636 = MECHANICAL_DESIGN_GEOMETRIC_PRESENTATION_REPRESENTATION (  '', ( #17868 ), #54904 ) ;
#15637 = CARTESIAN_POINT ( 'NONE',  ( 31.00000000000001421, 14.00000000000000000, 36.49999999999999289 ) ) ;
#15638 =( LENGTH_UNIT ( ) NAMED_UNIT ( * ) SI_UNIT ( .MILLI., .METRE. ) );
#15639 = SURFACE_STYLE_FILL_AREA ( #46984 ) ;
#15640 = SURFACE_STYLE_USAGE ( .BOTH. , #26504 ) ;
#15641 = DIRECTION ( 'NONE',  ( 0.7681514953298232973, -6.664128951862614066E-15, 0.6402681315062906942 ) ) ;
#15642 = MECHANICAL_DESIGN_GEOMETRIC_PRESENTATION_REPRESENTATION (  '', ( #35804 ), #6595 ) ;
#15643 = AXIS2_PLACEMENT_3D ( 'NONE', #24, #21559, #32809 ) ;
#15644 = CARTESIAN_POINT ( 'NONE',  ( -180.9550000000000125, -7.632228543268599452, 2.479861379858951054 ) ) ;
#15645 = ORIENTED_EDGE ( 'NONE', *, *, #24463, .T. ) ;
#15646 = SURFACE_SIDE_STYLE ('',( #63799 ) ) ;
#15647 = DIRECTION ( 'NONE',  ( 0.000000000000000000, -0.000000000000000000, -1.000000000000000000 ) ) ;
#15648 =( LENGTH_UNIT ( ) NAMED_UNIT ( * ) SI_UNIT ( .MILLI., .METRE. ) );
#15649 = STYLED_ITEM ( 'NONE', ( #42720 ), #14985 ) ;
#15650 = CARTESIAN_POINT ( 'NONE',  ( 6.826472737025121695, 147.6070736234661638, -4.959722759717905660 ) ) ;
#15651 = ORIENTED_EDGE ( 'NONE', *, *, #44930, .F. ) ;
#15652 = DIRECTION ( 'NONE',  ( 1.000000000000000000, 0.000000000000000000, 0.000000000000000000 ) ) ;
#15653 = CARTESIAN_POINT ( 'NONE',  ( -96.50499999999998124, -6.826472737025113702, -4.959722759717900331 ) ) ;
#15654 = VECTOR ( 'NONE', #1241, 1000.000000000000000 ) ;
#15655 = FILL_AREA_STYLE_COLOUR ( '', #62283 ) ;
#15656 = ORIENTED_EDGE ( 'NONE', *, *, #55417, .F. ) ;
#15657 = CARTESIAN_POINT ( 'NONE',  ( -39.44036755984751608, -13.33477445990380517, 0.9440656176847447290 ) ) ;
#15658 = FILL_AREA_STYLE_COLOUR ( '', #26022 ) ;
#15659 = EDGE_CURVE ( 'NONE', #15190, #10730, #11255, .T. ) ;
#15660 = VERTEX_POINT ( 'NONE', #55476 ) ;
#15661 = FACE_OUTER_BOUND ( 'NONE', #28640, .T. ) ;
#15662 = CARTESIAN_POINT ( 'NONE',  ( -74.09499999999998465, -2.607480562269071545, -8.024999999999991473 ) ) ;
#15663 = ORIENTED_EDGE ( 'NONE', *, *, #2904, .F. ) ;
#15664 = CARTESIAN_POINT ( 'NONE',  ( -23.21231517720798010, 117.4999999999999716, -10.00000000000000000 ) ) ;
#15665 =( NAMED_UNIT ( * ) SI_UNIT ( $, .STERADIAN. ) SOLID_ANGLE_UNIT ( ) );
#15666 = VERTEX_POINT ( 'NONE', #1937 ) ;
#15667 = FACE_OUTER_BOUND ( 'NONE', #1655, .T. ) ;
#15668 = FACE_OUTER_BOUND ( 'NONE', #59740, .T. ) ;
#15669 =( GEOMETRIC_REPRESENTATION_CONTEXT ( 3 ) GLOBAL_UNCERTAINTY_ASSIGNED_CONTEXT ( ( #36968 ) ) GLOBAL_UNIT_ASSIGNED_CONTEXT ( ( #43826, #64555, #38559 ) ) REPRESENTATION_CONTEXT ( 'NONE', 'WORKASPACE' ) );
#15671 = ADVANCED_FACE ( 'NONE', ( #28014 ), #22087, .T. ) ;
#15670 = LINE ( 'NONE', #58920, #16672 ) ;
#15672 = ORIENTED_EDGE ( 'NONE', *, *, #13731, .T. ) ;
#15673 = SURFACE_STYLE_FILL_AREA ( #52621 ) ;
#15674 = ADVANCED_FACE ( 'NONE', ( #16501 ), #49525, .T. ) ;
#15675 = ORIENTED_EDGE ( 'NONE', *, *, #46595, .T. ) ;
#15676 = COLOUR_RGB ( '', 0.31764706, 0.68627451, 0.89019608) ;
#15677 = SURFACE_STYLE_FILL_AREA ( #63832 ) ;
#15678 = CARTESIAN_POINT ( 'NONE',  ( -40.78947368421051323, 108.1536491499103505, 3.000000000000000000 ) ) ;
#15679 = CARTESIAN_POINT ( 'NONE',  ( -156.2070736234661581, 3.094860106618433360, 9.524999999999991473 ) ) ;
#15680 = EDGE_CURVE ( 'NONE', #18052, #61901, #885, .T. ) ;
#15681 =( GEOMETRIC_REPRESENTATION_CONTEXT ( 3 ) GLOBAL_UNCERTAINTY_ASSIGNED_CONTEXT ( ( #17326 ) ) GLOBAL_UNIT_ASSIGNED_CONTEXT ( ( #67704, #19499, #36435 ) ) REPRESENTATION_CONTEXT ( 'NONE', 'WORKASPACE' ) );
#15682 = CARTESIAN_POINT ( 'NONE',  ( -1.166476076187854022E-15, 119.9449999999999790, 9.525000000000000355 ) ) ;
#15683 = CARTESIAN_POINT ( 'NONE',  ( -101.3070736234661950, -10.01517768586948698, 6.132527647946031529E-16 ) ) ;
#15684 = CIRCLE ( 'NONE', #21266, 4.999999999999997335 ) ;
#15685 = EDGE_CURVE ( 'NONE', #61874, #14945, #17851, .T. ) ;
#15686 = DIRECTION ( 'NONE',  ( 0.000000000000000000, 0.000000000000000000, -1.000000000000000000 ) ) ;
#15687 = ORIENTED_EDGE ( 'NONE', *, *, #59147, .F. ) ;
#15688 = SURFACE_STYLE_USAGE ( .BOTH. , #65234 ) ;
#15689 = CARTESIAN_POINT ( 'NONE',  ( 0.000000000000000000, 2.299999999999999822, 0.000000000000000000 ) ) ;
#15690 = DIRECTION ( 'NONE',  ( 0.000000000000000000, -1.000000000000000000, 0.000000000000000000 ) ) ;
#15691 = EDGE_CURVE ( 'NONE', #2615, #53207, #41672, .T. ) ;
#15692 = CARTESIAN_POINT ( 'NONE',  ( -138.5049999999999955, -6.826472737025115478, -4.959722759717899443 ) ) ;
#15693 = PLANE ( 'NONE',  #18447 ) ;
#15694 = CARTESIAN_POINT ( 'NONE',  ( -158.0949999999999704, -2.607480562269071545, -8.024999999999991473 ) ) ;
#15695 = PRESENTATION_LAYER_ASSIGNMENT (  '', '', ( #4396 ) ) ;
#15696 = CARTESIAN_POINT ( 'NONE',  ( -142.7949999999999875, 2.607480562269069324, -8.024999999999993250 ) ) ;
#15697 = ORIENTED_EDGE ( 'NONE', *, *, #7213, .T. ) ;
#15698 = CIRCLE ( 'NONE', #48356, 1.000000000000001110 ) ;
#15699 = CARTESIAN_POINT ( 'NONE',  ( 59.00000000000000000, 11.99999999999999822, -3.499999999999999556 ) ) ;
#15700 = FACE_OUTER_BOUND ( 'NONE', #7653, .T. ) ;
#15701 = FILL_AREA_STYLE_COLOUR ( '', #2301 ) ;
#15702 = UNCERTAINTY_MEASURE_WITH_UNIT (LENGTH_MEASURE( 1.000000000000000082E-05 ), #60862, 'distance_accuracy_value', 'NONE');
#15703 = CARTESIAN_POINT ( 'NONE',  ( -49.55499999999998550, 0.000000000000000000, 8.024999999999991473 ) ) ;
#15704 =( NAMED_UNIT ( * ) SI_UNIT ( $, .STERADIAN. ) SOLID_ANGLE_UNIT ( ) );
#15705 = CIRCLE ( 'NONE', #7793, 0.5000000000000004441 ) ;
#15706 = DIRECTION ( 'NONE',  ( 0.000000000000000000, 0.000000000000000000, 1.000000000000000000 ) ) ;
#15707 = CARTESIAN_POINT ( 'NONE',  ( 3.000000000000030198, 34.80256050929376954, 80.00402776293826435 ) ) ;
#15708 = CARTESIAN_POINT ( 'NONE',  ( -49.12162162162162105, 13.70805908423323594, 9.500000000000000000 ) ) ;
#15709 = PLANE ( 'NONE',  #3065 ) ;
#15710 = AXIS2_PLACEMENT_3D ( 'NONE', #57525, #31116, #4366 ) ;
#15711 = CIRCLE ( 'NONE', #54979, 30.00000000000000000 ) ;
#15712 = UNCERTAINTY_MEASURE_WITH_UNIT (LENGTH_MEASURE( 1.000000000000000082E-05 ), #60246, 'distance_accuracy_value', 'NONE');
#15713 =( BOUNDED_CURVE ( )  B_SPLINE_CURVE ( 2, ( #35944, #57392, #25030, #20081, #45822, #30634, #52142, #3897, #3168, #25373, #8525 ),
 .UNSPECIFIED., .F., .F. ) 
 B_SPLINE_CURVE_WITH_KNOTS ( ( 3, 2, 2, 2, 2, 3 ),
 ( 0.8152173913043477826, 0.8173913043478261420, 0.8195652173913043903, 0.8217391304347826386, 0.8239130434782608869, 0.8260869565217391353 ),
 .UNSPECIFIED. ) 
 CURVE ( )  GEOMETRIC_REPRESENTATION_ITEM ( )  RATIONAL_B_SPLINE_CURVE ( ( 1.000000000000000000, 0.9510565162951535312, 1.000000000000000000, 0.9510565162951535312, 1.000000000000000000, 0.9510565162951535312, 1.000000000000000000, 0.9510565162951535312, 1.000000000000000000, 0.9510565162951535312, 1.000000000000000000 ) ) 
 REPRESENTATION_ITEM ( '' )  );
#15714 = DIRECTION ( 'NONE',  ( 1.110223024625156540E-16, -0.1585527532634883607, 0.9873505073845698643 ) ) ;
#15715 = CYLINDRICAL_SURFACE ( 'NONE', #20341, 0.2500000000000002220 ) ;
#15716 = COLOUR_RGB ( '', 0.09019608, 0.27058824, 0.51372549) ;
#15717 = LINE ( 'NONE', #4415, #56075 ) ;
#15718 = TOROIDAL_SURFACE ( 'NONE', #68477, 12.50000000000000000, 0.5000000000000000000 ) ;
#15719 = DIRECTION ( 'NONE',  ( 0.000000000000000000, 0.000000000000000000, -1.000000000000000000 ) ) ;
#15720 = FILL_AREA_STYLE_COLOUR ( '', #65581 ) ;
#15721 = COLOUR_RGB ( '', 0.08235294, 0.09019608, 0.10196078) ;
#15722 = DIRECTION ( 'NONE',  ( 1.000000000000000000, 0.000000000000000000, 0.000000000000000000 ) ) ;
#15723 = DIRECTION ( 'NONE',  ( 0.000000000000000000, 1.000000000000000000, -0.000000000000000000 ) ) ;
#15724 = VERTEX_POINT ( 'NONE', #7298 ) ;
#15725 = CIRCLE ( 'NONE', #30288, 9.500000000000005329 ) ;
#15726 = CARTESIAN_POINT ( 'NONE',  ( -4.716976649647098618, 116.2570736234661553, 6.492361379858953008 ) ) ;
#15728 = CARTESIAN_POINT ( 'NONE',  ( -195.0000000000000000, 0.000000000000000000, 9.524999999999991473 ) ) ;
#15727 = AXIS2_PLACEMENT_3D ( 'NONE', #51474, #3231, #31050 ) ;
#15729 = DIRECTION ( 'NONE',  ( 0.000000000000000000, 0.000000000000000000, -1.000000000000000000 ) ) ;
#15730 = FILL_AREA_STYLE_COLOUR ( '', #43207 ) ;
#15731 = ORIENTED_EDGE ( 'NONE', *, *, #57437, .F. ) ;
#15732 = ORIENTED_EDGE ( 'NONE', *, *, #14553, .F. ) ;
#15733 = DIRECTION ( 'NONE',  ( 0.000000000000000000, -0.000000000000000000, 1.000000000000000000 ) ) ;
#15734 = PRESENTATION_STYLE_ASSIGNMENT (( #20290 ) ) ;
#15735 = CARTESIAN_POINT ( 'NONE',  ( 30.50000000000000711, 18.74999999999997868, 4.000000000000000000 ) ) ;
#15736 = ORIENTED_EDGE ( 'NONE', *, *, #18413, .F. ) ;
#15737 = CARTESIAN_POINT ( 'NONE',  ( 9.058813317711338797, 115.9549999999999841, -2.943386871421372675 ) ) ;
#15738 = CARTESIAN_POINT ( 'NONE',  ( -71.62068965517238439, 63.58603185604027885, -7.500000000000000000 ) ) ;
#15739 = EDGE_CURVE ( 'NONE', #1324, #8679, #43587, .T. ) ;
#15740 = MECHANICAL_DESIGN_GEOMETRIC_PRESENTATION_REPRESENTATION (  '', ( #67388 ), #39304 ) ;
#15741 = CARTESIAN_POINT ( 'NONE',  ( -44.99999999999977973, 149.4999999999999716, -9.500000000000000000 ) ) ;
#15742 = CARTESIAN_POINT ( 'NONE',  ( -104.9949999999999761, -6.826472737025115478, 4.959722759717900331 ) ) ;
#15743 = ORIENTED_EDGE ( 'NONE', *, *, #35707, .F. ) ;
#15744 = MECHANICAL_DESIGN_GEOMETRIC_PRESENTATION_REPRESENTATION (  '', ( #31420 ), #3321 ) ;
#15745 = EDGE_CURVE ( 'NONE', #23974, #67099, #18028, .T. ) ;
#15746 = STYLED_ITEM ( 'NONE', ( #47231 ), #47271 ) ;
#15747 = CARTESIAN_POINT ( 'NONE',  ( 0.000000000000000000, 0.000000000000000000, -10.00000000000000000 ) ) ;
#15748 =( NAMED_UNIT ( * ) SI_UNIT ( $, .STERADIAN. ) SOLID_ANGLE_UNIT ( ) );
#15749 = CARTESIAN_POINT ( 'NONE',  ( 15.48999599679679662, 146.4999999999999716, -7.500000000000000000 ) ) ;
#15750 = ORIENTED_EDGE ( 'NONE', *, *, #18874, .T. ) ;
#15751 = CARTESIAN_POINT ( 'NONE',  ( -7.632228543268608334, 156.8429263765338249, 2.479861379858952830 ) ) ;
#15752 = FACE_OUTER_BOUND ( 'NONE', #47030, .T. ) ;
#15753 = AXIS2_PLACEMENT_3D ( 'NONE', #65776, #39077, #7024 ) ;
#15754 = ADVANCED_FACE ( 'NONE', ( #59344 ), #48863, .T. ) ;
#15755 = CARTESIAN_POINT ( 'NONE',  ( -195.0000000000000000, 0.000000000000000000, 0.000000000000000000 ) ) ;
#15756 =( NAMED_UNIT ( * ) SI_UNIT ( $, .STERADIAN. ) SOLID_ANGLE_UNIT ( ) );
#15757 = LINE ( 'NONE', #58994, #1482 ) ;
#15758 = EDGE_CURVE ( 'NONE', #58413, #18810, #18188, .T. ) ;
#15759 = EDGE_LOOP ( 'NONE', ( #29082, #64326, #15525, #56317 ) ) ;
#15760 = SURFACE_STYLE_FILL_AREA ( #38625 ) ;
#15761 = LINE ( 'NONE', #5168, #53760 ) ;
#15762 = DIRECTION ( 'NONE',  ( 1.000000000000000000, 0.000000000000000000, 0.000000000000000000 ) ) ;
#15763 = CARTESIAN_POINT ( 'NONE',  ( -195.0000000000000000, 0.000000000000000000, 0.000000000000000000 ) ) ;
#15764 = DIRECTION ( 'NONE',  ( -1.000000000000000000, 0.000000000000000000, 0.000000000000000000 ) ) ;
#15765 = AXIS2_PLACEMENT_3D ( 'NONE', #55174, #12615, #61481 ) ;
#15766 = DIRECTION ( 'NONE',  ( -1.000000000000000000, 0.000000000000000000, 0.000000000000000000 ) ) ;
#15767 = CARTESIAN_POINT ( 'NONE',  ( -125.3929263765338220, 8.102448949553176405, 5.886773742842740909 ) ) ;
#15768 = EDGE_CURVE ( 'NONE', #38442, #58700, #41065, .T. ) ;
#15769 = LINE ( 'NONE', #43228, #9209 ) ;
#15770 = CARTESIAN_POINT ( 'NONE',  ( -9.827790563157511022E-16, 115.4429263765338192, 8.025000000000000355 ) ) ;
#15771 = FACE_OUTER_BOUND ( 'NONE', #44586, .T. ) ;
#15772 = ORIENTED_EDGE ( 'NONE', *, *, #43959, .T. ) ;
#15773 = ORIENTED_EDGE ( 'NONE', *, *, #8836, .T. ) ;
#15774 = FACE_OUTER_BOUND ( 'NONE', #24902, .T. ) ;
#15775 = PRESENTATION_STYLE_ASSIGNMENT (( #19639 ) ) ;
#15776 = ORIENTED_EDGE ( 'NONE', *, *, #35675, .F. ) ;
#15777 = CARTESIAN_POINT ( 'NONE',  ( -174.0549999999999784, -9.827790563157499189E-16, -8.024999999999991473 ) ) ;
#15778 = CARTESIAN_POINT ( 'NONE',  ( -48.50000000000000000, 14.49137674618942562, 7.000000000000000000 ) ) ;
#15779 = DIRECTION ( 'NONE',  ( 1.000000000000000000, 0.000000000000000000, 0.000000000000000000 ) ) ;
#15780 = CARTESIAN_POINT ( 'NONE',  ( -47.60707362346616378, -8.102448949553172852, 5.886773742842742685 ) ) ;
#15781 = CARTESIAN_POINT ( 'NONE',  ( -165.7450000000000045, 4.716976649647094177, 6.492361379858945902 ) ) ;
#15782 = COLOUR_RGB ( '', 0.31764706, 0.68627451, 0.89019608) ;
#15783 = ORIENTED_EDGE ( 'NONE', *, *, #38759, .T. ) ;
#15784 =( LENGTH_UNIT ( ) NAMED_UNIT ( * ) SI_UNIT ( .MILLI., .METRE. ) );
#15785 = DIRECTION ( 'NONE',  ( 0.000000000000000000, 0.000000000000000000, 1.000000000000000000 ) ) ;
#15786 = CIRCLE ( 'NONE', #47243, 0.7499999999999997780 ) ;
#15787 = CARTESIAN_POINT ( 'NONE',  ( -11.94747633183538937, 11.32477212104151221, 3.973188058064621497 ) ) ;
#15788 = CARTESIAN_POINT ( 'NONE',  ( -78.80500000000000682, -8.437984349512085203, 5.166775262442717831E-16 ) ) ;
#15789 = DIRECTION ( 'NONE',  ( 0.000000000000000000, -1.000000000000000000, 0.000000000000000000 ) ) ;
#15790 = FACE_OUTER_BOUND ( 'NONE', #57231, .T. ) ;
#15791 = CARTESIAN_POINT ( 'NONE',  ( -74.61313452252784373, 36.44950204765962809, -10.00000000000000000 ) ) ;
#15792 = CARTESIAN_POINT ( 'NONE',  ( -83.69499999999997897, -8.437984349512086979, 5.166775262442717831E-16 ) ) ;
#15793 = CARTESIAN_POINT ( 'NONE',  ( 8.102448949553183510, 134.1049999999999329, -5.886773742842746238 ) ) ;
#15794 = CARTESIAN_POINT ( 'NONE',  ( -2.607480562269073321, 126.0929263765338249, -8.025000000000000355 ) ) ;
#15795 =( GEOMETRIC_REPRESENTATION_CONTEXT ( 3 ) GLOBAL_UNCERTAINTY_ASSIGNED_CONTEXT ( ( #58032 ) ) GLOBAL_UNIT_ASSIGNED_CONTEXT ( ( #51349, #13707, #68227 ) ) REPRESENTATION_CONTEXT ( 'NONE', 'WORKASPACE' ) );
#15796 = AXIS2_PLACEMENT_3D ( 'NONE', #54169, #12281, #66101 ) ;
#15797 = CARTESIAN_POINT ( 'NONE',  ( -171.3570736234661922, 5.598654528085804216, 7.705886871421366635 ) ) ;
#15798 = UNCERTAINTY_MEASURE_WITH_UNIT (LENGTH_MEASURE( 1.000000000000000082E-05 ), #28420, 'distance_accuracy_value', 'NONE');
#15799 = MECHANICAL_DESIGN_GEOMETRIC_PRESENTATION_REPRESENTATION (  '', ( #45044 ), #41674 ) ;
#15800 = EDGE_CURVE ( 'NONE', #64678, #30575, #63357, .T. ) ;
#15802 = DIRECTION ( 'NONE',  ( -0.000000000000000000, -0.000000000000000000, -1.000000000000000000 ) ) ;
#15801 = PRODUCT_DEFINITION_FORMATION_WITH_SPECIFIED_SOURCE ( 'ANY', '', #37873, .NOT_KNOWN. ) ;
#15803 = VERTEX_POINT ( 'NONE', #40353 ) ;
#15804 = CARTESIAN_POINT ( 'NONE',  ( -34.99999999999999289, 99.99999999999998579, 7.000000000000000000 ) ) ;
#15805 = STYLED_ITEM ( 'NONE', ( #3705 ), #69613 ) ;
#15806 = FACE_OUTER_BOUND ( 'NONE', #28311, .T. ) ;
#15807 = FACE_OUTER_BOUND ( 'NONE', #30927, .T. ) ;
#15808 = EDGE_LOOP ( 'NONE', ( #3387, #41785, #36162, #1480 ) ) ;
#15809 = ORIENTED_EDGE ( 'NONE', *, *, #3438, .F. ) ;
#15810 = FILL_AREA_STYLE ('',( #31248 ) ) ;
#15811 = VECTOR ( 'NONE', #36232, 1000.000000000000000 ) ;
#15812 = CARTESIAN_POINT ( 'NONE',  ( 6.826472737025119919, 130.8929263765338362, 4.959722759717908325 ) ) ;
#15813 =( BOUNDED_CURVE ( )  B_SPLINE_CURVE ( 2, ( #34389, #55495, #1636, #10942, #39353, #38062, #32378, #2680, #44978, #18210, #23474 ),
 .UNSPECIFIED., .F., .F. ) 
 B_SPLINE_CURVE_WITH_KNOTS ( ( 3, 2, 2, 2, 2, 3 ),
 ( 0.3586956521739045334, 0.3608695652173827817, 0.3630434782608609745, 0.3652173913043392228, 0.3673913043478174156, 0.3695652173912956084 ),
 .UNSPECIFIED. ) 
 CURVE ( )  GEOMETRIC_REPRESENTATION_ITEM ( )  RATIONAL_B_SPLINE_CURVE ( ( 1.000000000000191180, 0.9510565162949623508, 1.000000000000000000, 0.9510565162951535312, 1.000000000000000000, 0.9510565162951535312, 1.000000000000000000, 0.9510565162951535312, 1.000000000000000000, 0.9510565162953497076, 0.9999999999998038236 ) ) 
 REPRESENTATION_ITEM ( '' )  );
#15814 = TOROIDAL_SURFACE ( 'NONE', #14699, 0.5000000000000000000, 0.2500000000000000000 ) ;
#15815 = VECTOR ( 'NONE', #41942, 1000.000000000000000 ) ;
#15816 = FACE_OUTER_BOUND ( 'NONE', #35551, .T. ) ;
#15817 =( NAMED_UNIT ( * ) PLANE_ANGLE_UNIT ( ) SI_UNIT ( $, .RADIAN. ) );
#15818 = CYLINDRICAL_SURFACE ( 'NONE', #8290, 0.5000000000000004441 ) ;
#15819 = FACE_OUTER_BOUND ( 'NONE', #59224, .T. ) ;
#15820 = ORIENTED_EDGE ( 'NONE', *, *, #66531, .T. ) ;
#15821 = CARTESIAN_POINT ( 'NONE',  ( -121.5549999999999926, 0.000000000000000000, 8.024999999999991473 ) ) ;
#15823 = EDGE_CURVE ( 'NONE', #31185, #60007, #2281, .T. ) ;
#15822 = ORIENTED_EDGE ( 'NONE', *, *, #22287, .F. ) ;
#15824 = CARTESIAN_POINT ( 'NONE',  ( -136.7070736234667265, -3.094860106627910223, -9.524999999993106314 ) ) ;
#15825 = FILL_AREA_STYLE ('',( #42256 ) ) ;
#15826 = ADVANCED_FACE ( 'NONE', ( #51248 ), #56871, .T. ) ;
#15827 = ORIENTED_EDGE ( 'NONE', *, *, #12447, .F. ) ;
#15828 = FACE_OUTER_BOUND ( 'NONE', #9421, .T. ) ;
#15829 = FACE_OUTER_BOUND ( 'NONE', #6460, .T. ) ;
#15830 = VERTEX_POINT ( 'NONE', #8683 ) ;
#15831 = CIRCLE ( 'NONE', #59574, 0.2500000000000002220 ) ;
#15832 = CARTESIAN_POINT ( 'NONE',  ( 57.00000000000000000, 16.00000000000000000, 60.00402776293825724 ) ) ;
#15833 = STYLED_ITEM ( 'NONE', ( #25144 ), #34693 ) ;
#15834 = CARTESIAN_POINT ( 'NONE',  ( -3.094860106618434248, 146.7950000000000159, 9.525000000000000355 ) ) ;
#15835 = EDGE_CURVE ( 'NONE', #10952, #35366, #8344, .T. ) ;
#15836 = AXIS2_PLACEMENT_3D ( 'NONE', #14670, #67787, #24850 ) ;
#15837 = VERTEX_POINT ( 'NONE', #19208 ) ;
#15838 = CARTESIAN_POINT ( 'NONE',  ( -8.102448949553179958, 147.6049999999999898, 5.886773742842747126 ) ) ;
#15839 = DIRECTION ( 'NONE',  ( 0.000000000000000000, 0.000000000000000000, -1.000000000000000000 ) ) ;
#15840 = CARTESIAN_POINT ( 'NONE',  ( -48.00000000000000000, 14.49137674618942562, 7.500000000000000000 ) ) ;
#15841 = ORIENTED_EDGE ( 'NONE', *, *, #65936, .T. ) ;
#15842 = CARTESIAN_POINT ( 'NONE',  ( -4.716976649647097730, 126.2429263765338163, -6.492361379858953896 ) ) ;
#15843 = UNCERTAINTY_MEASURE_WITH_UNIT (LENGTH_MEASURE( 1.000000000000000082E-05 ), #14527, 'distance_accuracy_value', 'NONE');
#15844 = COLOUR_RGB ( '', 0.40784314, 0.44705882, 0.49803922) ;
#15845 = CARTESIAN_POINT ( 'NONE',  ( 82.09357085539566867, 5.000000000000000000, -32.00402776293823592 ) ) ;
#15846 = FILL_AREA_STYLE ('',( #26692 ) ) ;
#15847 = ORIENTED_EDGE ( 'NONE', *, *, #21849, .F. ) ;
#15848 = AXIS2_PLACEMENT_3D ( 'NONE', #49229, #60114, #16206 ) ;
#15849 = CARTESIAN_POINT ( 'NONE',  ( -41.38221592241692548, 107.7000202725880911, -3.906946855746217473 ) ) ;
#15850 = EDGE_CURVE ( 'NONE', #3825, #56118, #57240, .T. ) ;
#15851 = EDGE_LOOP ( 'NONE', ( #13899, #18181, #23243, #1679 ) ) ;
#15852 = CARTESIAN_POINT ( 'NONE',  ( -58.64292637653378648, -5.598654528085801552, 7.705886871421367523 ) ) ;
#15853 = DIRECTION ( 'NONE',  ( 0.000000000000000000, -0.000000000000000000, 1.000000000000000000 ) ) ;
#15854 = CARTESIAN_POINT ( 'NONE',  ( -141.8050000000000068, -8.437984349512085203, 5.166775262442717831E-16 ) ) ;
#15855 = DIRECTION ( 'NONE',  ( -1.000000000000000000, 0.000000000000000000, 0.000000000000000000 ) ) ;
#15856 = DIRECTION ( 'NONE',  ( 0.000000000000000000, 0.000000000000000000, -1.000000000000000000 ) ) ;
#15857 = UNCERTAINTY_MEASURE_WITH_UNIT (LENGTH_MEASURE( 1.000000000000000082E-05 ), #2658, 'distance_accuracy_value', 'NONE');
#15858 = VECTOR ( 'NONE', #40041, 1000.000000000000000 ) ;
#15859 = CARTESIAN_POINT ( 'NONE',  ( -4.041451884327381450, -7.000000000000002665, 1.082903768654759791 ) ) ;
#15860 = ADVANCED_FACE ( 'NONE', ( #67411 ), #30110, .T. ) ;
#15861 = FACE_OUTER_BOUND ( 'NONE', #56170, .T. ) ;
#15862 = ORIENTED_EDGE ( 'NONE', *, *, #50069, .F. ) ;
#15863 =( GEOMETRIC_REPRESENTATION_CONTEXT ( 3 ) GLOBAL_UNCERTAINTY_ASSIGNED_CONTEXT ( ( #8689 ) ) GLOBAL_UNIT_ASSIGNED_CONTEXT ( ( #38219, #42132, #52983 ) ) REPRESENTATION_CONTEXT ( 'NONE', 'WORKASPACE' ) );
#15864 = VERTEX_POINT ( 'NONE', #13240 ) ;
#15865 = DIRECTION ( 'NONE',  ( 0.000000000000000000, 0.000000000000000000, 1.000000000000000000 ) ) ;
#15866 = CARTESIAN_POINT ( 'NONE',  ( -69.99999999999998579, 50.00000000000000000, 6.999999999999988454 ) ) ;
#15867 = CARTESIAN_POINT ( 'NONE',  ( -70.25499999999998124, -4.716976649647092401, 6.492361379858946790 ) ) ;
#15868 = ORIENTED_EDGE ( 'NONE', *, *, #65445, .F. ) ;
#15869 = DIRECTION ( 'NONE',  ( -0.000000000000000000, -0.000000000000000000, -1.000000000000000000 ) ) ;
#15870 = PRESENTATION_STYLE_ASSIGNMENT (( #59789 ) ) ;
#15871 = CARTESIAN_POINT ( 'NONE',  ( -27.42392015114097958, -8.499999999999994671, 0.9999999999999991118 ) ) ;
#15872 = DIRECTION ( 'NONE',  ( -0.000000000000000000, -1.000000000000000000, -0.000000000000000000 ) ) ;
#15873 = CARTESIAN_POINT ( 'NONE',  ( -97.79292637653489351, -3.094860106600278993, 9.525000000013179147 ) ) ;
#15874 = ORIENTED_EDGE ( 'NONE', *, *, #11192, .T. ) ;
#15875 = STYLED_ITEM ( 'NONE', ( #1893 ), #45663 ) ;
#15876 = LINE ( 'NONE', #32357, #4313 ) ;
#15877 = DIRECTION ( 'NONE',  ( -1.000000000000000000, -0.000000000000000000, -0.000000000000000000 ) ) ;
#15878 =( LENGTH_UNIT ( ) NAMED_UNIT ( * ) SI_UNIT ( .MILLI., .METRE. ) );
#15879 = STYLED_ITEM ( 'NONE', ( #13336 ), #13584 ) ;
#15880 = CARTESIAN_POINT ( 'NONE',  ( -109.6449999999999960, 4.716976649647091513, -6.492361379858946790 ) ) ;
#15881 = CARTESIAN_POINT ( 'NONE',  ( -1.166476076187854022E-15, 152.9449999999999932, 9.525000000000000355 ) ) ;
#15882 = CARTESIAN_POINT ( 'NONE',  ( -91.19499999999999318, 8.437984349512085203, -1.550032578732815448E-15 ) ) ;
#15883 = VECTOR ( 'NONE', #40828, 1000.000000000000000 ) ;
#15884 =( NAMED_UNIT ( * ) PLANE_ANGLE_UNIT ( ) SI_UNIT ( $, .RADIAN. ) );
#15885 = CARTESIAN_POINT ( 'NONE',  ( -183.0000000000000000, 0.000000000000000000, 0.000000000000000000 ) ) ;
#15886 = VECTOR ( 'NONE', #64, 1000.000000000000000 ) ;
#15887 = UNCERTAINTY_MEASURE_WITH_UNIT (LENGTH_MEASURE( 1.000000000000000082E-05 ), #33268, 'distance_accuracy_value', 'NONE');
#15888 = EDGE_CURVE ( 'NONE', #52425, #16179, #41403, .T. ) ;
#15889 = AXIS2_PLACEMENT_3D ( 'NONE', #44213, #821, #11803 ) ;
#15890 = DIRECTION ( 'NONE',  ( 0.000000000000000000, -1.000000000000000000, 0.000000000000000000 ) ) ;
#15891 = VERTEX_POINT ( 'NONE', #27513 ) ;
#15892 = CARTESIAN_POINT ( 'NONE',  ( -135.1429263765338078, 5.598654528085800663, -7.705886871421367523 ) ) ;
#15893 =( NAMED_UNIT ( * ) SI_UNIT ( $, .STERADIAN. ) SOLID_ANGLE_UNIT ( ) );
#15894 = DIRECTION ( 'NONE',  ( 0.000000000000000000, 0.000000000000000000, 1.000000000000000000 ) ) ;
#15895 = CARTESIAN_POINT ( 'NONE',  ( -146.3950000000000102, -6.826472737025115478, -4.959722759717899443 ) ) ;
#15897 = DIRECTION ( 'NONE',  ( 0.000000000000000000, 1.000000000000000000, 0.000000000000000000 ) ) ;
#15896 = AXIS2_PLACEMENT_3D ( 'NONE', #13092, #45156, #61286 ) ;
#15898 = AXIS2_PLACEMENT_3D ( 'NONE', #54399, #48480, #37241 ) ;
#15899 = LINE ( 'NONE', #16932, #28434 ) ;
#15900 = ORIENTED_EDGE ( 'NONE', *, *, #62983, .T. ) ;
#15901 = ORIENTED_EDGE ( 'NONE', *, *, #34867, .F. ) ;
#15902 = STYLED_ITEM ( 'NONE', ( #33187 ), #17314 ) ;
#15903 = DIRECTION ( 'NONE',  ( 0.000000000000000000, 0.000000000000000000, -1.000000000000000000 ) ) ;
#15904 = UNCERTAINTY_MEASURE_WITH_UNIT (LENGTH_MEASURE( 1.000000000000000082E-05 ), #28086, 'distance_accuracy_value', 'NONE');
#15905 = DIRECTION ( 'NONE',  ( 0.000000000000000000, -1.000000000000000000, 0.000000000000000000 ) ) ;
#15906 = EDGE_CURVE ( 'NONE', #59113, #14523, #62815, .T. ) ;
#15907 = ADVANCED_FACE ( 'NONE', ( #68130 ), #43438, .T. ) ;
#15908 = DIRECTION ( 'NONE',  ( 1.000000000000000000, -0.000000000000000000, 0.000000000000000000 ) ) ;
#15909 = DIRECTION ( 'NONE',  ( -0.9704308468600219006, 0.2413793103448194366, 0.000000000000000000 ) ) ;
#15910 = CARTESIAN_POINT ( 'NONE',  ( -60.44292637653379785, -1.166476076187852838E-15, -9.524999999999991473 ) ) ;
#15911 = PRESENTATION_LAYER_ASSIGNMENT (  '', '', ( #1148 ) ) ;
#15912 = COLOUR_RGB ( '', 0.08235294, 0.09019608, 0.10196078) ;
#15913 = ORIENTED_EDGE ( 'NONE', *, *, #66134, .F. ) ;
#15914 = CARTESIAN_POINT ( 'NONE',  ( -154.8549999999999898, 4.716976649647094177, 6.492361379858945902 ) ) ;
#15915 = ADVANCED_FACE ( 'NONE', ( #10673 ), #44940, .F. ) ;
#15916 = EDGE_CURVE ( 'NONE', #16524, #25661, #727, .T. ) ;
#15917 = ORIENTED_EDGE ( 'NONE', *, *, #21203, .F. ) ;
#15918 = FACE_OUTER_BOUND ( 'NONE', #54653, .T. ) ;
#15919 = FACE_OUTER_BOUND ( 'NONE', #33359, .T. ) ;
#15920 = ORIENTED_EDGE ( 'NONE', *, *, #6993, .F. ) ;
#15921 = SURFACE_STYLE_FILL_AREA ( #69366 ) ;
#15922 = CARTESIAN_POINT ( 'NONE',  ( 0.04677136509298115974, 68.99999999999998579, 2.000000000000000000 ) ) ;
#15923 = CARTESIAN_POINT ( 'NONE',  ( 8.102448949553181734, 117.3949999999999818, 5.886773742842750679 ) ) ;
#15924 = ORIENTED_EDGE ( 'NONE', *, *, #46272, .T. ) ;
#15925 = PRESENTATION_LAYER_ASSIGNMENT (  '', '', ( #33852 ) ) ;
#15926 = CARTESIAN_POINT ( 'NONE',  ( -96.05707362346618083, 0.000000000000000000, 9.524999999999991473 ) ) ;
#15928 = EDGE_CURVE ( 'NONE', #23835, #1731, #46775, .T. ) ;
#15927 = CARTESIAN_POINT ( 'NONE',  ( 8.102448949553181734, 119.1049999999999756, -5.886773742842746238 ) ) ;
#15929 = VECTOR ( 'NONE', #57196, 1000.000000000000000 ) ;
#15930 = CARTESIAN_POINT ( 'NONE',  ( -59.90499999999997982, 2.607480562269069324, -8.024999999999993250 ) ) ;
#15931 = CARTESIAN_POINT ( 'NONE',  ( -116.9949999999999761, -6.826472737025115478, 4.959722759717900331 ) ) ;
#15932 = CARTESIAN_POINT ( 'NONE',  ( -41.84210526315789025, 107.2928455055531600, -4.000000000000000888 ) ) ;
#15933 = ORIENTED_EDGE ( 'NONE', *, *, #52906, .F. ) ;
#15934 = CARTESIAN_POINT ( 'NONE',  ( 0.000000000000000000, 143.5549999999999784, -9.525000000000000355 ) ) ;
#15935 = UNCERTAINTY_MEASURE_WITH_UNIT (LENGTH_MEASURE( 1.000000000000000082E-05 ), #41590, 'distance_accuracy_value', 'NONE');
#15936 = PRESENTATION_STYLE_ASSIGNMENT (( #6719 ) ) ;
#15937 = ADVANCED_FACE ( 'NONE', ( #34 ), #32818, .F. ) ;
#15938 = CIRCLE ( 'NONE', #63097, 4.999999999999997335 ) ;
#15939 = CARTESIAN_POINT ( 'NONE',  ( 4.041451884327375232, 1.417096231345241097, -7.000000000000002665 ) ) ;
#15940 =( GEOMETRIC_REPRESENTATION_CONTEXT ( 3 ) GLOBAL_UNCERTAINTY_ASSIGNED_CONTEXT ( ( #6115 ) ) GLOBAL_UNIT_ASSIGNED_CONTEXT ( ( #58706, #14771, #5220 ) ) REPRESENTATION_CONTEXT ( 'NONE', 'WORKASPACE' ) );
#15941 = CARTESIAN_POINT ( 'NONE',  ( 40.78947368421051323, 108.1536491499103363, -3.000000000000000444 ) ) ;
#15942 = ORIENTED_EDGE ( 'NONE', *, *, #52226, .F. ) ;
#15943 = DIRECTION ( 'NONE',  ( 1.000000000000000000, 1.027984282060330356E-15, 0.000000000000000000 ) ) ;
#15944 =( LENGTH_UNIT ( ) NAMED_UNIT ( * ) SI_UNIT ( .MILLI., .METRE. ) );
#15945 = CARTESIAN_POINT ( 'NONE',  ( -184.1049999999999613, -6.826472737025115478, 4.959722759717900331 ) ) ;
#15947 = ORIENTED_EDGE ( 'NONE', *, *, #3531, .F. ) ;
#15946 = STYLED_ITEM ( 'NONE', ( #27024 ), #35453 ) ;
#15948 = CARTESIAN_POINT ( 'NONE',  ( -15.75000000000000000, -0.9999999999999995559, 20.00000000000000000 ) ) ;
#15949 = PRESENTATION_LAYER_ASSIGNMENT (  '', '', ( #11435 ) ) ;
#15950 = PRESENTATION_STYLE_ASSIGNMENT (( #47989 ) ) ;
#15951 = DIRECTION ( 'NONE',  ( -0.000000000000000000, 1.000000000000000000, -0.000000000000000000 ) ) ;
#15952 =( NAMED_UNIT ( * ) PLANE_ANGLE_UNIT ( ) SI_UNIT ( $, .RADIAN. ) );
#15953 = CARTESIAN_POINT ( 'NONE',  ( -24.21231517720798010, 113.4999999999999858, -9.500000000000000000 ) ) ;
#15954 = VERTEX_POINT ( 'NONE', #59888 ) ;
#15955 = CARTESIAN_POINT ( 'NONE',  ( -0.7098155475105565326, -7.000000000000003553, 0.02753250691854188317 ) ) ;
#15956 = FACE_OUTER_BOUND ( 'NONE', #57506, .T. ) ;
#15957 = CIRCLE ( 'NONE', #16002, 0.2500000000000002220 ) ;
#15958 = CARTESIAN_POINT ( 'NONE',  ( -96.20499999999996987, -2.607480562269071545, -8.024999999999991473 ) ) ;
#15959 = ORIENTED_EDGE ( 'NONE', *, *, #60564, .T. ) ;
#15960 = DIRECTION ( 'NONE',  ( -1.000000000000000000, -0.000000000000000000, -0.000000000000000000 ) ) ;
#15961 = AXIS2_PLACEMENT_3D ( 'NONE', #34342, #60705, #49837 ) ;
#15962 = DIRECTION ( 'NONE',  ( -1.000000000000000000, 0.000000000000000000, 0.000000000000000000 ) ) ;
#15963 = CARTESIAN_POINT ( 'NONE',  ( -132.6570736234661751, 9.058813317711329915, 2.943386871421369566 ) ) ;
#15964 = EDGE_CURVE ( 'NONE', #47636, #1286, #11705, .T. ) ;
#15965 = CARTESIAN_POINT ( 'NONE',  ( -3.094860106618432471, 148.5949999999999136, -9.525000000000000355 ) ) ;
#15966 = CARTESIAN_POINT ( 'NONE',  ( -65.15707362346617515, -9.058813317711329915, -2.943386871421370898 ) ) ;
#15967 = VECTOR ( 'NONE', #12095, 1000.000000000000000 ) ;
#15968 = CARTESIAN_POINT ( 'NONE',  ( -80.09292637653379643, 3.094860106618433360, 9.524999999999991473 ) ) ;
#15969 = ORIENTED_EDGE ( 'NONE', *, *, #49668, .F. ) ;
#15970 = CARTESIAN_POINT ( 'NONE',  ( -13.25000000000000355, 28.24999999999998934, -3.750000000000000000 ) ) ;
#15972 = DIRECTION ( 'NONE',  ( 1.000000000000000000, 0.000000000000000000, 0.000000000000000000 ) ) ;
#15971 = CARTESIAN_POINT ( 'NONE',  ( -60.00000000000000000, -2.024042244987997205E-14, 10.00000000000000000 ) ) ;
#15973 = CARTESIAN_POINT ( 'NONE',  ( -112.8550000000000040, 4.716976649647094177, 6.492361379858945902 ) ) ;
#15974 = CARTESIAN_POINT ( 'NONE',  ( 3.094860106618431583, 123.0949999999999704, 9.525000000000000355 ) ) ;
#15975 = CARTESIAN_POINT ( 'NONE',  ( -118.0450000000000017, 7.632228543268600340, 2.479861379858949277 ) ) ;
#15976 = PRESENTATION_LAYER_ASSIGNMENT (  '', '', ( #61970 ) ) ;
#15977 = LINE ( 'NONE', #37460, #14539 ) ;
#15979 = DIRECTION ( 'NONE',  ( 1.000000000000000000, -1.445602896647339656E-16, 0.000000000000000000 ) ) ;
#15978 = CARTESIAN_POINT ( 'NONE',  ( 44.25000000000000000, 21.74999999999998579, 4.000000000000000000 ) ) ;
#15980 = PRESENTATION_LAYER_ASSIGNMENT (  '', '', ( #46309 ) ) ;
#15981 = ORIENTED_EDGE ( 'NONE', *, *, #30260, .T. ) ;
#15982 = CARTESIAN_POINT ( 'NONE',  ( -158.5429263765338135, 9.058813317711329915, 2.943386871421369566 ) ) ;
#15983 = PRESENTATION_STYLE_ASSIGNMENT (( #10677 ) ) ;
#15984 = CARTESIAN_POINT ( 'NONE',  ( -175.7950000000000159, 2.607480562269068880, -8.024999999999993250 ) ) ;
#15985 = COLOUR_RGB ( '', 0.40784314, 0.44705882, 0.49803922) ;
#15986 = VECTOR ( 'NONE', #44785, 1000.000000000000000 ) ;
#15987 = DIRECTION ( 'NONE',  ( 0.000000000000000000, 0.000000000000000000, -1.000000000000000000 ) ) ;
#15988 = VECTOR ( 'NONE', #53359, 1000.000000000000000 ) ;
#15989 = CARTESIAN_POINT ( 'NONE',  ( -20.57648123434812959, 114.5706806360227290, -10.27659574044459667 ) ) ;
#15990 = LINE ( 'NONE', #9669, #11044 ) ;
#15991 = ORIENTED_EDGE ( 'NONE', *, *, #26062, .F. ) ;
#15992 = CARTESIAN_POINT ( 'NONE',  ( -75.59292637653379643, -3.094860106618431139, -9.524999999999991473 ) ) ;
#15993 = DIRECTION ( 'NONE',  ( 0.000000000000000000, 0.000000000000000000, -1.000000000000000000 ) ) ;
#15994 = CARTESIAN_POINT ( 'NONE',  ( -165.8929263765338078, -8.102448949553174629, -5.886773742842741797 ) ) ;
#15995 = AXIS2_PLACEMENT_3D ( 'NONE', #34061, #27378, #1296 ) ;
#15996 = EDGE_CURVE ( 'NONE', #23645, #60509, #43082, .T. ) ;
#15997 =( NAMED_UNIT ( * ) PLANE_ANGLE_UNIT ( ) SI_UNIT ( $, .RADIAN. ) );
#15998 = DIRECTION ( 'NONE',  ( -3.552713678800500929E-15, 0.000000000000000000, 1.000000000000000000 ) ) ;
#15999 = MECHANICAL_DESIGN_GEOMETRIC_PRESENTATION_REPRESENTATION (  '', ( #54105 ), #45177 ) ;
#16000 = CARTESIAN_POINT ( 'NONE',  ( -183.0550000000000068, -9.827790563157499189E-16, -8.024999999999991473 ) ) ;
#16001 = ADVANCED_FACE ( 'NONE', ( #64487 ), #33646, .T. ) ;
#16002 = AXIS2_PLACEMENT_3D ( 'NONE', #35480, #25259, #46057 ) ;
#16003 = ORIENTED_EDGE ( 'NONE', *, *, #24665, .T. ) ;
#16004 = CONICAL_SURFACE ( 'NONE', #28286, 11.99999999999999645, 0.7853981633974552734 ) ;
#16005 = DIRECTION ( 'NONE',  ( 0.000000000000000000, 0.000000000000000000, 1.000000000000000000 ) ) ;
#16006 = CARTESIAN_POINT ( 'NONE',  ( 13.50000000000000355, 27.99999999999998934, 4.000000000000000000 ) ) ;
#16007 = LINE ( 'NONE', #47702, #64395 ) ;
#16008 = CARTESIAN_POINT ( 'NONE',  ( -44.50000000000000000, 99.99999999999992895, -4.000000000000000000 ) ) ;
#16009 = CARTESIAN_POINT ( 'NONE',  ( -7.632228543268608334, 139.9570736234661581, 2.479861379858952830 ) ) ;
#16010 = AXIS2_PLACEMENT_3D ( 'NONE', #9634, #4292, #68715 ) ;
#16011 = ORIENTED_EDGE ( 'NONE', *, *, #61318, .T. ) ;
#16012 = CARTESIAN_POINT ( 'NONE',  ( -32.39999086766104597, -8.921669375848802375, -1.645138194676287080 ) ) ;
#16013 = CARTESIAN_POINT ( 'NONE',  ( -90.35499999999998977, -4.716976649647093289, -6.492361379858945902 ) ) ;
#16014 = UNCERTAINTY_MEASURE_WITH_UNIT (LENGTH_MEASURE( 1.000000000000000082E-05 ), #7411, 'distance_accuracy_value', 'NONE');
#16015 = VECTOR ( 'NONE', #43800, 1000.000000000000000 ) ;
#16016 = DIRECTION ( 'NONE',  ( 0.000000000000000000, 0.000000000000000000, -1.000000000000000000 ) ) ;
#16017 = ORIENTED_EDGE ( 'NONE', *, *, #26958, .T. ) ;
#16018 = CARTESIAN_POINT ( 'NONE',  ( -35.39493682010693476, -11.23731683406899329, 1.831091074604741520 ) ) ;
#16019 = EDGE_CURVE ( 'NONE', #41524, #66584, #3270, .T. ) ;
#16020 = CARTESIAN_POINT ( 'NONE',  ( -44.99154893936433552, 9.591540374752316467, -3.000000000000000444 ) ) ;
#16021 = FILL_AREA_STYLE ('',( #21240 ) ) ;
#16022 = DIRECTION ( 'NONE',  ( 1.156482317317870344E-15, 1.000000000000000000, 0.000000000000000000 ) ) ;
#16023 = EDGE_LOOP ( 'NONE', ( #9989, #38321, #33772, #67051 ) ) ;
#16024 = CONICAL_SURFACE ( 'NONE', #3593, 6.999999999999997335, 0.7853981633974500554 ) ;
#16025 = SURFACE_STYLE_FILL_AREA ( #64167 ) ;
#16026 = CARTESIAN_POINT ( 'NONE',  ( -70.04499999999998749, 7.632228543268600340, 2.479861379858949277 ) ) ;
#16027 = ORIENTED_EDGE ( 'NONE', *, *, #41616, .F. ) ;
#16028 = DIRECTION ( 'NONE',  ( 0.000000000000000000, 0.000000000000000000, 1.000000000000000000 ) ) ;
#16029 = CIRCLE ( 'NONE', #37449, 0.7499999999999997780 ) ;
#16030 = CARTESIAN_POINT ( 'NONE',  ( 6.414213562373110022, 17.78868675966042190, -3.144186300207962859E-15 ) ) ;
#16031 =( LENGTH_UNIT ( ) NAMED_UNIT ( * ) SI_UNIT ( .MILLI., .METRE. ) );
#16032 = ORIENTED_EDGE ( 'NONE', *, *, #23654, .F. ) ;
#16033 = LINE ( 'NONE', #46678, #8936 ) ;
#16034 = FILL_AREA_STYLE_COLOUR ( '', #54772 ) ;
#16035 = CARTESIAN_POINT ( 'NONE',  ( -126.2049999999999841, -2.607480562269071545, -8.024999999999991473 ) ) ;
#16036 = ORIENTED_EDGE ( 'NONE', *, *, #30550, .F. ) ;
#16037 = EDGE_CURVE ( 'NONE', #55165, #27373, #23298, .T. ) ;
#16038 = DIRECTION ( 'NONE',  ( 0.000000000000000000, 0.000000000000000000, 1.000000000000000000 ) ) ;
#16039 = ORIENTED_EDGE ( 'NONE', *, *, #39333, .F. ) ;
#16040 = CARTESIAN_POINT ( 'NONE',  ( 57.00000000000000000, 5.000000000000000000, 60.00402776293825724 ) ) ;
#16041 = DIRECTION ( 'NONE',  ( 5.782411586589351722E-16, 1.000000000000000000, 0.000000000000000000 ) ) ;
#16042 = DIRECTION ( 'NONE',  ( -1.000000000000000000, 0.000000000000000000, 0.000000000000000000 ) ) ;
#16043 = CARTESIAN_POINT ( 'NONE',  ( -155.4570736234661581, -9.058813317711329915, 2.943386871421371787 ) ) ;
#16044 = EDGE_CURVE ( 'NONE', #37145, #11299, #23200, .T. ) ;
#16045 = CARTESIAN_POINT ( 'NONE',  ( -5.598654528085808657, 119.6449999999999818, 7.705886871421373741 ) ) ;
#16046 = CARTESIAN_POINT ( 'NONE',  ( -89.60707362346614957, -8.102448949553172852, 5.886773742842742685 ) ) ;
#16047 = STYLED_ITEM ( 'NONE', ( #27886 ), #54765 ) ;
#16048 = AXIS2_PLACEMENT_3D ( 'NONE', #3029, #8719, #13638 ) ;
#16049 = ORIENTED_EDGE ( 'NONE', *, *, #57961, .F. ) ;
#16051 = PRESENTATION_STYLE_ASSIGNMENT (( #43152 ) ) ;
#16050 = DIRECTION ( 'NONE',  ( 1.000000000000000000, -0.000000000000000000, 0.000000000000000000 ) ) ;
#16052 = DIRECTION ( 'NONE',  ( 0.000000000000000000, 0.000000000000000000, -1.000000000000000000 ) ) ;
#16053 = CARTESIAN_POINT ( 'NONE',  ( -136.7050000000000125, 2.607480562269073321, 8.024999999999991473 ) ) ;
#16054 = CARTESIAN_POINT ( 'NONE',  ( -8.750000000000001776, 25.24999999999998934, -3.750000000000000000 ) ) ;
#16055 = DIRECTION ( 'NONE',  ( 0.000000000000000000, 0.000000000000000000, 1.000000000000000000 ) ) ;
#16056 = VECTOR ( 'NONE', #16129, 1000.000000000000000 ) ;
#16057 = DIRECTION ( 'NONE',  ( 1.000000000000000000, 0.000000000000000000, 0.000000000000000000 ) ) ;
#16058 = CARTESIAN_POINT ( 'NONE',  ( -143.5449999999999875, -7.632228543268600340, -2.479861379858950166 ) ) ;
#16059 = CARTESIAN_POINT ( 'NONE',  ( -136.7949999999999875, 2.607480562269069324, -8.024999999999993250 ) ) ;
#16060 = ORIENTED_EDGE ( 'NONE', *, *, #16159, .F. ) ;
#16061 = PRESENTATION_STYLE_ASSIGNMENT (( #479 ) ) ;
#16062 = AXIS2_PLACEMENT_3D ( 'NONE', #13768, #7459, #29940 ) ;
#16063 = CARTESIAN_POINT ( 'NONE',  ( 60.00000000000000000, 1.797044900979284448E-15, 12.00000000000000000 ) ) ;
#16064 = SURFACE_STYLE_USAGE ( .BOTH. , #19906 ) ;
#16065 = CARTESIAN_POINT ( 'NONE',  ( -53.45499999999997698, 7.632228543268599452, -2.479861379858951942 ) ) ;
#16066 = DIRECTION ( 'NONE',  ( -1.000000000000000000, 3.552713678800500929E-15, 0.000000000000000000 ) ) ;
#16067 = PRESENTATION_LAYER_ASSIGNMENT (  '', '', ( #5914 ) ) ;
#16068 = DIRECTION ( 'NONE',  ( 8.673617379884026597E-16, -1.000000000000000000, 0.000000000000000000 ) ) ;
#16069 = EDGE_CURVE ( 'NONE', #27439, #67575, #813, .T. ) ;
#16070 =( GEOMETRIC_REPRESENTATION_CONTEXT ( 3 ) GLOBAL_UNCERTAINTY_ASSIGNED_CONTEXT ( ( #31851 ) ) GLOBAL_UNIT_ASSIGNED_CONTEXT ( ( #24899, #40419, #46412 ) ) REPRESENTATION_CONTEXT ( 'NONE', 'WORKASPACE' ) );
#16071 = AXIS2_PLACEMENT_3D ( 'NONE', #26909, #59641, #11460 ) ;
#16072 = CARTESIAN_POINT ( 'NONE',  ( -155.1570736234661751, -9.058813317711329915, -2.943386871421370898 ) ) ;
#16073 = CARTESIAN_POINT ( 'NONE',  ( -109.4929263765337879, -8.102448949553172852, 5.886773742842742685 ) ) ;
#16074 = DIRECTION ( 'NONE',  ( 4.528264053928432625E-17, 4.528264053928433857E-17, 1.000000000000000000 ) ) ;
#16075 = CARTESIAN_POINT ( 'NONE',  ( -8.082903768654762899, 3.516382302766490365E-15, 7.500000000000000000 ) ) ;
#16076 = FACE_OUTER_BOUND ( 'NONE', #53083, .T. ) ;
#16077 = DIRECTION ( 'NONE',  ( -5.782411586589351722E-16, 1.000000000000000000, 0.000000000000000000 ) ) ;
#16078 = EDGE_CURVE ( 'NONE', #2723, #36960, #66805, .T. ) ;
#16079 = CLOSED_SHELL ( 'NONE', ( #26654, #23825, #6136, #64670, #8263, #52437, #63621, #15303, #3444, #25835, #52392, #38332, #55285, #62385, #25634, #56743, #3801, #7149, #31830, #48965, #10805, #59840, #30226, #62030, #69158, #26658 ) ) ;
#16080 = VECTOR ( 'NONE', #31269, 1000.000000000000000 ) ;
#16081 = PLANE ( 'NONE',  #68971 ) ;
#16082 = CARTESIAN_POINT ( 'NONE',  ( 31.00000000000001421, -60.04052944165106709, 35.50000000000000000 ) ) ;
#16083 = ORIENTED_EDGE ( 'NONE', *, *, #47294, .T. ) ;
#16084 = FILL_AREA_STYLE_COLOUR ( '', #31843 ) ;
#16085 = EDGE_CURVE ( 'NONE', #49984, #54537, #56337, .T. ) ;
#16086 = CARTESIAN_POINT ( 'NONE',  ( -7.632228543268607446, 115.6570736234661467, -2.479861379858953718 ) ) ;
#16087 = EDGE_CURVE ( 'NONE', #42918, #38125, #15713, .T. ) ;
#16088 = FILL_AREA_STYLE ('',( #63552 ) ) ;
#16089 = DIRECTION ( 'NONE',  ( -1.000000000000000000, 0.000000000000000000, 0.000000000000000000 ) ) ;
#16090 = PRESENTATION_STYLE_ASSIGNMENT (( #42841 ) ) ;
#16091 = ORIENTED_EDGE ( 'NONE', *, *, #23310, .T. ) ;
#16092 = EDGE_LOOP ( 'NONE', ( #3100, #52839, #11590, #45759 ) ) ;
#16093 =( GEOMETRIC_REPRESENTATION_CONTEXT ( 3 ) GLOBAL_UNCERTAINTY_ASSIGNED_CONTEXT ( ( #368 ) ) GLOBAL_UNIT_ASSIGNED_CONTEXT ( ( #47808, #21007, #48827 ) ) REPRESENTATION_CONTEXT ( 'NONE', 'WORKASPACE' ) );
#16094 = CARTESIAN_POINT ( 'NONE',  ( 4.000000000000001776, 34.36176364315826248, -80.00402776293826435 ) ) ;
#16095 = EDGE_CURVE ( 'NONE', #49856, #23486, #38160, .T. ) ;
#16096 = DIRECTION ( 'NONE',  ( -1.000000000000000000, -0.000000000000000000, -0.000000000000000000 ) ) ;
#16097 = VECTOR ( 'NONE', #62988, 1000.000000000000000 ) ;
#16098 = LINE ( 'NONE', #26923, #50701 ) ;
#16099 = ORIENTED_EDGE ( 'NONE', *, *, #56064, .F. ) ;
#16100 = CARTESIAN_POINT ( 'NONE',  ( -8.102448949553181734, 129.6049999999999613, 5.886773742842747126 ) ) ;
#16101 =( NAMED_UNIT ( * ) SI_UNIT ( $, .STERADIAN. ) SOLID_ANGLE_UNIT ( ) );
#16102 = ORIENTED_EDGE ( 'NONE', *, *, #46904, .T. ) ;
#16103 = PRESENTATION_STYLE_ASSIGNMENT (( #26928 ) ) ;
#16104 = CARTESIAN_POINT ( 'NONE',  ( -101.3949999999999676, -6.826472737025115478, -4.959722759717899443 ) ) ;
#16105 = ORIENTED_EDGE ( 'NONE', *, *, #18268, .F. ) ;
#16106 = STYLED_ITEM ( 'NONE', ( #45038 ), #26271 ) ;
#16107 =( NAMED_UNIT ( * ) SI_UNIT ( $, .STERADIAN. ) SOLID_ANGLE_UNIT ( ) );
#16108 = DIRECTION ( 'NONE',  ( -0.000000000000000000, -0.000000000000000000, -1.000000000000000000 ) ) ;
#16109 = EDGE_LOOP ( 'NONE', ( #29270, #8383, #21698, #46672 ) ) ;
#16110 = CARTESIAN_POINT ( 'NONE',  ( -9.827790563157511022E-16, 151.4429263765338192, 8.025000000000000355 ) ) ;
#16111 =( BOUNDED_CURVE ( )  B_SPLINE_CURVE ( 2, ( #39083, #5283, #10928, #54848, #69665, #21479, #38042, #11617, #42990, #6668, #650 ),
 .UNSPECIFIED., .F., .F. ) 
 B_SPLINE_CURVE_WITH_KNOTS ( ( 3, 2, 2, 2, 2, 3 ),
 ( 0.05882352941176476058, 0.06470588235294123802, 0.07058823529411770159, 0.07647058823529419291, 0.08235294117647065648, 0.08823529411764713393 ),
 .UNSPECIFIED. ) 
 CURVE ( )  GEOMETRIC_REPRESENTATION_ITEM ( )  RATIONAL_B_SPLINE_CURVE ( ( 0.9999999999999995559, 0.9510565162951539753, 1.000000000000000000, 0.9510565162951535312, 1.000000000000000000, 0.9510565162951535312, 1.000000000000000000, 0.9510565162951535312, 1.000000000000000000, 0.9510565162951529761, 1.000000000000000666 ) ) 
 REPRESENTATION_ITEM ( '' )  );
#16112 = CYLINDRICAL_SURFACE ( 'NONE', #8221, 1.000000000000000000 ) ;
#16113 = CARTESIAN_POINT ( 'NONE',  ( -62.90707362346616804, -3.094860106618429807, 9.524999999999991473 ) ) ;
#16114 = ORIENTED_EDGE ( 'NONE', *, *, #6655, .F. ) ;
#16115 = CYLINDRICAL_SURFACE ( 'NONE', #63069, 0.2500000000000002220 ) ;
#16116 = FACE_OUTER_BOUND ( 'NONE', #48240, .T. ) ;
#16117 = SURFACE_SIDE_STYLE ('',( #855 ) ) ;
#16118 = SURFACE_STYLE_USAGE ( .BOTH. , #30868 ) ;
#16119 = AXIS2_PLACEMENT_3D ( 'NONE', #15004, #51928, #36478 ) ;
#16120 = TOROIDAL_SURFACE ( 'NONE', #34054, 8.500000000000012434, 0.5000000000000000000 ) ;
#16121 = PLANE ( 'NONE',  #58959 ) ;
#16122 = CARTESIAN_POINT ( 'NONE',  ( -25.00000000000000355, 36.75000000000000000, 4.000000000000000000 ) ) ;
#16123 = AXIS2_PLACEMENT_3D ( 'NONE', #40404, #12599, #34068 ) ;
#16124 = LINE ( 'NONE', #37601, #247 ) ;
#16125 = CARTESIAN_POINT ( 'NONE',  ( 0.000000000000000000, 2.500000000000000000, 0.000000000000000000 ) ) ;
#16126 = CARTESIAN_POINT ( 'NONE',  ( 2.128399401614408669E-13, 154.1464374838464266, 9.171437483846471395 ) ) ;
#16127 = ORIENTED_EDGE ( 'NONE', *, *, #65603, .T. ) ;
#16128 = EDGE_LOOP ( 'NONE', ( #18155, #2339 ) ) ;
#16129 = DIRECTION ( 'NONE',  ( -0.000000000000000000, -0.000000000000000000, 1.000000000000000000 ) ) ;
#16130 = DIRECTION ( 'NONE',  ( -1.156482317317870739E-15, 0.000000000000000000, -1.000000000000000000 ) ) ;
#16131 = CARTESIAN_POINT ( 'NONE',  ( -170.1570736234661751, -9.058813317711329915, -2.943386871421370898 ) ) ;
#16132 = ORIENTED_EDGE ( 'NONE', *, *, #14205, .F. ) ;
#16133 = LINE ( 'NONE', #69559, #68590 ) ;
#16134 = VECTOR ( 'NONE', #10688, 1000.000000000000000 ) ;
#16135 = CARTESIAN_POINT ( 'NONE',  ( -165.6550000000000011, -7.632228543268600340, -2.479861379858950166 ) ) ;
#16136 = DIRECTION ( 'NONE',  ( -1.189524669241239115E-16, -1.000000000000000000, -0.000000000000000000 ) ) ;
#16137 = DIRECTION ( 'NONE',  ( -0.000000000000000000, -0.000000000000000000, -1.000000000000000000 ) ) ;
#16138 = CARTESIAN_POINT ( 'NONE',  ( -183.1450000000000102, -4.716976649647092401, 6.492361379858946790 ) ) ;
#16139 = AXIS2_PLACEMENT_3D ( 'NONE', #51386, #35566, #29214 ) ;
#16140 = CARTESIAN_POINT ( 'NONE',  ( -169.7949999999999875, 2.607480562269069324, -8.024999999999993250 ) ) ;
#16141 = ORIENTED_EDGE ( 'NONE', *, *, #27780, .T. ) ;
#16142 = SURFACE_SIDE_STYLE ('',( #63264 ) ) ;
#16143 = AXIS2_PLACEMENT_3D ( 'NONE', #26335, #47876, #21069 ) ;
#16144 = CARTESIAN_POINT ( 'NONE',  ( -86.60500000000000398, 6.826472737025113702, -4.959722759717902107 ) ) ;
#16145 = DIRECTION ( 'NONE',  ( 0.000000000000000000, -1.000000000000000000, 0.000000000000000000 ) ) ;
#16146 = CARTESIAN_POINT ( 'NONE',  ( 30.99999999999999289, 0.000000000000000000, 37.00402776293829277 ) ) ;
#16147 = VECTOR ( 'NONE', #43393, 1000.000000000000000 ) ;
#16148 =( GEOMETRIC_REPRESENTATION_CONTEXT ( 3 ) GLOBAL_UNCERTAINTY_ASSIGNED_CONTEXT ( ( #18748 ) ) GLOBAL_UNIT_ASSIGNED_CONTEXT ( ( #40131, #8087, #33771 ) ) REPRESENTATION_CONTEXT ( 'NONE', 'WORKASPACE' ) );
#16149 = CARTESIAN_POINT ( 'NONE',  ( -82.19499999999999318, 8.437984349512086979, -1.550032578732815448E-15 ) ) ;
#16150 = CARTESIAN_POINT ( 'NONE',  ( -10.01517768586949231, 135.3049999999999784, -6.132527647946036459E-16 ) ) ;
#16151 = EDGE_CURVE ( 'NONE', #49912, #56811, #40547, .T. ) ;
#16152 = CARTESIAN_POINT ( 'NONE',  ( 30.99999999999999289, 0.000000000000000000, 24.00402776293822171 ) ) ;
#16153 = EDGE_CURVE ( 'NONE', #44124, #12301, #47155, .T. ) ;
#16154 = FACE_OUTER_BOUND ( 'NONE', #56297, .T. ) ;
#16155 = FILL_AREA_STYLE ('',( #37978 ) ) ;
#16156 = ADVANCED_FACE ( 'NONE', ( #19401 ), #62318, .F. ) ;
#16157 = STYLED_ITEM ( 'NONE', ( #65962 ), #9068 ) ;
#16158 = ORIENTED_EDGE ( 'NONE', *, *, #14728, .F. ) ;
#16159 = EDGE_CURVE ( 'NONE', #29580, #23615, #30267, .T. ) ;
#16160 =( GEOMETRIC_REPRESENTATION_CONTEXT ( 3 ) GLOBAL_UNCERTAINTY_ASSIGNED_CONTEXT ( ( #63619 ) ) GLOBAL_UNIT_ASSIGNED_CONTEXT ( ( #57073, #56374, #35984 ) ) REPRESENTATION_CONTEXT ( 'NONE', 'WORKASPACE' ) );
#16161 = FACE_OUTER_BOUND ( 'NONE', #23338, .T. ) ;
#16162 = EDGE_CURVE ( 'NONE', #42594, #55407, #978, .T. ) ;
#16163 = EDGE_CURVE ( 'NONE', #34861, #24214, #40395, .T. ) ;
#16165 = PRESENTATION_STYLE_ASSIGNMENT (( #58697 ) ) ;
#16164 = FILL_AREA_STYLE ('',( #64992 ) ) ;
#16166 = EDGE_LOOP ( 'NONE', ( #31468, #47829 ) ) ;
#16168 = ORIENTED_EDGE ( 'NONE', *, *, #33137, .F. ) ;
#16167 = STYLED_ITEM ( 'NONE', ( #36521 ), #48348 ) ;
#16169 = COLOUR_RGB ( '', 0.72549020, 0.75294118, 0.79215686) ;
#16170 = CARTESIAN_POINT ( 'NONE',  ( 60.00000000000000000, -2.024042244987997205E-14, -7.500000000000000000 ) ) ;
#16171 = ADVANCED_FACE ( 'NONE', ( #13787 ), #35601, .F. ) ;
#16172 = CARTESIAN_POINT ( 'NONE',  ( 4.716976649647096842, 130.7429263765338021, 6.492361379858953896 ) ) ;
#16173 = PRESENTATION_LAYER_ASSIGNMENT (  '', '', ( #61020 ) ) ;
#16174 = STYLED_ITEM ( 'NONE', ( #50406 ), #2318 ) ;
#16175 = EDGE_CURVE ( 'NONE', #61539, #8709, #59441, .T. ) ;
#16176 = SURFACE_STYLE_USAGE ( .BOTH. , #42568 ) ;
#16177 = FACE_OUTER_BOUND ( 'NONE', #4487, .T. ) ;
#16178 = CARTESIAN_POINT ( 'NONE',  ( 8.437984349512095861, 140.1929263765337907, 1.550032578732816828E-15 ) ) ;
#16179 = VERTEX_POINT ( 'NONE', #10932 ) ;
#16180 = CARTESIAN_POINT ( 'NONE',  ( -126.3549999999999898, -4.716976649647093289, -6.492361379858945902 ) ) ;
#16181 = EDGE_LOOP ( 'NONE', ( #31648, #49518 ) ) ;
#16182 = VERTEX_POINT ( 'NONE', #42995 ) ;
#16183 = CARTESIAN_POINT ( 'NONE',  ( -82.94292637653380496, 0.000000000000000000, 9.524999999999991473 ) ) ;
#16184 = ORIENTED_EDGE ( 'NONE', *, *, #4048, .F. ) ;
#16185 = CIRCLE ( 'NONE', #34125, 5.249999999999997335 ) ;
#16186 =( NAMED_UNIT ( * ) PLANE_ANGLE_UNIT ( ) SI_UNIT ( $, .RADIAN. ) );
#16187 = CARTESIAN_POINT ( 'NONE',  ( 9.058813317711337021, 147.5449999999999875, 2.943386871421375783 ) ) ;
#16188 = CARTESIAN_POINT ( 'NONE',  ( 14.98999599679679662, 118.4999999999999716, 9.500000000000000000 ) ) ;
#16189 = VECTOR ( 'NONE', #16803, 1000.000000000000000 ) ;
#16190 = EDGE_LOOP ( 'NONE', ( #67738, #6770, #63, #57552 ) ) ;
#16191 = FACE_OUTER_BOUND ( 'NONE', #35, .T. ) ;
#16192 = DIRECTION ( 'NONE',  ( 0.000000000000000000, 0.000000000000000000, -1.000000000000000000 ) ) ;
#16193 = FACE_OUTER_BOUND ( 'NONE', #58740, .T. ) ;
#16194 = TOROIDAL_SURFACE ( 'NONE', #57748, 0.7500000000000000000, 0.2500000000000000000 ) ;
#16195 = ORIENTED_EDGE ( 'NONE', *, *, #48261, .F. ) ;
#16196 = CARTESIAN_POINT ( 'NONE',  ( 4.716976649647096842, 130.7429263765338021, 6.492361379858953896 ) ) ;
#16197 = CARTESIAN_POINT ( 'NONE',  ( -9.827790563157511022E-16, 115.4429263765338192, 8.025000000000000355 ) ) ;
#16198 = DIRECTION ( 'NONE',  ( -0.000000000000000000, -0.000000000000000000, 1.000000000000000000 ) ) ;
#16199 = AXIS2_PLACEMENT_3D ( 'NONE', #8480, #52441, #35194 ) ;
#16200 = STYLED_ITEM ( 'NONE', ( #61437 ), #29799 ) ;
#16201 = CARTESIAN_POINT ( 'NONE',  ( 0.000000000000000000, 125.9429263765338192, -8.025000000000000355 ) ) ;
#16202 = CYLINDRICAL_SURFACE ( 'NONE', #19756, 0.2500000000000002220 ) ;
#16203 = ORIENTED_EDGE ( 'NONE', *, *, #47302, .F. ) ;
#16204 = CARTESIAN_POINT ( 'NONE',  ( 8.250000000000001776, 31.24999999999998579, -3.750000000000000000 ) ) ;
#16205 = ORIENTED_EDGE ( 'NONE', *, *, #9491, .T. ) ;
#16206 = DIRECTION ( 'NONE',  ( -1.000000000000000000, 0.000000000000000000, 0.000000000000000000 ) ) ;
#16207 = DIRECTION ( 'NONE',  ( 0.000000000000000000, 0.000000000000000000, -1.000000000000000000 ) ) ;
#16208 = FACE_OUTER_BOUND ( 'NONE', #48598, .T. ) ;
#16209 = CIRCLE ( 'NONE', #46553, 0.5000000000000004441 ) ;
#16210 = CARTESIAN_POINT ( 'NONE',  ( -144.0549999999999784, -9.827790563157499189E-16, -8.024999999999991473 ) ) ;
#16211 = DIRECTION ( 'NONE',  ( -1.000000000000000000, 1.189524669241239115E-16, 0.000000000000000000 ) ) ;
#16212 = CARTESIAN_POINT ( 'NONE',  ( 6.330869393641157750, 43.00000000000000000, -28.38386403503541899 ) ) ;
#16213 = ADVANCED_FACE ( 'NONE', ( #31690 ), #27430, .T. ) ;
#16214 = VECTOR ( 'NONE', #11426, 1000.000000000000000 ) ;
#16215 = VECTOR ( 'NONE', #34943, 1000.000000000000000 ) ;
#16216 = DIRECTION ( 'NONE',  ( -1.000000000000000000, 1.189524669241239115E-16, 0.000000000000000000 ) ) ;
#16217 = CARTESIAN_POINT ( 'NONE',  ( 41.13967244528110712, 107.8968002066633574, 3.376844662569574940 ) ) ;
#16218 = DIRECTION ( 'NONE',  ( 0.000000000000000000, 0.000000000000000000, 1.000000000000000000 ) ) ;
#16219 = ORIENTED_EDGE ( 'NONE', *, *, #40533, .F. ) ;
#16220 = ORIENTED_EDGE ( 'NONE', *, *, #47874, .T. ) ;
#16221 = DIRECTION ( 'NONE',  ( 1.000000000000000000, 0.000000000000000000, 0.000000000000000000 ) ) ;
#16222 = CARTESIAN_POINT ( 'NONE',  ( 31.00000000000000711, 42.00000000000000000, -35.50000000000000000 ) ) ;
#16224 = CARTESIAN_POINT ( 'NONE',  ( -59.30499999999999972, 8.437984349512085203, -1.550032578732815448E-15 ) ) ;
#16223 = MECHANICAL_DESIGN_GEOMETRIC_PRESENTATION_REPRESENTATION (  '', ( #65586 ), #3796 ) ;
#16225 = ORIENTED_EDGE ( 'NONE', *, *, #33436, .F. ) ;
#16226 = LINE ( 'NONE', #10231, #11280 ) ;
#16227 =( NAMED_UNIT ( * ) SI_UNIT ( $, .STERADIAN. ) SOLID_ANGLE_UNIT ( ) );
#16228 = CARTESIAN_POINT ( 'NONE',  ( 14.98999599679679662, 146.4999999999999716, 9.500000000000000000 ) ) ;
#16229 = AXIS2_PLACEMENT_3D ( 'NONE', #46741, #47067, #41431 ) ;
#16230 =( NAMED_UNIT ( * ) SI_UNIT ( $, .STERADIAN. ) SOLID_ANGLE_UNIT ( ) );
#16231 = FACE_OUTER_BOUND ( 'NONE', #68759, .T. ) ;
#16232 = ORIENTED_EDGE ( 'NONE', *, *, #12464, .F. ) ;
#16233 = LINE ( 'NONE', #54165, #51498 ) ;
#16234 = LINE ( 'NONE', #45049, #29284 ) ;
#16235 = DIRECTION ( 'NONE',  ( -1.982541115402069054E-16, 0.000000000000000000, 1.000000000000000000 ) ) ;
#16236 = SURFACE_STYLE_USAGE ( .BOTH. , #64389 ) ;
#16237 = EDGE_CURVE ( 'NONE', #56481, #63720, #15698, .T. ) ;
#16238 = CARTESIAN_POINT ( 'NONE',  ( -106.9449999999999790, -9.827790563157499189E-16, -8.024999999999991473 ) ) ;
#16239 = CARTESIAN_POINT ( 'NONE',  ( -10.01517768586949231, 111.3049999999999784, -6.132527647946036459E-16 ) ) ;
#16240 = CARTESIAN_POINT ( 'NONE',  ( -85.34499999999998465, 7.632228543268599452, -2.479861379858951942 ) ) ;
#16241 = DIRECTION ( 'NONE',  ( 1.000000000000000000, -0.000000000000000000, -1.300977106640434891E-16 ) ) ;
#16242 = CIRCLE ( 'NONE', #26327, 5.000000000000000888 ) ;
#16243 = DIRECTION ( 'NONE',  ( -2.312964634635740689E-15, 1.000000000000000000, 0.000000000000000000 ) ) ;
#16244 = CARTESIAN_POINT ( 'NONE',  ( -168.0570736234661808, 0.000000000000000000, 9.524999999999991473 ) ) ;
#16245 = VECTOR ( 'NONE', #53311, 1000.000000000000000 ) ;
#16246 = EDGE_CURVE ( 'NONE', #8395, #67546, #43680, .T. ) ;
#16247 =( BOUNDED_CURVE ( )  B_SPLINE_CURVE ( 2, ( #41513, #42244, #5218, #26664, #48187, #63634, #20371, #68576, #25985, #15476, #4163 ),
 .UNSPECIFIED., .F., .F. ) 
 B_SPLINE_CURVE_WITH_KNOTS ( ( 3, 2, 2, 2, 2, 3 ),
 ( 0.3586956521739044224, 0.3608695652173826707, 0.3630434782608608635, 0.3652173913043391118, 0.3673913043478173046, 0.3695652173912954974 ),
 .UNSPECIFIED. ) 
 CURVE ( )  GEOMETRIC_REPRESENTATION_ITEM ( )  RATIONAL_B_SPLINE_CURVE ( ( 1.000000000000193623, 0.9510565162949597973, 1.000000000000000000, 0.9510565162951535312, 1.000000000000000000, 0.9510565162951535312, 1.000000000000000000, 0.9510565162951535312, 1.000000000000000000, 0.9510565162953522611, 0.9999999999998012701 ) ) 
 REPRESENTATION_ITEM ( '' )  );
#16248 = CARTESIAN_POINT ( 'NONE',  ( 18.25000000000000711, 0.000000000000000000, 3.750000000000000000 ) ) ;
#16249 = COLOUR_RGB ( '', 0.40784314, 0.44705882, 0.49803922) ;
#16250 = ORIENTED_EDGE ( 'NONE', *, *, #9760, .T. ) ;
#16251 = CARTESIAN_POINT ( 'NONE',  ( -134.9929263765337737, 8.102448949553171076, -5.886773742842744461 ) ) ;
#16252 = AXIS2_PLACEMENT_3D ( 'NONE', #44715, #66105, #29871 ) ;
#16253 =( NAMED_UNIT ( * ) PLANE_ANGLE_UNIT ( ) SI_UNIT ( $, .RADIAN. ) );
#16254 = CARTESIAN_POINT ( 'NONE',  ( -149.9949999999999193, -6.826472737025115478, 4.959722759717900331 ) ) ;
#16255 = FILL_AREA_STYLE_COLOUR ( '', #24635 ) ;
#16256 = VECTOR ( 'NONE', #17029, 1000.000000000000000 ) ;
#16257 = ADVANCED_FACE ( 'NONE', ( #5287 ), #19067, .F. ) ;
#16258 = CARTESIAN_POINT ( 'NONE',  ( -47.09499999999999886, -2.607480562269071545, -8.024999999999991473 ) ) ;
#16259 = SURFACE_STYLE_USAGE ( .BOTH. , #65077 ) ;
#16260 = EDGE_LOOP ( 'NONE', ( #43220, #32483, #23115, #5993 ) ) ;
#16261 = EDGE_LOOP ( 'NONE', ( #23022, #25680, #64635, #27368 ) ) ;
#16262 = SURFACE_STYLE_FILL_AREA ( #47953 ) ;
#16263 = AXIS2_PLACEMENT_3D ( 'NONE', #49582, #61475, #28071 ) ;
#16264 = ADVANCED_FACE ( 'NONE', ( #53167 ), #58428, .T. ) ;
#16265 = CARTESIAN_POINT ( 'NONE',  ( -155.8429263765337964, 9.058813317711329915, -2.943386871421373119 ) ) ;
#16266 = CARTESIAN_POINT ( 'NONE',  ( -45.90836907650464127, 9.403269179647979925, 6.097839204891423392 ) ) ;
#16267 = DIRECTION ( 'NONE',  ( -1.000000000000000000, 0.000000000000000000, 0.000000000000000000 ) ) ;
#16268 = CARTESIAN_POINT ( 'NONE',  ( -116.9929263765337879, 8.102448949553172852, -5.886773742842744461 ) ) ;
#16269 = DIRECTION ( 'NONE',  ( 0.000000000000000000, 1.000000000000000000, 0.000000000000000000 ) ) ;
#16270 = ORIENTED_EDGE ( 'NONE', *, *, #44751, .T. ) ;
#16271 = CARTESIAN_POINT ( 'NONE',  ( -146.9049999999999727, 2.607480562269069324, -8.024999999999993250 ) ) ;
#16272 = CIRCLE ( 'NONE', #42102, 0.2500000000000002220 ) ;
#16273 = ORIENTED_EDGE ( 'NONE', *, *, #63058, .F. ) ;
#16274 = SURFACE_SIDE_STYLE ('',( #64425 ) ) ;
#16275 = EDGE_LOOP ( 'NONE', ( #21952, #46117, #27117, #48230 ) ) ;
#16276 = MECHANICAL_DESIGN_GEOMETRIC_PRESENTATION_REPRESENTATION (  '', ( #53353 ), #21872 ) ;
#16277 = VECTOR ( 'NONE', #43791, 1000.000000000000000 ) ;
#16278 =( LENGTH_UNIT ( ) NAMED_UNIT ( * ) SI_UNIT ( .MILLI., .METRE. ) );
#16279 = PLANE ( 'NONE',  #59036 ) ;
#16280 = CARTESIAN_POINT ( 'NONE',  ( 9.058813317711338797, 117.8449999999999847, -2.943386871421372675 ) ) ;
#16281 = CARTESIAN_POINT ( 'NONE',  ( 0.7152599553061416149, 42.96841831342779017, -74.40727961101599419 ) ) ;
#16282 = ORIENTED_EDGE ( 'NONE', *, *, #58239, .F. ) ;
#16283 = CARTESIAN_POINT ( 'NONE',  ( -71.50000000000000000, 35.92875272052971525, 7.000000000000000000 ) ) ;
#16284 = CARTESIAN_POINT ( 'NONE',  ( -1.166476076187854022E-15, 130.0549999999999784, 9.525000000000000355 ) ) ;
#16285 = CARTESIAN_POINT ( 'NONE',  ( -61.85499999999998266, 4.716976649647094177, 6.492361379858945902 ) ) ;
#16286 = CARTESIAN_POINT ( 'NONE',  ( -120.5949999999999704, 2.607480562269073321, 8.024999999999991473 ) ) ;
#16287 = CARTESIAN_POINT ( 'NONE',  ( -7.511572993685798115E-16, -2.500000000000000000, 6.999999999999997335 ) ) ;
#16288 = ORIENTED_EDGE ( 'NONE', *, *, #19128, .F. ) ;
#16289 = CARTESIAN_POINT ( 'NONE',  ( 8.102448949553181734, 151.5049999999999955, 5.886773742842750679 ) ) ;
#16290 = DIRECTION ( 'NONE',  ( -1.000000000000000000, 0.000000000000000000, 0.000000000000000000 ) ) ;
#16291 = AXIS2_PLACEMENT_3D ( 'NONE', #35739, #51923, #51561 ) ;
#16292 = PRESENTATION_STYLE_ASSIGNMENT (( #20851 ) ) ;
#16293 = PRESENTATION_LAYER_ASSIGNMENT (  '', '', ( #33135 ) ) ;
#16294 = CARTESIAN_POINT ( 'NONE',  ( -49.12162162162162105, 13.70805908423323238, -9.500000000000000000 ) ) ;
#16295 = PRESENTATION_STYLE_ASSIGNMENT (( #9949 ) ) ;
#16296 = ORIENTED_EDGE ( 'NONE', *, *, #34466, .T. ) ;
#16297 = DIRECTION ( 'NONE',  ( 0.000000000000000000, 0.000000000000000000, 1.000000000000000000 ) ) ;
#16299 = PRESENTATION_STYLE_ASSIGNMENT (( #63052 ) ) ;
#16298 = AXIS2_PLACEMENT_3D ( 'NONE', #61329, #28617, #66259 ) ;
#16300 = CARTESIAN_POINT ( 'NONE',  ( -168.5049999999999955, -6.826472737025115478, -4.959722759717899443 ) ) ;
#16301 = ORIENTED_EDGE ( 'NONE', *, *, #28177, .F. ) ;
#16302 = CARTESIAN_POINT ( 'NONE',  ( -144.4429263765337907, -1.166476076187852838E-15, -9.524999999999991473 ) ) ;
#16303 = STYLED_ITEM ( 'NONE', ( #19509 ), #56294 ) ;
#16304 = EDGE_CURVE ( 'NONE', #33822, #68848, #16910, .T. ) ;
#16305 = MECHANICAL_DESIGN_GEOMETRIC_PRESENTATION_REPRESENTATION (  '', ( #48888 ), #25239 ) ;
#16306 = ADVANCED_FACE ( 'NONE', ( #53830 ), #5627, .T. ) ;
#16307 = ORIENTED_EDGE ( 'NONE', *, *, #58494, .T. ) ;
#16308 = CARTESIAN_POINT ( 'NONE',  ( 0.000000000000000000, -7.000000000000000888, 0.000000000000000000 ) ) ;
#16309 = CARTESIAN_POINT ( 'NONE',  ( -88.25499999999998124, -4.716976649647092401, 6.492361379858946790 ) ) ;
#16310 = ORIENTED_EDGE ( 'NONE', *, *, #16849, .F. ) ;
#16311 = CARTESIAN_POINT ( 'NONE',  ( -195.0000000000000000, 1.166476076187852838E-15, -9.524999999999991473 ) ) ;
#16312 = FACE_OUTER_BOUND ( 'NONE', #16109, .T. ) ;
#16313 = DIRECTION ( 'NONE',  ( -0.000000000000000000, -0.000000000000000000, -1.000000000000000000 ) ) ;
#16314 = CARTESIAN_POINT ( 'NONE',  ( -64.25707362346616947, 5.598654528085800663, -7.705886871421367523 ) ) ;
#16315 = AXIS2_PLACEMENT_3D ( 'NONE', #55198, #7023, #49960 ) ;
#16316 =( NAMED_UNIT ( * ) PLANE_ANGLE_UNIT ( ) SI_UNIT ( $, .RADIAN. ) );
#16317 = ORIENTED_EDGE ( 'NONE', *, *, #49262, .F. ) ;
#16318 = CARTESIAN_POINT ( 'NONE',  ( 8.000000000000030198, 5.000000000000000000, 29.00402776293826079 ) ) ;
#16319 = PRESENTATION_STYLE_ASSIGNMENT (( #69073 ) ) ;
#16321 = DIRECTION ( 'NONE',  ( 1.000000000000000000, 0.000000000000000000, 0.000000000000000000 ) ) ;
#16320 = PRESENTATION_STYLE_ASSIGNMENT (( #64477 ) ) ;
#16322 = EDGE_CURVE ( 'NONE', #34272, #25644, #5991, .T. ) ;
#16323 = CARTESIAN_POINT ( 'NONE',  ( -113.1549999999999869, 7.632228543268600340, 2.479861379858949277 ) ) ;
#16324 = EDGE_CURVE ( 'NONE', #22411, #44784, #53926, .T. ) ;
#16325 = CARTESIAN_POINT ( 'NONE',  ( -5.598654528085808657, 131.6449999999999818, 7.705886871421373741 ) ) ;
#16326 = CARTESIAN_POINT ( 'NONE',  ( -112.1949999999999932, 8.437984349512085203, -1.550032578732815448E-15 ) ) ;
#16327 = COLOUR_RGB ( '', 0.66274510, 0.83137255, 0.94901961) ;
#16328 = PRESENTATION_LAYER_ASSIGNMENT (  '', '', ( #58970 ) ) ;
#16329 = SURFACE_STYLE_USAGE ( .BOTH. , #32443 ) ;
#16331 = CARTESIAN_POINT ( 'NONE',  ( 1.000000000000000000, 0.9999999999999991118, 79.00402776293826435 ) ) ;
#16330 = LINE ( 'NONE', #60555, #52617 ) ;
#16332 = EDGE_CURVE ( 'NONE', #52016, #31350, #30306, .T. ) ;
#16333 = CARTESIAN_POINT ( 'NONE',  ( -164.3929263765337510, 8.102448949553176405, 5.886773742842740909 ) ) ;
#16334 = CARTESIAN_POINT ( 'NONE',  ( -179.2449999999999761, -4.716976649647093289, -6.492361379858945902 ) ) ;
#16335 = ADVANCED_FACE ( 'NONE', ( #47940 ), #21132, .F. ) ;
#16336 = STYLED_ITEM ( 'NONE', ( #22991 ), #38953 ) ;
#16337 = CARTESIAN_POINT ( 'NONE',  ( 6.000000000000017764, 42.74314482547740113, -27.71473342867655987 ) ) ;
#16338 = CIRCLE ( 'NONE', #20833, 0.2500000000000002220 ) ;
#16339 = ADVANCED_FACE ( 'NONE', ( #7393 ), #17993, .F. ) ;
#16340 = CARTESIAN_POINT ( 'NONE',  ( -46.95366099282699679, -13.64295980804098996, 2.693440547789818673 ) ) ;
#16341 = CARTESIAN_POINT ( 'NONE',  ( -61.79292637653379217, -3.094860106618429807, 9.524999999999991473 ) ) ;
#16342 = DIRECTION ( 'NONE',  ( -1.000000000000000000, 0.000000000000000000, 0.000000000000000000 ) ) ;
#16343 = ORIENTED_EDGE ( 'NONE', *, *, #31527, .T. ) ;
#16344 = CARTESIAN_POINT ( 'NONE',  ( -80.39292637653379359, 8.102448949553176405, 5.886773742842740909 ) ) ;
#16345 = AXIS2_PLACEMENT_3D ( 'NONE', #14497, #20476, #62347 ) ;
#16346 = DIRECTION ( 'NONE',  ( -0.000000000000000000, -0.000000000000000000, -1.000000000000000000 ) ) ;
#16347 = LINE ( 'NONE', #54619, #59696 ) ;
#16348 = MECHANICAL_DESIGN_GEOMETRIC_PRESENTATION_REPRESENTATION (  '', ( #28687 ), #7380 ) ;
#16349 = ADVANCED_FACE ( 'NONE', ( #28824 ), #7721, .T. ) ;
#16350 = DIRECTION ( 'NONE',  ( 0.000000000000000000, 0.000000000000000000, -1.000000000000000000 ) ) ;
#16351 = DIRECTION ( 'NONE',  ( -1.000000000000000000, 0.000000000000000000, 0.000000000000000000 ) ) ;
#16352 = DIRECTION ( 'NONE',  ( 0.000000000000000000, 0.000000000000000000, 1.000000000000000000 ) ) ;
#16353 = CARTESIAN_POINT ( 'NONE',  ( -183.5049999999999955, -6.826472737025113702, -4.959722759717900331 ) ) ;
#16354 = ORIENTED_EDGE ( 'NONE', *, *, #13027, .F. ) ;
#16355 = DIRECTION ( 'NONE',  ( 0.000000000000000000, 0.000000000000000000, -1.000000000000000000 ) ) ;
#16356 = CARTESIAN_POINT ( 'NONE',  ( -74.00707362346615525, -8.102448949553174629, -5.886773742842741797 ) ) ;
#16357 = CARTESIAN_POINT ( 'NONE',  ( 4.716976649647099507, 138.7570736234661695, -6.492361379858953008 ) ) ;
#16358 = PRESENTATION_LAYER_ASSIGNMENT (  '', '', ( #46710 ) ) ;
#16359 = AXIS2_PLACEMENT_3D ( 'NONE', #68192, #20332, #30174 ) ;
#16360 = ORIENTED_EDGE ( 'NONE', *, *, #67266, .T. ) ;
#16361 = CARTESIAN_POINT ( 'NONE',  ( -101.4570736234661723, -9.058813317711329915, 2.943386871421371787 ) ) ;
#16362 = CARTESIAN_POINT ( 'NONE',  ( -90.20499999999999829, -2.607480562269071545, -8.024999999999991473 ) ) ;
#16363 = PRESENTATION_STYLE_ASSIGNMENT (( #26175 ) ) ;
#16364 = VERTEX_POINT ( 'NONE', #12649 ) ;
#16365 = CARTESIAN_POINT ( 'NONE',  ( -93.05707362346616662, 0.000000000000000000, 9.524999999999991473 ) ) ;
#16366 = VECTOR ( 'NONE', #49448, 1000.000000000000000 ) ;
#16367 = CARTESIAN_POINT ( 'NONE',  ( -141.4429263765337907, -1.166476076187852838E-15, -9.524999999999991473 ) ) ;
#16368 = DIRECTION ( 'NONE',  ( 0.000000000000000000, 0.000000000000000000, -1.000000000000000000 ) ) ;
#16369 = DIRECTION ( 'NONE',  ( 0.000000000000000000, -1.000000000000000000, 0.000000000000000000 ) ) ;
#16370 = CARTESIAN_POINT ( 'NONE',  ( 3.109477999331723641, -1.987149502472171703, 9.000000000000001776 ) ) ;
#16371 = CIRCLE ( 'NONE', #15274, 0.2500000000000002220 ) ;
#16372 = ORIENTED_EDGE ( 'NONE', *, *, #38213, .F. ) ;
#16373 = VECTOR ( 'NONE', #33319, 1000.000000000000000 ) ;
#16374 = DIRECTION ( 'NONE',  ( 0.000000000000000000, 0.000000000000000000, -1.000000000000000000 ) ) ;
#16375 = CARTESIAN_POINT ( 'NONE',  ( -63.74499999999998323, 4.716976649647094177, 6.492361379858945902 ) ) ;
#16376 = VERTEX_POINT ( 'NONE', #11967 ) ;
#16377 = EDGE_CURVE ( 'NONE', #27439, #16813, #22529, .T. ) ;
#16378 = DIRECTION ( 'NONE',  ( 0.000000000000000000, 1.000000000000000000, 0.000000000000000000 ) ) ;
#16379 = PLANE ( 'NONE',  #29686 ) ;
#16380 = VERTEX_POINT ( 'NONE', #33424 ) ;
#16381 = PRESENTATION_STYLE_ASSIGNMENT (( #43129 ) ) ;
#16382 = EDGE_LOOP ( 'NONE', ( #63963, #34123, #27262 ) ) ;
#16383 = CARTESIAN_POINT ( 'NONE',  ( 45.50000000000000000, 9.639620389971918613, -6.500000000000000888 ) ) ;
#16384 = STYLED_ITEM ( 'NONE', ( #30577 ), #39347 ) ;
#16385 = DIRECTION ( 'NONE',  ( -1.000000000000000000, -0.000000000000000000, -0.000000000000000000 ) ) ;
#16386 = CARTESIAN_POINT ( 'NONE',  ( -125.6050000000000040, 6.826472737025113702, -4.959722759717902107 ) ) ;
#16387 = VERTEX_POINT ( 'NONE', #23905 ) ;
#16388 = CARTESIAN_POINT ( 'NONE',  ( 31.28474004469385861, 42.96841831342779727, -45.59272038898399160 ) ) ;
#16389 = AXIS2_PLACEMENT_3D ( 'NONE', #60109, #6994, #43980 ) ;
#16390 = VERTEX_POINT ( 'NONE', #54855 ) ;
#16391 = LINE ( 'NONE', #48065, #23475 ) ;
#16392 = LINE ( 'NONE', #779, #733 ) ;
#16393 = CARTESIAN_POINT ( 'NONE',  ( -161.9070736234662036, -3.094860106618429807, 9.524999999999991473 ) ) ;
#16394 = CARTESIAN_POINT ( 'NONE',  ( -8.102448949553179958, 130.8949999999999818, -5.886773742842749790 ) ) ;
#16395 = COLOUR_RGB ( '', 0.40784314, 0.44705882, 0.49803922) ;
#16396 = CARTESIAN_POINT ( 'NONE',  ( -90.65707362346617515, 9.058813317711329915, 2.943386871421369566 ) ) ;
#16397 = EDGE_CURVE ( 'NONE', #56763, #38684, #65128, .T. ) ;
#16398 = MECHANICAL_DESIGN_GEOMETRIC_PRESENTATION_REPRESENTATION (  '', ( #5140 ), #45626 ) ;
#16399 = DIRECTION ( 'NONE',  ( 0.000000000000000000, 0.000000000000000000, 1.000000000000000000 ) ) ;
#16400 = ORIENTED_EDGE ( 'NONE', *, *, #69634, .F. ) ;
#16401 = FILL_AREA_STYLE_COLOUR ( '', #34033 ) ;
#16402 = EDGE_CURVE ( 'NONE', #25558, #17986, #56129, .T. ) ;
#16404 = FACE_OUTER_BOUND ( 'NONE', #31897, .T. ) ;
#16403 = DIRECTION ( 'NONE',  ( -1.000000000000000000, -0.000000000000000000, 1.300977106640434891E-16 ) ) ;
#16405 = CARTESIAN_POINT ( 'NONE',  ( -4.716976649647098618, 131.2570736234661695, 6.492361379858953008 ) ) ;
#16406 = EDGE_CURVE ( 'NONE', #23835, #51461, #18295, .T. ) ;
#16407 = CARTESIAN_POINT ( 'NONE',  ( -145.2549999999999955, -4.716976649647092401, 6.492361379858946790 ) ) ;
#16408 = FILL_AREA_STYLE ('',( #63848 ) ) ;
#16409 = EDGE_CURVE ( 'NONE', #44595, #10638, #4446, .T. ) ;
#16410 = CARTESIAN_POINT ( 'NONE',  ( 75.00000000000000000, 20.36037961002804053, 6.000000000000000888 ) ) ;
#16411 = CARTESIAN_POINT ( 'NONE',  ( 57.00000000000000000, 13.00000000000000178, 79.00402776293826435 ) ) ;
#16412 = CARTESIAN_POINT ( 'NONE',  ( -148.0449999999999875, 7.632228543268600340, 2.479861379858949277 ) ) ;
#16413 = CARTESIAN_POINT ( 'NONE',  ( -137.6949999999999932, -8.437984349512086979, 5.166775262442717831E-16 ) ) ;
#16414 = ORIENTED_EDGE ( 'NONE', *, *, #10343, .T. ) ;
#16415 = LINE ( 'NONE', #38214, #27967 ) ;
#16416 = CIRCLE ( 'NONE', #49007, 0.5000000000000004441 ) ;
#16417 = CARTESIAN_POINT ( 'NONE',  ( -15.75000000000000000, -0.9999999999999995559, 20.00000000000000000 ) ) ;
#16418 = PRESENTATION_STYLE_ASSIGNMENT (( #119 ) ) ;
#16419 = UNCERTAINTY_MEASURE_WITH_UNIT (LENGTH_MEASURE( 1.000000000000000082E-05 ), #7799, 'distance_accuracy_value', 'NONE');
#16420 = CARTESIAN_POINT ( 'NONE',  ( -56.75499999999997414, 4.716976649647091513, -6.492361379858946790 ) ) ;
#16421 = CARTESIAN_POINT ( 'NONE',  ( -55.49499999999999034, 6.826472737025113702, -4.959722759717902107 ) ) ;
#16422 = ADVANCED_FACE ( 'NONE', ( #57657 ), #40122, .F. ) ;
#16423 = STYLED_ITEM ( 'NONE', ( #35604 ), #64234 ) ;
#16424 = CARTESIAN_POINT ( 'NONE',  ( 48.75000000000000000, 22.24999999999998579, 4.000000000000000000 ) ) ;
#16425 = CARTESIAN_POINT ( 'NONE',  ( -52.64292637653380780, -5.598654528085801552, 7.705886871421367523 ) ) ;
#16426 = CARTESIAN_POINT ( 'NONE',  ( 6.422934014168398598, 153.0000000000000000, 4.811085495980990778 ) ) ;
#16427 = CIRCLE ( 'NONE', #54593, 0.5000000000000004441 ) ;
#16428 = AXIS2_PLACEMENT_3D ( 'NONE', #46760, #56909, #55867 ) ;
#16429 =( GEOMETRIC_REPRESENTATION_CONTEXT ( 3 ) GLOBAL_UNCERTAINTY_ASSIGNED_CONTEXT ( ( #19169 ) ) GLOBAL_UNIT_ASSIGNED_CONTEXT ( ( #18171, #50541, #56493 ) ) REPRESENTATION_CONTEXT ( 'NONE', 'WORKASPACE' ) );
#16430 = DIRECTION ( 'NONE',  ( 0.000000000000000000, 0.000000000000000000, 1.000000000000000000 ) ) ;
#16431 = PRODUCT_DEFINITION_CONTEXT ( 'detailed design', #5990, 'design' ) ;
#16432 = CARTESIAN_POINT ( 'NONE',  ( -107.0929263765337964, 3.094860106618433360, 9.524999999999991473 ) ) ;
#16433 = DIRECTION ( 'NONE',  ( 5.775339657480442461E-17, -1.000000000000000000, 4.528264053928433241E-17 ) ) ;
#16434 = DIRECTION ( 'NONE',  ( 1.000000000000000000, 0.000000000000000000, 0.000000000000000000 ) ) ;
#16435 = LINE ( 'NONE', #4788, #60633 ) ;
#16436 = CARTESIAN_POINT ( 'NONE',  ( -14.98999599679678951, 146.4999999999999716, -9.500000000000000000 ) ) ;
#16437 = TOROIDAL_SURFACE ( 'NONE', #47947, 7.499999999999998224, 0.5000000000000000000 ) ;
#16438 = ADVANCED_FACE ( 'NONE', ( #3083 ), #61511, .T. ) ;
#16439 = ORIENTED_EDGE ( 'NONE', *, *, #27135, .T. ) ;
#16440 = DIRECTION ( 'NONE',  ( -0.000000000000000000, -0.000000000000000000, 1.000000000000000000 ) ) ;
#16441 = PRESENTATION_LAYER_ASSIGNMENT (  '', '', ( #44522 ) ) ;
#16442 = ORIENTED_EDGE ( 'NONE', *, *, #27454, .F. ) ;
#16443 = DIRECTION ( 'NONE',  ( 0.000000000000000000, 0.000000000000000000, -1.000000000000000000 ) ) ;
#16444 = ADVANCED_FACE ( 'NONE', ( #35854 ), #30548, .F. ) ;
#16446 = CARTESIAN_POINT ( 'NONE',  ( -6.826472737025120807, 118.5070736234661695, -4.959722759717907437 ) ) ;
#16445 = COLOUR_RGB ( '', 0.72549020, 0.75294118, 0.79215686) ;
#16447 = SPHERICAL_SURFACE ( 'NONE', #7973, 0.5000000000000000000 ) ;
#16448 = CARTESIAN_POINT ( 'NONE',  ( 75.00000000000000000, 20.14920990499773268, -6.614546734589650256 ) ) ;
#16449 =( NAMED_UNIT ( * ) PLANE_ANGLE_UNIT ( ) SI_UNIT ( $, .RADIAN. ) );
#16450 = VERTEX_POINT ( 'NONE', #24576 ) ;
#16451 = VERTEX_POINT ( 'NONE', #50994 ) ;
#16452 = FILL_AREA_STYLE_COLOUR ( '', #50094 ) ;
#16453 = CARTESIAN_POINT ( 'NONE',  ( -101.5429263765338135, 9.058813317711329915, 2.943386871421369566 ) ) ;
#16454 = ORIENTED_EDGE ( 'NONE', *, *, #62101, .T. ) ;
#16455 = CARTESIAN_POINT ( 'NONE',  ( 5.598654528085805993, 124.3549999999999898, 7.705886871421374629 ) ) ;
#16456 = DIRECTION ( 'NONE',  ( 0.000000000000000000, -1.000000000000000000, 0.000000000000000000 ) ) ;
#16457 = DIRECTION ( 'NONE',  ( 0.000000000000000000, 0.000000000000000000, 1.000000000000000000 ) ) ;
#16458 = CARTESIAN_POINT ( 'NONE',  ( -102.1449999999999818, -4.716976649647092401, 6.492361379858946790 ) ) ;
#16459 = ORIENTED_EDGE ( 'NONE', *, *, #58106, .F. ) ;
#16460 = VECTOR ( 'NONE', #14672, 1000.000000000000000 ) ;
#16461 = CARTESIAN_POINT ( 'NONE',  ( 8.425467196792491009, 153.5331836710477660, -1.554025292114362022 ) ) ;
#16462 = CARTESIAN_POINT ( 'NONE',  ( -43.75000000000000000, 0.000000000000000000, -7.000000000000000000 ) ) ;
#16463 = VERTEX_POINT ( 'NONE', #66837 ) ;
#16464 = CARTESIAN_POINT ( 'NONE',  ( -175.9429263765337907, 0.000000000000000000, 9.524999999999991473 ) ) ;
#16465 = DIRECTION ( 'NONE',  ( 0.000000000000000000, 1.000000000000000000, 0.000000000000000000 ) ) ;
#16466 = CARTESIAN_POINT ( 'NONE',  ( 0.000000000000000000, 87.30187232391182306, 0.000000000000000000 ) ) ;
#16467 = ORIENTED_EDGE ( 'NONE', *, *, #9870, .F. ) ;
#16468 = VECTOR ( 'NONE', #56545, 1000.000000000000000 ) ;
#16469 = EDGE_CURVE ( 'NONE', #16642, #47549, #57359, .T. ) ;
#16470 = LINE ( 'NONE', #55444, #52087 ) ;
#16471 = ORIENTED_EDGE ( 'NONE', *, *, #61146, .F. ) ;
#16472 = FILL_AREA_STYLE_COLOUR ( '', #65270 ) ;
#16473 = VECTOR ( 'NONE', #1752, 1000.000000000000000 ) ;
#16474 = CYLINDRICAL_SURFACE ( 'NONE', #67233, 9.524999999999991473 ) ;
#16475 = FACE_OUTER_BOUND ( 'NONE', #50692, .T. ) ;
#16476 = CARTESIAN_POINT ( 'NONE',  ( 5.000000000000000000, 6.123233995736766282E-16, 0.7500000000000000000 ) ) ;
#16477 = CARTESIAN_POINT ( 'NONE',  ( 35.99999999999999289, 5.000000000000000000, -24.00402776293825369 ) ) ;
#16478 = ADVANCED_FACE ( 'NONE', ( #40455 ), #62910, .T. ) ;
#16479 = CARTESIAN_POINT ( 'NONE',  ( 0.000000000000000000, 42.00000000000000000, -80.00402776293826435 ) ) ;
#16480 = LINE ( 'NONE', #54059, #12404 ) ;
#16481 = CARTESIAN_POINT ( 'NONE',  ( -115.1929263765338050, -10.01517768586948698, 6.132527647946031529E-16 ) ) ;
#16482 = ORIENTED_EDGE ( 'NONE', *, *, #27401, .F. ) ;
#16483 = ORIENTED_EDGE ( 'NONE', *, *, #41702, .T. ) ;
#16484 = CARTESIAN_POINT ( 'NONE',  ( -48.50707362346618368, 8.102448949553176405, 5.886773742842740909 ) ) ;
#16485 = DIRECTION ( 'NONE',  ( 7.709882115452468306E-16, -1.000000000000000000, 0.000000000000000000 ) ) ;
#16486 = CARTESIAN_POINT ( 'NONE',  ( -17.75000000000000711, 31.24999999999999289, -4.000000000000000000 ) ) ;
#16488 = ORIENTED_EDGE ( 'NONE', *, *, #51175, .T. ) ;
#16487 = PRESENTATION_LAYER_ASSIGNMENT (  '', '', ( #10825 ) ) ;
#16489 = DIRECTION ( 'NONE',  ( 0.000000000000000000, -1.000000000000000000, 0.000000000000000000 ) ) ;
#16490 = EDGE_CURVE ( 'NONE', #58312, #47531, #21389, .T. ) ;
#16491 = CARTESIAN_POINT ( 'NONE',  ( -173.7549999999999955, 4.716976649647091513, -6.492361379858946790 ) ) ;
#16492 = DIRECTION ( 'NONE',  ( 1.000000000000000000, 0.000000000000000000, 0.000000000000000000 ) ) ;
#16493 = CARTESIAN_POINT ( 'NONE',  ( 30.25000000000000711, 18.74999999999997868, 4.000000000000000000 ) ) ;
#16494 = CARTESIAN_POINT ( 'NONE',  ( -176.9950000000000045, -6.826472737025115478, 4.959722759717900331 ) ) ;
#16495 = CARTESIAN_POINT ( 'NONE',  ( -163.4949999999999761, 6.826472737025113702, -4.959722759717902107 ) ) ;
#16496 = VERTEX_POINT ( 'NONE', #18952 ) ;
#16497 = FACE_OUTER_BOUND ( 'NONE', #14853, .T. ) ;
#16498 = CARTESIAN_POINT ( 'NONE',  ( -0.4575609230677321060, -2.491211107078691089, 9.000000000000003553 ) ) ;
#16499 = CARTESIAN_POINT ( 'NONE',  ( -79.25499999999999545, -4.716976649647092401, 6.492361379858946790 ) ) ;
#16500 = DIRECTION ( 'NONE',  ( -1.000000000000000000, -0.000000000000000000, -0.000000000000000000 ) ) ;
#16501 = FACE_OUTER_BOUND ( 'NONE', #9340, .T. ) ;
#16502 = EDGE_CURVE ( 'NONE', #22240, #51729, #38311, .T. ) ;
#16503 = CARTESIAN_POINT ( 'NONE',  ( -76.34499999999998465, 7.632228543268599452, -2.479861379858951942 ) ) ;
#16504 = CARTESIAN_POINT ( 'NONE',  ( -3.094860106618432471, 137.7049999999999841, -9.525000000000000355 ) ) ;
#16505 = PLANE ( 'NONE',  #10690 ) ;
#16506 = CARTESIAN_POINT ( 'NONE',  ( 72.50000000000000000, 35.92875272052971525, 9.500000000000000000 ) ) ;
#16507 = UNCERTAINTY_MEASURE_WITH_UNIT (LENGTH_MEASURE( 1.000000000000000082E-05 ), #48435, 'distance_accuracy_value', 'NONE');
#16508 = PRESENTATION_STYLE_ASSIGNMENT (( #43261 ) ) ;
#16509 = DIRECTION ( 'NONE',  ( 0.000000000000000000, 1.000000000000000000, 0.000000000000000000 ) ) ;
#16510 = ORIENTED_EDGE ( 'NONE', *, *, #68452, .T. ) ;
#16511 = CARTESIAN_POINT ( 'NONE',  ( -19.49999999999997513, 8.000000000000000000, -4.000000000000000000 ) ) ;
#16512 =( LENGTH_UNIT ( ) NAMED_UNIT ( * ) SI_UNIT ( .MILLI., .METRE. ) );
#16514 =( NAMED_UNIT ( * ) SI_UNIT ( $, .STERADIAN. ) SOLID_ANGLE_UNIT ( ) );
#16513 = DIRECTION ( 'NONE',  ( 0.000000000000000000, 0.000000000000000000, -1.000000000000000000 ) ) ;
#16515 = PRESENTATION_LAYER_ASSIGNMENT (  '', '', ( #17619 ) ) ;
#16516 = FILL_AREA_STYLE_COLOUR ( '', #35064 ) ;
#16517 = ORIENTED_EDGE ( 'NONE', *, *, #3878, .F. ) ;
#16518 = EDGE_LOOP ( 'NONE', ( #3126, #26674, #62930, #30471 ) ) ;
#16519 = CARTESIAN_POINT ( 'NONE',  ( -7.632228543268608334, 135.8429263765337964, 2.479861379858952830 ) ) ;
#16520 =( NAMED_UNIT ( * ) PLANE_ANGLE_UNIT ( ) SI_UNIT ( $, .RADIAN. ) );
#16521 = SURFACE_STYLE_FILL_AREA ( #32649 ) ;
#16522 = CARTESIAN_POINT ( 'NONE',  ( -34.99999999999999289, 99.99999999999998579, 9.500000000000000000 ) ) ;
#16523 =( BOUNDED_CURVE ( )  B_SPLINE_CURVE ( 2, ( #2122, #65177, #44479, #17026, #33189, #54621, #6433, #65883, #66210, #39523, #7484 ),
 .UNSPECIFIED., .F., .F. ) 
 B_SPLINE_CURVE_WITH_KNOTS ( ( 3, 2, 2, 2, 2, 3 ),
 ( 0.3043478260869493801, 0.3065217391304275729, 0.3086956521739057657, 0.3108695652173839585, 0.3130434782608622069, 0.3152173913043403997 ),
 .UNSPECIFIED. ) 
 CURVE ( )  GEOMETRIC_REPRESENTATION_ITEM ( )  RATIONAL_B_SPLINE_CURVE ( ( 1.000000000000161204, 0.9510565162949923268, 1.000000000000000000, 0.9510565162951535312, 1.000000000000000000, 0.9510565162951535312, 1.000000000000000000, 0.9510565162951535312, 1.000000000000000000, 0.9510565162953209528, 0.9999999999998325784 ) ) 
 REPRESENTATION_ITEM ( '' )  );
#16524 = VERTEX_POINT ( 'NONE', #56611 ) ;
#16525 = CARTESIAN_POINT ( 'NONE',  ( -109.7049999999999699, 2.607480562269072433, 8.024999999999991473 ) ) ;
#16526 = VERTEX_POINT ( 'NONE', #8443 ) ;
#16527 =( NAMED_UNIT ( * ) PLANE_ANGLE_UNIT ( ) SI_UNIT ( $, .RADIAN. ) );
#16528 = VECTOR ( 'NONE', #44913, 1000.000000000000000 ) ;
#16529 = PRESENTATION_STYLE_ASSIGNMENT (( #31261 ) ) ;
#16530 = VERTEX_POINT ( 'NONE', #67507 ) ;
#16531 = DIRECTION ( 'NONE',  ( 1.000000000000000000, 0.000000000000000000, 0.000000000000000000 ) ) ;
#16532 = CARTESIAN_POINT ( 'NONE',  ( -15.75000000000000000, -3.000000000000000000, 20.00000000000000000 ) ) ;
#16533 = ORIENTED_EDGE ( 'NONE', *, *, #42548, .T. ) ;
#16534 = DIRECTION ( 'NONE',  ( -1.000000000000000000, 0.000000000000000000, 0.000000000000000000 ) ) ;
#16535 = CARTESIAN_POINT ( 'NONE',  ( 9.058813317711337021, 156.5449999999999875, 2.943386871421375783 ) ) ;
#16536 = SURFACE_SIDE_STYLE ('',( #21784 ) ) ;
#16537 = ORIENTED_EDGE ( 'NONE', *, *, #35025, .T. ) ;
#16538 =( LENGTH_UNIT ( ) NAMED_UNIT ( * ) SI_UNIT ( .MILLI., .METRE. ) );
#16539 = SURFACE_SIDE_STYLE ('',( #64344 ) ) ;
#16540 = DIRECTION ( 'NONE',  ( -0.000000000000000000, 1.000000000000000000, -0.000000000000000000 ) ) ;
#16541 = DIRECTION ( 'NONE',  ( 0.000000000000000000, 0.000000000000000000, 1.000000000000000000 ) ) ;
#16542 = ORIENTED_EDGE ( 'NONE', *, *, #32236, .T. ) ;
#16543 = CARTESIAN_POINT ( 'NONE',  ( 8.437984349512095861, 122.1929263765337907, 1.550032578732817026E-15 ) ) ;
#16544 = DIRECTION ( 'NONE',  ( -1.000000000000000000, 0.000000000000000000, 0.000000000000000000 ) ) ;
#16545 = DIRECTION ( 'NONE',  ( -1.224646799147353207E-16, 1.000000000000000000, 0.000000000000000000 ) ) ;
#16546 = DIRECTION ( 'NONE',  ( 0.000000000000000000, 0.000000000000000000, 1.000000000000000000 ) ) ;
#16547 = FACE_OUTER_BOUND ( 'NONE', #50064, .T. ) ;
#16548 = EDGE_LOOP ( 'NONE', ( #50583, #3653, #4727, #58723 ) ) ;
#16549 = EDGE_CURVE ( 'NONE', #58067, #34410, #55069, .T. ) ;
#16550 = DIRECTION ( 'NONE',  ( 0.000000000000000000, 0.000000000000000000, -1.000000000000000000 ) ) ;
#16551 = EDGE_LOOP ( 'NONE', ( #65651, #54945 ) ) ;
#16552 = CARTESIAN_POINT ( 'NONE',  ( -51.59292637653378932, -3.094860106618431139, -9.524999999999991473 ) ) ;
#16553 = LINE ( 'NONE', #54135, #21672 ) ;
#16554 = LINE ( 'NONE', #1670, #19794 ) ;
#16555 = CARTESIAN_POINT ( 'NONE',  ( -146.6049999999999329, 6.826472737025113702, -4.959722759717902107 ) ) ;
#16556 = CARTESIAN_POINT ( 'NONE',  ( -175.7070736234663002, -3.094860106619918838, -9.524999999998913225 ) ) ;
#16557 = DIRECTION ( 'NONE',  ( -0.000000000000000000, -0.000000000000000000, -1.000000000000000000 ) ) ;
#16558 = UNCERTAINTY_MEASURE_WITH_UNIT (LENGTH_MEASURE( 1.000000000000000082E-05 ), #802, 'distance_accuracy_value', 'NONE');
#16559 = CARTESIAN_POINT ( 'NONE',  ( -45.18758536601421127, -13.94086583230001963, 0.7847372218215835638 ) ) ;
#16560 = SURFACE_STYLE_USAGE ( .BOTH. , #48580 ) ;
#16561 = VERTEX_POINT ( 'NONE', #25290 ) ;
#16562 = EDGE_CURVE ( 'NONE', #14271, #12616, #33740, .T. ) ;
#16563 = EDGE_LOOP ( 'NONE', ( #24680, #29601, #3549, #33129 ) ) ;
#16564 = DIRECTION ( 'NONE',  ( 0.000000000000000000, -0.000000000000000000, 1.000000000000000000 ) ) ;
#16565 = CIRCLE ( 'NONE', #13192, 0.2500000000000000000 ) ;
#16566 = CARTESIAN_POINT ( 'NONE',  ( 74.99999999999998579, 50.00000000000000000, -9.500000000000000000 ) ) ;
#16567 = CARTESIAN_POINT ( 'NONE',  ( -53.75499999999999545, 4.716976649647091513, -6.492361379858946790 ) ) ;
#16568 = ORIENTED_EDGE ( 'NONE', *, *, #18955, .T. ) ;
#16569 = FILL_AREA_STYLE_COLOUR ( '', #68541 ) ;
#16570 = EDGE_CURVE ( 'NONE', #22515, #5568, #10163, .T. ) ;
#16571 =( LENGTH_UNIT ( ) NAMED_UNIT ( * ) SI_UNIT ( .MILLI., .METRE. ) );
#16572 = SURFACE_SIDE_STYLE ('',( #32700 ) ) ;
#16573 = EDGE_CURVE ( 'NONE', #1147, #10174, #68295, .T. ) ;
#16574 = AXIS2_PLACEMENT_3D ( 'NONE', #49482, #60356, #844 ) ;
#16575 = EDGE_CURVE ( 'NONE', #30495, #45750, #10611, .T. ) ;
#16576 = DIRECTION ( 'NONE',  ( 1.000000000000000000, -0.000000000000000000, 0.000000000000000000 ) ) ;
#16577 = ORIENTED_EDGE ( 'NONE', *, *, #11434, .T. ) ;
#16578 = ADVANCED_FACE ( 'NONE', ( #16154 ), #19119, .T. ) ;
#16579 = DIRECTION ( 'NONE',  ( -0.7071067811865426878, 8.659560562354994488E-17, -0.7071067811865524577 ) ) ;
#16580 = PRESENTATION_STYLE_ASSIGNMENT (( #58092 ) ) ;
#16581 = SURFACE_STYLE_USAGE ( .BOTH. , #59428 ) ;
#16582 = SURFACE_STYLE_FILL_AREA ( #53820 ) ;
#16583 = AXIS2_PLACEMENT_3D ( 'NONE', #53873, #68415, #57512 ) ;
#16584 = CARTESIAN_POINT ( 'NONE',  ( -114.1449999999999960, -4.716976649647092401, 6.492361379858946790 ) ) ;
#16585 = CARTESIAN_POINT ( 'NONE',  ( 10.01517768586949231, 112.8049999999999784, 1.839758294383810543E-15 ) ) ;
#16586 = CARTESIAN_POINT ( 'NONE',  ( -85.79499999999997328, 2.607480562269068880, -8.024999999999993250 ) ) ;
#16587 = DIRECTION ( 'NONE',  ( 0.000000000000000000, 0.000000000000000000, 1.000000000000000000 ) ) ;
#16588 = CARTESIAN_POINT ( 'NONE',  ( -23.71231517720798010, 113.4999999999999858, 9.500000000000000000 ) ) ;
#16589 = CARTESIAN_POINT ( 'NONE',  ( -4.682380833558966060, 2.003239292658526516, -5.889878495889164789 ) ) ;
#16590 = UNCERTAINTY_MEASURE_WITH_UNIT (LENGTH_MEASURE( 1.000000000000000082E-05 ), #4741, 'distance_accuracy_value', 'NONE');
#16591 = DIRECTION ( 'NONE',  ( -0.3420201433256663814, 0.9396926207859092051, 0.000000000000000000 ) ) ;
#16592 = ORIENTED_EDGE ( 'NONE', *, *, #34062, .T. ) ;
#16593 = CARTESIAN_POINT ( 'NONE',  ( -122.8429263765338106, 9.058813317711329915, -2.943386871421373119 ) ) ;
#16594 = CARTESIAN_POINT ( 'NONE',  ( -144.8949999999999818, 6.826472737025116366, 4.959722759717898555 ) ) ;
#16595 = PLANE ( 'NONE',  #63088 ) ;
#16596 = ORIENTED_EDGE ( 'NONE', *, *, #66733, .F. ) ;
#16597 = ORIENTED_EDGE ( 'NONE', *, *, #34896, .T. ) ;
#16598 = DIRECTION ( 'NONE',  ( 0.000000000000000000, -0.3420201433256629953, -0.9396926207859104263 ) ) ;
#16599 = CARTESIAN_POINT ( 'NONE',  ( -20.71231517720798010, 149.9999999999999716, 10.00000000000000000 ) ) ;
#16600 = DIRECTION ( 'NONE',  ( 0.000000000000000000, 0.000000000000000000, -1.000000000000000000 ) ) ;
#16601 = DIRECTION ( 'NONE',  ( -1.000000000000000000, -0.000000000000000000, -0.000000000000000000 ) ) ;
#16602 = AXIS2_PLACEMENT_3D ( 'NONE', #62860, #40405, #4823 ) ;
#16603 = CARTESIAN_POINT ( 'NONE',  ( -116.0929263765346775, 3.094860106632819186, 9.524999999989539390 ) ) ;
#16604 = CIRCLE ( 'NONE', #48059, 0.2500000000000002220 ) ;
#16605 = CARTESIAN_POINT ( 'NONE',  ( 23.00000000000000000, 5.000000000000000000, -24.00402776293825013 ) ) ;
#16606 = ORIENTED_EDGE ( 'NONE', *, *, #1303, .T. ) ;
#16607 = CARTESIAN_POINT ( 'NONE',  ( -137.7549999999999955, 4.716976649647091513, -6.492361379858946790 ) ) ;
#16608 = EDGE_LOOP ( 'NONE', ( #65834, #43788, #51742, #31210 ) ) ;
#16609 = STYLED_ITEM ( 'NONE', ( #269 ), #3945 ) ;
#16610 = EDGE_LOOP ( 'NONE', ( #38757, #69594, #67122, #65007 ) ) ;
#16611 = CARTESIAN_POINT ( 'NONE',  ( 9.250000000000003553, 27.74999999999998934, 4.000000000000000000 ) ) ;
#16612 = ORIENTED_EDGE ( 'NONE', *, *, #17349, .F. ) ;
#16613 = CARTESIAN_POINT ( 'NONE',  ( -4.390521455347699664, 1.510510638266201466, -9.000000000000003553 ) ) ;
#16614 = CARTESIAN_POINT ( 'NONE',  ( -1.166476076187854022E-15, 131.9449999999999932, 9.525000000000000355 ) ) ;
#16615 = CARTESIAN_POINT ( 'NONE',  ( 62.24999999999998579, 33.74999999999999289, 3.750000000000000000 ) ) ;
#16616 = ORIENTED_EDGE ( 'NONE', *, *, #68650, .F. ) ;
#16617 = CARTESIAN_POINT ( 'NONE',  ( -67.99999999999998579, -2.024042244987997205E-14, 12.00000000000000000 ) ) ;
#16618 = CARTESIAN_POINT ( 'NONE',  ( -5.598654528085806881, 128.8549999999999898, -7.705886871421374629 ) ) ;
#16619 = CARTESIAN_POINT ( 'NONE',  ( -62.45499999999998408, 7.632228543268599452, -2.479861379858951942 ) ) ;
#16620 = CARTESIAN_POINT ( 'NONE',  ( -118.7950000000000017, 2.607480562269068880, -8.024999999999993250 ) ) ;
#16621 = CARTESIAN_POINT ( 'NONE',  ( -17.41962728626436530, -0.1139526552317604857, -12.50000000000000000 ) ) ;
#16622 = VERTEX_POINT ( 'NONE', #5206 ) ;
#16623 = CARTESIAN_POINT ( 'NONE',  ( -9.058813317711337021, 147.1549999999999727, -2.943386871421374895 ) ) ;
#16624 = FILL_AREA_STYLE ('',( #27119 ) ) ;
#16625 = UNCERTAINTY_MEASURE_WITH_UNIT (LENGTH_MEASURE( 1.000000000000000082E-05 ), #3002, 'distance_accuracy_value', 'NONE');
#16626 = DIRECTION ( 'NONE',  ( 1.000000000000000000, -0.000000000000000000, 0.000000000000000000 ) ) ;
#16627 = VECTOR ( 'NONE', #24614, 1000.000000000000000 ) ;
#16628 =( NAMED_UNIT ( * ) PLANE_ANGLE_UNIT ( ) SI_UNIT ( $, .RADIAN. ) );
#16629 = DIRECTION ( 'NONE',  ( 0.000000000000000000, 0.000000000000000000, 1.000000000000000000 ) ) ;
#16630 = EDGE_CURVE ( 'NONE', #36960, #9072, #47137, .T. ) ;
#16631 = ORIENTED_EDGE ( 'NONE', *, *, #29025, .F. ) ;
#16632 = CARTESIAN_POINT ( 'NONE',  ( -33.93450318706182856, -9.954220776862968023, -2.519071624164639367 ) ) ;
#16633 = PRESENTATION_STYLE_ASSIGNMENT (( #49665 ) ) ;
#16634 = CARTESIAN_POINT ( 'NONE',  ( -176.3050000000000068, 8.437984349512085203, -1.550032578732815448E-15 ) ) ;
#16635 = EDGE_LOOP ( 'NONE', ( #42332, #44822, #38162 ) ) ;
#16636 = CARTESIAN_POINT ( 'NONE',  ( 3.105708046185522875, 111.8963703285356104, -7.531667776144067794 ) ) ;
#16637 = UNCERTAINTY_MEASURE_WITH_UNIT (LENGTH_MEASURE( 1.000000000000000082E-05 ), #42793, 'distance_accuracy_value', 'NONE');
#16638 = EDGE_CURVE ( 'NONE', #57494, #25423, #46146, .T. ) ;
#16639 = FILL_AREA_STYLE_COLOUR ( '', #59321 ) ;
#16640 = DIRECTION ( 'NONE',  ( 0.000000000000000000, 0.000000000000000000, 1.000000000000000000 ) ) ;
#16641 = LINE ( 'NONE', #10988, #17535 ) ;
#16642 = VERTEX_POINT ( 'NONE', #20718 ) ;
#16643 =( NAMED_UNIT ( * ) SI_UNIT ( $, .STERADIAN. ) SOLID_ANGLE_UNIT ( ) );
#16644 = DIRECTION ( 'NONE',  ( 0.000000000000000000, 0.000000000000000000, 1.000000000000000000 ) ) ;
#16645 = CARTESIAN_POINT ( 'NONE',  ( -83.45499999999998408, 7.632228543268599452, -2.479861379858951942 ) ) ;
#16646 = EDGE_LOOP ( 'NONE', ( #50620, #61471, #10575, #41954 ) ) ;
#16647 = PRESENTATION_STYLE_ASSIGNMENT (( #38476 ) ) ;
#16648 = ADVANCED_FACE ( 'NONE', ( #42551 ), #3365, .F. ) ;
#16649 = PRESENTATION_STYLE_ASSIGNMENT (( #64466 ) ) ;
#16650 = DIRECTION ( 'NONE',  ( -0.000000000000000000, -0.000000000000000000, 1.000000000000000000 ) ) ;
#16651 = DIRECTION ( 'NONE',  ( -0.000000000000000000, -1.000000000000000000, -0.000000000000000000 ) ) ;
#16652 = CARTESIAN_POINT ( 'NONE',  ( -60.95707362346616520, 9.058813317711329915, -2.943386871421373119 ) ) ;
#16653 =( BOUNDED_SURFACE ( )  B_SPLINE_SURFACE ( 3, 2, ( 
 ( #21874, #22915, #5657 ),
 ( #65815, #54555, #60506 ),
 ( #1009, #1383, #12318 ),
 ( #17647, #11649, #64128 ),
 ( #33788, #65464, #7066 ),
 ( #38438, #48280, #17313 ),
 ( #64773, #21507, #32391 ),
 ( #38775, #43025, #33453 ) ),
 .UNSPECIFIED., .F., .F., .F. ) 
 B_SPLINE_SURFACE_WITH_KNOTS ( ( 4, 2, 2, 4 ),
 ( 3, 3 ),
 ( 1.468465106457816916E-14, 0.0009031189008530563856, 0.001806237801691428120, 0.003612475603368171806 ),
 ( 0.000000000000000000, 1.000000000000000000 ),
 .UNSPECIFIED. ) 
 GEOMETRIC_REPRESENTATION_ITEM ( )  RATIONAL_B_SPLINE_SURFACE ( (
 ( 1.000000000000000000, 0.9473232638936814887, 1.000000000000000000),
 ( 1.000000000000000000, 0.9379074176463484402, 1.000000000000000000),
 ( 1.000000000000000000, 0.9271920136555387160, 1.000000000000000000),
 ( 1.000000000000000000, 0.9038526065441394586, 1.000000000000000000),
 ( 1.000000000000000000, 0.8912230047972187208, 1.000000000000000000),
 ( 1.000000000000000000, 0.8514336325998846933, 1.000000000000000000),
 ( 1.000000000000000000, 0.8221224512773489534, 1.000000000000000000),
 ( 1.000000000000000000, 0.7942671885213410388, 1.000000000000000000) ) ) 
 REPRESENTATION_ITEM ( '' )  SURFACE ( )  );
#16654 = VECTOR ( 'NONE', #63351, 1000.000000000000000 ) ;
#16655 = ADVANCED_FACE ( 'NONE', ( #21749 ), #33677, .T. ) ;
#16656 = CARTESIAN_POINT ( 'NONE',  ( -53.60138881051016568, -9.947368421052624754, 2.722470280083841843 ) ) ;
#16657 = ORIENTED_EDGE ( 'NONE', *, *, #7937, .T. ) ;
#16658 = CARTESIAN_POINT ( 'NONE',  ( -8.750000000000001776, 25.24999999999998934, 3.750000000000000000 ) ) ;
#16659 = AXIS2_PLACEMENT_3D ( 'NONE', #17739, #59932, #33217 ) ;
#16661 = DIRECTION ( 'NONE',  ( 0.000000000000000000, 1.000000000000000000, 0.000000000000000000 ) ) ;
#16660 =( NAMED_UNIT ( * ) PLANE_ANGLE_UNIT ( ) SI_UNIT ( $, .RADIAN. ) );
#16662 = CONICAL_SURFACE ( 'NONE', #22253, 7.000000000000000888, 0.7853981633974500554 ) ;
#16663 = CARTESIAN_POINT ( 'NONE',  ( -106.7049999999999983, 2.607480562269073321, 8.024999999999991473 ) ) ;
#16664 = CARTESIAN_POINT ( 'NONE',  ( -3.094860106618432471, 133.5949999999999989, -9.525000000000000355 ) ) ;
#16665 = CARTESIAN_POINT ( 'NONE',  ( -112.0449999999999875, 7.632228543268600340, 2.479861379858949277 ) ) ;
#16666 = AXIS2_PLACEMENT_3D ( 'NONE', #3713, #51255, #41417 ) ;
#16668 = CARTESIAN_POINT ( 'NONE',  ( 1.000000000000000000, 42.00000000000000000, 0.000000000000000000 ) ) ;
#16667 = DIRECTION ( 'NONE',  ( 0.000000000000000000, 0.000000000000000000, -1.000000000000000000 ) ) ;
#16669 = CARTESIAN_POINT ( 'NONE',  ( -157.6429263765338078, -5.598654528085801552, 7.705886871421367523 ) ) ;
#16670 = CARTESIAN_POINT ( 'NONE',  ( -173.2449999999999761, -4.716976649647093289, -6.492361379858945902 ) ) ;
#16671 =( GEOMETRIC_REPRESENTATION_CONTEXT ( 3 ) GLOBAL_UNCERTAINTY_ASSIGNED_CONTEXT ( ( #9397 ) ) GLOBAL_UNIT_ASSIGNED_CONTEXT ( ( #40987, #2567, #66998 ) ) REPRESENTATION_CONTEXT ( 'NONE', 'WORKASPACE' ) );
#16672 = VECTOR ( 'NONE', #27569, 1000.000000000000000 ) ;
#16673 = CARTESIAN_POINT ( 'NONE',  ( -9.827790563157511022E-16, 149.5570736234661524, 8.025000000000000355 ) ) ;
#16674 = CARTESIAN_POINT ( 'NONE',  ( 30.25000000000000711, 18.99999999999997868, 3.750000000000000000 ) ) ;
#16675 = ORIENTED_EDGE ( 'NONE', *, *, #58951, .F. ) ;
#16676 = DIRECTION ( 'NONE',  ( 0.000000000000000000, 0.000000000000000000, -1.000000000000000000 ) ) ;
#16677 = DIRECTION ( 'NONE',  ( 0.000000000000000000, 0.000000000000000000, -1.000000000000000000 ) ) ;
#16678 = ORIENTED_EDGE ( 'NONE', *, *, #25562, .F. ) ;
#16679 = CARTESIAN_POINT ( 'NONE',  ( -80.69292637653380496, 10.01517768586948698, -1.839758294383808571E-15 ) ) ;
#16680 = CARTESIAN_POINT ( 'NONE',  ( 17.15973193263811680, -3.000000000000000000, 2.000000000000000000 ) ) ;
#16681 = LINE ( 'NONE', #60253, #50730 ) ;
#16682 = ADVANCED_FACE ( 'NONE', ( #6578 ), #31478, .T. ) ;
#16683 = SURFACE_STYLE_USAGE ( .BOTH. , #23311 ) ;
#16684 = DIRECTION ( 'NONE',  ( -0.000000000000000000, -0.000000000000000000, 1.000000000000000000 ) ) ;
#16685 = CARTESIAN_POINT ( 'NONE',  ( 0.000000000000000000, -2.500000000000000000, 0.000000000000000000 ) ) ;
#16686 = ORIENTED_EDGE ( 'NONE', *, *, #33349, .F. ) ;
#16687 = CARTESIAN_POINT ( 'NONE',  ( -176.3049999999999784, 8.437984349512086979, -1.550032578732815448E-15 ) ) ;
#16688 = ORIENTED_EDGE ( 'NONE', *, *, #455, .F. ) ;
#16689 = SURFACE_STYLE_USAGE ( .BOTH. , #64509 ) ;
#16690 = CARTESIAN_POINT ( 'NONE',  ( -12.34222745343792127, 149.9999999999999716, -10.18181818181818166 ) ) ;
#16691 = DIRECTION ( 'NONE',  ( 0.000000000000000000, 0.000000000000000000, -1.000000000000000000 ) ) ;
#16692 = FILL_AREA_STYLE ('',( #59203 ) ) ;
#16693 = CARTESIAN_POINT ( 'NONE',  ( -182.8766231262712552, -3.603138673335301689, 9.155714005206574413 ) ) ;
#16694 = CARTESIAN_POINT ( 'NONE',  ( -7.632228543268607446, 142.6570736234661751, -2.479861379858953718 ) ) ;
#16695 = EDGE_LOOP ( 'NONE', ( #45419, #41455, #27797 ) ) ;
#16696 = DIRECTION ( 'NONE',  ( -1.300977106640434891E-16, 0.000000000000000000, -1.000000000000000000 ) ) ;
#16697 = CARTESIAN_POINT ( 'NONE',  ( -88.85499999999998977, 4.716976649647094177, 6.492361379858945902 ) ) ;
#16698 = UNCERTAINTY_MEASURE_WITH_UNIT (LENGTH_MEASURE( 1.000000000000000082E-05 ), #940, 'distance_accuracy_value', 'NONE');
#16699 = DIRECTION ( 'NONE',  ( -1.000000000000000000, -0.000000000000000000, -0.000000000000000000 ) ) ;
#16700 = CIRCLE ( 'NONE', #33493, 1.000000000000000888 ) ;
#16701 = ORIENTED_EDGE ( 'NONE', *, *, #2917, .F. ) ;
#16702 = COLOUR_RGB ( '', 0.72549020, 0.75294118, 0.79215686) ;
#16703 = PRESENTATION_STYLE_ASSIGNMENT (( #60596 ) ) ;
#16704 = EDGE_CURVE ( 'NONE', #33108, #25004, #37163, .T. ) ;
#16705 = CARTESIAN_POINT ( 'NONE',  ( -127.6429263765337936, -5.598654528085801552, 7.705886871421367523 ) ) ;
#16706 = EDGE_CURVE ( 'NONE', #9623, #37678, #43309, .T. ) ;
#16707 = CARTESIAN_POINT ( 'NONE',  ( -33.93619543054067123, -9.954544408048933590, -2.527596102671208822 ) ) ;
#16708 =( NAMED_UNIT ( * ) PLANE_ANGLE_UNIT ( ) SI_UNIT ( $, .RADIAN. ) );
#16709 = ORIENTED_EDGE ( 'NONE', *, *, #39651, .T. ) ;
#16710 = DIRECTION ( 'NONE',  ( 0.000000000000000000, 0.000000000000000000, -1.000000000000000000 ) ) ;
#16711 = CARTESIAN_POINT ( 'NONE',  ( -65.84499999999998465, -7.632228543268599452, 2.479861379858951054 ) ) ;
#16712 = EDGE_LOOP ( 'NONE', ( #58834, #9700, #18080, #67954 ) ) ;
#16713 = CARTESIAN_POINT ( 'NONE',  ( 20.12916642283592950, 110.4999999999999858, -10.05319148936170137 ) ) ;
#16714 = PRESENTATION_LAYER_ASSIGNMENT (  '', '', ( #18921 ) ) ;
#16715 = EDGE_CURVE ( 'NONE', #69269, #60522, #46360, .T. ) ;
#16716 = CARTESIAN_POINT ( 'NONE',  ( -45.00000000000000711, 8.092690183932669257, -5.807220890438251182 ) ) ;
#16717 = ORIENTED_EDGE ( 'NONE', *, *, #22503, .F. ) ;
#16718 = SURFACE_STYLE_FILL_AREA ( #59585 ) ;
#16719 = CARTESIAN_POINT ( 'NONE',  ( 7.750000000000000000, 33.74999999999998579, 3.750000000000000000 ) ) ;
#16720 = ORIENTED_EDGE ( 'NONE', *, *, #2144, .T. ) ;
#16721 = AXIS2_PLACEMENT_3D ( 'NONE', #59419, #11253, #32701 ) ;
#16722 = CARTESIAN_POINT ( 'NONE',  ( 31.00000000000000000, 42.00000000000000000, -80.00402776293826435 ) ) ;
#16723 = CARTESIAN_POINT ( 'NONE',  ( -75.00000000000000000, 8.062885781073912739, 6.000000000000000888 ) ) ;
#16724 = CARTESIAN_POINT ( 'NONE',  ( -111.6549999999999869, -7.632228543268600340, -2.479861379858950166 ) ) ;
#16725 = ORIENTED_EDGE ( 'NONE', *, *, #33304, .T. ) ;
#16726 = CARTESIAN_POINT ( 'NONE',  ( -72.89292637653380780, -8.102448949553174629, -5.886773742842741797 ) ) ;
#16727 = EDGE_CURVE ( 'NONE', #16804, #20191, #23707, .T. ) ;
#16728 = CARTESIAN_POINT ( 'NONE',  ( -72.50000000000001421, 1.797044900979284448E-15, -9.500000000000000000 ) ) ;
#16729 = FACE_OUTER_BOUND ( 'NONE', #22908, .T. ) ;
#16730 = CARTESIAN_POINT ( 'NONE',  ( -161.6070736234661354, -8.102448949553172852, 5.886773742842742685 ) ) ;
#16731 = CARTESIAN_POINT ( 'NONE',  ( -3.094860106618434248, 134.7949999999999875, 9.525000000000000355 ) ) ;
#16732 = CARTESIAN_POINT ( 'NONE',  ( -95.75707362346618368, -5.598654528085801552, 7.705886871421367523 ) ) ;
#16733 = AXIS2_PLACEMENT_3D ( 'NONE', #63348, #41941, #5615 ) ;
#16734 = EDGE_CURVE ( 'NONE', #42940, #59896, #5811, .T. ) ;
#16735 = ORIENTED_EDGE ( 'NONE', *, *, #32471, .F. ) ;
#16736 = CARTESIAN_POINT ( 'NONE',  ( 22.00000000000000711, 50.00000000000000000, -60.00000000000000711 ) ) ;
#16737 = AXIS2_PLACEMENT_3D ( 'NONE', #5345, #42017, #10991 ) ;
#16738 = CARTESIAN_POINT ( 'NONE',  ( -131.0049999999999670, 6.826472737025116366, 4.959722759717898555 ) ) ;
#16739 = FILL_AREA_STYLE_COLOUR ( '', #28500 ) ;
#16740 = CARTESIAN_POINT ( 'NONE',  ( 4.286263797015733637E-16, -2.500000000000000000, 3.499999999999997780 ) ) ;
#16741 = CARTESIAN_POINT ( 'NONE',  ( -54.74292637653380211, -5.598654528085803328, -7.705886871421366635 ) ) ;
#16742 = CARTESIAN_POINT ( 'NONE',  ( -144.5950000000000273, 2.607480562269073321, 8.024999999999991473 ) ) ;
#16743 = AXIS2_PLACEMENT_3D ( 'NONE', #58324, #46799, #31581 ) ;
#16744 = MECHANICAL_DESIGN_GEOMETRIC_PRESENTATION_REPRESENTATION (  '', ( #23426 ), #36999 ) ;
#16745 = CARTESIAN_POINT ( 'NONE',  ( -139.3449999999999989, 7.632228543268599452, -2.479861379858951942 ) ) ;
#16746 = VERTEX_POINT ( 'NONE', #8690 ) ;
#16747 = CARTESIAN_POINT ( 'NONE',  ( 44.82807636874883173, 9.942692122916261255, -2.999113325960748533 ) ) ;
#16748 = FACE_OUTER_BOUND ( 'NONE', #15434, .T. ) ;
#16749 = CARTESIAN_POINT ( 'NONE',  ( -55.25499999999999545, -4.716976649647092401, 6.492361379858946790 ) ) ;
#16750 = PLANE ( 'NONE',  #41683 ) ;
#16751 = CARTESIAN_POINT ( 'NONE',  ( -55.94499999999999318, -9.827790563157499189E-16, -8.024999999999991473 ) ) ;
#16752 = CIRCLE ( 'NONE', #48245, 1.000000000000000888 ) ;
#16753 = DIRECTION ( 'NONE',  ( 1.000000000000000000, 8.673617379884027583E-16, 0.000000000000000000 ) ) ;
#16754 = CARTESIAN_POINT ( 'NONE',  ( -102.8070736234661666, 10.01517768586948698, -1.839758294383808966E-15 ) ) ;
#16755 = VECTOR ( 'NONE', #17014, 1000.000000000000000 ) ;
#16756 = CYLINDRICAL_SURFACE ( 'NONE', #8799, 0.5000000000000004441 ) ;
#16757 = CARTESIAN_POINT ( 'NONE',  ( -102.2929263765338135, 3.094860106618428031, -9.524999999999993250 ) ) ;
#16758 = CARTESIAN_POINT ( 'NONE',  ( -0.7999999999998532729, 100.0000000000000426, 75.00000000000001421 ) ) ;
#16759 = VECTOR ( 'NONE', #46434, 1000.000000000000000 ) ;
#16760 = CARTESIAN_POINT ( 'NONE',  ( 0.000000000000000000, 87.30187232391182306, 8.025000000000000355 ) ) ;
#16761 = EDGE_CURVE ( 'NONE', #45200, #31185, #54022, .T. ) ;
#16762 = CARTESIAN_POINT ( 'NONE',  ( 48.50000000000000000, 21.99999999999998579, 4.000000000000000000 ) ) ;
#16763 = CARTESIAN_POINT ( 'NONE',  ( -99.50707362346614104, 8.102448949553176405, 5.886773742842740909 ) ) ;
#16764 = DIRECTION ( 'NONE',  ( -1.000000000000000000, 0.000000000000000000, -0.000000000000000000 ) ) ;
#16765 = ORIENTED_EDGE ( 'NONE', *, *, #9897, .F. ) ;
#16766 = CARTESIAN_POINT ( 'NONE',  ( -6.826472737025120807, 138.9929263765338305, 4.959722759717906548 ) ) ;
#16767 = CARTESIAN_POINT ( 'NONE',  ( -5.000000000000000000, 0.000000000000000000, 0.7500000000000000000 ) ) ;
#16768 = VERTEX_POINT ( 'NONE', #24487 ) ;
#16769 = LINE ( 'NONE', #44220, #52170 ) ;
#16770 = CARTESIAN_POINT ( 'NONE',  ( -2.607480562269073765, 115.2070736234661723, -8.025000000000000355 ) ) ;
#16771 = ADVANCED_FACE ( 'NONE', ( #2666 ), #19918, .T. ) ;
#16772 = COLOUR_RGB ( '', 0.08235294, 0.09019608, 0.10196078) ;
#16773 = DIRECTION ( 'NONE',  ( 1.156482317317870344E-15, -1.000000000000000000, -0.000000000000000000 ) ) ;
#16774 = FILL_AREA_STYLE_COLOUR ( '', #20714 ) ;
#16775 = ORIENTED_EDGE ( 'NONE', *, *, #33043, .F. ) ;
#16777 = EDGE_LOOP ( 'NONE', ( #54100, #25170, #50530, #931 ) ) ;
#16776 = AXIS2_PLACEMENT_3D ( 'NONE', #69476, #53977, #27911 ) ;
#16778 = CARTESIAN_POINT ( 'NONE',  ( -5.885195493260865440, -2.499999999999996447, -3.806542393196803431 ) ) ;
#16779 = CARTESIAN_POINT ( 'NONE',  ( 48.74999999999999289, 24.74999999999998579, -3.750000000000000000 ) ) ;
#16780 = EDGE_CURVE ( 'NONE', #47468, #9347, #67488, .T. ) ;
#16781 = DIRECTION ( 'NONE',  ( -0.000000000000000000, -0.000000000000000000, 1.000000000000000000 ) ) ;
#16782 = VERTEX_POINT ( 'NONE', #51594 ) ;
#16783 = EDGE_CURVE ( 'NONE', #44684, #30484, #65274, .T. ) ;
#16784 = FILL_AREA_STYLE_COLOUR ( '', #23231 ) ;
#16785 = AXIS2_PLACEMENT_3D ( 'NONE', #66647, #33926, #45579 ) ;
#16786 = AXIS2_PLACEMENT_3D ( 'NONE', #5089, #26541, #31816 ) ;
#16787 = DIRECTION ( 'NONE',  ( 0.000000000000000000, 0.000000000000000000, 1.000000000000000000 ) ) ;
#16788 = CARTESIAN_POINT ( 'NONE',  ( -91.94499999999997897, -9.827790563157499189E-16, -8.024999999999991473 ) ) ;
#16790 = ORIENTED_EDGE ( 'NONE', *, *, #40458, .F. ) ;
#16789 = AXIS2_PLACEMENT_3D ( 'NONE', #34029, #28738, #18562 ) ;
#16791 = AXIS2_PLACEMENT_3D ( 'NONE', #11333, #9971, #36741 ) ;
#16792 = CARTESIAN_POINT ( 'NONE',  ( 8.301136498571505484, 153.5927615316110746, -2.349027669732494772 ) ) ;
#16793 = DIRECTION ( 'NONE',  ( 0.000000000000000000, 0.000000000000000000, 1.000000000000000000 ) ) ;
#16794 = EDGE_CURVE ( 'NONE', #10834, #22530, #6829, .T. ) ;
#16795 = FACE_OUTER_BOUND ( 'NONE', #22601, .T. ) ;
#16796 = ORIENTED_EDGE ( 'NONE', *, *, #15594, .T. ) ;
#16797 = CYLINDRICAL_SURFACE ( 'NONE', #5535, 0.2500000000000002220 ) ;
#16798 = CARTESIAN_POINT ( 'NONE',  ( 21.75000000000001066, 21.74999999999998224, 3.750000000000000000 ) ) ;
#16799 = MECHANICAL_DESIGN_GEOMETRIC_PRESENTATION_REPRESENTATION (  '', ( #25751 ), #969 ) ;
#16800 = EDGE_CURVE ( 'NONE', #62320, #2411, #5712, .T. ) ;
#16801 = CYLINDRICAL_SURFACE ( 'NONE', #45353, 0.5000000000000004441 ) ;
#16802 = ORIENTED_EDGE ( 'NONE', *, *, #38950, .T. ) ;
#16803 = DIRECTION ( 'NONE',  ( 1.000000000000000000, 0.000000000000000000, 4.625929269271505635E-16 ) ) ;
#16804 = VERTEX_POINT ( 'NONE', #13249 ) ;
#16805 = LINE ( 'NONE', #42871, #50674 ) ;
#16806 = DIRECTION ( 'NONE',  ( 0.000000000000000000, 0.000000000000000000, 1.000000000000000000 ) ) ;
#16807 = SURFACE_STYLE_USAGE ( .BOTH. , #43903 ) ;
#16808 = FILL_AREA_STYLE_COLOUR ( '', #39913 ) ;
#16809 = AXIS2_PLACEMENT_3D ( 'NONE', #63003, #14844, #36321 ) ;
#16810 =( NAMED_UNIT ( * ) PLANE_ANGLE_UNIT ( ) SI_UNIT ( $, .RADIAN. ) );
#16811 = APPLICATION_CONTEXT ( 'automotive_design' ) ;
#16812 = CARTESIAN_POINT ( 'NONE',  ( -6.257356667978481113, 153.2770626485485650, -5.482883996731844789 ) ) ;
#16813 = VERTEX_POINT ( 'NONE', #57209 ) ;
#16814 = CIRCLE ( 'NONE', #29102, 0.2500000000000002220 ) ;
#16815 = FILL_AREA_STYLE_COLOUR ( '', #59806 ) ;
#16816 = CARTESIAN_POINT ( 'NONE',  ( 6.000000000000017764, 26.00000000000000355, -27.50000000000000355 ) ) ;
#16817 = FILL_AREA_STYLE_COLOUR ( '', #33495 ) ;
#16818 = ORIENTED_EDGE ( 'NONE', *, *, #9816, .F. ) ;
#16819 = CARTESIAN_POINT ( 'NONE',  ( -169.1049999999999613, -6.826472737025115478, 4.959722759717900331 ) ) ;
#16820 = DIRECTION ( 'NONE',  ( -1.000000000000000000, 0.000000000000000000, 0.000000000000000000 ) ) ;
#16821 = DIRECTION ( 'NONE',  ( -0.000000000000000000, 1.000000000000000000, -0.000000000000000000 ) ) ;
#16822 = CARTESIAN_POINT ( 'NONE',  ( -178.0450000000000159, 7.632228543268600340, 2.479861379858949277 ) ) ;
#16823 = CARTESIAN_POINT ( 'NONE',  ( -165.4450000000000216, 0.000000000000000000, 8.024999999999991473 ) ) ;
#16824 = EDGE_CURVE ( 'NONE', #30575, #16901, #46726, .T. ) ;
#16825 = AXIS2_PLACEMENT_3D ( 'NONE', #23419, #54728, #11490 ) ;
#16826 = VERTEX_POINT ( 'NONE', #7633 ) ;
#16827 = CARTESIAN_POINT ( 'NONE',  ( 45.00000000000000000, 10.69371294334680300, 3.912397846414697788 ) ) ;
#16829 = FACE_OUTER_BOUND ( 'NONE', #52591, .T. ) ;
#16828 = VECTOR ( 'NONE', #39506, 1000.000000000000000 ) ;
#16830 =( NAMED_UNIT ( * ) PLANE_ANGLE_UNIT ( ) SI_UNIT ( $, .RADIAN. ) );
#16831 = CARTESIAN_POINT ( 'NONE',  ( -78.20499999999996987, -2.607480562269071545, -8.024999999999991473 ) ) ;
#16832 = CARTESIAN_POINT ( 'NONE',  ( 24.70582419978697786, 25.82281152269784386, 27.50002557046276763 ) ) ;
#16833 = DIRECTION ( 'NONE',  ( -0.000000000000000000, -0.000000000000000000, -1.000000000000000000 ) ) ;
#16834 = AXIS2_PLACEMENT_3D ( 'NONE', #7461, #12722, #38817 ) ;
#16835 = CARTESIAN_POINT ( 'NONE',  ( -78.44499999999999318, 0.000000000000000000, 8.024999999999991473 ) ) ;
#16836 = CARTESIAN_POINT ( 'NONE',  ( 8.102448949553181734, 139.5049999999999955, 5.886773742842750679 ) ) ;
#16837 = DIRECTION ( 'NONE',  ( -0.5000000000000001110, 0.8660254037844384856, 0.000000000000000000 ) ) ;
#16838 = AXIS2_PLACEMENT_3D ( 'NONE', #3130, #35207, #50695 ) ;
#16839 = AXIS2_PLACEMENT_3D ( 'NONE', #64175, #30776, #51913 ) ;
#16840 = CARTESIAN_POINT ( 'NONE',  ( 20.42000000000000526, 0.000000000000000000, 12.50000000000000000 ) ) ;
#16841 = AXIS2_PLACEMENT_3D ( 'NONE', #16685, #23652, #44132 ) ;
#16842 =( BOUNDED_CURVE ( )  B_SPLINE_CURVE ( 3, ( #31841, #32523, #43506, #36487 ),
 .UNSPECIFIED., .F., .F. ) 
 B_SPLINE_CURVE_WITH_KNOTS ( ( 4, 4 ),
 ( 1.570796326794896558, 3.141592653589792228 ),
 .UNSPECIFIED. ) 
 CURVE ( )  GEOMETRIC_REPRESENTATION_ITEM ( )  RATIONAL_B_SPLINE_CURVE ( ( 1.000000000000000000, 0.8047378541243652705, 0.8047378541243652705, 1.000000000000000000 ) ) 
 REPRESENTATION_ITEM ( '' )  );
#16843 = COLOUR_RGB ( '', 0.40784314, 0.44705882, 0.49803922) ;
#16844 = FACE_OUTER_BOUND ( 'NONE', #58789, .T. ) ;
#16845 = VERTEX_POINT ( 'NONE', #67082 ) ;
#16846 = CARTESIAN_POINT ( 'NONE',  ( -50.39292637653380780, 8.102448949553176405, 5.886773742842740909 ) ) ;
#16847 = PRESENTATION_LAYER_ASSIGNMENT (  '', '', ( #61729 ) ) ;
#16848 =( NAMED_UNIT ( * ) PLANE_ANGLE_UNIT ( ) SI_UNIT ( $, .RADIAN. ) );
#16849 = EDGE_CURVE ( 'NONE', #25215, #22405, #50563, .T. ) ;
#16850 = CARTESIAN_POINT ( 'NONE',  ( -72.49999999999998579, 64.07124727947029896, -10.00000000000000000 ) ) ;
#16851 = EDGE_LOOP ( 'NONE', ( #63894, #58110, #66405, #62977 ) ) ;
#16852 =( GEOMETRIC_REPRESENTATION_CONTEXT ( 3 ) GLOBAL_UNCERTAINTY_ASSIGNED_CONTEXT ( ( #27042 ) ) GLOBAL_UNIT_ASSIGNED_CONTEXT ( ( #23627, #2830, #25022 ) ) REPRESENTATION_CONTEXT ( 'NONE', 'WORKASPACE' ) );
#16853 = ORIENTED_EDGE ( 'NONE', *, *, #39621, .T. ) ;
#16854 = CARTESIAN_POINT ( 'NONE',  ( 3.749999999999999556, 33.99999999999998579, 4.000000000000000000 ) ) ;
#16855 = ADVANCED_FACE ( 'NONE', ( #61429 ), #9751, .F. ) ;
#16856 = DIRECTION ( 'NONE',  ( 0.000000000000000000, 1.000000000000000000, -0.000000000000000000 ) ) ;
#16857 = COLOUR_RGB ( '', 0.72549020, 0.75294118, 0.79215686) ;
#16858 = DIRECTION ( 'NONE',  ( 1.000000000000000000, 0.000000000000000000, 0.000000000000000000 ) ) ;
#16859 = CARTESIAN_POINT ( 'NONE',  ( 44.99999999999998579, 119.9999999999999716, -7.000000000000000000 ) ) ;
#16860 = ORIENTED_EDGE ( 'NONE', *, *, #49886, .F. ) ;
#16861 = CARTESIAN_POINT ( 'NONE',  ( -108.0549999999999784, -9.827790563157499189E-16, -8.024999999999991473 ) ) ;
#16862 = EDGE_LOOP ( 'NONE', ( #42937, #63709, #64249, #38723 ) ) ;
#16863 = SURFACE_STYLE_USAGE ( .BOTH. , #29085 ) ;
#16864 = ADVANCED_FACE ( 'NONE', ( #34705 ), #58958, .F. ) ;
#16865 = ORIENTED_EDGE ( 'NONE', *, *, #23420, .T. ) ;
#16866 = FILL_AREA_STYLE_COLOUR ( '', #38098 ) ;
#16867 = LINE ( 'NONE', #33025, #50157 ) ;
#16868 = EDGE_LOOP ( 'NONE', ( #518, #54575, #5296, #66856 ) ) ;
#16869 = STYLED_ITEM ( 'NONE', ( #53304 ), #1334 ) ;
#16871 = CARTESIAN_POINT ( 'NONE',  ( 11.00000000000001776, 26.00000000000000355, -24.00000000000000355 ) ) ;
#16870 = MECHANICAL_DESIGN_GEOMETRIC_PRESENTATION_REPRESENTATION (  '', ( #41581 ), #48369 ) ;
#16872 = CARTESIAN_POINT ( 'NONE',  ( -5.598654528085808657, 155.6449999999999818, 7.705886871421373741 ) ) ;
#16873 = DIRECTION ( 'NONE',  ( -0.000000000000000000, -0.000000000000000000, -1.000000000000000000 ) ) ;
#16874 = ORIENTED_EDGE ( 'NONE', *, *, #49595, .F. ) ;
#16875 = VERTEX_POINT ( 'NONE', #52991 ) ;
#16876 = CARTESIAN_POINT ( 'NONE',  ( -117.8070736234661808, 10.01517768586948698, -1.839758294383808966E-15 ) ) ;
#16877 = PLANE ( 'NONE',  #54102 ) ;
#16878 = PRESENTATION_LAYER_ASSIGNMENT (  '', '', ( #39326 ) ) ;
#16879 = CARTESIAN_POINT ( 'NONE',  ( 5.356721384544673725, 2.367558512213880473, 4.721886399977921478 ) ) ;
#16880 = ORIENTED_EDGE ( 'NONE', *, *, #60648, .T. ) ;
#16881 = CARTESIAN_POINT ( 'NONE',  ( -4.716976649647098618, 133.1429263765338362, 6.492361379858953008 ) ) ;
#16882 = CARTESIAN_POINT ( 'NONE',  ( -74.99999999999998579, 50.00000000000000000, 10.50000000000000000 ) ) ;
#16883 = ADVANCED_FACE ( 'NONE', ( #37193 ), #15715, .T. ) ;
#16884 = CARTESIAN_POINT ( 'NONE',  ( 4.383403428314272432, -9.000000000000005329, 1.003298500868273102 ) ) ;
#16885 = VERTEX_POINT ( 'NONE', #4786 ) ;
#16886 = CARTESIAN_POINT ( 'NONE',  ( -23.71231517720798010, 113.4999999999999858, -9.500000000000000000 ) ) ;
#16887 = ORIENTED_EDGE ( 'NONE', *, *, #28441, .F. ) ;
#16888 = CARTESIAN_POINT ( 'NONE',  ( -50.99292637653380211, 8.102448949553171076, -5.886773742842744461 ) ) ;
#16889 = AXIS2_PLACEMENT_3D ( 'NONE', #41932, #14825, #5267 ) ;
#16890 = DIRECTION ( 'NONE',  ( 0.000000000000000000, 1.000000000000000000, 0.000000000000000000 ) ) ;
#16891 = CYLINDRICAL_SURFACE ( 'NONE', #58842, 4.999999999999997335 ) ;
#16892 = CARTESIAN_POINT ( 'NONE',  ( -142.4049999999999443, -2.607480562269069768, 8.024999999999991473 ) ) ;
#16893 = CARTESIAN_POINT ( 'NONE',  ( 5.196152422706636465, -9.000000000000005329, 1.392304845413258274 ) ) ;
#16894 = FILL_AREA_STYLE_COLOUR ( '', #30625 ) ;
#16895 = ORIENTED_EDGE ( 'NONE', *, *, #46261, .T. ) ;
#16896 = CARTESIAN_POINT ( 'NONE',  ( 6.999798566743339556, 49.77026365512251971, -7.251305755767528005 ) ) ;
#16897 = MECHANICAL_DESIGN_GEOMETRIC_PRESENTATION_REPRESENTATION (  '', ( #29196 ), #30290 ) ;
#16898 = SURFACE_STYLE_USAGE ( .BOTH. , #69637 ) ;
#16899 = ORIENTED_EDGE ( 'NONE', *, *, #62291, .T. ) ;
#16900 = AXIS2_PLACEMENT_3D ( 'NONE', #59634, #61021, #43857 ) ;
#16901 = VERTEX_POINT ( 'NONE', #26573 ) ;
#16902 = LINE ( 'NONE', #60458, #55284 ) ;
#16903 = CARTESIAN_POINT ( 'NONE',  ( -55.25499999999999545, -4.716976649647092401, 6.492361379858946790 ) ) ;
#16904 = VERTEX_POINT ( 'NONE', #26242 ) ;
#16905 = PLANE ( 'NONE',  #66648 ) ;
#16906 = CARTESIAN_POINT ( 'NONE',  ( 26.00000000000001066, 21.74999999999998224, -3.750000000000000000 ) ) ;
#16907 = COLOUR_RGB ( '', 0.72549020, 0.75294118, 0.79215686) ;
#16908 = EDGE_CURVE ( 'NONE', #11014, #32568, #13016, .T. ) ;
#16909 = CARTESIAN_POINT ( 'NONE',  ( -75.50000000000000000, 35.50862325381056905, -9.500000000000000000 ) ) ;
#16910 = CIRCLE ( 'NONE', #38262, 0.5000000000000004441 ) ;
#16911 = ORIENTED_EDGE ( 'NONE', *, *, #14953, .F. ) ;
#16912 = PRESENTATION_LAYER_ASSIGNMENT (  '', '', ( #44980 ) ) ;
#16913 = DIRECTION ( 'NONE',  ( -1.000000000000000000, 0.000000000000000000, 0.000000000000000000 ) ) ;
#16915 = DIRECTION ( 'NONE',  ( 1.000000000000000000, 0.000000000000000000, 0.000000000000000000 ) ) ;
#16914 = VECTOR ( 'NONE', #67076, 1000.000000000000000 ) ;
#16916 = FILL_AREA_STYLE_COLOUR ( '', #53918 ) ;
#16917 = CARTESIAN_POINT ( 'NONE',  ( -109.3449999999999847, 7.632228543268599452, -2.479861379858951942 ) ) ;
#16918 = CARTESIAN_POINT ( 'NONE',  ( -8.102448949553181734, 155.4950000000000045, 5.886773742842747126 ) ) ;
#16919 = CARTESIAN_POINT ( 'NONE',  ( -90.89499999999999602, 6.826472737025116366, 4.959722759717898555 ) ) ;
#16920 = LINE ( 'NONE', #26729, #51010 ) ;
#16921 = DIRECTION ( 'NONE',  ( -1.068252564556022042E-16, 0.9944852160011111719, 0.1048768571002353378 ) ) ;
#16922 =( GEOMETRIC_REPRESENTATION_CONTEXT ( 3 ) GLOBAL_UNCERTAINTY_ASSIGNED_CONTEXT ( ( #24937 ) ) GLOBAL_UNIT_ASSIGNED_CONTEXT ( ( #46089, #63278, #52737 ) ) REPRESENTATION_CONTEXT ( 'NONE', 'WORKASPACE' ) );
#16923 = CARTESIAN_POINT ( 'NONE',  ( 0.000000000000000000, 30.74999999999999289, 3.750000000000000000 ) ) ;
#16924 =( NAMED_UNIT ( * ) SI_UNIT ( $, .STERADIAN. ) SOLID_ANGLE_UNIT ( ) );
#16926 = ORIENTED_EDGE ( 'NONE', *, *, #53690, .F. ) ;
#16925 = STYLED_ITEM ( 'NONE', ( #62908 ), #44851 ) ;
#16927 = CARTESIAN_POINT ( 'NONE',  ( -126.2929263765338135, 3.094860106618428031, -9.524999999999993250 ) ) ;
#16928 = FILL_AREA_STYLE_COLOUR ( '', #35976 ) ;
#16929 = CARTESIAN_POINT ( 'NONE',  ( -151.6450000000000102, 4.716976649647091513, -6.492361379858946790 ) ) ;
#16930 = CARTESIAN_POINT ( 'NONE',  ( 32.00000000000002132, 42.00000000000000000, 75.00000000000000000 ) ) ;
#16931 = EDGE_CURVE ( 'NONE', #43539, #63360, #22469, .T. ) ;
#16932 = CARTESIAN_POINT ( 'NONE',  ( 8.000000000000030198, 5.000000000000000000, 29.00402776293826079 ) ) ;
#16933 = MECHANICAL_DESIGN_GEOMETRIC_PRESENTATION_REPRESENTATION (  '', ( #25885 ), #5784 ) ;
#16934 = ORIENTED_EDGE ( 'NONE', *, *, #5104, .F. ) ;
#16935 = EDGE_LOOP ( 'NONE', ( #7974, #17306, #54878, #44650, #34654 ) ) ;
#16936 = CARTESIAN_POINT ( 'NONE',  ( 13.75000000000000533, 30.74999999999999289, 4.000000000000000000 ) ) ;
#16937 = CYLINDRICAL_SURFACE ( 'NONE', #62301, 8.025000000000000355 ) ;
#16938 = MECHANICAL_DESIGN_GEOMETRIC_PRESENTATION_REPRESENTATION (  '', ( #4380 ), #2225 ) ;
#16939 = CARTESIAN_POINT ( 'NONE',  ( -129.3570736234661922, 5.598654528085804216, 7.705886871421366635 ) ) ;
#16940 = CARTESIAN_POINT ( 'NONE',  ( -1.000000000000028644, 0.000000000000000000, 0.000000000000000000 ) ) ;
#16941 = CARTESIAN_POINT ( 'NONE',  ( -151.9429263765338192, 0.000000000000000000, 9.524999999999991473 ) ) ;
#16942 = VERTEX_POINT ( 'NONE', #66299 ) ;
#16943 = CARTESIAN_POINT ( 'NONE',  ( -140.7549999999999955, 4.716976649647091513, -6.492361379858946790 ) ) ;
#16944 = ORIENTED_EDGE ( 'NONE', *, *, #2647, .T. ) ;
#16945 = EDGE_CURVE ( 'NONE', #46101, #30840, #39462, .T. ) ;
#16946 = ORIENTED_EDGE ( 'NONE', *, *, #15232, .T. ) ;
#16947 = DIRECTION ( 'NONE',  ( 0.5000000000000001110, -0.8660254037844384856, 0.000000000000000000 ) ) ;
#16948 = EDGE_LOOP ( 'NONE', ( #47508, #64377, #5758, #21344 ) ) ;
#16949 = AXIS2_PLACEMENT_3D ( 'NONE', #61151, #56561, #3039 ) ;
#16950 = DIRECTION ( 'NONE',  ( 0.000000000000000000, -0.000000000000000000, 1.000000000000000000 ) ) ;
#16951 = ADVANCED_FACE ( 'NONE', ( #49127 ), #58509, .F. ) ;
#16952 = CARTESIAN_POINT ( 'NONE',  ( 0.000000000000000000, 0.000000000000000000, 0.000000000000000000 ) ) ;
#16953 = CARTESIAN_POINT ( 'NONE',  ( -3.094860106618434248, 131.7950000000000159, 9.525000000000000355 ) ) ;
#16954 = PRESENTATION_LAYER_ASSIGNMENT (  '', '', ( #13503 ) ) ;
#16955 = AXIS2_PLACEMENT_3D ( 'NONE', #64217, #59267, #58956 ) ;
#16956 = ORIENTED_EDGE ( 'NONE', *, *, #34366, .F. ) ;
#16957 = DIRECTION ( 'NONE',  ( 0.000000000000000000, 0.000000000000000000, -1.000000000000000000 ) ) ;
#16959 = ADVANCED_FACE ( 'NONE', ( #59268 ), #60662, .T. ) ;
#16958 = CARTESIAN_POINT ( 'NONE',  ( -5.598654528085808657, 132.7549999999999955, 7.705886871421373741 ) ) ;
#16960 = CARTESIAN_POINT ( 'NONE',  ( -56.75499999999997414, 4.716976649647091513, -6.492361379858946790 ) ) ;
#16961 = CARTESIAN_POINT ( 'NONE',  ( -115.9449999999999932, -9.827790563157499189E-16, -8.024999999999991473 ) ) ;
#16962 = CARTESIAN_POINT ( 'NONE',  ( -41.36494435661896318, 107.7173713599242717, -3.929015280517311748 ) ) ;
#16963 = EDGE_LOOP ( 'NONE', ( #20728, #62670, #55445 ) ) ;
#16964 = CARTESIAN_POINT ( 'NONE',  ( -1.166476076187854022E-15, 157.0550000000000068, 9.525000000000000355 ) ) ;
#16965 = DIRECTION ( 'NONE',  ( 0.000000000000000000, 0.000000000000000000, 1.000000000000000000 ) ) ;
#16966 = PRESENTATION_STYLE_ASSIGNMENT (( #59853 ) ) ;
#16967 = EDGE_CURVE ( 'NONE', #67575, #41256, #17460, .T. ) ;
#16968 = DIRECTION ( 'NONE',  ( -1.000000000000000000, 0.000000000000000000, 0.000000000000000000 ) ) ;
#16969 = VERTEX_POINT ( 'NONE', #32547 ) ;
#16970 = CARTESIAN_POINT ( 'NONE',  ( -71.49999999999998579, 119.9999999999997868, 7.000000000000000000 ) ) ;
#16972 = CARTESIAN_POINT ( 'NONE',  ( -169.5549999999999784, 0.000000000000000000, 8.024999999999991473 ) ) ;
#16971 = AXIS2_PLACEMENT_3D ( 'NONE', #38139, #48351, #33180 ) ;
#16973 = EDGE_LOOP ( 'NONE', ( #50077, #19813, #34739, #45380 ) ) ;
#16974 = CARTESIAN_POINT ( 'NONE',  ( 43.75000000000000000, 18.99999999999998224, -4.000000000000000000 ) ) ;
#16975 = SURFACE_STYLE_USAGE ( .BOTH. , #6734 ) ;
#16976 = VECTOR ( 'NONE', #53859, 1000.000000000000000 ) ;
#16977 = CARTESIAN_POINT ( 'NONE',  ( 44.50000000000000000, 99.99999999999992895, 4.000000000000000000 ) ) ;
#16978 = DIRECTION ( 'NONE',  ( 0.000000000000000000, 0.000000000000000000, 1.000000000000000000 ) ) ;
#16979 = ORIENTED_EDGE ( 'NONE', *, *, #23147, .T. ) ;
#16980 = CARTESIAN_POINT ( 'NONE',  ( -9.827790563157511022E-16, 152.5570736234661524, 8.025000000000000355 ) ) ;
#16981 = VECTOR ( 'NONE', #63951, 1000.000000000000114 ) ;
#16982 = DIRECTION ( 'NONE',  ( 0.000000000000000000, 0.000000000000000000, -1.000000000000000000 ) ) ;
#16983 = CARTESIAN_POINT ( 'NONE',  ( -89.00499999999999545, 6.826472737025116366, 4.959722759717898555 ) ) ;
#16984 = EDGE_LOOP ( 'NONE', ( #34396, #63384, #61896, #50595, #30668 ) ) ;
#16985 = UNCERTAINTY_MEASURE_WITH_UNIT (LENGTH_MEASURE( 1.000000000000000082E-05 ), #41478, 'distance_accuracy_value', 'NONE');
#16986 = SURFACE_SIDE_STYLE ('',( #44097 ) ) ;
#16987 = CIRCLE ( 'NONE', #38343, 7.000000000000000888 ) ;
#16988 = FILL_AREA_STYLE ('',( #22243 ) ) ;
#16989 =( LENGTH_UNIT ( ) NAMED_UNIT ( * ) SI_UNIT ( .MILLI., .METRE. ) );
#16990 = CARTESIAN_POINT ( 'NONE',  ( -64.70707362346617231, -3.094860106618431139, -9.524999999999991473 ) ) ;
#16991 = AXIS2_PLACEMENT_3D ( 'NONE', #53750, #12560, #38672 ) ;
#16992 = SURFACE_STYLE_FILL_AREA ( #53239 ) ;
#16993 = ORIENTED_EDGE ( 'NONE', *, *, #51484, .T. ) ;
#16994 = DIRECTION ( 'NONE',  ( 0.000000000000000000, 0.000000000000000000, 1.000000000000000000 ) ) ;
#16995 =( GEOMETRIC_REPRESENTATION_CONTEXT ( 3 ) GLOBAL_UNCERTAINTY_ASSIGNED_CONTEXT ( ( #41244 ) ) GLOBAL_UNIT_ASSIGNED_CONTEXT ( ( #12569, #27096, #54193 ) ) REPRESENTATION_CONTEXT ( 'NONE', 'WORKASPACE' ) );
#16996 = CARTESIAN_POINT ( 'NONE',  ( -106.4049999999999727, -2.607480562269069768, 8.024999999999991473 ) ) ;
#16997 = CARTESIAN_POINT ( 'NONE',  ( 5.598654528085805993, 132.2450000000000045, 7.705886871421374629 ) ) ;
#16998 = CARTESIAN_POINT ( 'NONE',  ( -116.0949999999999704, -2.607480562269071545, -8.024999999999991473 ) ) ;
#16999 =( GEOMETRIC_REPRESENTATION_CONTEXT ( 3 ) GLOBAL_UNCERTAINTY_ASSIGNED_CONTEXT ( ( #21495 ) ) GLOBAL_UNIT_ASSIGNED_CONTEXT ( ( #20676, #36187, #52001 ) ) REPRESENTATION_CONTEXT ( 'NONE', 'WORKASPACE' ) );
#17000 =( NAMED_UNIT ( * ) SI_UNIT ( $, .STERADIAN. ) SOLID_ANGLE_UNIT ( ) );
#17001 = B_SPLINE_CURVE_WITH_KNOTS ( 'NONE', 3,
 ( #39395, #1320, #60453, #12968, #56217, #66437, #12258, #33725 ),
 .UNSPECIFIED., .F., .F.,
 ( 4, 2, 2, 4 ),
 ( 0.01337289451763051980, 0.01607096743472092790, 0.01742000389326613108, 0.01876904035181133773 ),
 .UNSPECIFIED. ) ;
#17002 = CARTESIAN_POINT ( 'NONE',  ( 6.999798566743339556, 49.77026365512251971, 7.251305755767526229 ) ) ;
#17004 = DIRECTION ( 'NONE',  ( 1.000000000000000000, 4.336808689941999001E-16, 0.000000000000000000 ) ) ;
#17003 = CARTESIAN_POINT ( 'NONE',  ( -33.73135404569435281, -9.688118915736252390, -3.017821087819916315 ) ) ;
#17005 = CARTESIAN_POINT ( 'NONE',  ( -153.4429263765338192, -1.166476076187852838E-15, -9.524999999999991473 ) ) ;
#17006 =( NAMED_UNIT ( * ) PLANE_ANGLE_UNIT ( ) SI_UNIT ( $, .RADIAN. ) );
#17007 = MECHANICAL_DESIGN_GEOMETRIC_PRESENTATION_REPRESENTATION (  '', ( #38380 ), #55024 ) ;
#17008 = CARTESIAN_POINT ( 'NONE',  ( -178.9449999999999932, -9.827790563157499189E-16, -8.024999999999991473 ) ) ;
#17009 = B_SPLINE_CURVE_WITH_KNOTS ( 'NONE', 3,
 ( #30223, #51716, #24273, #29905 ),
 .UNSPECIFIED., .F., .F.,
 ( 4, 4 ),
 ( -4.944132332486997984E-06, 0.0004171697701591836637 ),
 .UNSPECIFIED. ) ;
#17010 = CARTESIAN_POINT ( 'NONE',  ( -60.00000000000000000, -2.024042244987997205E-14, 6.500000000000000000 ) ) ;
#17011 = EDGE_CURVE ( 'NONE', #69035, #54309, #17117, .T. ) ;
#17012 = CARTESIAN_POINT ( 'NONE',  ( -46.49706195760896321, -11.95311037025569867, 3.244122449748929160 ) ) ;
#17013 = VERTEX_POINT ( 'NONE', #27256 ) ;
#17014 = DIRECTION ( 'NONE',  ( 1.000000000000000000, -0.000000000000000000, -1.300977106640434891E-16 ) ) ;
#17015 = FACE_OUTER_BOUND ( 'NONE', #18722, .T. ) ;
#17016 = ORIENTED_EDGE ( 'NONE', *, *, #25959, .F. ) ;
#17017 = MECHANICAL_DESIGN_GEOMETRIC_PRESENTATION_REPRESENTATION (  '', ( #23721 ), #42908 ) ;
#17018 = CARTESIAN_POINT ( 'NONE',  ( -66.29292637653381348, 3.094860106618428031, -9.524999999999993250 ) ) ;
#17020 = ADVANCED_FACE ( 'NONE', ( #54359 ), #27943, .T. ) ;
#17019 = CARTESIAN_POINT ( 'NONE',  ( 71.50000000000000000, 35.92875272052971525, 7.500000000000000000 ) ) ;
#17021 = SURFACE_SIDE_STYLE ('',( #21943 ) ) ;
#17022 = EDGE_CURVE ( 'NONE', #37089, #48904, #63016, .T. ) ;
#17023 =( GEOMETRIC_REPRESENTATION_CONTEXT ( 3 ) GLOBAL_UNCERTAINTY_ASSIGNED_CONTEXT ( ( #15702 ) ) GLOBAL_UNIT_ASSIGNED_CONTEXT ( ( #60862, #4089, #40489 ) ) REPRESENTATION_CONTEXT ( 'NONE', 'WORKASPACE' ) );
#17024 =( GEOMETRIC_REPRESENTATION_CONTEXT ( 3 ) GLOBAL_UNCERTAINTY_ASSIGNED_CONTEXT ( ( #51750 ) ) GLOBAL_UNIT_ASSIGNED_CONTEXT ( ( #28277, #21649, #23050 ) ) REPRESENTATION_CONTEXT ( 'NONE', 'WORKASPACE' ) );
#17025 = DIRECTION ( 'NONE',  ( 0.000000000000000000, 0.000000000000000000, 1.000000000000000000 ) ) ;
#17026 = CARTESIAN_POINT ( 'NONE',  ( -142.4929263765338590, -8.102448949553174629, 5.886773742842742685 ) ) ;
#17027 = DIRECTION ( 'NONE',  ( 1.000000000000000000, -1.387778780781444256E-14, 0.000000000000000000 ) ) ;
#17028 = EDGE_CURVE ( 'NONE', #2194, #51098, #65616, .T. ) ;
#17030 = CIRCLE ( 'NONE', #12511, 0.5000000000000004441 ) ;
#17029 = DIRECTION ( 'NONE',  ( -1.000000000000000000, 0.000000000000000000, 0.000000000000000000 ) ) ;
#17031 = ORIENTED_EDGE ( 'NONE', *, *, #39057, .T. ) ;
#17032 = CARTESIAN_POINT ( 'NONE',  ( -172.7049999999999841, 2.607480562269072433, 8.024999999999991473 ) ) ;
#17033 = ADVANCED_FACE ( 'NONE', ( #6177 ), #1176, .F. ) ;
#17034 = ORIENTED_EDGE ( 'NONE', *, *, #34232, .F. ) ;
#17035 = SURFACE_STYLE_FILL_AREA ( #50405 ) ;
#17036 = STYLED_ITEM ( 'NONE', ( #54453 ), #22097 ) ;
#17037 = EDGE_CURVE ( 'NONE', #28244, #66508, #12443, .T. ) ;
#17038 = CARTESIAN_POINT ( 'NONE',  ( -127.1070736234661780, 8.102448949553172852, -5.886773742842744461 ) ) ;
#17039 = DIRECTION ( 'NONE',  ( 0.000000000000000000, 0.000000000000000000, 1.000000000000000000 ) ) ;
#17040 = AXIS2_PLACEMENT_3D ( 'NONE', #63126, #30754, #31800 ) ;
#17041 = DIRECTION ( 'NONE',  ( 0.000000000000000000, 0.000000000000000000, 1.000000000000000000 ) ) ;
#17042 = CARTESIAN_POINT ( 'NONE',  ( -2.607480562269075097, 152.4070736234661751, 8.025000000000000355 ) ) ;
#17043 =( GEOMETRIC_REPRESENTATION_CONTEXT ( 3 ) GLOBAL_UNCERTAINTY_ASSIGNED_CONTEXT ( ( #56700 ) ) GLOBAL_UNIT_ASSIGNED_CONTEXT ( ( #65621, #60332, #65267 ) ) REPRESENTATION_CONTEXT ( 'NONE', 'WORKASPACE' ) );
#17044 = VERTEX_POINT ( 'NONE', #7563 ) ;
#17046 = EDGE_CURVE ( 'NONE', #26176, #60543, #13882, .T. ) ;
#17045 = FILL_AREA_STYLE ('',( #55331 ) ) ;
#17047 = CARTESIAN_POINT ( 'NONE',  ( -83.15499999999998693, 7.632228543268600340, 2.479861379858949277 ) ) ;
#17048 = DIRECTION ( 'NONE',  ( 0.000000000000000000, -1.000000000000000000, 0.000000000000000000 ) ) ;
#17049 = CARTESIAN_POINT ( 'NONE',  ( -92.30707362346618083, -10.01517768586948698, 6.132527647946031529E-16 ) ) ;
#17050 = CARTESIAN_POINT ( 'NONE',  ( -168.7429263765338305, -5.598654528085803328, -7.705886871421366635 ) ) ;
#17051 = DIRECTION ( 'NONE',  ( -0.000000000000000000, 1.000000000000000000, -0.000000000000000000 ) ) ;
#17052 = DIRECTION ( 'NONE',  ( 1.000000000000000000, 0.000000000000000000, 0.000000000000000000 ) ) ;
#17053 = SURFACE_STYLE_USAGE ( .BOTH. , #10712 ) ;
#17054 = EDGE_LOOP ( 'NONE', ( #31536, #68946, #59272, #7200 ) ) ;
#17055 = CARTESIAN_POINT ( 'NONE',  ( 16.75000000000000711, 25.24999999999998224, -3.750000000000000000 ) ) ;
#17056 = SURFACE_SIDE_STYLE ('',( #65908 ) ) ;
#17057 = CARTESIAN_POINT ( 'NONE',  ( -62.39499999999998181, -6.826472737025115478, -4.959722759717899443 ) ) ;
#17058 = ORIENTED_EDGE ( 'NONE', *, *, #33793, .T. ) ;
#17059 = MECHANICAL_DESIGN_GEOMETRIC_PRESENTATION_REPRESENTATION (  '', ( #38422 ), #37265 ) ;
#17060 =( NAMED_UNIT ( * ) SI_UNIT ( $, .STERADIAN. ) SOLID_ANGLE_UNIT ( ) );
#17061 = DIRECTION ( 'NONE',  ( -0.000000000000000000, -0.000000000000000000, -1.000000000000000000 ) ) ;
#17062 = CARTESIAN_POINT ( 'NONE',  ( -45.76717108624533381, 8.859195963244948402, -6.389740745940694744 ) ) ;
#17063 = VERTEX_POINT ( 'NONE', #3272 ) ;
#17064 = FACE_OUTER_BOUND ( 'NONE', #69456, .T. ) ;
#17065 = EDGE_LOOP ( 'NONE', ( #55593, #8742, #51272 ) ) ;
#17066 = PRESENTATION_LAYER_ASSIGNMENT (  '', '', ( #30464 ) ) ;
#17067 = CARTESIAN_POINT ( 'NONE',  ( 68.99999999999998579, 8.450062914116736267E-15, 3.000000000000000000 ) ) ;
#17068 = LINE ( 'NONE', #53963, #67376 ) ;
#17069 = CARTESIAN_POINT ( 'NONE',  ( -115.1049999999999756, -6.826472737025115478, 4.959722759717900331 ) ) ;
#17070 = ORIENTED_EDGE ( 'NONE', *, *, #33222, .F. ) ;
#17071 = CARTESIAN_POINT ( 'NONE',  ( 4.041451884327375232, 1.417096231345241097, -7.000000000000002665 ) ) ;
#17072 = CARTESIAN_POINT ( 'NONE',  ( -72.74292637653380211, -5.598654528085803328, -7.705886871421366635 ) ) ;
#17073 = CYLINDRICAL_SURFACE ( 'NONE', #57175, 0.5000000000000004441 ) ;
#17074 = SURFACE_SIDE_STYLE ('',( #59946 ) ) ;
#17075 =( LENGTH_UNIT ( ) NAMED_UNIT ( * ) SI_UNIT ( .MILLI., .METRE. ) );
#17076 = CARTESIAN_POINT ( 'NONE',  ( -148.5570736234661808, -1.166476076187852838E-15, -9.524999999999991473 ) ) ;
#17077 = AXIS2_PLACEMENT_3D ( 'NONE', #15472, #20727, #25299 ) ;
#17078 = CARTESIAN_POINT ( 'NONE',  ( 5.598654528085805993, 132.2450000000000045, 7.705886871421374629 ) ) ;
#17079 = CARTESIAN_POINT ( 'NONE',  ( -95.90707362346618936, -3.094860106618429807, 9.524999999999991473 ) ) ;
#17080 = EDGE_CURVE ( 'NONE', #7834, #65093, #40557, .T. ) ;
#17081 = VECTOR ( 'NONE', #24406, 1000.000000000000000 ) ;
#17082 = DIRECTION ( 'NONE',  ( -1.000000000000000000, 0.000000000000000000, 0.000000000000000000 ) ) ;
#17083 = PRODUCT_DEFINITION_SHAPE ( 'NONE', 'NONE',  #69704 ) ;
#17084 = ORIENTED_EDGE ( 'NONE', *, *, #42233, .F. ) ;
#17085 = CIRCLE ( 'NONE', #56351, 0.5000000000000004441 ) ;
#17088 =( GEOMETRIC_REPRESENTATION_CONTEXT ( 3 ) GLOBAL_UNCERTAINTY_ASSIGNED_CONTEXT ( ( #13057 ) ) GLOBAL_UNIT_ASSIGNED_CONTEXT ( ( #23975, #3514, #51074 ) ) REPRESENTATION_CONTEXT ( 'NONE', 'WORKASPACE' ) );
#17087 = FACE_BOUND ( 'NONE', #52153, .T. ) ;
#17086 = CARTESIAN_POINT ( 'NONE',  ( -4.750000000000002665, 22.24999999999998579, -4.000000000000000000 ) ) ;
#17089 = CARTESIAN_POINT ( 'NONE',  ( -15.98999599679679839, 147.4999999999999716, 10.00000000000000000 ) ) ;
#17090 = CARTESIAN_POINT ( 'NONE',  ( -132.5049999999999670, -6.826472737025115478, -4.959722759717899443 ) ) ;
#17091 = CARTESIAN_POINT ( 'NONE',  ( -22.75000000000000711, 36.75000000000000000, -3.750000000000000000 ) ) ;
#17092 = CARTESIAN_POINT ( 'NONE',  ( -146.5429263765338135, 9.058813317711329915, 2.943386871421369566 ) ) ;
#17093 = CARTESIAN_POINT ( 'NONE',  ( -140.5450000000000159, -7.632228543268600340, -2.479861379858950166 ) ) ;
#17094 = CARTESIAN_POINT ( 'NONE',  ( -128.3949999999999534, -6.826472737025113702, -4.959722759717900331 ) ) ;
#17095 = COLOUR_RGB ( '', 0.72549020, 0.75294118, 0.79215686) ;
#17096 = EDGE_LOOP ( 'NONE', ( #9023, #54994, #67940, #43626 ) ) ;
#17097 = CARTESIAN_POINT ( 'NONE',  ( -123.4429263765338192, -1.166476076187852838E-15, -9.524999999999991473 ) ) ;
#17098 = VECTOR ( 'NONE', #51371, 1000.000000000000000 ) ;
#17099 = FACE_OUTER_BOUND ( 'NONE', #17348, .T. ) ;
#17100 = DIRECTION ( 'NONE',  ( 0.000000000000000000, 0.000000000000000000, 1.000000000000000000 ) ) ;
#17101 = UNCERTAINTY_MEASURE_WITH_UNIT (LENGTH_MEASURE( 1.000000000000000082E-05 ), #62400, 'distance_accuracy_value', 'NONE');
#17102 = CARTESIAN_POINT ( 'NONE',  ( -183.2929263765338135, 3.094860106618428031, -9.524999999999993250 ) ) ;
#17103 = VECTOR ( 'NONE', #14479, 1000.000000000000000 ) ;
#17104 = CARTESIAN_POINT ( 'NONE',  ( -55.79499999999998039, 2.607480562269068880, -8.024999999999993250 ) ) ;
#17105 = AXIS2_PLACEMENT_3D ( 'NONE', #41130, #67839, #30875 ) ;
#17106 = ADVANCED_FACE ( 'NONE', ( #29717 ), #8272, .F. ) ;
#17107 = CARTESIAN_POINT ( 'NONE',  ( -139.4929263765338021, -8.102448949553174629, 5.886773742842742685 ) ) ;
#17108 = DIRECTION ( 'NONE',  ( 0.000000000000000000, 0.000000000000000000, 1.000000000000000000 ) ) ;
#17109 = DIRECTION ( 'NONE',  ( 0.000000000000000000, 0.000000000000000000, -1.000000000000000000 ) ) ;
#17110 = PRESENTATION_LAYER_ASSIGNMENT (  '', '', ( #54175 ) ) ;
#17111 = CARTESIAN_POINT ( 'NONE',  ( 34.99999999999999289, 99.99999999999997158, -9.500000000000000000 ) ) ;
#17112 = CARTESIAN_POINT ( 'NONE',  ( -75.80707362346616662, 10.01517768586948698, -1.839758294383808966E-15 ) ) ;
#17113 = CARTESIAN_POINT ( 'NONE',  ( -106.4929263765338163, -8.102448949553172852, 5.886773742842742685 ) ) ;
#17114 = DIRECTION ( 'NONE',  ( -1.000000000000000000, -5.775339657480442461E-17, 4.528264053928433241E-17 ) ) ;
#17116 = EDGE_CURVE ( 'NONE', #24476, #22828, #18479, .T. ) ;
#17115 = CARTESIAN_POINT ( 'NONE',  ( -84.49999999999998579, -3.499999999999999556, 24.00000000000000000 ) ) ;
#17117 = LINE ( 'NONE', #54010, #52901 ) ;
#17118 = STYLED_ITEM ( 'NONE', ( #46608 ), #25726 ) ;
#17119 = SURFACE_STYLE_USAGE ( .BOTH. , #38929 ) ;
#17120 = PRESENTATION_STYLE_ASSIGNMENT (( #50488 ) ) ;
#17121 = VERTEX_POINT ( 'NONE', #12835 ) ;
#17122 = CARTESIAN_POINT ( 'NONE',  ( 6.000000000000017764, -0.1486183402614471571, 18.42691897641805099 ) ) ;
#17123 = EDGE_CURVE ( 'NONE', #24951, #12385, #30457, .T. ) ;
#17124 = CARTESIAN_POINT ( 'NONE',  ( -74.99999999999998579, 50.00000000000000000, 11.50000000000003730 ) ) ;
#17125 = VERTEX_POINT ( 'NONE', #25129 ) ;
#17126 = FILL_AREA_STYLE_COLOUR ( '', #66748 ) ;
#17127 = STYLED_ITEM ( 'NONE', ( #56885 ), #60819 ) ;
#17128 = CARTESIAN_POINT ( 'NONE',  ( 7.632228543268607446, 123.1570736234661609, 2.479861379858954606 ) ) ;
#17129 = CIRCLE ( 'NONE', #54142, 17.42000000000001236 ) ;
#17131 = EDGE_CURVE ( 'NONE', #60346, #29727, #3472, .T. ) ;
#17130 = DIRECTION ( 'NONE',  ( 0.000000000000000000, 1.000000000000000000, 0.000000000000000000 ) ) ;
#17132 = DIRECTION ( 'NONE',  ( 1.000000000000000000, -0.000000000000000000, 0.000000000000000000 ) ) ;
#17133 = VERTEX_POINT ( 'NONE', #18125 ) ;
#17134 = ORIENTED_EDGE ( 'NONE', *, *, #60236, .F. ) ;
#17135 = CARTESIAN_POINT ( 'NONE',  ( -116.4570736234661723, -9.058813317711329915, 2.943386871421371787 ) ) ;
#17136 = VERTEX_POINT ( 'NONE', #40640 ) ;
#17137 = LINE ( 'NONE', #64931, #68174 ) ;
#17138 = STYLED_ITEM ( 'NONE', ( #47806 ), #35600 ) ;
#17139 = CARTESIAN_POINT ( 'NONE',  ( 4.716976649647099507, 134.6429263765338362, -6.492361379858953008 ) ) ;
#17140 = CARTESIAN_POINT ( 'NONE',  ( -91.79500000000000171, 2.607480562269068880, -8.024999999999993250 ) ) ;
#17141 = ORIENTED_EDGE ( 'NONE', *, *, #39438, .T. ) ;
#17142 = MECHANICAL_DESIGN_GEOMETRIC_PRESENTATION_REPRESENTATION (  '', ( #44128 ), #29448 ) ;
#17143 = CARTESIAN_POINT ( 'NONE',  ( -2.607480562269095969, 124.2929263765338135, 8.024999999999986144 ) ) ;
#17144 = DIRECTION ( 'NONE',  ( 0.000000000000000000, 0.000000000000000000, -1.000000000000000000 ) ) ;
#17145 = FACE_OUTER_BOUND ( 'NONE', #52666, .T. ) ;
#17146 = ORIENTED_EDGE ( 'NONE', *, *, #15680, .F. ) ;
#17147 = DIRECTION ( 'NONE',  ( -0.000000000000000000, -0.000000000000000000, 1.000000000000000000 ) ) ;
#17148 =( GEOMETRIC_REPRESENTATION_CONTEXT ( 3 ) GLOBAL_UNCERTAINTY_ASSIGNED_CONTEXT ( ( #45535 ) ) GLOBAL_UNIT_ASSIGNED_CONTEXT ( ( #64110, #44100, #54917 ) ) REPRESENTATION_CONTEXT ( 'NONE', 'WORKASPACE' ) );
#17149 = CARTESIAN_POINT ( 'NONE',  ( 6.021969435454494146, 1.863712308906143589, -7.569642976165943615 ) ) ;
#17150 = ORIENTED_EDGE ( 'NONE', *, *, #20745, .F. ) ;
#17151 = COLOUR_RGB ( '', 0.08235294, 0.09019608, 0.10196078) ;
#17152 = CARTESIAN_POINT ( 'NONE',  ( -7.440601873764705054, 2.005109422339667269, -1.112499515747341183 ) ) ;
#17153 = ORIENTED_EDGE ( 'NONE', *, *, #33836, .F. ) ;
#17154 = SURFACE_STYLE_USAGE ( .BOTH. , #32586 ) ;
#17155 = DIRECTION ( 'NONE',  ( 0.000000000000000000, -0.000000000000000000, -1.000000000000000000 ) ) ;
#17156 = DIRECTION ( 'NONE',  ( -1.000000000000000000, 0.000000000000000000, -0.000000000000000000 ) ) ;
#17157 = PRESENTATION_STYLE_ASSIGNMENT (( #16807 ) ) ;
#17158 = CARTESIAN_POINT ( 'NONE',  ( -175.4070736234662036, 3.094860106618428031, -9.524999999999993250 ) ) ;
#17159 = DIRECTION ( 'NONE',  ( 1.000000000000000000, 0.000000000000000000, 0.000000000000000000 ) ) ;
#17160 = ADVANCED_FACE ( 'NONE', ( #13174, #45236 ), #18804, .T. ) ;
#17161 =( GEOMETRIC_REPRESENTATION_CONTEXT ( 3 ) GLOBAL_UNCERTAINTY_ASSIGNED_CONTEXT ( ( #1816 ) ) GLOBAL_UNIT_ASSIGNED_CONTEXT ( ( #38811, #712, #59163 ) ) REPRESENTATION_CONTEXT ( 'NONE', 'WORKASPACE' ) );
#17162 = FACE_OUTER_BOUND ( 'NONE', #54825, .T. ) ;
#17163 = CARTESIAN_POINT ( 'NONE',  ( -115.7929263765346519, -3.094860106604043981, 9.525000000010443557 ) ) ;
#17164 = ORIENTED_EDGE ( 'NONE', *, *, #24946, .T. ) ;
#17165 = CARTESIAN_POINT ( 'NONE',  ( -48.95707362346615810, 9.058813317711329915, -2.943386871421373119 ) ) ;
#17166 = DIRECTION ( 'NONE',  ( -0.000000000000000000, -0.000000000000000000, 1.000000000000000000 ) ) ;
#17167 = SURFACE_STYLE_FILL_AREA ( #37952 ) ;
#17168 = ORIENTED_EDGE ( 'NONE', *, *, #23555, .T. ) ;
#17169 = DIRECTION ( 'NONE',  ( 0.000000000000000000, 0.000000000000000000, 1.000000000000000000 ) ) ;
#17170 = CARTESIAN_POINT ( 'NONE',  ( -158.0049999999999955, 6.826472737025116366, 4.959722759717898555 ) ) ;
#17171 = DIRECTION ( 'NONE',  ( 0.000000000000000000, 0.000000000000000000, -1.000000000000000000 ) ) ;
#17172 = CARTESIAN_POINT ( 'NONE',  ( -74.99999999999998579, 50.00000000000000000, 11.50000000000000000 ) ) ;
#17173 = CARTESIAN_POINT ( 'NONE',  ( -170.2450000000000045, -4.716976649647093289, -6.492361379858945902 ) ) ;
#17174 =( GEOMETRIC_REPRESENTATION_CONTEXT ( 3 ) GLOBAL_UNCERTAINTY_ASSIGNED_CONTEXT ( ( #36835 ) ) GLOBAL_UNIT_ASSIGNED_CONTEXT ( ( #38466, #28527, #65842 ) ) REPRESENTATION_CONTEXT ( 'NONE', 'WORKASPACE' ) );
#17175 = TOROIDAL_SURFACE ( 'NONE', #44159, 1.000000000000000000, 0.5000000000000000000 ) ;
#17176 = CARTESIAN_POINT ( 'NONE',  ( -158.6949999999999648, -8.437984349512086979, 5.166775262442717831E-16 ) ) ;
#17177 = ORIENTED_EDGE ( 'NONE', *, *, #67014, .F. ) ;
#17178 = CARTESIAN_POINT ( 'NONE',  ( -88.94292637653380496, 0.000000000000000000, 9.524999999999991473 ) ) ;
#17179 = PRESENTATION_LAYER_ASSIGNMENT (  '', '', ( #47532 ) ) ;
#17180 = EDGE_CURVE ( 'NONE', #14431, #7659, #56334, .T. ) ;
#17181 = CARTESIAN_POINT ( 'NONE',  ( 45.43546989188912022, 10.14515663062970496, 3.347022959407293996 ) ) ;
#17182 = CARTESIAN_POINT ( 'NONE',  ( -69.50499999999996703, -6.826472737025115478, -4.959722759717899443 ) ) ;
#17183 = CARTESIAN_POINT ( 'NONE',  ( 24.16082825257855760, 24.77175885999242766, 27.27794882343791372 ) ) ;
#17184 = AXIS2_PLACEMENT_3D ( 'NONE', #51131, #24368, #45862 ) ;
#17185 = CARTESIAN_POINT ( 'NONE',  ( -83.99999999999997158, 50.00000000000000000, 12.00000000000000000 ) ) ;
#17186 = ADVANCED_FACE ( 'NONE', ( #19495 ), #56092, .T. ) ;
#17187 = CARTESIAN_POINT ( 'NONE',  ( -84.89499999999996760, 6.826472737025115478, 4.959722759717899443 ) ) ;
#17188 = CLOSED_SHELL ( 'NONE', ( #44217, #27677, #54164, #37972, #14239, #60821, #21697, #28663, #40713, #58934, #17525, #15377, #59104, #3022, #2136, #15937, #43512, #37152, #38893, #67997, #61565, #13644, #66117, #57677, #27696, #419, #4319, #4036, #22392, #53624, #58080, #53764, #14257, #20014, #54550, #18552, #21049, #932, #20492, #7475, #65664, #20405, #20158, #57989, #42460, #59234, #41928, #32959, #54781, #35533, #49345, #18685, #41332, #51610, #35929, #66030, #44309, #62107, #47472, #18525, #19885, #44137, #59968, #22778, #17020, #59300, #26809, #59222, #55436, #53527, #16771, #39221, #55261, #61476, #6504, #15860, #4698, #27071, #3870, #67889, #14620, #2234, #5878, #10960, #11913, #30137, #68741, #51235, #50060, #36423, #11820, #54077, #22092, #38106, #23491, #25303, #8516, #34088, #7946, #59701, #38976, #11838, #52447, #29381, #56313, #18762, #21973, #35350, #13263, #51556, #27680, #40333, #52833, #38017, #41092, #11107, #19457, #65694, #4824, #68642, #53074, #68384, #6838, #34783, #30880, #46052, #10800, #58049, #43727, #55937, #66082, #58693, #37310, #41748, #28882, #13257, #47421, #45405, #20815, #16213, #18022, #43979, #11190, #23367, #14612, #5711, #55496, #36430, #34686, #37550, #32239, #30391, #585, #11561, #68084, #19123, #7696, #45008 ) ) ;
#17189 = EDGE_CURVE ( 'NONE', #30575, #3787, #20198, .T. ) ;
#17190 = CARTESIAN_POINT ( 'NONE',  ( -3.094860106618432471, 140.7049999999999557, -9.525000000000000355 ) ) ;
#17191 = AXIS2_PLACEMENT_3D ( 'NONE', #16615, #15242, #32074 ) ;
#17192 =( LENGTH_UNIT ( ) NAMED_UNIT ( * ) SI_UNIT ( .MILLI., .METRE. ) );
#17193 = PRESENTATION_LAYER_ASSIGNMENT (  '', '', ( #8183 ) ) ;
#17194 = CARTESIAN_POINT ( 'NONE',  ( -176.3929263765338078, 8.102448949553176405, 5.886773742842740909 ) ) ;
#17195 = UNCERTAINTY_MEASURE_WITH_UNIT (LENGTH_MEASURE( 1.000000000000000082E-05 ), #35580, 'distance_accuracy_value', 'NONE');
#17196 = COLOUR_RGB ( '', 0.72549020, 0.75294118, 0.79215686) ;
#17197 = DIRECTION ( 'NONE',  ( 0.000000000000000000, 0.000000000000000000, -1.000000000000000000 ) ) ;
#17198 = FACE_OUTER_BOUND ( 'NONE', #45333, .T. ) ;
#17199 = ORIENTED_EDGE ( 'NONE', *, *, #50209, .F. ) ;
#17200 = EDGE_CURVE ( 'NONE', #18031, #443, #62744, .T. ) ;
#17201 = FILL_AREA_STYLE_COLOUR ( '', #68494 ) ;
#17202 = CARTESIAN_POINT ( 'NONE',  ( -74.99999999999998579, 64.49137674618943095, -6.500000000000000888 ) ) ;
#17203 = EDGE_CURVE ( 'NONE', #35681, #47180, #39507, .T. ) ;
#17204 =( GEOMETRIC_REPRESENTATION_CONTEXT ( 3 ) GLOBAL_UNCERTAINTY_ASSIGNED_CONTEXT ( ( #24119 ) ) GLOBAL_UNIT_ASSIGNED_CONTEXT ( ( #20669, #15416, #58986 ) ) REPRESENTATION_CONTEXT ( 'NONE', 'WORKASPACE' ) );
#17205 = AXIS2_PLACEMENT_3D ( 'NONE', #69653, #6317, #38391 ) ;
#17206 = PLANE ( 'NONE',  #23688 ) ;
#17207 = CONICAL_SURFACE ( 'NONE', #62093, 5.000000000000004441, 0.7853981633974587151 ) ;
#17208 = SURFACE_STYLE_USAGE ( .BOTH. , #53432 ) ;
#17209 = EDGE_CURVE ( 'NONE', #54091, #25430, #25468, .T. ) ;
#17210 = ORIENTED_EDGE ( 'NONE', *, *, #61855, .T. ) ;
#17211 = EDGE_LOOP ( 'NONE', ( #46151, #57627, #32751, #20659, #23873, #17640, #13996, #53141, #42657, #53293 ) ) ;
#17212 = DIRECTION ( 'NONE',  ( 0.000000000000000000, 0.000000000000000000, 1.000000000000000000 ) ) ;
#17213 = PRESENTATION_LAYER_ASSIGNMENT (  '', '', ( #9366 ) ) ;
#17214 = EDGE_CURVE ( 'NONE', #49204, #33857, #31579, .T. ) ;
#17215 = FILL_AREA_STYLE ('',( #65367 ) ) ;
#17216 = DIRECTION ( 'NONE',  ( -0.000000000000000000, -1.000000000000000000, -0.000000000000000000 ) ) ;
#17217 = DIRECTION ( 'NONE',  ( 0.000000000000000000, 0.000000000000000000, -1.000000000000000000 ) ) ;
#17218 = ORIENTED_EDGE ( 'NONE', *, *, #17037, .F. ) ;
#17219 = CARTESIAN_POINT ( 'NONE',  ( -113.7549999999999955, 4.716976649647091513, -6.492361379858946790 ) ) ;
#17220 = VERTEX_POINT ( 'NONE', #53270 ) ;
#17221 = DIRECTION ( 'NONE',  ( 0.000000000000000000, 0.000000000000000000, -1.000000000000000000 ) ) ;
#17222 = VERTEX_POINT ( 'NONE', #46982 ) ;
#17223 = DIRECTION ( 'NONE',  ( -0.000000000000000000, 1.000000000000000000, -0.000000000000000000 ) ) ;
#17224 = ORIENTED_EDGE ( 'NONE', *, *, #51949, .F. ) ;
#17225 = AXIS2_PLACEMENT_3D ( 'NONE', #36563, #36891, #30512 ) ;
#17226 = STYLED_ITEM ( 'NONE', ( #68069 ), #61247 ) ;
#17227 =( NAMED_UNIT ( * ) SI_UNIT ( $, .STERADIAN. ) SOLID_ANGLE_UNIT ( ) );
#17228 = CARTESIAN_POINT ( 'NONE',  ( -1.166476076187854022E-15, 158.9449999999999932, 9.525000000000000355 ) ) ;
#17229 = DIRECTION ( 'NONE',  ( 1.000000000000000000, 0.000000000000000000, 0.000000000000000000 ) ) ;
#17230 = ORIENTED_EDGE ( 'NONE', *, *, #8144, .F. ) ;
#17231 = ORIENTED_EDGE ( 'NONE', *, *, #11988, .F. ) ;
#17232 = AXIS2_PLACEMENT_3D ( 'NONE', #14338, #57248, #51998 ) ;
#17233 = CARTESIAN_POINT ( 'NONE',  ( -117.5070736234661553, 8.102448949553176405, 5.886773742842740909 ) ) ;
#17234 =( NAMED_UNIT ( * ) SI_UNIT ( $, .STERADIAN. ) SOLID_ANGLE_UNIT ( ) );
#17235 = FILL_AREA_STYLE_COLOUR ( '', #46282 ) ;
#17236 = VERTEX_POINT ( 'NONE', #37118 ) ;
#17237 = CARTESIAN_POINT ( 'NONE',  ( 8.437984349512095861, 137.1929263765338192, 1.550032578732817026E-15 ) ) ;
#17238 = SPHERICAL_SURFACE ( 'NONE', #4212, 0.2500000000000000000 ) ;
#17239 = DIRECTION ( 'NONE',  ( 0.000000000000000000, 0.000000000000000000, -1.000000000000000000 ) ) ;
#17240 = CARTESIAN_POINT ( 'NONE',  ( 4.716976649647099507, 125.6429263765338220, -6.492361379858953008 ) ) ;
#17241 = CARTESIAN_POINT ( 'NONE',  ( -22.50000000000000711, 34.24999999999999289, 3.750000000000000000 ) ) ;
#17242 = ORIENTED_EDGE ( 'NONE', *, *, #68650, .T. ) ;
#17243 = MECHANICAL_DESIGN_GEOMETRIC_PRESENTATION_REPRESENTATION (  '', ( #40788 ), #57635 ) ;
#17244 =( LENGTH_UNIT ( ) NAMED_UNIT ( * ) SI_UNIT ( .MILLI., .METRE. ) );
#17245 = ORIENTED_EDGE ( 'NONE', *, *, #36499, .F. ) ;
#17246 = CARTESIAN_POINT ( 'NONE',  ( -52.64292637653380780, -5.598654528085801552, 7.705886871421367523 ) ) ;
#17247 = DIRECTION ( 'NONE',  ( -0.000000000000000000, 0.000000000000000000, -1.000000000000000000 ) ) ;
#17248 =( LENGTH_UNIT ( ) NAMED_UNIT ( * ) SI_UNIT ( .MILLI., .METRE. ) );
#17249 = SURFACE_STYLE_USAGE ( .BOTH. , #49580 ) ;
#17250 = CARTESIAN_POINT ( 'NONE',  ( -146.4550000000000125, 7.632228543268599452, -2.479861379858951942 ) ) ;
#17251 = AXIS2_PLACEMENT_3D ( 'NONE', #62613, #14429, #58390 ) ;
#17252 = CARTESIAN_POINT ( 'NONE',  ( -176.7570736234661695, -5.598654528085801552, 7.705886871421367523 ) ) ;
#17253 = SURFACE_STYLE_FILL_AREA ( #1673 ) ;
#17254 = UNCERTAINTY_MEASURE_WITH_UNIT (LENGTH_MEASURE( 1.000000000000000082E-05 ), #58853, 'distance_accuracy_value', 'NONE');
#17255 = VERTEX_POINT ( 'NONE', #63464 ) ;
#17256 = VECTOR ( 'NONE', #46497, 1000.000000000000000 ) ;
#17258 = CARTESIAN_POINT ( 'NONE',  ( 0.000000000000000000, 13.00000000000000178, 36.50000000000000000 ) ) ;
#17257 = STYLED_ITEM ( 'NONE', ( #33779 ), #30480 ) ;
#17259 = CARTESIAN_POINT ( 'NONE',  ( -45.00000000000000000, 8.554728201919928665, -6.928664365919924073 ) ) ;
#17260 = ORIENTED_EDGE ( 'NONE', *, *, #43114, .T. ) ;
#17261 = ORIENTED_EDGE ( 'NONE', *, *, #25892, .F. ) ;
#17262 = CARTESIAN_POINT ( 'NONE',  ( -45.13107125746175541, 8.257302774158723935, 3.517169940558448893 ) ) ;
#17263 = SURFACE_STYLE_FILL_AREA ( #22155 ) ;
#17264 = CARTESIAN_POINT ( 'NONE',  ( -58.85499999999998977, 4.716976649647094177, 6.492361379858945902 ) ) ;
#17265 = EDGE_LOOP ( 'NONE', ( #45547, #23103, #37917, #1269 ) ) ;
#17266 = CARTESIAN_POINT ( 'NONE',  ( 10.00000000000001776, 43.00000000000000000, -29.68999999999999417 ) ) ;
#17267 = CARTESIAN_POINT ( 'NONE',  ( -17.41059898028469277, 6.938893903907228378E-15, -12.50000000000000000 ) ) ;
#17268 = CARTESIAN_POINT ( 'NONE',  ( 5.196152422706628471, 1.107695154586738173, -9.000000000000005329 ) ) ;
#17269 = CARTESIAN_POINT ( 'NONE',  ( 0.000000000000000000, 87.30187232391182306, 0.000000000000000000 ) ) ;
#17270 = ORIENTED_EDGE ( 'NONE', *, *, #62719, .F. ) ;
#17271 = CIRCLE ( 'NONE', #7136, 8.500000000000007105 ) ;
#17272 = ADVANCED_FACE ( 'NONE', ( #69431 ), #31422, .F. ) ;
#17273 = CARTESIAN_POINT ( 'NONE',  ( -5.603568002170373319, 1.515110734050471919, -8.294335516573692502 ) ) ;
#17274 = CARTESIAN_POINT ( 'NONE',  ( -43.75000000000000000, 4.336808689942018722E-16, -5.099999999999999645 ) ) ;
#17275 =( NAMED_UNIT ( * ) SI_UNIT ( $, .STERADIAN. ) SOLID_ANGLE_UNIT ( ) );
#17276 = DIRECTION ( 'NONE',  ( -0.000000000000000000, 0.000000000000000000, 1.000000000000000000 ) ) ;
#17277 = EDGE_CURVE ( 'NONE', #29444, #65459, #66435, .T. ) ;
#17278 = EDGE_CURVE ( 'NONE', #35366, #68002, #11397, .T. ) ;
#17279 = CARTESIAN_POINT ( 'NONE',  ( -111.2949999999999733, -2.607480562269069768, 8.024999999999991473 ) ) ;
#17280 = CARTESIAN_POINT ( 'NONE',  ( -9.058813317711337021, 155.0449999999999875, -2.943386871421374895 ) ) ;
#17281 = CARTESIAN_POINT ( 'NONE',  ( -76.49500000000000455, 6.826472737025113702, -4.959722759717902107 ) ) ;
#17282 = CARTESIAN_POINT ( 'NONE',  ( -60.00000000000000000, -2.024042244987997205E-14, -7.500000000000000000 ) ) ;
#17283 = VECTOR ( 'NONE', #18573, 1000.000000000000000 ) ;
#17284 = DIRECTION ( 'NONE',  ( -0.000000000000000000, -0.000000000000000000, 1.000000000000000000 ) ) ;
#17285 = UNCERTAINTY_MEASURE_WITH_UNIT (LENGTH_MEASURE( 1.000000000000000082E-05 ), #37060, 'distance_accuracy_value', 'NONE');
#17286 = SURFACE_STYLE_FILL_AREA ( #49618 ) ;
#17287 = VERTEX_POINT ( 'NONE', #17379 ) ;
#17288 = STYLED_ITEM ( 'NONE', ( #23667 ), #2427 ) ;
#17289 = CARTESIAN_POINT ( 'NONE',  ( -124.6429263765338078, -5.598654528085801552, 7.705886871421367523 ) ) ;
#17290 = CARTESIAN_POINT ( 'NONE',  ( -148.9449999999999932, -9.827790563157499189E-16, -8.024999999999991473 ) ) ;
#17291 = EDGE_CURVE ( 'NONE', #9702, #17044, #22609, .T. ) ;
#17292 = CIRCLE ( 'NONE', #32979, 0.5000000000000004441 ) ;
#17293 = CARTESIAN_POINT ( 'NONE',  ( 0.000000000000000000, 24.74999999999998579, 3.750000000000000000 ) ) ;
#17294 = VERTEX_POINT ( 'NONE', #48358 ) ;
#17295 = ORIENTED_EDGE ( 'NONE', *, *, #3485, .F. ) ;
#17296 = AXIS2_PLACEMENT_3D ( 'NONE', #57615, #31558, #15762 ) ;
#17297 = DIRECTION ( 'NONE',  ( 0.000000000000000000, -1.000000000000000000, 0.000000000000000000 ) ) ;
#17298 =( NAMED_UNIT ( * ) PLANE_ANGLE_UNIT ( ) SI_UNIT ( $, .RADIAN. ) );
#17299 = AXIS2_PLACEMENT_3D ( 'NONE', #11137, #27296, #528 ) ;
#17300 = AXIS2_PLACEMENT_3D ( 'NONE', #588, #43607, #38330 ) ;
#17301 = DIRECTION ( 'NONE',  ( 0.000000000000000000, 0.000000000000000000, -1.000000000000000000 ) ) ;
#17302 = CARTESIAN_POINT ( 'NONE',  ( -195.0000000000000000, 0.000000000000000000, 0.000000000000000000 ) ) ;
#17303 = CARTESIAN_POINT ( 'NONE',  ( -9.000000000000007105, 0.000000000000000000, 0.000000000000000000 ) ) ;
#17304 = PRESENTATION_LAYER_ASSIGNMENT (  '', '', ( #42034 ) ) ;
#17305 = SURFACE_STYLE_USAGE ( .BOTH. , #671 ) ;
#17306 = ORIENTED_EDGE ( 'NONE', *, *, #30377, .T. ) ;
#17307 = CARTESIAN_POINT ( 'NONE',  ( -141.5049999999999955, -6.826472737025113702, -4.959722759717900331 ) ) ;
#17308 = VERTEX_POINT ( 'NONE', #54274 ) ;
#17309 = EDGE_CURVE ( 'NONE', #31359, #52155, #61910, .T. ) ;
#17310 = VERTEX_POINT ( 'NONE', #48711 ) ;
#17311 = VERTEX_POINT ( 'NONE', #37820 ) ;
#17312 = VECTOR ( 'NONE', #9167, 1000.000000000000000 ) ;
#17313 = CARTESIAN_POINT ( 'NONE',  ( -56.65976306744538959, -7.924810552015186360, -1.308190166797568166 ) ) ;
#17314 = ADVANCED_FACE ( 'NONE', ( #48 ), #64171, .F. ) ;
#17315 = CARTESIAN_POINT ( 'NONE',  ( -3.094860106618434248, 128.7949999999999875, 9.525000000000000355 ) ) ;
#17316 = CARTESIAN_POINT ( 'NONE',  ( 28.00000000000000000, 43.00000000000000000, -90.00000000000000000 ) ) ;
#17317 = EDGE_LOOP ( 'NONE', ( #36447, #9765 ) ) ;
#17318 = VECTOR ( 'NONE', #55927, 1000.000000000000000 ) ;
#17319 = CARTESIAN_POINT ( 'NONE',  ( -48.50000000000000000, 13.41640786499872284, -7.000000000000000000 ) ) ;
#17320 = CARTESIAN_POINT ( 'NONE',  ( -9.058813317711337021, 135.1550000000000011, -2.943386871421374895 ) ) ;
#17321 = CARTESIAN_POINT ( 'NONE',  ( -52.55499999999999261, 0.000000000000000000, 8.024999999999991473 ) ) ;
#17322 = CARTESIAN_POINT ( 'NONE',  ( 40.99999999999998579, 107.7459666924148252, -3.000000000000000444 ) ) ;
#17323 = ORIENTED_EDGE ( 'NONE', *, *, #32115, .T. ) ;
#17324 = CARTESIAN_POINT ( 'NONE',  ( 8.102448949553183510, 158.1049999999999898, -5.886773742842746238 ) ) ;
#17325 = CARTESIAN_POINT ( 'NONE',  ( 44.99999999999998579, 119.9999999999999716, -10.00000000000000000 ) ) ;
#17326 = UNCERTAINTY_MEASURE_WITH_UNIT (LENGTH_MEASURE( 1.000000000000000082E-05 ), #67704, 'distance_accuracy_value', 'NONE');
#17327 = VECTOR ( 'NONE', #22065, 1000.000000000000000 ) ;
#17328 = DIRECTION ( 'NONE',  ( 0.000000000000000000, 0.000000000000000000, 1.000000000000000000 ) ) ;
#17329 = LINE ( 'NONE', #55258, #24167 ) ;
#17330 = VERTEX_POINT ( 'NONE', #38845 ) ;
#17331 = CYLINDRICAL_SURFACE ( 'NONE', #21674, 0.5000000000000004441 ) ;
#17332 = ORIENTED_EDGE ( 'NONE', *, *, #10336, .F. ) ;
#17333 = PRESENTATION_LAYER_ASSIGNMENT (  '', '', ( #54341 ) ) ;
#17334 = DIRECTION ( 'NONE',  ( 0.000000000000000000, 0.000000000000000000, 1.000000000000000000 ) ) ;
#17335 = CARTESIAN_POINT ( 'NONE',  ( -167.3049999999999784, 8.437984349512085203, -1.550032578732815448E-15 ) ) ;
#17336 = VERTEX_POINT ( 'NONE', #11720 ) ;
#17337 = CARTESIAN_POINT ( 'NONE',  ( -88.55707362346616662, -1.166476076187852838E-15, -9.524999999999991473 ) ) ;
#17338 = UNCERTAINTY_MEASURE_WITH_UNIT (LENGTH_MEASURE( 1.000000000000000082E-05 ), #46025, 'distance_accuracy_value', 'NONE');
#17339 = STYLED_ITEM ( 'NONE', ( #40517 ), #47220 ) ;
#17340 = DIRECTION ( 'NONE',  ( 0.000000000000000000, 0.000000000000000000, 1.000000000000000000 ) ) ;
#17341 = SURFACE_STYLE_USAGE ( .BOTH. , #10309 ) ;
#17342 = CARTESIAN_POINT ( 'NONE',  ( -78.14292637653380780, 5.598654528085800663, -7.705886871421367523 ) ) ;
#17343 = B_SPLINE_CURVE_WITH_KNOTS ( 'NONE', 3,
 ( #25551, #47787, #68148, #69189, #20989, #31170, #57584, #36152, #20648, #9415, #42159, #30836 ),
 .UNSPECIFIED., .F., .F.,
 ( 4, 2, 2, 2, 2, 4 ),
 ( 0.000000000000000000, 0.0005293381373090682695, 0.001058676274618136539, 0.001323345343272677721, 0.001588014411927218686, 0.002117352549236312977 ),
 .UNSPECIFIED. ) ;
#17344 = ORIENTED_EDGE ( 'NONE', *, *, #42146, .F. ) ;
#17345 = PRESENTATION_STYLE_ASSIGNMENT (( #50033 ) ) ;
#17346 = FACE_OUTER_BOUND ( 'NONE', #20407, .T. ) ;
#17347 = CARTESIAN_POINT ( 'NONE',  ( -81.65499999999998693, -7.632228543268600340, -2.479861379858950166 ) ) ;
#17348 = EDGE_LOOP ( 'NONE', ( #22372, #7694, #26595 ) ) ;
#17349 = EDGE_CURVE ( 'NONE', #56901, #61113, #16347, .T. ) ;
#17350 = STYLED_ITEM ( 'NONE', ( #22321 ), #37076 ) ;
#17351 = CARTESIAN_POINT ( 'NONE',  ( 69.99999999999998579, 36.75000000000000000, -3.750000000000000000 ) ) ;
#17352 = CARTESIAN_POINT ( 'NONE',  ( -54.80707362346617373, 10.01517768586948698, -1.839758294383808571E-15 ) ) ;
#17353 = COLOUR_RGB ( '', 0.09019608, 0.27058824, 0.51372549) ;
#17354 = DIRECTION ( 'NONE',  ( -1.000000000000000000, 0.000000000000000000, 0.000000000000000000 ) ) ;
#17355 = EDGE_LOOP ( 'NONE', ( #59752, #869, #48531, #41978 ) ) ;
#17356 = AXIS2_PLACEMENT_3D ( 'NONE', #45838, #19055, #67262 ) ;
#17357 = ADVANCED_FACE ( 'NONE', ( #11018 ), #27859, .T. ) ;
#17358 = CARTESIAN_POINT ( 'NONE',  ( -8.102448949553181734, 128.4950000000000045, 5.886773742842747126 ) ) ;
#17359 = CARTESIAN_POINT ( 'NONE',  ( -114.2950000000000017, -2.607480562269069768, 8.024999999999991473 ) ) ;
#17360 = VECTOR ( 'NONE', #69371, 1000.000000000000000 ) ;
#17361 = SURFACE_STYLE_FILL_AREA ( #61592 ) ;
#17362 = CIRCLE ( 'NONE', #69068, 0.2500000000000002220 ) ;
#17364 = CARTESIAN_POINT ( 'NONE',  ( -17.07366864973394982, 11.10307524832556503, -4.552615482027356109 ) ) ;
#17363 = CARTESIAN_POINT ( 'NONE',  ( -32.60021343251996484, -9.015750088255582995, -2.278575939230253589 ) ) ;
#17365 = VECTOR ( 'NONE', #12084, 1000.000000000000227 ) ;
#17366 = CARTESIAN_POINT ( 'NONE',  ( -154.0429263765338135, -9.058813317711329915, -2.943386871421370898 ) ) ;
#17367 = CARTESIAN_POINT ( 'NONE',  ( -178.3449999999999989, 7.632228543268599452, -2.479861379858951942 ) ) ;
#17368 = EDGE_CURVE ( 'NONE', #8636, #51304, #16681, .T. ) ;
#17369 = VECTOR ( 'NONE', #30978, 1000.000000000000000 ) ;
#17370 = CARTESIAN_POINT ( 'NONE',  ( -64.55707362346618083, -1.166476076187852838E-15, -9.524999999999991473 ) ) ;
#17371 = AXIS2_PLACEMENT_3D ( 'NONE', #59276, #142, #16443 ) ;
#17373 = CARTESIAN_POINT ( 'NONE',  ( -44.52084369503066341, -13.99284662042119365, 2.674043755914946363 ) ) ;
#17372 =( GEOMETRIC_REPRESENTATION_CONTEXT ( 3 ) GLOBAL_UNCERTAINTY_ASSIGNED_CONTEXT ( ( #21387 ) ) GLOBAL_UNIT_ASSIGNED_CONTEXT ( ( #45938, #46299, #25148 ) ) REPRESENTATION_CONTEXT ( 'NONE', 'WORKASPACE' ) );
#17374 = ORIENTED_EDGE ( 'NONE', *, *, #36763, .T. ) ;
#17375 = PRESENTATION_STYLE_ASSIGNMENT (( #28560 ) ) ;
#17376 = ORIENTED_EDGE ( 'NONE', *, *, #46021, .T. ) ;
#17377 = CARTESIAN_POINT ( 'NONE',  ( -70.49292637653378790, -8.102448949553172852, 5.886773742842742685 ) ) ;
#17378 = DIRECTION ( 'NONE',  ( -1.000000000000000000, 0.000000000000000000, 0.000000000000000000 ) ) ;
#17379 = CARTESIAN_POINT ( 'NONE',  ( 1.000000000000000000, 42.00000000000000000, 80.00402776293826435 ) ) ;
#17380 = DIRECTION ( 'NONE',  ( 0.000000000000000000, 1.000000000000000000, 0.000000000000000000 ) ) ;
#17381 = CARTESIAN_POINT ( 'NONE',  ( 0.8561460859850876792, 43.00000000000000711, 74.38749456993821241 ) ) ;
#17382 = CARTESIAN_POINT ( 'NONE',  ( -79.49292637653380211, -8.102448949553174629, 5.886773742842742685 ) ) ;
#17383 = EDGE_LOOP ( 'NONE', ( #24577, #31072, #6908, #18534 ) ) ;
#17384 = CARTESIAN_POINT ( 'NONE',  ( -172.8550000000000182, 4.716976649647094177, 6.492361379858945902 ) ) ;
#17385 = ORIENTED_EDGE ( 'NONE', *, *, #36135, .F. ) ;
#17386 = CARTESIAN_POINT ( 'NONE',  ( -45.00000000000000000, 10.49999999999998579, 4.000000000000000000 ) ) ;
#17387 = SURFACE_STYLE_USAGE ( .BOTH. , #28577 ) ;
#17388 =( LENGTH_UNIT ( ) NAMED_UNIT ( * ) SI_UNIT ( .MILLI., .METRE. ) );
#17389 = PRESENTATION_STYLE_ASSIGNMENT (( #53604 ) ) ;
#17390 = PRESENTATION_LAYER_ASSIGNMENT (  '', '', ( #38748 ) ) ;
#17391 = FACE_OUTER_BOUND ( 'NONE', #52522, .T. ) ;
#17392 = CARTESIAN_POINT ( 'NONE',  ( 2.607480562269076430, 150.9070736234661183, -8.025000000000000355 ) ) ;
#17393 = AXIS2_PLACEMENT_3D ( 'NONE', #19857, #68404, #62755 ) ;
#17394 = ORIENTED_EDGE ( 'NONE', *, *, #62987, .T. ) ;
#17395 = FILL_AREA_STYLE ('',( #5744 ) ) ;
#17396 = CARTESIAN_POINT ( 'NONE',  ( -86.00499999999998124, 6.826472737025115478, 4.959722759717899443 ) ) ;
#17397 = VECTOR ( 'NONE', #16241, 1000.000000000000000 ) ;
#17398 = UNCERTAINTY_MEASURE_WITH_UNIT (LENGTH_MEASURE( 1.000000000000000082E-05 ), #61940, 'distance_accuracy_value', 'NONE');
#17399 = CARTESIAN_POINT ( 'NONE',  ( -91.85707362346617799, -5.598654528085803328, -7.705886871421366635 ) ) ;
#17400 = AXIS2_PLACEMENT_3D ( 'NONE', #66130, #66854, #40138 ) ;
#17401 = CARTESIAN_POINT ( 'NONE',  ( -74.50000000000000000, 64.00000000000000000, 10.00000000000000000 ) ) ;
#17402 = DIRECTION ( 'NONE',  ( 0.000000000000000000, 0.000000000000000000, 1.000000000000000000 ) ) ;
#17403 = CARTESIAN_POINT ( 'NONE',  ( 31.00000000000000000, 42.00000000000000000, -75.00000000000001421 ) ) ;
#17404 =( LENGTH_UNIT ( ) NAMED_UNIT ( * ) SI_UNIT ( .MILLI., .METRE. ) );
#17405 = ORIENTED_EDGE ( 'NONE', *, *, #48098, .T. ) ;
#17406 = FACE_OUTER_BOUND ( 'NONE', #834, .T. ) ;
#17407 = CARTESIAN_POINT ( 'NONE',  ( -59.39499999999998892, -6.826472737025115478, -4.959722759717899443 ) ) ;
#17408 = ORIENTED_EDGE ( 'NONE', *, *, #12, .F. ) ;
#17409 = PRESENTATION_STYLE_ASSIGNMENT (( #1121 ) ) ;
#17410 = AXIS2_PLACEMENT_3D ( 'NONE', #2558, #25020, #67957 ) ;
#17411 = AXIS2_PLACEMENT_3D ( 'NONE', #12611, #56210, #8038 ) ;
#17412 = PRESENTATION_STYLE_ASSIGNMENT (( #22659 ) ) ;
#17413 = CARTESIAN_POINT ( 'NONE',  ( -44.99999999999999289, 8.589831058620415405, -5.576814063796836862 ) ) ;
#17414 = ORIENTED_EDGE ( 'NONE', *, *, #30657, .T. ) ;
#17415 = ORIENTED_EDGE ( 'NONE', *, *, #44120, .T. ) ;
#17416 = STYLED_ITEM ( 'NONE', ( #35836 ), #63851 ) ;
#17417 = CARTESIAN_POINT ( 'NONE',  ( -75.00000000000000000, 9.289150624329691297, 6.641434857031756955 ) ) ;
#17418 = CARTESIAN_POINT ( 'NONE',  ( -111.0549999999999926, -9.827790563157499189E-16, -8.024999999999991473 ) ) ;
#17419 = VERTEX_POINT ( 'NONE', #54949 ) ;
#17420 = DIRECTION ( 'NONE',  ( -0.000000000000000000, -1.000000000000000000, -0.000000000000000000 ) ) ;
#17421 = CARTESIAN_POINT ( 'NONE',  ( -74.99999999999998579, 50.00000000000000000, -9.500000000000000000 ) ) ;
#17422 = ADVANCED_FACE ( 'NONE', ( #6776 ), #38146, .F. ) ;
#17423 =( NAMED_UNIT ( * ) PLANE_ANGLE_UNIT ( ) SI_UNIT ( $, .RADIAN. ) );
#17424 = DIRECTION ( 'NONE',  ( -1.000000000000000000, 0.000000000000000000, 0.000000000000000000 ) ) ;
#17425 = AXIS2_PLACEMENT_3D ( 'NONE', #5739, #5389, #38855 ) ;
#17426 = CARTESIAN_POINT ( 'NONE',  ( -153.8070736234661808, 10.01517768586948698, -1.839758294383808571E-15 ) ) ;
#17427 =( GEOMETRIC_REPRESENTATION_CONTEXT ( 3 ) GLOBAL_UNCERTAINTY_ASSIGNED_CONTEXT ( ( #17338 ) ) GLOBAL_UNIT_ASSIGNED_CONTEXT ( ( #46025, #46380, #63558 ) ) REPRESENTATION_CONTEXT ( 'NONE', 'WORKASPACE' ) );
#17428 = CARTESIAN_POINT ( 'NONE',  ( -9.058813317711337021, 134.0449999999999875, -2.943386871421374895 ) ) ;
#17429 = EDGE_CURVE ( 'NONE', #23235, #29534, #48400, .T. ) ;
#17430 = CARTESIAN_POINT ( 'NONE',  ( -83.75707362346616947, -5.598654528085801552, 7.705886871421367523 ) ) ;
#17431 = CARTESIAN_POINT ( 'NONE',  ( -54.36101593760355399, -9.269969316126742243, -2.682282536902753645 ) ) ;
#17432 = ORIENTED_EDGE ( 'NONE', *, *, #2507, .F. ) ;
#17433 = AXIS2_PLACEMENT_3D ( 'NONE', #12523, #21108, #12882 ) ;
#17435 = CARTESIAN_POINT ( 'NONE',  ( 12.72792206135785698, 115.4999999999999574, -10.50000000000000000 ) ) ;
#17434 = DIRECTION ( 'NONE',  ( 0.000000000000000000, -1.000000000000000000, -0.000000000000000000 ) ) ;
#17436 = FACE_OUTER_BOUND ( 'NONE', #66044, .T. ) ;
#17437 = AXIS2_PLACEMENT_3D ( 'NONE', #16006, #749, #15647 ) ;
#17438 = CARTESIAN_POINT ( 'NONE',  ( -132.3549999999999898, -4.716976649647093289, -6.492361379858945902 ) ) ;
#17439 = EDGE_CURVE ( 'NONE', #49204, #53532, #24586, .T. ) ;
#17440 = CARTESIAN_POINT ( 'NONE',  ( -44.99999999999998579, 119.9999999999999716, -7.500000000000000000 ) ) ;
#17441 = PRESENTATION_STYLE_ASSIGNMENT (( #65589 ) ) ;
#17442 = CARTESIAN_POINT ( 'NONE',  ( -149.5449999999999875, -7.632228543268600340, -2.479861379858950166 ) ) ;
#17443 = ADVANCED_FACE ( 'NONE', ( #45756 ), #41507, .F. ) ;
#17444 = AXIS2_PLACEMENT_3D ( 'NONE', #27195, #16368, #64856 ) ;
#17445 = CARTESIAN_POINT ( 'NONE',  ( -130.9449999999999648, -9.827790563157499189E-16, -8.024999999999991473 ) ) ;
#17446 = EDGE_CURVE ( 'NONE', #35727, #42295, #46099, .T. ) ;
#17447 = ORIENTED_EDGE ( 'NONE', *, *, #52039, .F. ) ;
#17448 = CYLINDRICAL_SURFACE ( 'NONE', #385, 0.2500000000000002220 ) ;
#17449 = EDGE_CURVE ( 'NONE', #58089, #38966, #23601, .T. ) ;
#17450 = AXIS2_PLACEMENT_3D ( 'NONE', #31154, #63189, #30818 ) ;
#17451 = CARTESIAN_POINT ( 'NONE',  ( -182.8429263765338249, 9.058813317711329915, -2.943386871421373119 ) ) ;
#17452 = CARTESIAN_POINT ( 'NONE',  ( -61.19499999999997897, 8.437984349512085203, -1.550032578732815448E-15 ) ) ;
#17453 =( NAMED_UNIT ( * ) SI_UNIT ( $, .STERADIAN. ) SOLID_ANGLE_UNIT ( ) );
#17454 = DIRECTION ( 'NONE',  ( 0.000000000000000000, 0.000000000000000000, 1.000000000000000000 ) ) ;
#17455 = DIRECTION ( 'NONE',  ( -0.000000000000000000, 0.000000000000000000, -1.000000000000000000 ) ) ;
#17456 = DIRECTION ( 'NONE',  ( 1.000000000000000000, 7.709882115452468306E-16, -0.000000000000000000 ) ) ;
#17457 = CARTESIAN_POINT ( 'NONE',  ( -94.34292637653379643, -9.058813317711329915, 2.943386871421371787 ) ) ;
#17458 = CARTESIAN_POINT ( 'NONE',  ( -52.16324889301085221, -11.19354186750540059, 1.856282217695744530 ) ) ;
#17459 = AXIS2_PLACEMENT_3D ( 'NONE', #27332, #15789, #64654 ) ;
#17460 = LINE ( 'NONE', #16760, #57405 ) ;
#17461 = VECTOR ( 'NONE', #61169, 1000.000000000000000 ) ;
#17462 = FILL_AREA_STYLE_COLOUR ( '', #21320 ) ;
#17463 = DIRECTION ( 'NONE',  ( 0.000000000000000000, -0.000000000000000000, 1.000000000000000000 ) ) ;
#17464 = CARTESIAN_POINT ( 'NONE',  ( -100.5570736234661808, -1.166476076187852838E-15, -9.524999999999991473 ) ) ;
#17465 = CIRCLE ( 'NONE', #38823, 0.4999999999999991118 ) ;
#17466 = ORIENTED_EDGE ( 'NONE', *, *, #345, .T. ) ;
#17467 = LINE ( 'NONE', #50836, #27343 ) ;
#17468 = DIRECTION ( 'NONE',  ( 0.000000000000000000, 1.000000000000000000, -0.000000000000000000 ) ) ;
#17469 = EDGE_LOOP ( 'NONE', ( #28874, #21576, #8964, #23625 ) ) ;
#17470 = CIRCLE ( 'NONE', #18607, 5.000000000000004441 ) ;
#17471 = CARTESIAN_POINT ( 'NONE',  ( 4.716976649647096842, 122.8570736234661638, 6.492361379858953896 ) ) ;
#17472 = FILL_AREA_STYLE_COLOUR ( '', #34938 ) ;
#17473 = PLANE ( 'NONE',  #45217 ) ;
#17474 = ORIENTED_EDGE ( 'NONE', *, *, #14953, .T. ) ;
#17475 = FILL_AREA_STYLE ('',( #16452 ) ) ;
#17476 = CIRCLE ( 'NONE', #21930, 1.000000000000000888 ) ;
#17477 =( NAMED_UNIT ( * ) PLANE_ANGLE_UNIT ( ) SI_UNIT ( $, .RADIAN. ) );
#17478 = VERTEX_POINT ( 'NONE', #25629 ) ;
#17480 = SURFACE_STYLE_USAGE ( .BOTH. , #49821 ) ;
#17479 = B_SPLINE_CURVE_WITH_KNOTS ( 'NONE', 3,
 ( #64702, #37999, #32668, #54123, #5934, #3027, #18589, #8021, #56192, #24192, #29096, #18898, #34409, #46037, #12946, #50592, #2327, #67113, #61138, #23849, #2699, #7664, #13281, #55862, #34737, #45006, #45356, #1972, #29820, #50941, #35100, #40398, #24521, #29471, #66774, #61806, #45697, #56547, #13637, #51285 ),
 .UNSPECIFIED., .F., .F.,
 ( 4, 2, 2, 2, 2, 2, 2, 2, 2, 2, 2, 2, 2, 2, 2, 2, 2, 2, 2, 4 ),
 ( 0.007910652177015307582, 0.008898557670442612533, 0.009886463163869915749, 0.01087436865729721897, 0.01186227415072452392, 0.01285017964415182713, 0.01334413239086547701, 0.01383808513757912861, 0.01482599063100643183, 0.01581389612443373505, 0.01630784887114738319, 0.01680180161786103479, 0.01778970711128833801, 0.01828365985800198962, 0.01877761260471563776, 0.01976551809814294097, 0.02075342359157024419, 0.02174132908499755087, 0.02272923457842485409, 0.02371714007185216078 ),
 .UNSPECIFIED. ) ;
#17481 = CARTESIAN_POINT ( 'NONE',  ( 0.000000000000000000, 87.30187232391182306, 8.025000000000000355 ) ) ;
#17482 = AXIS2_PLACEMENT_3D ( 'NONE', #68691, #69041, #4647 ) ;
#17483 = LINE ( 'NONE', #23088, #31662 ) ;
#17484 = CARTESIAN_POINT ( 'NONE',  ( -89.09499999999998465, -2.607480562269071545, -8.024999999999991473 ) ) ;
#17485 = ORIENTED_EDGE ( 'NONE', *, *, #65521, .T. ) ;
#17486 = STYLED_ITEM ( 'NONE', ( #11994 ), #56833 ) ;
#17487 = DIRECTION ( 'NONE',  ( 0.000000000000000000, 1.000000000000000000, 0.000000000000000000 ) ) ;
#17488 = SURFACE_SIDE_STYLE ('',( #55784 ) ) ;
#17489 =( GEOMETRIC_REPRESENTATION_CONTEXT ( 3 ) GLOBAL_UNCERTAINTY_ASSIGNED_CONTEXT ( ( #47630 ) ) GLOBAL_UNIT_ASSIGNED_CONTEXT ( ( #7221, #66291, #35339 ) ) REPRESENTATION_CONTEXT ( 'NONE', 'WORKASPACE' ) );
#17490 = ORIENTED_EDGE ( 'NONE', *, *, #60742, .T. ) ;
#17491 = FACE_OUTER_BOUND ( 'NONE', #8040, .T. ) ;
#17492 = CARTESIAN_POINT ( 'NONE',  ( 40.99999999999998579, 108.0000000000000000, 3.500000000000000000 ) ) ;
#17493 = DIRECTION ( 'NONE',  ( 1.000000000000000000, 0.000000000000000000, 0.000000000000000000 ) ) ;
#17494 = ORIENTED_EDGE ( 'NONE', *, *, #39753, .F. ) ;
#17495 = FILL_AREA_STYLE ('',( #65653 ) ) ;
#17497 = ORIENTED_EDGE ( 'NONE', *, *, #20051, .F. ) ;
#17496 = ADVANCED_FACE ( 'NONE', ( #3448 ), #47150, .T. ) ;
#17498 = CARTESIAN_POINT ( 'NONE',  ( -138.4429263765337907, -1.166476076187852838E-15, -9.524999999999991473 ) ) ;
#17499 = SURFACE_STYLE_USAGE ( .BOTH. , #50531 ) ;
#17500 = CYLINDRICAL_SURFACE ( 'NONE', #46536, 9.524999999999991473 ) ;
#17501 = FILL_AREA_STYLE ('',( #54054 ) ) ;
#17502 = CARTESIAN_POINT ( 'NONE',  ( -181.4070736234661183, 3.094860106618428031, -9.524999999999993250 ) ) ;
#17503 = DIRECTION ( 'NONE',  ( -0.07898106964430656740, -0.9968761159932768567, -0.000000000000000000 ) ) ;
#17504 = DIRECTION ( 'NONE',  ( 1.300977106640434891E-16, 0.000000000000000000, 1.000000000000000000 ) ) ;
#17505 = ADVANCED_FACE ( 'NONE', ( #57665 ), #15134, .T. ) ;
#17506 = CARTESIAN_POINT ( 'NONE',  ( -3.109213548236402502, 9.000000000000007105, 0.5129086262188717882 ) ) ;
#17507 = CARTESIAN_POINT ( 'NONE',  ( -2.056319983864984824, 153.0517686201319805, -7.829595205988884032 ) ) ;
#17508 = ORIENTED_EDGE ( 'NONE', *, *, #3976, .F. ) ;
#17509 = CARTESIAN_POINT ( 'NONE',  ( -49.40707362346615383, 3.094860106618428031, -9.524999999999993250 ) ) ;
#17510 = CARTESIAN_POINT ( 'NONE',  ( 22.99999999999995381, 5.000000000000000000, 32.00402776293825724 ) ) ;
#17511 = CARTESIAN_POINT ( 'NONE',  ( -148.5570736234661808, -1.166476076187852838E-15, -9.524999999999991473 ) ) ;
#17512 = CIRCLE ( 'NONE', #56810, 10.02499999999997904 ) ;
#17513 = ORIENTED_EDGE ( 'NONE', *, *, #16945, .F. ) ;
#17514 = CARTESIAN_POINT ( 'NONE',  ( -162.5049999999999386, -6.826472737025115478, -4.959722759717899443 ) ) ;
#17515 = DIRECTION ( 'NONE',  ( -0.000000000000000000, -0.000000000000000000, -1.000000000000000000 ) ) ;
#17516 = PRESENTATION_STYLE_ASSIGNMENT (( #65670 ) ) ;
#17517 = CARTESIAN_POINT ( 'NONE',  ( -172.4950000000000045, 6.826472737025113702, -4.959722759717902107 ) ) ;
#17518 = EDGE_CURVE ( 'NONE', #66411, #58978, #65276, .T. ) ;
#17519 = AXIS2_PLACEMENT_3D ( 'NONE', #41795, #58276, #52339 ) ;
#17520 = TOROIDAL_SURFACE ( 'NONE', #40028, 1.000000000000000000, 0.5000000000000000000 ) ;
#17521 = CARTESIAN_POINT ( 'NONE',  ( -154.7949999999999875, 2.607480562269069324, -8.024999999999993250 ) ) ;
#17522 = ORIENTED_EDGE ( 'NONE', *, *, #61752, .F. ) ;
#17523 = DIRECTION ( 'NONE',  ( 0.000000000000000000, 0.000000000000000000, 1.000000000000000000 ) ) ;
#17524 = CARTESIAN_POINT ( 'NONE',  ( 44.34845674352007450, 9.782818914506686170, 3.509226550553890878 ) ) ;
#17525 = ADVANCED_FACE ( 'NONE', ( #68570 ), #29886, .F. ) ;
#17526 = PLANE ( 'NONE',  #19229 ) ;
#17527 = CARTESIAN_POINT ( 'NONE',  ( -76.55499999999997840, 0.000000000000000000, 8.024999999999991473 ) ) ;
#17528 = CARTESIAN_POINT ( 'NONE',  ( -36.04767328987400532, -11.70694734933133141, 3.186424117865112926 ) ) ;
#17529 = CARTESIAN_POINT ( 'NONE',  ( 68.99999999999998579, 36.75000000000000000, 3.750000000000000000 ) ) ;
#17530 =( GEOMETRIC_REPRESENTATION_CONTEXT ( 3 ) GLOBAL_UNCERTAINTY_ASSIGNED_CONTEXT ( ( #41901 ) ) GLOBAL_UNIT_ASSIGNED_CONTEXT ( ( #38436, #44409, #12673 ) ) REPRESENTATION_CONTEXT ( 'NONE', 'WORKASPACE' ) );
#17531 = CARTESIAN_POINT ( 'NONE',  ( -74.24499999999999034, -4.716976649647093289, -6.492361379858945902 ) ) ;
#17532 = CARTESIAN_POINT ( 'NONE',  ( 10.01517768586949231, 145.8050000000000068, 1.839758294383810543E-15 ) ) ;
#17533 = CARTESIAN_POINT ( 'NONE',  ( 7.511572993685799101E-16, 2.500000000000000000, -6.999999999999997335 ) ) ;
#17534 = COLOUR_RGB ( '', 0.09019608, 0.27058824, 0.51372549) ;
#17535 = VECTOR ( 'NONE', #59865, 1000.000000000000000 ) ;
#17536 = DIRECTION ( 'NONE',  ( 1.000000000000000000, 0.000000000000000000, 0.000000000000000000 ) ) ;
#17537 = CIRCLE ( 'NONE', #38895, 9.499999999999998224 ) ;
#17538 = DIRECTION ( 'NONE',  ( 1.000000000000000000, 0.000000000000000000, 0.000000000000000000 ) ) ;
#17539 =( NAMED_UNIT ( * ) SI_UNIT ( $, .STERADIAN. ) SOLID_ANGLE_UNIT ( ) );
#17540 = ORIENTED_EDGE ( 'NONE', *, *, #40533, .T. ) ;
#17541 = CIRCLE ( 'NONE', #24235, 7.499999999999985789 ) ;
#17542 = SURFACE_SIDE_STYLE ('',( #44634 ) ) ;
#17543 = CARTESIAN_POINT ( 'NONE',  ( -54.05707362346618083, 0.000000000000000000, 9.524999999999991473 ) ) ;
#17544 = FILL_AREA_STYLE ('',( #21396 ) ) ;
#17545 = ORIENTED_EDGE ( 'NONE', *, *, #11757, .F. ) ;
#17546 = EDGE_LOOP ( 'NONE', ( #40092, #46038, #38450, #42053 ) ) ;
#17547 = CARTESIAN_POINT ( 'NONE',  ( -15.98999599679679839, 147.4999999999999716, -10.00000000000000000 ) ) ;
#17548 = EDGE_CURVE ( 'NONE', #32528, #22579, #8452, .T. ) ;
#17549 = CIRCLE ( 'NONE', #51227, 0.2500000000000000000 ) ;
#17550 =( NAMED_UNIT ( * ) PLANE_ANGLE_UNIT ( ) SI_UNIT ( $, .RADIAN. ) );
#17551 = DIRECTION ( 'NONE',  ( 0.000000000000000000, -1.000000000000000000, 0.000000000000000000 ) ) ;
#17552 = ORIENTED_EDGE ( 'NONE', *, *, #55130, .F. ) ;
#17553 = CARTESIAN_POINT ( 'NONE',  ( -116.1550000000000011, 7.632228543268600340, 2.479861379858949277 ) ) ;
#17554 = VERTEX_POINT ( 'NONE', #62238 ) ;
#17555 = CIRCLE ( 'NONE', #4055, 0.5000000000000004441 ) ;
#17556 =( LENGTH_UNIT ( ) NAMED_UNIT ( * ) SI_UNIT ( .MILLI., .METRE. ) );
#17557 = ORIENTED_EDGE ( 'NONE', *, *, #3147, .T. ) ;
#17558 = DIRECTION ( 'NONE',  ( 1.000000000000000000, 0.000000000000000000, -1.300977106640442040E-16 ) ) ;
#17559 = CARTESIAN_POINT ( 'NONE',  ( -67.70707362346617231, -3.094860106618431139, -9.524999999999991473 ) ) ;
#17560 = ORIENTED_EDGE ( 'NONE', *, *, #27934, .T. ) ;
#17561 = AXIS2_PLACEMENT_3D ( 'NONE', #5401, #43471, #33542 ) ;
#17562 = AXIS2_PLACEMENT_3D ( 'NONE', #21430, #16198, #21090 ) ;
#17563 = CARTESIAN_POINT ( 'NONE',  ( 10.99999999999999645, 11.99999999999999289, -3.499999999999991118 ) ) ;
#17564 =( BOUNDED_CURVE ( )  B_SPLINE_CURVE ( 2, ( #45891, #46252, #19472, #67319, #19825, #40974, #40614, #31063, #62394, #62029, #25788 ),
 .UNSPECIFIED., .F., .F. ) 
 B_SPLINE_CURVE_WITH_KNOTS ( ( 3, 2, 2, 2, 2, 3 ),
 ( 0.6086956521738985382, 0.6108695652173767865, 0.6130434782608549238, 0.6152173913043331721, 0.6173913043478113094, 0.6195652173912895577 ),
 .UNSPECIFIED. ) 
 CURVE ( )  GEOMETRIC_REPRESENTATION_ITEM ( )  RATIONAL_B_SPLINE_CURVE ( ( 1.000000000000327516, 0.9510565162948261264, 1.000000000000000000, 0.9510565162951535312, 1.000000000000000000, 0.9510565162951535312, 1.000000000000000000, 0.9510565162951535312, 1.000000000000000000, 0.9510565162954859320, 0.9999999999996675992 ) ) 
 REPRESENTATION_ITEM ( '' )  );
#17565 = CARTESIAN_POINT ( 'NONE',  ( 24.15983302833083712, 27.22897014610288480, -27.27767451507459029 ) ) ;
#17566 = FACE_OUTER_BOUND ( 'NONE', #52102, .T. ) ;
#17567 = EDGE_LOOP ( 'NONE', ( #55077, #65221, #39828, #31302 ) ) ;
#17568 = EDGE_LOOP ( 'NONE', ( #51618, #23131, #6600 ) ) ;
#17569 = CARTESIAN_POINT ( 'NONE',  ( -7.593134170275801509, 110.5000000000000000, -5.767355889360383792 ) ) ;
#17570 = FILL_AREA_STYLE_COLOUR ( '', #55209 ) ;
#17571 = CARTESIAN_POINT ( 'NONE',  ( 22.75000000000000711, 36.75000000000000000, 4.000000000000000000 ) ) ;
#17572 = CARTESIAN_POINT ( 'NONE',  ( 44.50000000000000000, 10.36037961002804408, 3.500000000000000000 ) ) ;
#17573 = VERTEX_POINT ( 'NONE', #30207 ) ;
#17574 = CARTESIAN_POINT ( 'NONE',  ( -7.632228543268608334, 138.8429263765337964, 2.479861379858952830 ) ) ;
#17575 = CARTESIAN_POINT ( 'NONE',  ( -75.00000000000000000, -2.215169945516535778E-14, 6.999999999999999112 ) ) ;
#17576 = ADVANCED_FACE ( 'NONE', ( #19675 ), #2190, .F. ) ;
#17577 = DIRECTION ( 'NONE',  ( 0.000000000000000000, 0.000000000000000000, -1.000000000000000000 ) ) ;
#17578 = COLOUR_RGB ( '', 0.31764706, 0.68627451, 0.89019608) ;
#17579 = CARTESIAN_POINT ( 'NONE',  ( -2.607480562269094637, 114.0929263765338106, -8.024999999999986144 ) ) ;
#17580 = EDGE_CURVE ( 'NONE', #68346, #37399, #14671, .T. ) ;
#17581 = EDGE_LOOP ( 'NONE', ( #22814, #63303, #15006, #12651 ) ) ;
#17582 = ORIENTED_EDGE ( 'NONE', *, *, #41906, .F. ) ;
#17583 = STYLED_ITEM ( 'NONE', ( #18767 ), #1461 ) ;
#17584 = DIRECTION ( 'NONE',  ( 0.000000000000000000, 0.000000000000000000, -1.000000000000000000 ) ) ;
#17585 = DIRECTION ( 'NONE',  ( 0.000000000000000000, 0.000000000000000000, 1.000000000000000000 ) ) ;
#17586 = CARTESIAN_POINT ( 'NONE',  ( -131.1550000000000011, 7.632228543268600340, 2.479861379858949277 ) ) ;
#17587 = DIRECTION ( 'NONE',  ( 1.000000000000000000, 0.000000000000000000, 0.000000000000000000 ) ) ;
#17588 = DIRECTION ( 'NONE',  ( 0.000000000000000000, 0.000000000000000000, 1.000000000000000000 ) ) ;
#17589 = ORIENTED_EDGE ( 'NONE', *, *, #46893, .F. ) ;
#17590 = CIRCLE ( 'NONE', #20791, 0.2500000000000002220 ) ;
#17591 = EDGE_CURVE ( 'NONE', #57659, #41595, #36931, .T. ) ;
#17592 = CARTESIAN_POINT ( 'NONE',  ( -106.0429263765337993, -9.058813317711329915, -2.943386871421370898 ) ) ;
#17593 = CARTESIAN_POINT ( 'NONE',  ( -107.4570736234661865, -9.058813317711329915, 2.943386871421371787 ) ) ;
#17594 = DIRECTION ( 'NONE',  ( -0.000000000000000000, -0.000000000000000000, 1.000000000000000000 ) ) ;
#17595 = VERTEX_POINT ( 'NONE', #26660 ) ;
#17596 = ORIENTED_EDGE ( 'NONE', *, *, #61532, .F. ) ;
#17597 = CARTESIAN_POINT ( 'NONE',  ( -45.90821247049333920, 9.419343807758844278, 3.356427483424777147 ) ) ;
#17598 = SURFACE_STYLE_FILL_AREA ( #22859 ) ;
#17599 = CARTESIAN_POINT ( 'NONE',  ( -60.35499999999998977, -4.716976649647093289, -6.492361379858945902 ) ) ;
#17600 = ORIENTED_EDGE ( 'NONE', *, *, #62709, .T. ) ;
#17601 = SURFACE_SIDE_STYLE ('',( #34438 ) ) ;
#17602 = CARTESIAN_POINT ( 'NONE',  ( 57.24999999999999289, 28.24999999999998934, -3.750000000000000000 ) ) ;
#17603 = EDGE_CURVE ( 'NONE', #32928, #37155, #69265, .T. ) ;
#17604 = FACE_OUTER_BOUND ( 'NONE', #30487, .T. ) ;
#17605 = ORIENTED_EDGE ( 'NONE', *, *, #68811, .T. ) ;
#17606 = CARTESIAN_POINT ( 'NONE',  ( -45.50000000000000000, 9.708372675170618749, -3.611004237778681514 ) ) ;
#17607 = DIRECTION ( 'NONE',  ( 0.000000000000000000, 0.000000000000000000, 1.000000000000000000 ) ) ;
#17608 = EDGE_CURVE ( 'NONE', #2615, #63718, #25979, .T. ) ;
#17609 = DIRECTION ( 'NONE',  ( 0.000000000000000000, 1.000000000000000000, 0.000000000000000000 ) ) ;
#17610 = CARTESIAN_POINT ( 'NONE',  ( -58.24585058663792125, -8.499999999999992895, 0.6021708687696052387 ) ) ;
#17611 = SURFACE_STYLE_FILL_AREA ( #2744 ) ;
#17612 = DIRECTION ( 'NONE',  ( -1.000000000000000000, -0.000000000000000000, -0.000000000000000000 ) ) ;
#17613 =( GEOMETRIC_REPRESENTATION_CONTEXT ( 3 ) GLOBAL_UNCERTAINTY_ASSIGNED_CONTEXT ( ( #11530 ) ) GLOBAL_UNIT_ASSIGNED_CONTEXT ( ( #69140, #64185, #14629 ) ) REPRESENTATION_CONTEXT ( 'NONE', 'WORKASPACE' ) );
#17614 = CARTESIAN_POINT ( 'NONE',  ( -98.99499999999997613, -6.826472737025113702, 4.959722759717902107 ) ) ;
#17615 = CARTESIAN_POINT ( 'NONE',  ( -3.094860106618434248, 155.7950000000000159, 9.525000000000000355 ) ) ;
#17616 = PRESENTATION_LAYER_ASSIGNMENT (  '', '', ( #53545 ) ) ;
#17617 = CARTESIAN_POINT ( 'NONE',  ( -81.44499999999999318, 0.000000000000000000, 8.024999999999991473 ) ) ;
#17618 = DIRECTION ( 'NONE',  ( 0.000000000000000000, 1.000000000000000000, 0.000000000000000000 ) ) ;
#17619 = STYLED_ITEM ( 'NONE', ( #15936 ), #50144 ) ;
#17620 = DIRECTION ( 'NONE',  ( 0.9418169057949938860, 0.000000000000000000, -0.3361263392814427542 ) ) ;
#17621 = CARTESIAN_POINT ( 'NONE',  ( 53.24999999999999289, 27.74999999999998579, 4.000000000000000000 ) ) ;
#17622 = DIRECTION ( 'NONE',  ( 0.000000000000000000, 0.000000000000000000, -1.000000000000000000 ) ) ;
#17623 = PRESENTATION_STYLE_ASSIGNMENT (( #23226 ) ) ;
#17624 = ORIENTED_EDGE ( 'NONE', *, *, #17189, .F. ) ;
#17625 = CARTESIAN_POINT ( 'NONE',  ( -128.5429263765338135, 9.058813317711329915, 2.943386871421369566 ) ) ;
#17626 = CARTESIAN_POINT ( 'NONE',  ( -134.5449999999999875, -7.632228543268600340, -2.479861379858950166 ) ) ;
#17627 = CYLINDRICAL_SURFACE ( 'NONE', #60537, 0.5000000000000004441 ) ;
#17628 = PRESENTATION_LAYER_ASSIGNMENT (  '', '', ( #26569 ) ) ;
#17629 = CARTESIAN_POINT ( 'NONE',  ( 0.000000000000000000, 2.500000000000000000, 0.000000000000000000 ) ) ;
#17630 = CARTESIAN_POINT ( 'NONE',  ( 0.000000000000000000, 1.999999999999998668, 5.000000000000000000 ) ) ;
#17631 = ORIENTED_EDGE ( 'NONE', *, *, #37100, .T. ) ;
#17632 = ORIENTED_EDGE ( 'NONE', *, *, #62339, .T. ) ;
#17633 = CARTESIAN_POINT ( 'NONE',  ( 15.48999599679679662, 118.4999999999999716, -10.00000000000000000 ) ) ;
#17634 =( NAMED_UNIT ( * ) SI_UNIT ( $, .STERADIAN. ) SOLID_ANGLE_UNIT ( ) );
#17635 = EDGE_CURVE ( 'NONE', #47666, #23836, #52745, .T. ) ;
#17636 = CARTESIAN_POINT ( 'NONE',  ( 3.249999999999998668, 36.74999999999999289, 3.750000000000000000 ) ) ;
#17637 = SURFACE_STYLE_FILL_AREA ( #13020 ) ;
#17638 = COLOUR_RGB ( '', 0.66274510, 0.83137255, 0.94901961) ;
#17639 = CARTESIAN_POINT ( 'NONE',  ( 4.000000000000030198, 38.70020753820971748, 89.00000000000000000 ) ) ;
#17640 = ORIENTED_EDGE ( 'NONE', *, *, #58684, .T. ) ;
#17641 = CARTESIAN_POINT ( 'NONE',  ( -140.6049999999999613, 6.826472737025113702, -4.959722759717902107 ) ) ;
#17642 = VERTEX_POINT ( 'NONE', #20726 ) ;
#17643 = ORIENTED_EDGE ( 'NONE', *, *, #53084, .T. ) ;
#17644 = CARTESIAN_POINT ( 'NONE',  ( -60.00000000000000000, -2.024042244987997205E-14, 6.500000000000000000 ) ) ;
#17645 = CARTESIAN_POINT ( 'NONE',  ( 3.000000000000030198, 42.00000000000000000, 80.00402776293826435 ) ) ;
#17646 = ORIENTED_EDGE ( 'NONE', *, *, #58530, .T. ) ;
#17647 = CARTESIAN_POINT ( 'NONE',  ( -55.47384865756040284, -8.774376589852767694, -1.283477359179545862 ) ) ;
#17648 = DIRECTION ( 'NONE',  ( 1.000000000000000000, 0.000000000000000000, 0.000000000000000000 ) ) ;
#17649 = CARTESIAN_POINT ( 'NONE',  ( -8.102448949553181734, 130.8949999999999818, -5.886773742842749790 ) ) ;
#17650 = CARTESIAN_POINT ( 'NONE',  ( -4.500000000000002665, 21.99999999999998579, 3.750000000000000000 ) ) ;
#17651 = EDGE_LOOP ( 'NONE', ( #19046, #11296, #34224, #46166 ) ) ;
#17652 = ADVANCED_FACE ( 'NONE', ( #15807 ), #20230, .F. ) ;
#17653 = CYLINDRICAL_SURFACE ( 'NONE', #11648, 1.000000000000001998 ) ;
#17654 = CARTESIAN_POINT ( 'NONE',  ( -3.094860106618434248, 129.9050000000000011, 9.525000000000000355 ) ) ;
#17655 = CARTESIAN_POINT ( 'NONE',  ( -54.95499999999997698, -7.632228543268599452, 2.479861379858951054 ) ) ;
#17656 = LINE ( 'NONE', #23938, #57647 ) ;
#17657 = ORIENTED_EDGE ( 'NONE', *, *, #19217, .F. ) ;
#17658 = CARTESIAN_POINT ( 'NONE',  ( -5.598654528085806881, 152.8549999999999898, -7.705886871421374629 ) ) ;
#17659 = CARTESIAN_POINT ( 'NONE',  ( 30.99999999999998579, 0.000000000000000000, 72.00402776293822171 ) ) ;
#17660 = CARTESIAN_POINT ( 'NONE',  ( -88.49292637653380211, -8.102448949553174629, 5.886773742842742685 ) ) ;
#17661 = CIRCLE ( 'NONE', #35619, 1.000000000000000888 ) ;
#17662 = EDGE_CURVE ( 'NONE', #10834, #47340, #64726, .T. ) ;
#17663 = FACE_OUTER_BOUND ( 'NONE', #23827, .T. ) ;
#17664 = ADVANCED_FACE ( 'NONE', ( #37701 ), #58408, .F. ) ;
#17665 = EDGE_LOOP ( 'NONE', ( #25692, #8835, #52937, #25547 ) ) ;
#17666 = DIRECTION ( 'NONE',  ( 0.000000000000000000, 0.000000000000000000, 1.000000000000000000 ) ) ;
#17667 = ORIENTED_EDGE ( 'NONE', *, *, #53672, .F. ) ;
#17668 = DIRECTION ( 'NONE',  ( 1.000000000000000000, -0.000000000000000000, -1.300977106640434891E-16 ) ) ;
#17669 = CARTESIAN_POINT ( 'NONE',  ( 0.9728900412908074724, 111.9999999999999858, -7.965808808122197604 ) ) ;
#17670 = CARTESIAN_POINT ( 'NONE',  ( -172.2549999999999955, -4.716976649647092401, 6.492361379858946790 ) ) ;
#17671 = ORIENTED_EDGE ( 'NONE', *, *, #9476, .T. ) ;
#17672 = CYLINDRICAL_SURFACE ( 'NONE', #51997, 5.000000000000004441 ) ;
#17673 =( BOUNDED_CURVE ( )  B_SPLINE_CURVE ( 2, ( #63144, #14983, #31813, #53299, #20936, #57883, #48055, #47355, #10035, #9704, #68786 ),
 .UNSPECIFIED., .F., .F. ) 
 B_SPLINE_CURVE_WITH_KNOTS ( ( 3, 2, 2, 2, 2, 3 ),
 ( 0.4456521739130330229, 0.4478260869565112712, 0.4499999999999894640, 0.4521739130434676568, 0.4543478260869458496, 0.4565217391304240424 ),
 .UNSPECIFIED. ) 
 CURVE ( )  GEOMETRIC_REPRESENTATION_ITEM ( )  RATIONAL_B_SPLINE_CURVE ( ( 1.000000000000234923, 0.9510565162949186080, 1.000000000000000000, 0.9510565162951535312, 1.000000000000000000, 0.9510565162951535312, 1.000000000000000000, 0.9510565162951535312, 1.000000000000000000, 0.9510565162953947826, 0.9999999999997587485 ) ) 
 REPRESENTATION_ITEM ( '' )  );
#17674 = ADVANCED_FACE ( 'NONE', ( #69648 ), #10232, .F. ) ;
#17675 = CYLINDRICAL_SURFACE ( 'NONE', #29486, 0.5000000000000004441 ) ;
#17676 = DIRECTION ( 'NONE',  ( 0.000000000000000000, 0.000000000000000000, -1.000000000000000000 ) ) ;
#17677 = CARTESIAN_POINT ( 'NONE',  ( -22.25000000000000711, 33.74999999999999289, -4.000000000000000000 ) ) ;
#17678 = ORIENTED_EDGE ( 'NONE', *, *, #46951, .F. ) ;
#17680 = EDGE_CURVE ( 'NONE', #9757, #2410, #30355, .T. ) ;
#17679 = ORIENTED_EDGE ( 'NONE', *, *, #14888, .T. ) ;
#17681 = FACE_OUTER_BOUND ( 'NONE', #28042, .T. ) ;
#17682 = AXIS2_PLACEMENT_3D ( 'NONE', #44070, #33131, #7757 ) ;
#17683 = FACE_OUTER_BOUND ( 'NONE', #58386, .T. ) ;
#17684 = CARTESIAN_POINT ( 'NONE',  ( -81.50499999999999545, -6.826472737025115478, -4.959722759717899443 ) ) ;
#17685 = ORIENTED_EDGE ( 'NONE', *, *, #59289, .T. ) ;
#17686 = LINE ( 'NONE', #34870, #10420 ) ;
#17687 = SURFACE_STYLE_USAGE ( .BOTH. , #66903 ) ;
#17688 = CARTESIAN_POINT ( 'NONE',  ( -74.29315614335106943, 8.620779964796561501, -6.438673729883925390 ) ) ;
#17689 = VERTEX_POINT ( 'NONE', #47922 ) ;
#17690 = SURFACE_STYLE_FILL_AREA ( #12724 ) ;
#17691 = CARTESIAN_POINT ( 'NONE',  ( -75.00000000000000000, -2.215169945516535778E-14, -9.500000000000000000 ) ) ;
#17692 = ADVANCED_FACE ( 'NONE', ( #21820 ), #11598, .F. ) ;
#17693 = CARTESIAN_POINT ( 'NONE',  ( -9.058813317711337021, 134.0449999999999875, -2.943386871421374895 ) ) ;
#17694 = CARTESIAN_POINT ( 'NONE',  ( -102.4449999999999932, 0.000000000000000000, 8.024999999999991473 ) ) ;
#17695 = LINE ( 'NONE', #2475, #63990 ) ;
#17696 = ADVANCED_FACE ( 'NONE', ( #65763 ), #9109, .F. ) ;
#17697 = CARTESIAN_POINT ( 'NONE',  ( 66.49999999999998579, 37.00000000000000000, 3.750000000000000000 ) ) ;
#17698 = CARTESIAN_POINT ( 'NONE',  ( -148.3429263765338249, -9.058813317711329915, 2.943386871421371787 ) ) ;
#17699 = SURFACE_SIDE_STYLE ('',( #11708 ) ) ;
#17700 = CARTESIAN_POINT ( 'NONE',  ( -168.1449999999999818, -4.716976649647092401, 6.492361379858946790 ) ) ;
#17701 = COLOUR_RGB ( '', 0.31764706, 0.68627451, 0.89019608) ;
#17702 = CIRCLE ( 'NONE', #28900, 0.2500000000000002220 ) ;
#17703 = AXIS2_PLACEMENT_3D ( 'NONE', #14804, #15853, #10214 ) ;
#17704 = CARTESIAN_POINT ( 'NONE',  ( 4.250000000000001776, 21.99999999999998579, -4.000000000000000000 ) ) ;
#17705 = DIRECTION ( 'NONE',  ( 0.000000000000000000, 0.000000000000000000, 1.000000000000000000 ) ) ;
#17706 = ORIENTED_EDGE ( 'NONE', *, *, #40356, .T. ) ;
#17707 = DIRECTION ( 'NONE',  ( -0.000000000000000000, 0.000000000000000000, -1.000000000000000000 ) ) ;
#17708 = EDGE_LOOP ( 'NONE', ( #49619, #68445, #2036, #66810 ) ) ;
#17709 = CARTESIAN_POINT ( 'NONE',  ( -67.79292637653381348, -3.094860106618429807, 9.524999999999991473 ) ) ;
#17710 = CARTESIAN_POINT ( 'NONE',  ( 20.00000000000001776, 14.00000000000000000, 29.68999999999999417 ) ) ;
#17711 = DIRECTION ( 'NONE',  ( -1.000000000000000000, 0.000000000000000000, 0.000000000000000000 ) ) ;
#17712 = DIRECTION ( 'NONE',  ( 0.000000000000000000, 0.000000000000000000, -1.000000000000000000 ) ) ;
#17713 = AXIS2_PLACEMENT_3D ( 'NONE', #18991, #52444, #51037 ) ;
#17714 = VERTEX_POINT ( 'NONE', #28801 ) ;
#17715 = CARTESIAN_POINT ( 'NONE',  ( -170.1550000000000011, 7.632228543268600340, 2.479861379858949277 ) ) ;
#17716 = VERTEX_POINT ( 'NONE', #50283 ) ;
#17717 = CARTESIAN_POINT ( 'NONE',  ( -74.75000000000000000, -3.000000000000000000, 7.000000000000001776 ) ) ;
#17719 = ADVANCED_FACE ( 'NONE', ( #39068 ), #29505, .T. ) ;
#17718 = CARTESIAN_POINT ( 'NONE',  ( 60.00000000000000000, 147.4999999999999716, -9.500000000000000000 ) ) ;
#17720 =( NAMED_UNIT ( * ) PLANE_ANGLE_UNIT ( ) SI_UNIT ( $, .RADIAN. ) );
#17721 = CARTESIAN_POINT ( 'NONE',  ( -40.99999999999997868, 10.49999999999998046, -3.000000000000000444 ) ) ;
#17722 = CARTESIAN_POINT ( 'NONE',  ( 2.607480562269071989, 149.7070736234661581, 8.025000000000002132 ) ) ;
#17723 = APPLICATION_CONTEXT ( 'automotive_design' ) ;
#17724 = VERTEX_POINT ( 'NONE', #17267 ) ;
#17725 = ADVANCED_FACE ( 'NONE', ( #33404 ), #11300, .T. ) ;
#17726 =( NAMED_UNIT ( * ) SI_UNIT ( $, .STERADIAN. ) SOLID_ANGLE_UNIT ( ) );
#17727 = CARTESIAN_POINT ( 'NONE',  ( -79.10499999999998977, -6.826472737025113702, 4.959722759717902107 ) ) ;
#17728 = CARTESIAN_POINT ( 'NONE',  ( 8.102448949553181734, 130.5049999999999670, 5.886773742842750679 ) ) ;
#17729 = SURFACE_STYLE_FILL_AREA ( #28930 ) ;
#17730 = CARTESIAN_POINT ( 'NONE',  ( -91.70707362346730918, -3.094860106637120190, -9.524999999986416555 ) ) ;
#17731 = EDGE_CURVE ( 'NONE', #40860, #13573, #39405, .T. ) ;
#17732 = CARTESIAN_POINT ( 'NONE',  ( -72.50707362346616947, 8.102448949553176405, 5.886773742842740909 ) ) ;
#17733 = CARTESIAN_POINT ( 'NONE',  ( -113.5429263765338135, 9.058813317711329915, 2.943386871421369566 ) ) ;
#17734 = FILL_AREA_STYLE ('',( #18419 ) ) ;
#17735 = ORIENTED_EDGE ( 'NONE', *, *, #54628, .F. ) ;
#17736 = CARTESIAN_POINT ( 'NONE',  ( 23.71231517720798010, 117.4999999999999716, 7.000000000000000000 ) ) ;
#17737 = CARTESIAN_POINT ( 'NONE',  ( -67.34499999999998465, 7.632228543268599452, -2.479861379858951942 ) ) ;
#17738 = ORIENTED_EDGE ( 'NONE', *, *, #36755, .T. ) ;
#17739 = CARTESIAN_POINT ( 'NONE',  ( -4.750000000000002665, 24.74999999999998579, -3.750000000000000000 ) ) ;
#17740 = CARTESIAN_POINT ( 'NONE',  ( 11.00000000000001776, -0.1486183402614471571, 18.42691897641805099 ) ) ;
#17741 = AXIS2_PLACEMENT_3D ( 'NONE', #48858, #3888, #52817 ) ;
#17742 = ORIENTED_EDGE ( 'NONE', *, *, #21060, .F. ) ;
#17743 = PRESENTATION_STYLE_ASSIGNMENT (( #38879 ) ) ;
#17744 = CARTESIAN_POINT ( 'NONE',  ( -50.69499999999998607, -8.437984349512086979, 5.166775262442717831E-16 ) ) ;
#17745 = FILL_AREA_STYLE_COLOUR ( '', #10128 ) ;
#17746 = ORIENTED_EDGE ( 'NONE', *, *, #19280, .F. ) ;
#17747 = CIRCLE ( 'NONE', #43631, 0.2500000000000002220 ) ;
#17748 = ADVANCED_FACE ( 'NONE', ( #2005 ), #27370, .T. ) ;
#17749 = CARTESIAN_POINT ( 'NONE',  ( -74.23282891375464487, 8.859195963244939520, 6.389740745940710731 ) ) ;
#17750 = CARTESIAN_POINT ( 'NONE',  ( -118.4049999999999869, -2.607480562269069768, 8.024999999999991473 ) ) ;
#17751 = ORIENTED_EDGE ( 'NONE', *, *, #57620, .T. ) ;
#17752 = SURFACE_SIDE_STYLE ('',( #28616 ) ) ;
#17753 = CYLINDRICAL_SURFACE ( 'NONE', #53332, 9.524999999999991473 ) ;
#17754 =( LENGTH_UNIT ( ) NAMED_UNIT ( * ) SI_UNIT ( .MILLI., .METRE. ) );
#17755 =( GEOMETRIC_REPRESENTATION_CONTEXT ( 3 ) GLOBAL_UNCERTAINTY_ASSIGNED_CONTEXT ( ( #69309 ) ) GLOBAL_UNIT_ASSIGNED_CONTEXT ( ( #59714, #54764, #13598 ) ) REPRESENTATION_CONTEXT ( 'NONE', 'WORKASPACE' ) );
#17756 = CARTESIAN_POINT ( 'NONE',  ( -145.7070736234661297, -3.094860106618431139, -9.524999999999991473 ) ) ;
#17757 = PRODUCT_DEFINITION_SHAPE ( 'NONE', 'NONE',  #69717 ) ;
#17758 = CARTESIAN_POINT ( 'NONE',  ( -9.058813317711338797, 137.3449999999999989, 2.943386871421373563 ) ) ;
#17759 = CARTESIAN_POINT ( 'NONE',  ( -89.15707362346617515, -9.058813317711329915, -2.943386871421370898 ) ) ;
#17760 = DIRECTION ( 'NONE',  ( -0.000000000000000000, -1.000000000000000000, 0.000000000000000000 ) ) ;
#17761 = ORIENTED_EDGE ( 'NONE', *, *, #1773, .T. ) ;
#17762 = CARTESIAN_POINT ( 'NONE',  ( -71.75000000000000000, -0.9999999999999995559, 19.00000000000000000 ) ) ;
#17763 = AXIS2_PLACEMENT_3D ( 'NONE', #59887, #64821, #32817 ) ;
#17765 =( NAMED_UNIT ( * ) SI_UNIT ( $, .STERADIAN. ) SOLID_ANGLE_UNIT ( ) );
#17764 = SURFACE_STYLE_USAGE ( .BOTH. , #44532 ) ;
#17766 =( GEOMETRIC_REPRESENTATION_CONTEXT ( 3 ) GLOBAL_UNCERTAINTY_ASSIGNED_CONTEXT ( ( #42590 ) ) GLOBAL_UNIT_ASSIGNED_CONTEXT ( ( #7668, #34741, #8025 ) ) REPRESENTATION_CONTEXT ( 'NONE', 'WORKASPACE' ) );
#17767 = CARTESIAN_POINT ( 'NONE',  ( -128.7549999999999955, 4.716976649647091513, -6.492361379858946790 ) ) ;
#17768 = FACE_OUTER_BOUND ( 'NONE', #59642, .T. ) ;
#17769 = DIRECTION ( 'NONE',  ( -0.000000000000000000, -1.000000000000000000, 0.000000000000000000 ) ) ;
#17770 = CYLINDRICAL_SURFACE ( 'NONE', #24155, 1.000000000000001998 ) ;
#17771 = CARTESIAN_POINT ( 'NONE',  ( -135.5949999999999989, 2.607480562269073321, 8.024999999999991473 ) ) ;
#17772 = CARTESIAN_POINT ( 'NONE',  ( -126.7449999999999903, 4.716976649647094177, 6.492361379858945902 ) ) ;
#17773 = ADVANCED_FACE ( 'NONE', ( #11233 ), #42955, .T. ) ;
#17774 = ORIENTED_EDGE ( 'NONE', *, *, #47398, .T. ) ;
#17775 = FACE_OUTER_BOUND ( 'NONE', #68156, .T. ) ;
#17776 =( LENGTH_UNIT ( ) NAMED_UNIT ( * ) SI_UNIT ( .MILLI., .METRE. ) );
#17777 = DIRECTION ( 'NONE',  ( 0.000000000000000000, 1.000000000000000000, -0.000000000000000000 ) ) ;
#17778 = CARTESIAN_POINT ( 'NONE',  ( -177.5929263765337680, -3.094860106618431139, -9.524999999999991473 ) ) ;
#17779 = CARTESIAN_POINT ( 'NONE',  ( -57.14499999999997470, -4.716976649647092401, 6.492361379858946790 ) ) ;
#17780 = FACE_OUTER_BOUND ( 'NONE', #46278, .T. ) ;
#17781 = SURFACE_STYLE_USAGE ( .BOTH. , #11443 ) ;
#17782 = SURFACE_STYLE_USAGE ( .BOTH. , #44886 ) ;
#17783 = DIRECTION ( 'NONE',  ( 1.000000000000000000, 0.000000000000000000, 0.000000000000000000 ) ) ;
#17784 = PRODUCT_DEFINITION_CONTEXT ( 'detailed design', #58591, 'design' ) ;
#17785 = CARTESIAN_POINT ( 'NONE',  ( -94.94292637653380496, 0.000000000000000000, 9.524999999999991473 ) ) ;
#17786 = SHAPE_DEFINITION_REPRESENTATION ( #63622, #46015 ) ;
#17787 = SURFACE_SIDE_STYLE ('',( #60661 ) ) ;
#17788 = LINE ( 'NONE', #49128, #53914 ) ;
#17789 = CYLINDRICAL_SURFACE ( 'NONE', #23630, 0.5000000000000004441 ) ;
#17790 = CARTESIAN_POINT ( 'NONE',  ( -163.3429263765337964, -9.058813317711329915, 2.943386871421371787 ) ) ;
#17791 = PRESENTATION_LAYER_ASSIGNMENT (  '', '', ( #49277 ) ) ;
#17792 = CARTESIAN_POINT ( 'NONE',  ( -74.99999999999998579, 50.00000000000000000, 10.00000000000000000 ) ) ;
#17793 = ORIENTED_EDGE ( 'NONE', *, *, #55670, .F. ) ;
#17794 = DIRECTION ( 'NONE',  ( 1.000000000000000000, 0.000000000000000000, 1.073081856240828813E-16 ) ) ;
#17795 = EDGE_CURVE ( 'NONE', #57518, #11461, #32625, .T. ) ;
#17796 = DIRECTION ( 'NONE',  ( -1.000000000000000000, 0.000000000000000000, 0.000000000000000000 ) ) ;
#17797 = ORIENTED_EDGE ( 'NONE', *, *, #7814, .T. ) ;
#17798 = CARTESIAN_POINT ( 'NONE',  ( 0.000000000000000000, 121.0570736234661524, -8.025000000000000355 ) ) ;
#17799 = CARTESIAN_POINT ( 'NONE',  ( 17.15973193263811680, -3.000000000000000000, -12.50000000000000000 ) ) ;
#17800 = CARTESIAN_POINT ( 'NONE',  ( 0.000000000000000000, 0.000000000000000000, 1.000000000000000000 ) ) ;
#17801 = MECHANICAL_DESIGN_GEOMETRIC_PRESENTATION_REPRESENTATION (  '', ( #36970 ), #69465 ) ;
#17802 = EDGE_LOOP ( 'NONE', ( #17875, #18652, #19881, #40822 ) ) ;
#17803 = EDGE_CURVE ( 'NONE', #66756, #24087, #2233, .T. ) ;
#17804 = ORIENTED_EDGE ( 'NONE', *, *, #6267, .T. ) ;
#17805 = CARTESIAN_POINT ( 'NONE',  ( 34.99999999999992895, 109.9999999999999858, -9.500000000000000000 ) ) ;
#17806 = EDGE_CURVE ( 'NONE', #13013, #11552, #68608, .T. ) ;
#17807 = EDGE_CURVE ( 'NONE', #21355, #14431, #55116, .T. ) ;
#17808 = FACE_OUTER_BOUND ( 'NONE', #32806, .T. ) ;
#17809 = CARTESIAN_POINT ( 'NONE',  ( -90.14499999999999602, -4.716976649647092401, 6.492361379858946790 ) ) ;
#17810 = ORIENTED_EDGE ( 'NONE', *, *, #12602, .T. ) ;
#17811 = CARTESIAN_POINT ( 'NONE',  ( -20.40110905463057023, 114.8435661791816358, -10.33328836125512851 ) ) ;
#17812 = CARTESIAN_POINT ( 'NONE',  ( 45.58253334211660501, 9.942242644401712681, 6.446113437190048145 ) ) ;
#17813 = ADVANCED_FACE ( 'NONE', ( #2340 ), #29829, .T. ) ;
#17814 = DIRECTION ( 'NONE',  ( 0.000000000000000000, 0.000000000000000000, 1.000000000000000000 ) ) ;
#17815 = ORIENTED_EDGE ( 'NONE', *, *, #16715, .F. ) ;
#17816 = DIRECTION ( 'NONE',  ( 0.000000000000000000, 1.000000000000000000, 0.000000000000000000 ) ) ;
#17817 = ADVANCED_FACE ( 'NONE', ( #40767 ), #1667, .T. ) ;
#17818 = CARTESIAN_POINT ( 'NONE',  ( -54.93556801395976663, -8.762778093175660032, -2.499999999999992895 ) ) ;
#17819 = ORIENTED_EDGE ( 'NONE', *, *, #21464, .F. ) ;
#17820 = CARTESIAN_POINT ( 'NONE',  ( -4.041451884327381450, 7.000000000000006217, 7.500000000000000000 ) ) ;
#17821 = ORIENTED_EDGE ( 'NONE', *, *, #3288, .F. ) ;
#17822 = FACE_OUTER_BOUND ( 'NONE', #14981, .T. ) ;
#17823 = SURFACE_STYLE_USAGE ( .BOTH. , #13214 ) ;
#17824 = DIRECTION ( 'NONE',  ( 0.3420201433256660484, -0.9396926207859094271, 0.000000000000000000 ) ) ;
#17825 = PRESENTATION_LAYER_ASSIGNMENT (  '', '', ( #14391 ) ) ;
#17826 = CARTESIAN_POINT ( 'NONE',  ( -180.0570736234661808, 0.000000000000000000, 9.524999999999991473 ) ) ;
#17827 = DIRECTION ( 'NONE',  ( 0.000000000000000000, 0.000000000000000000, 1.000000000000000000 ) ) ;
#17828 =( LENGTH_UNIT ( ) NAMED_UNIT ( * ) SI_UNIT ( .MILLI., .METRE. ) );
#17829 = CARTESIAN_POINT ( 'NONE',  ( -110.4570736234661723, -9.058813317711329915, 2.943386871421371787 ) ) ;
#17830 = DIRECTION ( 'NONE',  ( 1.156482317317873451E-16, 1.000000000000000000, -0.000000000000000000 ) ) ;
#17831 = CARTESIAN_POINT ( 'NONE',  ( -48.00000000000000000, 13.41640786499872284, -9.500000000000000000 ) ) ;
#17832 = ORIENTED_EDGE ( 'NONE', *, *, #62690, .F. ) ;
#17833 = AXIS2_PLACEMENT_3D ( 'NONE', #45229, #47600, #20087 ) ;
#17834 = DIRECTION ( 'NONE',  ( -0.000000000000000000, -0.000000000000000000, -1.000000000000000000 ) ) ;
#17835 = DIRECTION ( 'NONE',  ( 1.000000000000000000, 0.000000000000000000, 0.000000000000000000 ) ) ;
#17836 = DIRECTION ( 'NONE',  ( 0.000000000000000000, -1.000000000000000000, 0.000000000000000000 ) ) ;
#17837 = FACE_OUTER_BOUND ( 'NONE', #62153, .T. ) ;
#17838 = ORIENTED_EDGE ( 'NONE', *, *, #51315, .T. ) ;
#17839 = CARTESIAN_POINT ( 'NONE',  ( -160.2549999999999670, -4.716976649647092401, 6.492361379858946790 ) ) ;
#17840 = CARTESIAN_POINT ( 'NONE',  ( 68.99999999999998579, 8.572527594031471415E-15, -4.000000000000000000 ) ) ;
#17841 = CARTESIAN_POINT ( 'NONE',  ( -169.7949999999999875, 2.607480562269068880, -8.024999999999993250 ) ) ;
#17842 = AXIS2_PLACEMENT_3D ( 'NONE', #17435, #56061, #22684 ) ;
#17843 = CARTESIAN_POINT ( 'NONE',  ( -154.0449999999999875, 7.632228543268600340, 2.479861379858949277 ) ) ;
#17844 = ORIENTED_EDGE ( 'NONE', *, *, #40846, .T. ) ;
#17845 = CARTESIAN_POINT ( 'NONE',  ( -66.89292637653377938, -8.102448949553174629, -5.886773742842741797 ) ) ;
#17846 = CARTESIAN_POINT ( 'NONE',  ( 44.58498124287052633, 10.41703377194163949, 3.499556662980364496 ) ) ;
#17847 = SURFACE_STYLE_USAGE ( .BOTH. , #37963 ) ;
#17848 = CARTESIAN_POINT ( 'NONE',  ( -73.40500000000000114, -2.607480562269069768, 8.024999999999991473 ) ) ;
#17849 = CARTESIAN_POINT ( 'NONE',  ( 23.85560559829669458, 24.60330559701304409, 27.21038588406899805 ) ) ;
#17851 = LINE ( 'NONE', #17185, #32626 ) ;
#17850 = VECTOR ( 'NONE', #59692, 1000.000000000000114 ) ;
#17852 = CARTESIAN_POINT ( 'NONE',  ( -75.14499999999999602, -4.716976649647092401, 6.492361379858946790 ) ) ;
#17853 = CARTESIAN_POINT ( 'NONE',  ( -10.01517768586949231, 144.3049999999999784, -6.132527647946036459E-16 ) ) ;
#17854 = FACE_OUTER_BOUND ( 'NONE', #16548, .T. ) ;
#17855 = LINE ( 'NONE', #32627, #6858 ) ;
#17856 = UNCERTAINTY_MEASURE_WITH_UNIT (LENGTH_MEASURE( 1.000000000000000082E-05 ), #56252, 'distance_accuracy_value', 'NONE');
#17857 =( NAMED_UNIT ( * ) PLANE_ANGLE_UNIT ( ) SI_UNIT ( $, .RADIAN. ) );
#17858 = FACE_OUTER_BOUND ( 'NONE', #58666, .T. ) ;
#17859 = VECTOR ( 'NONE', #18105, 1000.000000000000000 ) ;
#17860 = FACE_OUTER_BOUND ( 'NONE', #19971, .T. ) ;
#17861 = CIRCLE ( 'NONE', #42610, 0.5000000000000004441 ) ;
#17862 = EDGE_CURVE ( 'NONE', #40174, #30006, #6874, .T. ) ;
#17863 = AXIS2_PLACEMENT_3D ( 'NONE', #14740, #41846, #52390 ) ;
#17864 = CARTESIAN_POINT ( 'NONE',  ( -44.99999999999977973, 146.4999999999999716, -7.000000000000000000 ) ) ;
#17865 = ORIENTED_EDGE ( 'NONE', *, *, #52082, .T. ) ;
#17866 = VERTEX_POINT ( 'NONE', #18909 ) ;
#17867 = CARTESIAN_POINT ( 'NONE',  ( 48.00000000000000000, 13.41640786499872462, 9.500000000000000000 ) ) ;
#17868 = STYLED_ITEM ( 'NONE', ( #9004 ), #4500 ) ;
#17869 = EDGE_CURVE ( 'NONE', #18515, #22486, #54071, .T. ) ;
#17870 = CARTESIAN_POINT ( 'NONE',  ( 0.000000000000000000, 0.000000000000000000, 7.500000000000000000 ) ) ;
#17871 = CARTESIAN_POINT ( 'NONE',  ( 14.98999599679679662, 118.4999999999999716, 10.00000000000000000 ) ) ;
#17872 = DIRECTION ( 'NONE',  ( 1.000000000000000000, 0.000000000000000000, 0.000000000000000000 ) ) ;
#17873 = EDGE_CURVE ( 'NONE', #31107, #24916, #14784, .T. ) ;
#17874 = FILL_AREA_STYLE ('',( #29452 ) ) ;
#17875 = ORIENTED_EDGE ( 'NONE', *, *, #32399, .T. ) ;
#17876 = CARTESIAN_POINT ( 'NONE',  ( -111.8049999999999784, -8.437984349512086979, 5.166775262442717831E-16 ) ) ;
#17877 = ORIENTED_EDGE ( 'NONE', *, *, #60811, .T. ) ;
#17878 =( NAMED_UNIT ( * ) PLANE_ANGLE_UNIT ( ) SI_UNIT ( $, .RADIAN. ) );
#17879 = ORIENTED_EDGE ( 'NONE', *, *, #1122, .F. ) ;
#17880 = DIRECTION ( 'NONE',  ( 1.300977106640434891E-16, -0.000000000000000000, 1.000000000000000000 ) ) ;
#17881 = DIRECTION ( 'NONE',  ( 0.000000000000000000, 1.000000000000000000, 0.000000000000000000 ) ) ;
#17882 = ORIENTED_EDGE ( 'NONE', *, *, #10386, .T. ) ;
#17883 = ADVANCED_FACE ( 'NONE', ( #31198 ), #68517, .F. ) ;
#17884 = AXIS2_PLACEMENT_3D ( 'NONE', #34529, #12367, #2469 ) ;
#17885 = DIRECTION ( 'NONE',  ( -1.000000000000000000, -0.000000000000000000, 0.000000000000000000 ) ) ;
#17886 = CARTESIAN_POINT ( 'NONE',  ( 8.750000000000001776, 25.24999999999998934, 3.750000000000000000 ) ) ;
#17887 = VERTEX_POINT ( 'NONE', #10126 ) ;
#17888 = CIRCLE ( 'NONE', #68407, 0.5000000000000004441 ) ;
#17889 = ORIENTED_EDGE ( 'NONE', *, *, #18741, .T. ) ;
#17890 = CARTESIAN_POINT ( 'NONE',  ( 179.4098300562505415, 6.123233995736766282E-16, -5.000000000000000000 ) ) ;
#17891 = LINE ( 'NONE', #45696, #29446 ) ;
#17892 = DIRECTION ( 'NONE',  ( 0.000000000000000000, -0.000000000000000000, 1.000000000000000000 ) ) ;
#17893 = EDGE_CURVE ( 'NONE', #11547, #45027, #62147, .T. ) ;
#17894 = CARTESIAN_POINT ( 'NONE',  ( 0.000000000000000000, 0.000000000000000000, 0.000000000000000000 ) ) ;
#17895 = EDGE_LOOP ( 'NONE', ( #56185, #46849, #48201, #58475 ) ) ;
#17896 = CARTESIAN_POINT ( 'NONE',  ( -7.632228543268607446, 135.5429263765338135, -2.479861379858953718 ) ) ;
#17897 = DIRECTION ( 'NONE',  ( 0.000000000000000000, 0.000000000000000000, 1.000000000000000000 ) ) ;
#17898 = CIRCLE ( 'NONE', #46042, 26.99999999999999645 ) ;
#17899 = PLANE ( 'NONE',  #28899 ) ;
#17900 = EDGE_LOOP ( 'NONE', ( #68862, #18044, #66549, #8829 ) ) ;
#17901 = ORIENTED_EDGE ( 'NONE', *, *, #47156, .F. ) ;
#17902 = PRESENTATION_STYLE_ASSIGNMENT (( #66426 ) ) ;
#17903 = LINE ( 'NONE', #39388, #46820 ) ;
#17904 = CARTESIAN_POINT ( 'NONE',  ( -129.0549999999999784, -9.827790563157499189E-16, -8.024999999999991473 ) ) ;
#17905 = SURFACE_SIDE_STYLE ('',( #1672 ) ) ;
#17906 = AXIS2_PLACEMENT_3D ( 'NONE', #59668, #1573, #17493 ) ;
#17907 = ORIENTED_EDGE ( 'NONE', *, *, #28091, .F. ) ;
#17908 = DIRECTION ( 'NONE',  ( -0.000000000000000000, -0.000000000000000000, -1.000000000000000000 ) ) ;
#17909 = CARTESIAN_POINT ( 'NONE',  ( -106.8570736234661780, -5.598654528085803328, -7.705886871421366635 ) ) ;
#17910 =( NAMED_UNIT ( * ) PLANE_ANGLE_UNIT ( ) SI_UNIT ( $, .RADIAN. ) );
#17911 = ORIENTED_EDGE ( 'NONE', *, *, #54468, .T. ) ;
#17912 = VERTEX_POINT ( 'NONE', #20314 ) ;
#17913 = FILL_AREA_STYLE_COLOUR ( '', #62000 ) ;
#17914 = CARTESIAN_POINT ( 'NONE',  ( 4.041451884327375232, -1.417096231345241097, -7.000000000000002665 ) ) ;
#17915 = DIRECTION ( 'NONE',  ( -0.000000000000000000, 1.000000000000000000, -0.000000000000000000 ) ) ;
#17916 = EDGE_LOOP ( 'NONE', ( #26563, #45463, #52946, #11632 ) ) ;
#17917 = CARTESIAN_POINT ( 'NONE',  ( -44.99154893936433552, 9.591540374752312914, 3.500000000000000000 ) ) ;
#17918 = DIRECTION ( 'NONE',  ( -1.000000000000000000, 0.000000000000000000, 0.000000000000000000 ) ) ;
#17919 = DIRECTION ( 'NONE',  ( 0.000000000000000000, 0.000000000000000000, 1.000000000000000000 ) ) ;
#17920 = COLOUR_RGB ( '', 0.08235294, 0.09019608, 0.10196078) ;
#17921 = CARTESIAN_POINT ( 'NONE',  ( 22.99999999999995026, 5.000000000000000000, -32.00402776293824303 ) ) ;
#17922 = ORIENTED_EDGE ( 'NONE', *, *, #19932, .T. ) ;
#17923 = ADVANCED_FACE ( 'NONE', ( #62527 ), #36882, .T. ) ;
#17924 = AXIS2_PLACEMENT_3D ( 'NONE', #18811, #34998, #29725 ) ;
#17925 = PRESENTATION_STYLE_ASSIGNMENT (( #60810 ) ) ;
#17926 = DIRECTION ( 'NONE',  ( -0.000000000000000000, -0.000000000000000000, 1.000000000000000000 ) ) ;
#17927 = CARTESIAN_POINT ( 'NONE',  ( 4.716976649647096842, 116.8570736234661638, 6.492361379858953896 ) ) ;
#17928 = CARTESIAN_POINT ( 'NONE',  ( 5.728833613173035744, 154.5000000000000568, -7.622147220416790603 ) ) ;
#17929 = TOROIDAL_SURFACE ( 'NONE', #47203, 0.5000000000000000000, 0.2500000000000000000 ) ;
#17930 = DIRECTION ( 'NONE',  ( 1.000000000000000000, 0.000000000000000000, 0.000000000000000000 ) ) ;
#17931 = CARTESIAN_POINT ( 'NONE',  ( -103.3449999999999989, 7.632228543268599452, -2.479861379858951942 ) ) ;
#17932 = CARTESIAN_POINT ( 'NONE',  ( 3.094860106618435136, 116.4049999999999869, -9.525000000000000355 ) ) ;
#17933 = CARTESIAN_POINT ( 'NONE',  ( -79.34499999999998465, 7.632228543268599452, -2.479861379858951942 ) ) ;
#17934 = DIRECTION ( 'NONE',  ( 0.000000000000000000, 0.000000000000000000, -1.000000000000000000 ) ) ;
#17935 = VECTOR ( 'NONE', #10244, 1000.000000000000000 ) ;
#17936 = CARTESIAN_POINT ( 'NONE',  ( -7.632228543268608334, 141.8429263765338249, 2.479861379858952830 ) ) ;
#17937 = CARTESIAN_POINT ( 'NONE',  ( 8.000000000000001776, 31.24999999999998579, -3.750000000000000000 ) ) ;
#17938 = CARTESIAN_POINT ( 'NONE',  ( -5.356721384544675502, 2.367558512213879141, -4.721886399977922366 ) ) ;
#17939 = UNCERTAINTY_MEASURE_WITH_UNIT (LENGTH_MEASURE( 1.000000000000000082E-05 ), #33564, 'distance_accuracy_value', 'NONE');
#17940 = AXIS2_PLACEMENT_3D ( 'NONE', #61423, #3706, #56507 ) ;
#17941 = LINE ( 'NONE', #8080, #61054 ) ;
#17942 = ORIENTED_EDGE ( 'NONE', *, *, #61776, .T. ) ;
#17943 = CARTESIAN_POINT ( 'NONE',  ( -125.5429263765337993, 9.058813317711329915, 2.943386871421369566 ) ) ;
#17944 =( LENGTH_UNIT ( ) NAMED_UNIT ( * ) SI_UNIT ( .MILLI., .METRE. ) );
#17945 = CARTESIAN_POINT ( 'NONE',  ( -136.7949999999999875, 2.607480562269068880, -8.024999999999993250 ) ) ;
#17946 = SURFACE_SIDE_STYLE ('',( #34803 ) ) ;
#17947 = STYLED_ITEM ( 'NONE', ( #50635 ), #69178 ) ;
#17948 = EDGE_CURVE ( 'NONE', #37046, #46653, #65188, .T. ) ;
#17949 = ADVANCED_FACE ( 'NONE', ( #51641 ), #38363, .F. ) ;
#17950 = PLANE ( 'NONE',  #29570 ) ;
#17951 = ORIENTED_EDGE ( 'NONE', *, *, #65456, .F. ) ;
#17952 = ORIENTED_EDGE ( 'NONE', *, *, #18692, .F. ) ;
#17953 = MECHANICAL_DESIGN_GEOMETRIC_PRESENTATION_REPRESENTATION (  '', ( #22417 ), #20145 ) ;
#17954 = MECHANICAL_DESIGN_GEOMETRIC_PRESENTATION_REPRESENTATION (  '', ( #18003 ), #40529 ) ;
#17955 =( BOUNDED_SURFACE ( )  B_SPLINE_SURFACE ( 1, 2, ( 
 ( #7332, #8710, #13271, #30134, #61453, #1964, #61795, #24511, #3376, #55852, #7651, #13625, #56183, #51276, #29087, #46383, #66403, #39705, #24869, #12937, #34399, #8009, #35086, #56536, #8378, #29811, #20293, #47434, #52343, #57594, #35790, #57232, #25228, #9770, #36866, #68502, #15737, #4811, #37218, #30845, #31180, #4091, #30485, #68856, #14690, #5151, #51981, #15063, #9422, #42848, #46747, #52672, #36535, #25559, #42169, #4439, #64242, #20998, #9065, #69197, #63220, #58631, #47074, #3736, #20657, #26263, #53018, #36164, #41799, #25910, #57955, #31537, #63561, #26596, #58279, #68157, #15406, #69522, #53366, #10107, #47799, #42496, #10454, #19944, #21326, #63888, #41437, #31887, #48119, #62849, #13116, #39898, #16455, #60593, #18414, #2517, #5836, #29287, #59293, #39197, #7838, #27275, #23330, #32240, #43205, #513, #44495, #56022, #37582, #21686, #50768, #66595, #18058, #48462, #65898, #24026, #23000, #34569, #28590, #61305, #45534, #11119, #32569, #60948, #33872, #54031, #48815, #16100, #58979, #50087, #12766, #2141, #7160, #17728, #12411, #55335, #10792, #1815, #44828, #66232, #64609, #39543, #53688, #50416, #37918, #34238, #155, #55692, #23672, #7500, #28929, #45176, #5474, #26925, #3205, #68336, #62680, #56372, #19438, #8209, #66950, #46216, #35636, #51818, #57787, #13822, #31029, #68003, #45854, #57072, #4268, #61994, #40228, #40580, #25749, #52181, #29991, #14507, #29656, #34926, #35283, #30314, #56746, #52523, #8889, #2870, #35983, #57428, #40935, #18747, #3940, #25411, #67636, #3567, #46926, #9257, #24698, #9612, #62357, #30673, #8558, #20116, #25069, #14180, #51455, #61633, #13458, #41624, #51123, #63042, #46578, #19791, #41283, #24359, #14884, #67285, #36367, #19074, #32770, #48296, #15934, #36718, #58817, #43395, #37765, #10967, #21168, #9943, #59141, #37053, #54219, #27118, #32405, #6035, #26769, #28187, #21520, #31366, #10293, #53208, #4993, #64786, #31724, #43037, #16623, #26446, #4642, #59487, #58133, #15250, #68688, #53872, #350, #38089, #37416, #47266, #42680, #11313, #10632, #26097, #20486, #32083, #64442, #41993, #52864, #21885, #47629, #63403, #69036, #47978, #20847, #42347, #63731, #16289, #64081, #15579, #58468, #69377, #53540, #5326, #5669, #48651, #17658, #28144, #49652, #22567, #61233, #44424, #44069, #1397, #54567, #60197, #28859, #60872, #688, #13044, #45104, #39468, #6375, #39818, #65110, #50341, #22220, #17981, #12004, #39126, #65473, #49309, #27472, #48999, #16964, #22925, #28509, #33465, #7437, #66151, #2065, #17324, #65826, #38784, #43715, #60516, #27803, #66516, #38451, #6717, #1020, #34498, #59851, #12328, #33801, #54890, #55252, #7078, #55950, #12685, #11660, #34156, #50011, #23593, #1749 ),
 ( #18338, #23259, #33130, #44756, #55614, #25329, #18990, #14097, #67916, #30587, #29199, #41534, #8482, #14796, #2795, #19708, #3844, #46850, #52094, #8123, #51375, #9171, #62950, #67201, #20035, #51036, #29916, #68255, #40499, #35557, #23941, #34839, #61916, #35196, #36273, #50687, #13378, #7756, #57337, #8807, #40157, #56655, #2430, #13736, #45454, #19349, #66874, #18679, #24284, #61551, #56291, #24613, #3118, #45781, #56994, #46130, #29566, #62604, #67552, #41203, #40853, #62270, #30232, #51730, #3478, #46490, #24979, #14418, #35891, #47896, #20761, #53459, #58054, #48562, #58730, #16543, #53119, #21793, #5581, #68952, #63993, #48211, #10887, #9527, #43306, #58378, #64705, #52778, #69619, #53779, #27028, #32328, #9861, #31640, #59068, #57698, #47538, #258, #31279, #10203, #30946, #42269, #15842, #4187, #15165, #63657, #15500, #52443, #25662, #63315, #47181, #37672, #10549, #20397, #36966, #68601, #4907, #41899, #69295, #36636, #4552, #26009, #26358, #31988, #21089, #42588, #37323, #5243, #26687, #21428, #42947, #64349, #16196, #38703, #60103, #33040, #1975, #54805, #54476, #11920, #65023, #926, #39376, #1661, #11223, #23497, #55521, #49922, #16881, #50256, #5937, #60775, #32672, #28410, #22477, #49567, #6290, #59758, #38003, #59390, #27382, #33380, #39039, #43975, #17896, #6989, #12595, #27721, #6615, #49219, #54126, #1299, #38356, #7345, #48913, #17237, #11568, #65390, #28056, #34065, #28772, #22832, #33708, #23179, #44332, #65729, #17574, #60436, #45011, #12243, #55157, #44669, #66062, #66419, #610, #22133, #43627, #51995, #35801, #30150, #66778, #30496, #55865, #41113, #12949, #8721, #2703, #29822, #34740, #40078, #18236, #39720, #7667, #61810, #19251, #50944, #67817, #56908, #19615, #13284, #13640, #56196, #34411, #51288, #18593, #57246, #29099, #67116, #61466, #25241, #50596, #35103, #18900, #8024, #24523, #56552, #46759, #3388, #61143, #51631, #45701, #62519, #29474, #2331, #3031, #24883, #35466, #24195, #40401, #8390, #46039, #14003, #67454, #9079, #40755, #23852, #62172, #3749, #45359, #46395, #14335, #58641, #21338, #19951, #32249, #68870, #5485, #63230, #10467, #64255, #16110, #42862, #68512, #42182, #69535, #53697, #57964, #10802, #41813, #20671, #58989, #9780, #4820, #14703, #21009, #26273, #63572, #4451, #26936, #20306, #25920, #37591, #63899, #57606, #15418, #9431, #68172, #47447, #36875, #53030, #41449, #15076, #62858, #69208, #47085, #37232, #15751, #36548, #31190, #58291, #52686, #31898, #10121, #36177, #42503, #30858, #31548, #52353, #4103, #47810, #53379, #5162, #25572, #26608, #48129, #49151, #55438, #43554, #38960, #44587, #65987, #1572, #48829, #22389, #49832, #33978, #38270, #60698, #22051, #848, #39294 ) ),
 .UNSPECIFIED., .F., .F., .F. ) 
 B_SPLINE_SURFACE_WITH_KNOTS ( ( 2, 2 ),
 ( 3, 2, 2, 2, 2, 2, 2, 2, 2, 2, 2, 2, 2, 2, 2, 2, 2, 2, 2, 2, 2, 2, 2, 2, 2, 2, 2, 2, 2, 2, 2, 2, 2, 2, 2, 2, 2, 2, 2, 2, 2, 2, 2, 2, 2, 2, 2, 2, 2, 2, 2, 2, 2, 2, 2, 2, 2, 2, 2, 2, 2, 2, 2, 2, 2, 2, 2, 2, 2, 2, 2, 2, 2, 2, 2, 2, 2, 2, 2, 2, 2, 2, 2, 2, 2, 2, 2, 2, 2, 2, 2, 2, 2, 2, 2, 2, 2, 2, 2, 2, 2, 2, 2, 2, 2, 2, 2, 2, 2, 2, 2, 2, 2, 2, 2, 2, 2, 2, 2, 2, 2, 2, 2, 2, 2, 2, 2, 2, 2, 2, 2, 2, 2, 2, 2, 2, 2, 2, 2, 2, 2, 2, 2, 2, 2, 2, 2, 2, 2, 2, 2, 2, 2, 2, 2, 2, 2, 2, 2, 2, 2, 2, 2, 2, 2, 2, 2, 2, 2, 2, 3 ),
 ( 0.000000000000000000, 1.000000000000000000 ),
 ( 0.000000000000000000, 0.005882352941176470507, 0.01176470588235294101, 0.01764705882352941152, 0.02352941176470588203, 0.02941176470588235253, 0.03529411764705882304, 0.04117647058823529355, 0.04705882352941176405, 0.05294117647058823456, 0.05882352941176470507, 0.06470588235294118251, 0.07058823529411764608, 0.07647058823529412352, 0.08235294117647058709, 0.08823529411764706454, 0.09411764705882352811, 0.1000000000000000056, 0.1058823529411764691, 0.1117647058823529466, 0.1176470588235294101, 0.1235294117647058876, 0.1294117647058823650, 0.1352941176470588147, 0.1411764705882352922, 0.1470588235294117696, 0.1529411764705882470, 0.1588235294117646967, 0.1647058823529411742, 0.1705882352941176516, 0.1764705882352941291, 0.1823529411764705788, 0.1882352941176470562, 0.1941176470588235337, 0.2000000000000000111, 0.2058823529411764608, 0.2117647058823529382, 0.2176470588235294157, 0.2235294117647058931, 0.2294117647058823428, 0.2352941176470588203, 0.2411764705882352977, 0.2470588235294117752, 0.2529411764705882248, 0.2588235294117647300, 0.2647058823529411797, 0.2705882352941176294, 0.2764705882352941346, 0.2823529411764705843, 0.2882352941176470340, 0.2941176470588235392, 0.2999999999999999889, 0.3058823529411764941, 0.3117647058823529438, 0.3176470588235293935, 0.3235294117647058987, 0.3294117647058823484, 0.3352941176470587981, 0.3411764705882353033, 0.3470588235294117530, 0.3529411764705882582, 0.3588235294117647078, 0.3647058823529411575, 0.3705882352941176627, 0.3764705882352941124, 0.3823529411764705621, 0.3882352941176470673, 0.3941176470588235170, 0.4000000000000000222, 0.4058823529411764719, 0.4117647058823529216, 0.4176470588235294268, 0.4235294117647058765, 0.4294117647058823262, 0.4352941176470588314, 0.4411764705882352811, 0.4470588235294117863, 0.4529411764705882359, 0.4588235294117646856, 0.4647058823529411908, 0.4705882352941176405, 0.4764705882352940902, 0.4823529411764705954, 0.4882352941176470451, 0.4941176470588235503, 0.5000000000000000000, 0.5058823529411764497, 0.5117647058823528994, 0.5176470588235294601, 0.5235294117647059098, 0.5294117647058823595, 0.5352941176470588092, 0.5411764705882352589, 0.5470588235294118196, 0.5529411764705882693, 0.5588235294117647189, 0.5647058823529411686, 0.5705882352941176183, 0.5764705882352940680, 0.5823529411764706287, 0.5882352941176470784, 0.5941176470588235281, 0.5999999999999999778, 0.6058823529411764275, 0.6117647058823529882, 0.6176470588235294379, 0.6235294117647058876, 0.6294117647058823373, 0.6352941176470587870, 0.6411764705882353477, 0.6470588235294117974, 0.6529411764705882470, 0.6588235294117646967, 0.6647058823529411464, 0.6705882352941175961, 0.6764705882352941568, 0.6823529411764706065, 0.6882352941176470562, 0.6941176470588235059, 0.6999999999999999556, 0.7058823529411765163, 0.7117647058823529660, 0.7176470588235294157, 0.7235294117647058654, 0.7294117647058823151, 0.7352941176470588758, 0.7411764705882353255, 0.7470588235294117752, 0.7529411764705882248, 0.7588235294117646745, 0.7647058823529411242, 0.7705882352941176849, 0.7764705882352941346, 0.7823529411764705843, 0.7882352941176470340, 0.7941176470588234837, 0.8000000000000000444, 0.8058823529411764941, 0.8117647058823529438, 0.8176470588235293935, 0.8235294117647058432, 0.8294117647058824039, 0.8352941176470588536, 0.8411764705882353033, 0.8470588235294117530, 0.8529411764705882026, 0.8588235294117646523, 0.8647058823529412130, 0.8705882352941176627, 0.8764705882352941124, 0.8823529411764705621, 0.8882352941176470118, 0.8941176470588235725, 0.9000000000000000222, 0.9058823529411764719, 0.9117647058823529216, 0.9176470588235293713, 0.9235294117647059320, 0.9294117647058823817, 0.9352941176470588314, 0.9411764705882352811, 0.9470588235294117307, 0.9529411764705881804, 0.9588235294117647411, 0.9647058823529411908, 0.9705882352941176405, 0.9764705882352940902, 0.9823529411764705399, 0.9882352941176471006, 0.9941176470588235503, 1.000000000000000000 ),
 .UNSPECIFIED. ) 
 GEOMETRIC_REPRESENTATION_ITEM ( )  RATIONAL_B_SPLINE_SURFACE ( (
 ( 1.000000000000000000, 0.9510565162951535312, 1.000000000000000000, 0.9510565162951535312, 1.000000000000000000, 0.9510565162951535312, 1.000000000000000000, 0.9510565162951535312, 1.000000000000000000, 0.9510565162951535312, 1.000000000000000000, 0.9510565162951535312, 1.000000000000000000, 0.9510565162951535312, 1.000000000000000000, 0.9510565162951535312, 1.000000000000000000, 0.9510565162951535312, 1.000000000000000000, 0.9510565162951535312, 1.000000000000000000, 0.9510565162951535312, 1.000000000000000000, 0.9510565162951535312, 1.000000000000000000, 0.9510565162951535312, 1.000000000000000000, 0.9510565162951535312, 1.000000000000000000, 0.9510565162951535312, 1.000000000000000000, 0.9510565162951535312, 1.000000000000000000, 0.9510565162951535312, 1.000000000000000000, 0.9510565162951535312, 1.000000000000000000, 0.9510565162951535312, 1.000000000000000000, 0.9510565162951535312, 1.000000000000000000, 0.9510565162951535312, 1.000000000000000000, 0.9510565162951535312, 1.000000000000000000, 0.9510565162951535312, 1.000000000000000000, 0.9510565162951535312, 1.000000000000000000, 0.9510565162951535312, 1.000000000000000000, 0.9510565162951535312, 1.000000000000000000, 0.9510565162951535312, 1.000000000000000000, 0.9510565162951535312, 1.000000000000000000, 0.9510565162951535312, 1.000000000000000000, 0.9510565162951535312, 1.000000000000000000, 0.9510565162951535312, 1.000000000000000000, 0.9510565162951535312, 1.000000000000000000, 0.9510565162951535312, 1.000000000000000000, 0.9510565162951535312, 1.000000000000000000, 0.9510565162951535312, 1.000000000000000000, 0.9510565162951535312, 1.000000000000000000, 0.9510565162951535312, 1.000000000000000000, 0.9510565162951535312, 1.000000000000000000, 0.9510565162951535312, 1.000000000000000000, 0.9510565162951535312, 1.000000000000000000, 0.9510565162951535312, 1.000000000000000000, 0.9510565162951535312, 1.000000000000000000, 0.9510565162951535312, 1.000000000000000000, 0.9510565162951535312, 1.000000000000000000, 0.9510565162951535312, 1.000000000000000000, 0.9510565162951535312, 1.000000000000000000, 0.9510565162951535312, 1.000000000000000000, 0.9510565162951535312, 1.000000000000000000, 0.9510565162951535312, 1.000000000000000000, 0.9510565162951535312, 1.000000000000000000, 0.9510565162951535312, 1.000000000000000000, 0.9510565162951535312, 1.000000000000000000, 0.9510565162951535312, 1.000000000000000000, 0.9510565162951535312, 1.000000000000000000, 0.9510565162951535312, 1.000000000000000000, 0.9510565162951535312, 1.000000000000000000, 0.9510565162951535312, 1.000000000000000000, 0.9510565162951535312, 1.000000000000000000, 0.9510565162951535312, 1.000000000000000000, 0.9510565162951535312, 1.000000000000000000, 0.9510565162951535312, 1.000000000000000000, 0.9510565162951535312, 1.000000000000000000, 0.9510565162951535312, 1.000000000000000000, 0.9510565162951535312, 1.000000000000000000, 0.9510565162951535312, 1.000000000000000000, 0.9510565162951535312, 1.000000000000000000, 0.9510565162951535312, 1.000000000000000000, 0.9510565162951535312, 1.000000000000000000, 0.9510565162951535312, 1.000000000000000000, 0.9510565162951535312, 1.000000000000000000, 0.9510565162951535312, 1.000000000000000000, 0.9510565162951535312, 1.000000000000000000, 0.9510565162951535312, 1.000000000000000000, 0.9510565162951535312, 1.000000000000000000, 0.9510565162951535312, 1.000000000000000000, 0.9510565162951535312, 1.000000000000000000, 0.9510565162951535312, 1.000000000000000000, 0.9510565162951535312, 1.000000000000000000, 0.9510565162951535312, 1.000000000000000000, 0.9510565162951535312, 1.000000000000000000, 0.9510565162951535312, 1.000000000000000000, 0.9510565162951535312, 1.000000000000000000, 0.9510565162951535312, 1.000000000000000000, 0.9510565162951535312, 1.000000000000000000, 0.9510565162951535312, 1.000000000000000000, 0.9510565162951535312, 1.000000000000000000, 0.9510565162951535312, 1.000000000000000000, 0.9510565162951535312, 1.000000000000000000, 0.9510565162951535312, 1.000000000000000000, 0.9510565162951535312, 1.000000000000000000, 0.9510565162951535312, 1.000000000000000000, 0.9510565162951535312, 1.000000000000000000, 0.9510565162951535312, 1.000000000000000000, 0.9510565162951535312, 1.000000000000000000, 0.9510565162951535312, 1.000000000000000000, 0.9510565162951535312, 1.000000000000000000, 0.9510565162951535312, 1.000000000000000000, 0.9510565162951535312, 1.000000000000000000, 0.9510565162951535312, 1.000000000000000000, 0.9510565162951535312, 1.000000000000000000, 0.9510565162951535312, 1.000000000000000000, 0.9510565162951535312, 1.000000000000000000, 0.9510565162951535312, 1.000000000000000000, 0.9510565162951535312, 1.000000000000000000, 0.9510565162951535312, 1.000000000000000000, 0.9510565162951535312, 1.000000000000000000, 0.9510565162951535312, 1.000000000000000000, 0.9510565162951535312, 1.000000000000000000, 0.9510565162951535312, 1.000000000000000000, 0.9510565162951535312, 1.000000000000000000, 0.9510565162951535312, 1.000000000000000000, 0.9510565162951535312, 1.000000000000000000, 0.9510565162951535312, 1.000000000000000000, 0.9510565162951535312, 1.000000000000000000, 0.9510565162951535312, 1.000000000000000000, 0.9510565162951535312, 1.000000000000000000, 0.9510565162951535312, 1.000000000000000000, 0.9510565162951535312, 1.000000000000000000, 0.9510565162951535312, 1.000000000000000000, 0.9510565162951535312, 1.000000000000000000, 0.9510565162951535312, 1.000000000000000000, 0.9510565162951535312, 1.000000000000000000, 0.9510565162951535312, 1.000000000000000000, 0.9510565162951535312, 1.000000000000000000, 0.9510565162951535312, 1.000000000000000000, 0.9510565162951535312, 1.000000000000000000, 0.9510565162951535312, 1.000000000000000000, 0.9510565162951535312, 1.000000000000000000, 0.9510565162951535312, 1.000000000000000000, 0.9510565162951535312, 1.000000000000000000, 0.9510565162951535312, 1.000000000000000000, 0.9510565162951535312, 1.000000000000000000, 0.9510565162951535312, 1.000000000000000000, 0.9510565162951535312, 1.000000000000000000, 0.9510565162951535312, 1.000000000000000000, 0.9510565162951535312, 1.000000000000000000, 0.9510565162951535312, 1.000000000000000000, 0.9510565162951535312, 1.000000000000000000, 0.9510565162951535312, 1.000000000000000000, 0.9510565162951535312, 1.000000000000000000, 0.9510565162951535312, 1.000000000000000000, 0.9510565162951535312, 1.000000000000000000, 0.9510565162951535312, 1.000000000000000000, 0.9510565162951535312, 1.000000000000000000, 0.9510565162951535312, 1.000000000000000000, 0.9510565162951535312, 1.000000000000000000, 0.9510565162951535312, 1.000000000000000000, 0.9510565162951535312, 1.000000000000000000, 0.9510565162951535312, 1.000000000000000000, 0.9510565162951535312, 1.000000000000000000, 0.9510565162951535312, 1.000000000000000000, 0.9510565162951535312, 1.000000000000000000, 0.9510565162951535312, 1.000000000000000000, 0.9510565162951535312, 1.000000000000000000, 0.9510565162951535312, 1.000000000000000000, 0.9510565162951535312, 1.000000000000000000, 0.9510565162951535312, 1.000000000000000000, 0.9510565162951535312, 1.000000000000000000, 0.9510565162951535312, 1.000000000000000000, 0.9510565162951535312, 1.000000000000000000, 0.9510565162951535312, 1.000000000000000000, 0.9510565162951535312, 1.000000000000000000, 0.9510565162951535312, 1.000000000000000000, 0.9510565162951535312, 1.000000000000000000, 0.9510565162951535312, 1.000000000000000000, 0.9510565162951535312, 1.000000000000000000, 0.9510565162951535312, 1.000000000000000000, 0.9510565162951535312, 1.000000000000000000, 0.9510565162951535312, 1.000000000000000000, 0.9510565162951535312, 1.000000000000000000),
 ( 1.000000000000000000, 0.9510565162951535312, 1.000000000000000000, 0.9510565162951535312, 1.000000000000000000, 0.9510565162951535312, 1.000000000000000000, 0.9510565162951535312, 1.000000000000000000, 0.9510565162951535312, 1.000000000000000000, 0.9510565162951535312, 1.000000000000000000, 0.9510565162951535312, 1.000000000000000000, 0.9510565162951535312, 1.000000000000000000, 0.9510565162951535312, 1.000000000000000000, 0.9510565162951535312, 1.000000000000000000, 0.9510565162951535312, 1.000000000000000000, 0.9510565162951535312, 1.000000000000000000, 0.9510565162951535312, 1.000000000000000000, 0.9510565162951535312, 1.000000000000000000, 0.9510565162951535312, 1.000000000000000000, 0.9510565162951535312, 1.000000000000000000, 0.9510565162951535312, 1.000000000000000000, 0.9510565162951535312, 1.000000000000000000, 0.9510565162951535312, 1.000000000000000000, 0.9510565162951535312, 1.000000000000000000, 0.9510565162951535312, 1.000000000000000000, 0.9510565162951535312, 1.000000000000000000, 0.9510565162951535312, 1.000000000000000000, 0.9510565162951535312, 1.000000000000000000, 0.9510565162951535312, 1.000000000000000000, 0.9510565162951535312, 1.000000000000000000, 0.9510565162951535312, 1.000000000000000000, 0.9510565162951535312, 1.000000000000000000, 0.9510565162951535312, 1.000000000000000000, 0.9510565162951535312, 1.000000000000000000, 0.9510565162951535312, 1.000000000000000000, 0.9510565162951535312, 1.000000000000000000, 0.9510565162951535312, 1.000000000000000000, 0.9510565162951535312, 1.000000000000000000, 0.9510565162951535312, 1.000000000000000000, 0.9510565162951535312, 1.000000000000000000, 0.9510565162951535312, 1.000000000000000000, 0.9510565162951535312, 1.000000000000000000, 0.9510565162951535312, 1.000000000000000000, 0.9510565162951535312, 1.000000000000000000, 0.9510565162951535312, 1.000000000000000000, 0.9510565162951535312, 1.000000000000000000, 0.9510565162951535312, 1.000000000000000000, 0.9510565162951535312, 1.000000000000000000, 0.9510565162951535312, 1.000000000000000000, 0.9510565162951535312, 1.000000000000000000, 0.9510565162951535312, 1.000000000000000000, 0.9510565162951535312, 1.000000000000000000, 0.9510565162951535312, 1.000000000000000000, 0.9510565162951535312, 1.000000000000000000, 0.9510565162951535312, 1.000000000000000000, 0.9510565162951535312, 1.000000000000000000, 0.9510565162951535312, 1.000000000000000000, 0.9510565162951535312, 1.000000000000000000, 0.9510565162951535312, 1.000000000000000000, 0.9510565162951535312, 1.000000000000000000, 0.9510565162951535312, 1.000000000000000000, 0.9510565162951535312, 1.000000000000000000, 0.9510565162951535312, 1.000000000000000000, 0.9510565162951535312, 1.000000000000000000, 0.9510565162951535312, 1.000000000000000000, 0.9510565162951535312, 1.000000000000000000, 0.9510565162951535312, 1.000000000000000000, 0.9510565162951535312, 1.000000000000000000, 0.9510565162951535312, 1.000000000000000000, 0.9510565162951535312, 1.000000000000000000, 0.9510565162951535312, 1.000000000000000000, 0.9510565162951535312, 1.000000000000000000, 0.9510565162951535312, 1.000000000000000000, 0.9510565162951535312, 1.000000000000000000, 0.9510565162951535312, 1.000000000000000000, 0.9510565162951535312, 1.000000000000000000, 0.9510565162951535312, 1.000000000000000000, 0.9510565162951535312, 1.000000000000000000, 0.9510565162951535312, 1.000000000000000000, 0.9510565162951535312, 1.000000000000000000, 0.9510565162951535312, 1.000000000000000000, 0.9510565162951535312, 1.000000000000000000, 0.9510565162951535312, 1.000000000000000000, 0.9510565162951535312, 1.000000000000000000, 0.9510565162951535312, 1.000000000000000000, 0.9510565162951535312, 1.000000000000000000, 0.9510565162951535312, 1.000000000000000000, 0.9510565162951535312, 1.000000000000000000, 0.9510565162951535312, 1.000000000000000000, 0.9510565162951535312, 1.000000000000000000, 0.9510565162951535312, 1.000000000000000000, 0.9510565162951535312, 1.000000000000000000, 0.9510565162951535312, 1.000000000000000000, 0.9510565162951535312, 1.000000000000000000, 0.9510565162951535312, 1.000000000000000000, 0.9510565162951535312, 1.000000000000000000, 0.9510565162951535312, 1.000000000000000000, 0.9510565162951535312, 1.000000000000000000, 0.9510565162951535312, 1.000000000000000000, 0.9510565162951535312, 1.000000000000000000, 0.9510565162951535312, 1.000000000000000000, 0.9510565162951535312, 1.000000000000000000, 0.9510565162951535312, 1.000000000000000000, 0.9510565162951535312, 1.000000000000000000, 0.9510565162951535312, 1.000000000000000000, 0.9510565162951535312, 1.000000000000000000, 0.9510565162951535312, 1.000000000000000000, 0.9510565162951535312, 1.000000000000000000, 0.9510565162951535312, 1.000000000000000000, 0.9510565162951535312, 1.000000000000000000, 0.9510565162951535312, 1.000000000000000000, 0.9510565162951535312, 1.000000000000000000, 0.9510565162951535312, 1.000000000000000000, 0.9510565162951535312, 1.000000000000000000, 0.9510565162951535312, 1.000000000000000000, 0.9510565162951535312, 1.000000000000000000, 0.9510565162951535312, 1.000000000000000000, 0.9510565162951535312, 1.000000000000000000, 0.9510565162951535312, 1.000000000000000000, 0.9510565162951535312, 1.000000000000000000, 0.9510565162951535312, 1.000000000000000000, 0.9510565162951535312, 1.000000000000000000, 0.9510565162951535312, 1.000000000000000000, 0.9510565162951535312, 1.000000000000000000, 0.9510565162951535312, 1.000000000000000000, 0.9510565162951535312, 1.000000000000000000, 0.9510565162951535312, 1.000000000000000000, 0.9510565162951535312, 1.000000000000000000, 0.9510565162951535312, 1.000000000000000000, 0.9510565162951535312, 1.000000000000000000, 0.9510565162951535312, 1.000000000000000000, 0.9510565162951535312, 1.000000000000000000, 0.9510565162951535312, 1.000000000000000000, 0.9510565162951535312, 1.000000000000000000, 0.9510565162951535312, 1.000000000000000000, 0.9510565162951535312, 1.000000000000000000, 0.9510565162951535312, 1.000000000000000000, 0.9510565162951535312, 1.000000000000000000, 0.9510565162951535312, 1.000000000000000000, 0.9510565162951535312, 1.000000000000000000, 0.9510565162951535312, 1.000000000000000000, 0.9510565162951535312, 1.000000000000000000, 0.9510565162951535312, 1.000000000000000000, 0.9510565162951535312, 1.000000000000000000, 0.9510565162951535312, 1.000000000000000000, 0.9510565162951535312, 1.000000000000000000, 0.9510565162951535312, 1.000000000000000000, 0.9510565162951535312, 1.000000000000000000, 0.9510565162951535312, 1.000000000000000000, 0.9510565162951535312, 1.000000000000000000, 0.9510565162951535312, 1.000000000000000000, 0.9510565162951535312, 1.000000000000000000, 0.9510565162951535312, 1.000000000000000000, 0.9510565162951535312, 1.000000000000000000, 0.9510565162951535312, 1.000000000000000000, 0.9510565162951535312, 1.000000000000000000, 0.9510565162951535312, 1.000000000000000000, 0.9510565162951535312, 1.000000000000000000, 0.9510565162951535312, 1.000000000000000000, 0.9510565162951535312, 1.000000000000000000, 0.9510565162951535312, 1.000000000000000000, 0.9510565162951535312, 1.000000000000000000, 0.9510565162951535312, 1.000000000000000000, 0.9510565162951535312, 1.000000000000000000, 0.9510565162951535312, 1.000000000000000000, 0.9510565162951535312, 1.000000000000000000, 0.9510565162951535312, 1.000000000000000000, 0.9510565162951535312, 1.000000000000000000, 0.9510565162951535312, 1.000000000000000000, 0.9510565162951535312, 1.000000000000000000, 0.9510565162951535312, 1.000000000000000000, 0.9510565162951535312, 1.000000000000000000, 0.9510565162951535312, 1.000000000000000000, 0.9510565162951535312, 1.000000000000000000) ) ) 
 REPRESENTATION_ITEM ( '' )  SURFACE ( )  );
#17956 = SURFACE_SIDE_STYLE ('',( #34127 ) ) ;
#17957 = EDGE_CURVE ( 'NONE', #50964, #37266, #46403, .T. ) ;
#17958 = VECTOR ( 'NONE', #9573, 1000.000000000000000 ) ;
#17959 = SPHERICAL_SURFACE ( 'NONE', #1169, 7.500000000000000000 ) ;
#17960 = CARTESIAN_POINT ( 'NONE',  ( 34.99999999999999289, 99.99999999999997158, 3.500000000000000000 ) ) ;
#17961 = CARTESIAN_POINT ( 'NONE',  ( -7.766391886667110001, -0.5482146608018571010, 0.7663918866669822139 ) ) ;
#17962 =( NAMED_UNIT ( * ) SI_UNIT ( $, .STERADIAN. ) SOLID_ANGLE_UNIT ( ) );
#17963 = ORIENTED_EDGE ( 'NONE', *, *, #2041, .T. ) ;
#17964 = CARTESIAN_POINT ( 'NONE',  ( -144.2050000000000125, -2.607480562269071545, -8.024999999999991473 ) ) ;
#17965 = VERTEX_POINT ( 'NONE', #41121 ) ;
#17966 = ORIENTED_EDGE ( 'NONE', *, *, #7716, .F. ) ;
#17967 = DIRECTION ( 'NONE',  ( -0.000000000000000000, -1.000000000000000000, -0.000000000000000000 ) ) ;
#17968 = ORIENTED_EDGE ( 'NONE', *, *, #23700, .F. ) ;
#17969 = EDGE_CURVE ( 'NONE', #53049, #46991, #55756, .T. ) ;
#17970 = CIRCLE ( 'NONE', #57279, 5.500000000000005329 ) ;
#17971 = CARTESIAN_POINT ( 'NONE',  ( -45.00000000000000000, 10.49999999999998224, -3.000000000000000444 ) ) ;
#17972 = CARTESIAN_POINT ( 'NONE',  ( -3.094860106618432471, 133.5949999999999989, -9.525000000000000355 ) ) ;
#17973 = DIRECTION ( 'NONE',  ( 1.000000000000000000, -0.000000000000000000, -0.000000000000000000 ) ) ;
#17974 = ORIENTED_EDGE ( 'NONE', *, *, #28739, .F. ) ;
#17975 = CARTESIAN_POINT ( 'NONE',  ( 23.50000000000001776, 14.00000000000000000, 29.68999999999999417 ) ) ;
#17976 = CARTESIAN_POINT ( 'NONE',  ( 8.102448949553181734, 140.1049999999999898, -5.886773742842746238 ) ) ;
#17977 = CARTESIAN_POINT ( 'NONE',  ( -55.85499999999998977, 4.716976649647094177, 6.492361379858945902 ) ) ;
#17978 = EDGE_CURVE ( 'NONE', #1306, #22643, #3757, .T. ) ;
#17979 = CARTESIAN_POINT ( 'NONE',  ( 41.27272961514506022, 107.3325180337009073, -3.464233254637873571 ) ) ;
#17980 = ORIENTED_EDGE ( 'NONE', *, *, #22088, .T. ) ;
#17981 = CARTESIAN_POINT ( 'NONE',  ( -8.102448949553181734, 156.0050000000000239, -5.886773742842749790 ) ) ;
#17982 = DIRECTION ( 'NONE',  ( 0.000000000000000000, 0.000000000000000000, -1.000000000000000000 ) ) ;
#17983 = UNCERTAINTY_MEASURE_WITH_UNIT (LENGTH_MEASURE( 1.000000000000000082E-05 ), #57353, 'distance_accuracy_value', 'NONE');
#17984 = PRESENTATION_LAYER_ASSIGNMENT (  '', '', ( #29202 ) ) ;
#17985 = VERTEX_POINT ( 'NONE', #37937 ) ;
#17986 = VERTEX_POINT ( 'NONE', #48836 ) ;
#17987 = DIRECTION ( 'NONE',  ( 0.000000000000000000, 0.000000000000000000, -1.000000000000000000 ) ) ;
#17988 = COLOUR_RGB ( '', 0.72549020, 0.75294118, 0.79215686) ;
#17989 = CARTESIAN_POINT ( 'NONE',  ( -122.4570736234661723, -9.058813317711329915, 2.943386871421371787 ) ) ;
#17990 = CARTESIAN_POINT ( 'NONE',  ( -158.0049999999999955, 6.826472737025116366, 4.959722759717898555 ) ) ;
#17991 = ORIENTED_EDGE ( 'NONE', *, *, #57470, .T. ) ;
#17992 = UNCERTAINTY_MEASURE_WITH_UNIT (LENGTH_MEASURE( 1.000000000000000082E-05 ), #45566, 'distance_accuracy_value', 'NONE');
#17993 = CONICAL_SURFACE ( 'NONE', #35975, 5.499999999999976907, 0.7853981633974309595 ) ;
#17994 = SURFACE_STYLE_FILL_AREA ( #66168 ) ;
#17995 = ORIENTED_EDGE ( 'NONE', *, *, #41413, .F. ) ;
#17996 = MECHANICAL_DESIGN_GEOMETRIC_PRESENTATION_REPRESENTATION (  '', ( #1090 ), #32582 ) ;
#17997 = ORIENTED_EDGE ( 'NONE', *, *, #4330, .T. ) ;
#17998 = DIRECTION ( 'NONE',  ( 1.000000000000000000, 0.000000000000000000, -0.000000000000000000 ) ) ;
#17999 = CARTESIAN_POINT ( 'NONE',  ( -87.50000000000000000, -8.499999999999989342, 2.999999999999999112 ) ) ;
#18000 = CARTESIAN_POINT ( 'NONE',  ( -80.60499999999996135, 6.826472737025113702, -4.959722759717902107 ) ) ;
#18001 = ORIENTED_EDGE ( 'NONE', *, *, #57141, .T. ) ;
#18002 = SURFACE_STYLE_USAGE ( .BOTH. , #18365 ) ;
#18003 = STYLED_ITEM ( 'NONE', ( #4121 ), #59305 ) ;
#18004 = CARTESIAN_POINT ( 'NONE',  ( 8.082903768654762899, -1.105959442090949618E-15, 7.500000000000000000 ) ) ;
#18005 = LINE ( 'NONE', #60901, #57822 ) ;
#18006 = EDGE_CURVE ( 'NONE', #34731, #59410, #37595, .T. ) ;
#18007 = COLOUR_RGB ( '', 0.66274510, 0.83137255, 0.94901961) ;
#18008 = FILL_AREA_STYLE_COLOUR ( '', #69575 ) ;
#18009 = ORIENTED_EDGE ( 'NONE', *, *, #45689, .T. ) ;
#18011 = SURFACE_SIDE_STYLE ('',( #44788 ) ) ;
#18010 = LINE ( 'NONE', #13777, #21224 ) ;
#18012 = CARTESIAN_POINT ( 'NONE',  ( -10.01517768586949231, 140.1949999999999932, -6.132527647946036459E-16 ) ) ;
#18013 = CARTESIAN_POINT ( 'NONE',  ( -105.1449999999999818, -4.716976649647092401, 6.492361379858946790 ) ) ;
#18014 = AXIS2_PLACEMENT_3D ( 'NONE', #55893, #56935, #13312 ) ;
#18015 = CARTESIAN_POINT ( 'NONE',  ( 15.98999599679679839, 117.4999999999999716, 9.500000000000000000 ) ) ;
#18016 = COLOUR_RGB ( '', 0.08235294, 0.09019608, 0.10196078) ;
#18017 = PRODUCT_RELATED_PRODUCT_CATEGORY ( 'part', '', ( #52408 ) ) ;
#18018 = DIRECTION ( 'NONE',  ( -1.000000000000000000, 0.000000000000000000, 6.938893903907221278E-15 ) ) ;
#18019 = EDGE_CURVE ( 'NONE', #63831, #6631, #32964, .T. ) ;
#18020 = CIRCLE ( 'NONE', #5642, 1.000000000000000888 ) ;
#18021 = CARTESIAN_POINT ( 'NONE',  ( -152.6929263765337907, 10.01517768586948698, -1.839758294383808571E-15 ) ) ;
#18022 = ADVANCED_FACE ( 'NONE', ( #33309 ), #16115, .T. ) ;
#18023 =( NAMED_UNIT ( * ) PLANE_ANGLE_UNIT ( ) SI_UNIT ( $, .RADIAN. ) );
#18024 = CARTESIAN_POINT ( 'NONE',  ( -167.9950000000000045, -6.826472737025115478, 4.959722759717900331 ) ) ;
#18025 = ADVANCED_FACE ( 'NONE', ( #54732 ), #38278, .T. ) ;
#18026 = EDGE_CURVE ( 'NONE', #29002, #64619, #50825, .T. ) ;
#18027 = AXIS2_PLACEMENT_3D ( 'NONE', #20366, #35164, #56622 ) ;
#18028 = CIRCLE ( 'NONE', #12383, 4.999999999999997335 ) ;
#18029 = ORIENTED_EDGE ( 'NONE', *, *, #18451, .T. ) ;
#18030 = DIRECTION ( 'NONE',  ( -1.000000000000000000, 0.000000000000000000, 0.000000000000000000 ) ) ;
#18031 = VERTEX_POINT ( 'NONE', #53703 ) ;
#18032 = CARTESIAN_POINT ( 'NONE',  ( -70.79292637653379927, -3.094860106618429807, 9.524999999999991473 ) ) ;
#18033 = AXIS2_PLACEMENT_3D ( 'NONE', #41500, #52404, #56959 ) ;
#18034 = CARTESIAN_POINT ( 'NONE',  ( 22.50000000000000711, 36.75000000000000000, -3.750000000000000000 ) ) ;
#18035 = PRODUCT_DEFINITION_FORMATION_WITH_SPECIFIED_SOURCE ( 'ANY', '', #51816, .NOT_KNOWN. ) ;
#18036 = EDGE_CURVE ( 'NONE', #54975, #6724, #2337, .T. ) ;
#18037 = CARTESIAN_POINT ( 'NONE',  ( 71.50000000000000000, 35.92875272052971525, 9.500000000000000000 ) ) ;
#18038 = DIRECTION ( 'NONE',  ( 0.6363636363636357984, 0.000000000000000000, -0.7713892158398705234 ) ) ;
#18039 = SURFACE_STYLE_USAGE ( .BOTH. , #39883 ) ;
#18040 =( GEOMETRIC_REPRESENTATION_CONTEXT ( 3 ) GLOBAL_UNCERTAINTY_ASSIGNED_CONTEXT ( ( #42470 ) ) GLOBAL_UNIT_ASSIGNED_CONTEXT ( ( #67001, #67335, #62731 ) ) REPRESENTATION_CONTEXT ( 'NONE', 'WORKASPACE' ) );
#18041 = EDGE_CURVE ( 'NONE', #49292, #41299, #16805, .T. ) ;
#18042 = ORIENTED_EDGE ( 'NONE', *, *, #34166, .T. ) ;
#18043 = CARTESIAN_POINT ( 'NONE',  ( -170.0049999999999955, 6.826472737025115478, 4.959722759717899443 ) ) ;
#18044 = ORIENTED_EDGE ( 'NONE', *, *, #68395, .F. ) ;
#18045 = CARTESIAN_POINT ( 'NONE',  ( -112.6429263765338078, -5.598654528085801552, 7.705886871421367523 ) ) ;
#18046 = DIRECTION ( 'NONE',  ( 1.000000000000000000, 0.000000000000000000, 0.000000000000000000 ) ) ;
#18047 = CARTESIAN_POINT ( 'NONE',  ( 0.000000000000000000, 110.4999999999999858, 0.000000000000000000 ) ) ;
#18048 = VECTOR ( 'NONE', #4839, 1000.000000000000000 ) ;
#18049 = FILL_AREA_STYLE ('',( #60267 ) ) ;
#18050 = CARTESIAN_POINT ( 'NONE',  ( -7.632228543268608334, 154.9570736234661581, 2.479861379858952830 ) ) ;
#18051 =( BOUNDED_CURVE ( )  B_SPLINE_CURVE ( 2, ( #60489, #61886, #13349, #28475, #39440, #34469, #44727, #55924, #12299, #2035, #44392 ),
 .UNSPECIFIED., .F., .F. ) 
 B_SPLINE_CURVE_WITH_KNOTS ( ( 3, 2, 2, 2, 2, 3 ),
 ( 0.07608695652173738666, 0.07826086956521560722, 0.08043478260869380003, 0.08260869565217202060, 0.08478260869565022728, 0.08695652173912844785 ),
 .UNSPECIFIED. ) 
 CURVE ( )  GEOMETRIC_REPRESENTATION_ITEM ( )  RATIONAL_B_SPLINE_CURVE ( ( 1.000000000000039302, 0.9510565162951140072, 1.000000000000000000, 0.9510565162951535312, 1.000000000000000000, 0.9510565162951535312, 1.000000000000000000, 0.9510565162951535312, 1.000000000000000000, 0.9510565162951981621, 0.9999999999999553690 ) ) 
 REPRESENTATION_ITEM ( '' )  );
#18052 = VERTEX_POINT ( 'NONE', #5857 ) ;
#18053 = VECTOR ( 'NONE', #53195, 1000.000000000000000 ) ;
#18054 = CARTESIAN_POINT ( 'NONE',  ( -71.74137931034481142, 36.89918356738973415, 9.500000000000000000 ) ) ;
#18055 = VECTOR ( 'NONE', #53493, 1000.000000000000000 ) ;
#18056 = CARTESIAN_POINT ( 'NONE',  ( -87.05499999999999261, -9.827790563157499189E-16, -8.024999999999991473 ) ) ;
#18057 = SURFACE_STYLE_FILL_AREA ( #45852 ) ;
#18058 = CARTESIAN_POINT ( 'NONE',  ( 5.598654528085805993, 127.3549999999999898, 7.705886871421374629 ) ) ;
#18059 = UNCERTAINTY_MEASURE_WITH_UNIT (LENGTH_MEASURE( 1.000000000000000082E-05 ), #40868, 'distance_accuracy_value', 'NONE');
#18060 = CARTESIAN_POINT ( 'NONE',  ( -71.49999999999998579, 119.9999999999997868, -7.500000000000000000 ) ) ;
#18061 = CARTESIAN_POINT ( 'NONE',  ( 185.0000000000000000, 0.000000000000000000, 0.000000000000000000 ) ) ;
#18062 = CARTESIAN_POINT ( 'NONE',  ( -72.95707362346617231, 9.058813317711329915, -2.943386871421373119 ) ) ;
#18063 = CARTESIAN_POINT ( 'NONE',  ( 48.81081081081080697, 14.09971791521132900, -9.500000000000000000 ) ) ;
#18064 = CARTESIAN_POINT ( 'NONE',  ( -83.49999999999998579, -2.499999999999999556, 24.00000000000000000 ) ) ;
#18065 =( NAMED_UNIT ( * ) PLANE_ANGLE_UNIT ( ) SI_UNIT ( $, .RADIAN. ) );
#18066 = EDGE_LOOP ( 'NONE', ( #18567, #68152, #62808, #40468 ) ) ;
#18067 = CARTESIAN_POINT ( 'NONE',  ( -140.6070736234661922, -8.102448949553174629, 5.886773742842742685 ) ) ;
#18068 = EDGE_CURVE ( 'NONE', #47699, #36693, #58996, .T. ) ;
#18069 = CARTESIAN_POINT ( 'NONE',  ( -51.89499999999998892, 6.826472737025116366, 4.959722759717898555 ) ) ;
#18071 = ORIENTED_EDGE ( 'NONE', *, *, #36974, .F. ) ;
#18070 = AXIS2_PLACEMENT_3D ( 'NONE', #41090, #7415, #67798 ) ;
#18072 = DIRECTION ( 'NONE',  ( 0.000000000000000000, -0.000000000000000000, 1.000000000000000000 ) ) ;
#18073 = PRESENTATION_STYLE_ASSIGNMENT (( #34942 ) ) ;
#18074 = CARTESIAN_POINT ( 'NONE',  ( -45.86631659065714928, 9.243037840626161739, -6.242508038240250912 ) ) ;
#18075 = DIRECTION ( 'NONE',  ( 0.000000000000000000, -1.000000000000000000, 0.000000000000000000 ) ) ;
#18076 = VERTEX_POINT ( 'NONE', #853 ) ;
#18077 = CARTESIAN_POINT ( 'NONE',  ( -51.51464445532459990, -11.66590569038438829, 3.204935539835279901 ) ) ;
#18078 = CARTESIAN_POINT ( 'NONE',  ( -53.69499999999999318, -8.437984349512086979, 5.166775262442717831E-16 ) ) ;
#18079 = AXIS2_PLACEMENT_3D ( 'NONE', #42652, #15908, #63018 ) ;
#18080 = ORIENTED_EDGE ( 'NONE', *, *, #32634, .T. ) ;
#18081 = CARTESIAN_POINT ( 'NONE',  ( -75.00000000000000000, 9.482577857128569931, 6.485016072424482303 ) ) ;
#18082 = CARTESIAN_POINT ( 'NONE',  ( -117.2049999999999841, -2.607480562269071545, -8.024999999999991473 ) ) ;
#18083 = VERTEX_POINT ( 'NONE', #48134 ) ;
#18084 = CARTESIAN_POINT ( 'NONE',  ( 0.04677136509298115974, 68.99999999999998579, 6.349999999999997868 ) ) ;
#18085 =( GEOMETRIC_REPRESENTATION_CONTEXT ( 3 ) GLOBAL_UNCERTAINTY_ASSIGNED_CONTEXT ( ( #13615 ) ) GLOBAL_UNIT_ASSIGNED_CONTEXT ( ( #16571, #59417, #637 ) ) REPRESENTATION_CONTEXT ( 'NONE', 'WORKASPACE' ) );
#18086 = CARTESIAN_POINT ( 'NONE',  ( -12.34222745343792127, 149.9999999999999716, 10.18181818181818166 ) ) ;
#18087 = CARTESIAN_POINT ( 'NONE',  ( -12.72792206135785698, 114.9999999999999574, -10.50000000000000000 ) ) ;
#18088 = CARTESIAN_POINT ( 'NONE',  ( -150.9570736234661581, 9.058813317711329915, -2.943386871421373119 ) ) ;
#18089 = DIRECTION ( 'NONE',  ( 0.000000000000000000, 0.000000000000000000, 1.000000000000000000 ) ) ;
#18090 = PRESENTATION_LAYER_ASSIGNMENT (  '', '', ( #60740 ) ) ;
#18091 = CARTESIAN_POINT ( 'NONE',  ( -9.058813317711338797, 143.3449999999999989, 2.943386871421373563 ) ) ;
#18092 = CARTESIAN_POINT ( 'NONE',  ( -81.05707362346618083, 0.000000000000000000, 9.524999999999991473 ) ) ;
#18093 = CARTESIAN_POINT ( 'NONE',  ( 8.000000000000024869, 5.000000000000000000, 32.00402776293825724 ) ) ;
#18094 = VERTEX_POINT ( 'NONE', #27986 ) ;
#18095 = STYLED_ITEM ( 'NONE', ( #18794 ), #28762 ) ;
#18096 = DIRECTION ( 'NONE',  ( 0.000000000000000000, -0.3420201433256630508, -0.9396926207859105373 ) ) ;
#18097 = FILL_AREA_STYLE ('',( #46251 ) ) ;
#18098 = CARTESIAN_POINT ( 'NONE',  ( -131.7549999999999955, 4.716976649647091513, -6.492361379858946790 ) ) ;
#18099 = CARTESIAN_POINT ( 'NONE',  ( 48.25000000000000000, 21.74999999999998579, 3.750000000000000000 ) ) ;
#18100 = DIRECTION ( 'NONE',  ( -0.000000000000000000, -0.000000000000000000, 1.000000000000000000 ) ) ;
#18101 = CARTESIAN_POINT ( 'NONE',  ( -7.731910350068054619E-16, -6.500000000000000888, 21.00000000000000000 ) ) ;
#18102 = CARTESIAN_POINT ( 'NONE',  ( -136.4949999999999477, 6.826472737025113702, -4.959722759717902107 ) ) ;
#18103 = CARTESIAN_POINT ( 'NONE',  ( -127.1950000000000074, 8.437984349512086979, -1.550032578732815448E-15 ) ) ;
#18104 = AXIS2_PLACEMENT_3D ( 'NONE', #12914, #34028, #11883 ) ;
#18105 = DIRECTION ( 'NONE',  ( 0.000000000000000000, 0.000000000000000000, -1.000000000000000000 ) ) ;
#18106 = ORIENTED_EDGE ( 'NONE', *, *, #36079, .T. ) ;
#18107 = DIRECTION ( 'NONE',  ( 0.000000000000000000, 0.000000000000000000, -1.000000000000000000 ) ) ;
#18108 = SURFACE_STYLE_FILL_AREA ( #1867 ) ;
#18109 = EDGE_CURVE ( 'NONE', #49901, #37663, #29313, .T. ) ;
#18111 =( GEOMETRIC_REPRESENTATION_CONTEXT ( 3 ) GLOBAL_UNCERTAINTY_ASSIGNED_CONTEXT ( ( #24300 ) ) GLOBAL_UNIT_ASSIGNED_CONTEXT ( ( #66822, #26304, #10837 ) ) REPRESENTATION_CONTEXT ( 'NONE', 'WORKASPACE' ) );
#18110 = CARTESIAN_POINT ( 'NONE',  ( 68.50000000000000000, 1.797044900979284448E-15, 10.00000000000000000 ) ) ;
#18112 = CARTESIAN_POINT ( 'NONE',  ( -179.0929263765338249, 3.094860106618433360, 9.524999999999991473 ) ) ;
#18113 =( LENGTH_UNIT ( ) NAMED_UNIT ( * ) SI_UNIT ( .MILLI., .METRE. ) );
#18114 = CARTESIAN_POINT ( 'NONE',  ( -53.39499999999998892, -6.826472737025115478, -4.959722759717899443 ) ) ;
#18115 = CIRCLE ( 'NONE', #68638, 2.499999999999998224 ) ;
#18116 = ADVANCED_FACE ( 'NONE', ( #42509 ), #63908, .T. ) ;
#18117 = SURFACE_STYLE_USAGE ( .BOTH. , #22703 ) ;
#18118 = FILL_AREA_STYLE ('',( #54352 ) ) ;
#18119 = CARTESIAN_POINT ( 'NONE',  ( 72.49999999999998579, 119.9999999999997868, -10.00000000000000000 ) ) ;
#18120 = AXIS2_PLACEMENT_3D ( 'NONE', #56005, #29634, #50747 ) ;
#18121 = DIRECTION ( 'NONE',  ( -1.000000000000000000, 0.000000000000000000, 0.000000000000000000 ) ) ;
#18122 = CARTESIAN_POINT ( 'NONE',  ( -96.14292637653380780, 5.598654528085800663, -7.705886871421367523 ) ) ;
#18123 = APPLICATION_PROTOCOL_DEFINITION ( 'draft international standard', 'automotive_design', 1998, #33423 ) ;
#18124 = DIRECTION ( 'NONE',  ( 0.000000000000000000, 0.000000000000000000, 1.000000000000000000 ) ) ;
#18125 = CARTESIAN_POINT ( 'NONE',  ( -62.28939201416945082, 4.336808689942018722E-16, 0.000000000000000000 ) ) ;
#18126 = AXIS2_PLACEMENT_3D ( 'NONE', #47776, #10776, #494 ) ;
#18127 = DIRECTION ( 'NONE',  ( -0.000000000000000000, -1.000000000000000000, -0.000000000000000000 ) ) ;
#18128 = SURFACE_STYLE_USAGE ( .BOTH. , #39964 ) ;
#18129 = AXIS2_PLACEMENT_3D ( 'NONE', #36768, #26151, #32134 ) ;
#18130 = ADVANCED_FACE ( 'NONE', ( #55446 ), #1910, .F. ) ;
#18131 = DIRECTION ( 'NONE',  ( -1.000000000000000000, 0.000000000000000000, 0.000000000000000000 ) ) ;
#18132 = ORIENTED_EDGE ( 'NONE', *, *, #55288, .F. ) ;
#18133 = CARTESIAN_POINT ( 'NONE',  ( 10.00000000000002132, 50.00000000000000000, 60.00000000000000711 ) ) ;
#18134 = SURFACE_STYLE_FILL_AREA ( #61025 ) ;
#18135 = DIRECTION ( 'NONE',  ( -1.000000000000000000, 0.000000000000000000, 0.000000000000000000 ) ) ;
#18136 = ORIENTED_EDGE ( 'NONE', *, *, #495, .T. ) ;
#18137 = FILL_AREA_STYLE_COLOUR ( '', #40981 ) ;
#18138 = CARTESIAN_POINT ( 'NONE',  ( 2.607480562269071989, 122.7070736234661439, 8.025000000000002132 ) ) ;
#18139 = MECHANICAL_DESIGN_GEOMETRIC_PRESENTATION_REPRESENTATION (  '', ( #22764 ), #54236 ) ;
#18140 = PRESENTATION_STYLE_ASSIGNMENT (( #7576 ) ) ;
#18141 = CARTESIAN_POINT ( 'NONE',  ( -195.0000000000000000, 1.166476076187852838E-15, -9.524999999999991473 ) ) ;
#18142 = DIRECTION ( 'NONE',  ( -1.000000000000000000, 0.000000000000000000, 0.000000000000000000 ) ) ;
#18143 = EDGE_LOOP ( 'NONE', ( #62337, #26028, #6206, #22856 ) ) ;
#18144 = CYLINDRICAL_SURFACE ( 'NONE', #4635, 1.000000000000000888 ) ;
#18145 = DIRECTION ( 'NONE',  ( 0.000000000000000000, 0.000000000000000000, 1.000000000000000000 ) ) ;
#18146 = ADVANCED_FACE ( 'NONE', ( #17822 ), #66338, .T. ) ;
#18147 = CYLINDRICAL_SURFACE ( 'NONE', #55517, 26.99999999999999645 ) ;
#18148 = CARTESIAN_POINT ( 'NONE',  ( -72.05707362346616662, 0.000000000000000000, 9.524999999999991473 ) ) ;
#18149 = ADVANCED_FACE ( 'NONE', ( #46602 ), #14840, .T. ) ;
#18150 = CARTESIAN_POINT ( 'NONE',  ( -92.69499999999996476, -8.437984349512085203, 5.166775262442717831E-16 ) ) ;
#18151 = ORIENTED_EDGE ( 'NONE', *, *, #25892, .T. ) ;
#18152 = AXIS2_PLACEMENT_3D ( 'NONE', #20209, #52606, #70 ) ;
#18153 = LINE ( 'NONE', #65297, #52473 ) ;
#18154 = CARTESIAN_POINT ( 'NONE',  ( 0.000000000000000000, 21.74999999999998579, 3.750000000000000000 ) ) ;
#18155 = ORIENTED_EDGE ( 'NONE', *, *, #61051, .T. ) ;
#18156 = CIRCLE ( 'NONE', #48527, 0.5000000000000004441 ) ;
#18157 = DIRECTION ( 'NONE',  ( 0.6363636363636357984, 0.000000000000000000, -0.7713892158398705234 ) ) ;
#18158 = ORIENTED_EDGE ( 'NONE', *, *, #7557, .T. ) ;
#18159 = ORIENTED_EDGE ( 'NONE', *, *, #21138, .F. ) ;
#18160 = DIRECTION ( 'NONE',  ( -0.000000000000000000, -0.000000000000000000, -1.000000000000000000 ) ) ;
#18161 = CARTESIAN_POINT ( 'NONE',  ( -182.3070736234662093, -10.01517768586948698, 6.132527647946031529E-16 ) ) ;
#18162 = AXIS2_PLACEMENT_3D ( 'NONE', #12763, #51451, #23668 ) ;
#18163 = LINE ( 'NONE', #56486, #56724 ) ;
#18164 = CARTESIAN_POINT ( 'NONE',  ( 24.21231517720798010, 112.9999999999999858, -7.000000000000000000 ) ) ;
#18165 = CARTESIAN_POINT ( 'NONE',  ( -111.0570736234661808, 0.000000000000000000, 9.524999999999991473 ) ) ;
#18166 = CIRCLE ( 'NONE', #33866, 0.5000000000000004441 ) ;
#18167 = CARTESIAN_POINT ( 'NONE',  ( 1.224646799147353256E-15, 0.000000000000000000, 10.00000000000000000 ) ) ;
#18168 = ORIENTED_EDGE ( 'NONE', *, *, #66895, .T. ) ;
#18169 =( GEOMETRIC_REPRESENTATION_CONTEXT ( 3 ) GLOBAL_UNCERTAINTY_ASSIGNED_CONTEXT ( ( #34888 ) ) GLOBAL_UNIT_ASSIGNED_CONTEXT ( ( #21575, #31081, #63102 ) ) REPRESENTATION_CONTEXT ( 'NONE', 'WORKASPACE' ) );
#18170 = CARTESIAN_POINT ( 'NONE',  ( -195.0000000000000000, 1.166476076187852838E-15, -9.524999999999991473 ) ) ;
#18171 =( LENGTH_UNIT ( ) NAMED_UNIT ( * ) SI_UNIT ( .MILLI., .METRE. ) );
#18172 = CARTESIAN_POINT ( 'NONE',  ( 66.49999999999998579, 36.75000000000000000, 4.000000000000000000 ) ) ;
#18173 = DIRECTION ( 'NONE',  ( 0.000000000000000000, 0.000000000000000000, 1.000000000000000000 ) ) ;
#18174 = ORIENTED_EDGE ( 'NONE', *, *, #46583, .T. ) ;
#18175 = CARTESIAN_POINT ( 'NONE',  ( -156.5050000000000239, -6.826472737025115478, -4.959722759717899443 ) ) ;
#18176 = DIRECTION ( 'NONE',  ( -1.000000000000000000, 0.000000000000000000, 0.000000000000000000 ) ) ;
#18177 = AXIS2_PLACEMENT_3D ( 'NONE', #20508, #21545, #36735 ) ;
#18178 = EDGE_CURVE ( 'NONE', #4472, #32880, #43677, .T. ) ;
#18179 = CARTESIAN_POINT ( 'NONE',  ( -159.7450000000000045, 4.716976649647094177, 6.492361379858945902 ) ) ;
#18180 = CARTESIAN_POINT ( 'NONE',  ( -158.3949999999999818, -6.826472737025113702, -4.959722759717900331 ) ) ;
#18181 = ORIENTED_EDGE ( 'NONE', *, *, #2008, .F. ) ;
#18182 = DIRECTION ( 'NONE',  ( -1.000000000000000000, -0.000000000000000000, -0.000000000000000000 ) ) ;
#18183 = CARTESIAN_POINT ( 'NONE',  ( 45.50000000000000000, 10.69371294336137801, 10.00000000000000000 ) ) ;
#18184 = DIRECTION ( 'NONE',  ( 0.000000000000000000, 0.000000000000000000, 1.000000000000000000 ) ) ;
#18185 = CARTESIAN_POINT ( 'NONE',  ( -74.60500000000000398, 6.826472737025113702, -4.959722759717902107 ) ) ;
#18186 = DIRECTION ( 'NONE',  ( -0.000000000000000000, -0.000000000000000000, 1.000000000000000000 ) ) ;
#18187 = PRESENTATION_LAYER_ASSIGNMENT (  '', '', ( #50787 ) ) ;
#18188 = LINE ( 'NONE', #66732, #5656 ) ;
#18189 = EDGE_CURVE ( 'NONE', #43113, #1595, #37309, .T. ) ;
#18190 = CARTESIAN_POINT ( 'NONE',  ( -73.19499999999997897, 8.437984349512086979, -1.550032578732815448E-15 ) ) ;
#18191 = CARTESIAN_POINT ( 'NONE',  ( 5.598654528085805993, 142.3549999999999898, 7.705886871421374629 ) ) ;
#18192 = DIRECTION ( 'NONE',  ( 0.000000000000000000, 0.000000000000000000, 1.000000000000000000 ) ) ;
#18193 = AXIS2_PLACEMENT_3D ( 'NONE', #23560, #49982, #29888 ) ;
#18194 = EDGE_CURVE ( 'NONE', #10174, #51919, #12518, .T. ) ;
#18195 = DIRECTION ( 'NONE',  ( 0.000000000000000000, -0.000000000000000000, 1.000000000000000000 ) ) ;
#18196 =( LENGTH_UNIT ( ) NAMED_UNIT ( * ) SI_UNIT ( .MILLI., .METRE. ) );
#18197 =( LENGTH_UNIT ( ) NAMED_UNIT ( * ) SI_UNIT ( .MILLI., .METRE. ) );
#18198 = CIRCLE ( 'NONE', #29382, 0.5000000000000004441 ) ;
#18199 = PRODUCT_DEFINITION_SHAPE ( 'NONE', 'NONE',  #69699 ) ;
#18200 = CARTESIAN_POINT ( 'NONE',  ( 12.25000000000000533, 28.24999999999998224, -3.750000000000000000 ) ) ;
#18201 = VECTOR ( 'NONE', #3023, 1000.000000000000000 ) ;
#18202 = EDGE_CURVE ( 'NONE', #9347, #47468, #40649, .T. ) ;
#18203 = DIRECTION ( 'NONE',  ( 0.000000000000000000, 1.000000000000000000, -0.000000000000000000 ) ) ;
#18204 = MECHANICAL_DESIGN_GEOMETRIC_PRESENTATION_REPRESENTATION (  '', ( #9241 ), #53020 ) ;
#18205 = CARTESIAN_POINT ( 'NONE',  ( -120.1429263765338078, 5.598654528085800663, -7.705886871421367523 ) ) ;
#18206 = ORIENTED_EDGE ( 'NONE', *, *, #57446, .T. ) ;
#18207 = ORIENTED_EDGE ( 'NONE', *, *, #16549, .T. ) ;
#18208 = CARTESIAN_POINT ( 'NONE',  ( -60.05707362346616662, 0.000000000000000000, 9.524999999999991473 ) ) ;
#18209 = CIRCLE ( 'NONE', #2445, 0.2500000000000002220 ) ;
#18210 = CARTESIAN_POINT ( 'NONE',  ( -132.2070736234668686, 3.094860106628988028, 9.524999999992326494 ) ) ;
#18211 = AXIS2_PLACEMENT_3D ( 'NONE', #32860, #27554, #49075 ) ;
#18212 = CYLINDRICAL_SURFACE ( 'NONE', #23824, 0.2500000000000002220 ) ;
#18213 = PLANE ( 'NONE',  #22539 ) ;
#18214 = SURFACE_SIDE_STYLE ('',( #1957 ) ) ;
#18215 = DIRECTION ( 'NONE',  ( 0.000000000000000000, 0.000000000000000000, 1.000000000000000000 ) ) ;
#18216 = ORIENTED_EDGE ( 'NONE', *, *, #51324, .F. ) ;
#18217 = CARTESIAN_POINT ( 'NONE',  ( -99.80499999999997840, -8.437984349512086979, 5.166775262442717831E-16 ) ) ;
#18218 = ORIENTED_EDGE ( 'NONE', *, *, #52296, .T. ) ;
#18219 = SURFACE_STYLE_USAGE ( .BOTH. , #12227 ) ;
#18220 = CARTESIAN_POINT ( 'NONE',  ( -74.99999999999998579, 113.4999999999999858, 7.500000000000000000 ) ) ;
#18221 = PRESENTATION_LAYER_ASSIGNMENT (  '', '', ( #50819 ) ) ;
#18222 = ORIENTED_EDGE ( 'NONE', *, *, #34227, .T. ) ;
#18223 = CARTESIAN_POINT ( 'NONE',  ( -65.54292637653379927, 9.058813317711329915, 2.943386871421369566 ) ) ;
#18224 = CARTESIAN_POINT ( 'NONE',  ( 72.49999999999998579, 119.9999999999997868, 9.500000000000000000 ) ) ;
#18225 = ORIENTED_EDGE ( 'NONE', *, *, #62709, .F. ) ;
#18226 =( GEOMETRIC_REPRESENTATION_CONTEXT ( 3 ) GLOBAL_UNCERTAINTY_ASSIGNED_CONTEXT ( ( #68663 ) ) GLOBAL_UNIT_ASSIGNED_CONTEXT ( ( #12972, #7689, #29499 ) ) REPRESENTATION_CONTEXT ( 'NONE', 'WORKASPACE' ) );
#18227 = DIRECTION ( 'NONE',  ( 0.000000000000000000, 0.000000000000000000, 1.000000000000000000 ) ) ;
#18228 = CARTESIAN_POINT ( 'NONE',  ( -123.2949999999999875, -2.607480562269069768, 8.024999999999991473 ) ) ;
#18229 = ORIENTED_EDGE ( 'NONE', *, *, #42617, .F. ) ;
#18230 = EDGE_LOOP ( 'NONE', ( #65539, #50043, #54162, #20228 ) ) ;
#18231 =( LENGTH_UNIT ( ) NAMED_UNIT ( * ) SI_UNIT ( .MILLI., .METRE. ) );
#18232 = CARTESIAN_POINT ( 'NONE',  ( -15.75000000000000000, -4.000000000000000000, 20.00000000000000000 ) ) ;
#18233 = CARTESIAN_POINT ( 'NONE',  ( 24.29096171535645965, 27.11720862454939507, -27.31743315471676681 ) ) ;
#18234 = FILL_AREA_STYLE ('',( #12241 ) ) ;
#18235 = ORIENTED_EDGE ( 'NONE', *, *, #59471, .T. ) ;
#18236 = CARTESIAN_POINT ( 'NONE',  ( -9.827790563157511022E-16, 142.4429263765338192, 8.025000000000000355 ) ) ;
#18237 = DIRECTION ( 'NONE',  ( -1.000000000000000000, 0.000000000000000000, 0.000000000000000000 ) ) ;
#18238 =( NAMED_UNIT ( * ) PLANE_ANGLE_UNIT ( ) SI_UNIT ( $, .RADIAN. ) );
#18239 = FILL_AREA_STYLE_COLOUR ( '', #2479 ) ;
#18240 = CARTESIAN_POINT ( 'NONE',  ( -6.826472737025120807, 114.3929263765337936, -4.959722759717907437 ) ) ;
#18241 = VERTEX_POINT ( 'NONE', #64460 ) ;
#18242 = CARTESIAN_POINT ( 'NONE',  ( 22.75000000000000711, 36.75000000000000000, -3.750000000000000000 ) ) ;
#18243 = ORIENTED_EDGE ( 'NONE', *, *, #31429, .F. ) ;
#18244 = CARTESIAN_POINT ( 'NONE',  ( -34.99999999999999289, 99.99999999999998579, -9.500000000000000000 ) ) ;
#18245 = DIRECTION ( 'NONE',  ( 0.000000000000000000, 0.000000000000000000, 1.000000000000000000 ) ) ;
#18246 = CARTESIAN_POINT ( 'NONE',  ( -9.566487832665407254, -1.430357023834055719, 0.6362876910938550790 ) ) ;
#18248 = CARTESIAN_POINT ( 'NONE',  ( -134.1550000000000011, 7.632228543268600340, 2.479861379858949277 ) ) ;
#18247 = MECHANICAL_DESIGN_GEOMETRIC_PRESENTATION_REPRESENTATION (  '', ( #9279 ), #5880 ) ;
#18249 = PRESENTATION_STYLE_ASSIGNMENT (( #55878 ) ) ;
#18250 = CARTESIAN_POINT ( 'NONE',  ( -45.00000000000000000, 9.708372675170618749, -6.000000000000000000 ) ) ;
#18251 = ORIENTED_EDGE ( 'NONE', *, *, #53319, .F. ) ;
#18252 = MECHANICAL_DESIGN_GEOMETRIC_PRESENTATION_REPRESENTATION (  '', ( #49744 ), #62068 ) ;
#18253 = DIRECTION ( 'NONE',  ( 0.000000000000000000, -1.000000000000000000, 0.000000000000000000 ) ) ;
#18254 =( LENGTH_UNIT ( ) NAMED_UNIT ( * ) SI_UNIT ( .MILLI., .METRE. ) );
#18255 = CARTESIAN_POINT ( 'NONE',  ( -1.745454270669493990, -2.292880170259729233, 7.000000000000000000 ) ) ;
#18256 = ORIENTED_EDGE ( 'NONE', *, *, #26119, .T. ) ;
#18257 = VECTOR ( 'NONE', #62078, 1000.000000000000114 ) ;
#18258 = ORIENTED_EDGE ( 'NONE', *, *, #10660, .F. ) ;
#18259 = CARTESIAN_POINT ( 'NONE',  ( -32.60021343250990356, -9.015750088250115368, -2.278575939223535407 ) ) ;
#18260 = CARTESIAN_POINT ( 'NONE',  ( -51.95707362346615810, 9.058813317711329915, -2.943386871421373119 ) ) ;
#18261 = CARTESIAN_POINT ( 'NONE',  ( 0.000000000000000000, 13.00000000000000178, -80.00402776293826435 ) ) ;
#18262 = ORIENTED_EDGE ( 'NONE', *, *, #11228, .T. ) ;
#18263 = CARTESIAN_POINT ( 'NONE',  ( -123.5070736234661695, 8.102448949553176405, 5.886773742842740909 ) ) ;
#18264 = CARTESIAN_POINT ( 'NONE',  ( -184.2549999999999955, -4.716976649647092401, 6.492361379858946790 ) ) ;
#18265 = CARTESIAN_POINT ( 'NONE',  ( -91.94292637653380496, 0.000000000000000000, 9.524999999999991473 ) ) ;
#18266 =( GEOMETRIC_REPRESENTATION_CONTEXT ( 3 ) GLOBAL_UNCERTAINTY_ASSIGNED_CONTEXT ( ( #11033 ) ) GLOBAL_UNIT_ASSIGNED_CONTEXT ( ( #49299, #11996, #61909 ) ) REPRESENTATION_CONTEXT ( 'NONE', 'WORKASPACE' ) );
#18267 = FACE_OUTER_BOUND ( 'NONE', #33288, .T. ) ;
#18268 = EDGE_CURVE ( 'NONE', #28936, #63225, #27624, .T. ) ;
#18269 = AXIS2_PLACEMENT_3D ( 'NONE', #698, #65122, #59860 ) ;
#18270 = CARTESIAN_POINT ( 'NONE',  ( 66.74999999999998579, 37.00000000000000000, -3.750000000000000000 ) ) ;
#18272 = ADVANCED_FACE ( 'NONE', ( #47994 ), #58152, .F. ) ;
#18271 = ORIENTED_EDGE ( 'NONE', *, *, #48419, .T. ) ;
#18273 = CIRCLE ( 'NONE', #1389, 26.99999999999999645 ) ;
#18274 = CARTESIAN_POINT ( 'NONE',  ( -45.91547277936962956, 9.430195807687216103, -6.000000000000000000 ) ) ;
#18275 = EDGE_CURVE ( 'NONE', #56480, #32986, #10318, .T. ) ;
#18276 = DIRECTION ( 'NONE',  ( 0.000000000000000000, 0.000000000000000000, 1.000000000000000000 ) ) ;
#18277 = CARTESIAN_POINT ( 'NONE',  ( -8.082903768654762899, 3.516382302766490365E-15, 7.500000000000000000 ) ) ;
#18278 = CARTESIAN_POINT ( 'NONE',  ( -99.20499999999999829, -2.607480562269071545, -8.024999999999991473 ) ) ;
#18279 = CARTESIAN_POINT ( 'NONE',  ( 1.754102292061050283, 154.4999999999999716, -9.372469107644919362 ) ) ;
#18280 = FACE_OUTER_BOUND ( 'NONE', #13639, .T. ) ;
#18281 = CARTESIAN_POINT ( 'NONE',  ( 68.99999999999998579, 1.000000000000008438, 3.000000000000000000 ) ) ;
#18282 = EDGE_CURVE ( 'NONE', #47636, #45878, #48552, .T. ) ;
#18283 = CIRCLE ( 'NONE', #7082, 0.5000000000000004441 ) ;
#18284 = TOROIDAL_SURFACE ( 'NONE', #14940, 0.5000000000000000000, 0.2500000000000000000 ) ;
#18285 = EDGE_CURVE ( 'NONE', #67099, #60790, #41644, .T. ) ;
#18286 = CARTESIAN_POINT ( 'NONE',  ( -97.79499999999998749, 2.607480562269069324, -8.024999999999993250 ) ) ;
#18287 = CARTESIAN_POINT ( 'NONE',  ( 5.598654528085805993, 121.3549999999999898, 7.705886871421374629 ) ) ;
#18288 = CARTESIAN_POINT ( 'NONE',  ( -73.94499999999997897, -9.827790563157499189E-16, -8.024999999999991473 ) ) ;
#18289 = EDGE_CURVE ( 'NONE', #23696, #60435, #58031, .T. ) ;
#18290 = DIRECTION ( 'NONE',  ( -0.000000000000000000, 1.000000000000000000, -0.000000000000000000 ) ) ;
#18291 = CARTESIAN_POINT ( 'NONE',  ( -6.826472737025120807, 141.9929263765338305, 4.959722759717906548 ) ) ;
#18292 = ADVANCED_FACE ( 'NONE', ( #37782 ), #48317, .T. ) ;
#18293 = CARTESIAN_POINT ( 'NONE',  ( 9.250000000000003553, 27.74999999999998934, -4.000000000000000000 ) ) ;
#18294 = VECTOR ( 'NONE', #32108, 1000.000000000000000 ) ;
#18295 = LINE ( 'NONE', #61194, #22452 ) ;
#18296 = DIRECTION ( 'NONE',  ( -1.000000000000000000, 0.000000000000000000, 0.000000000000000000 ) ) ;
#18297 = VERTEX_POINT ( 'NONE', #64103 ) ;
#18298 = EDGE_CURVE ( 'NONE', #19782, #53539, #3958, .T. ) ;
#18299 = CARTESIAN_POINT ( 'NONE',  ( -114.7429263765338021, -5.598654528085803328, -7.705886871421366635 ) ) ;
#18300 = DIRECTION ( 'NONE',  ( 0.000000000000000000, 0.000000000000000000, 1.000000000000000000 ) ) ;
#18301 = CARTESIAN_POINT ( 'NONE',  ( -140.2450000000000045, -4.716976649647093289, -6.492361379858945902 ) ) ;
#18302 = CARTESIAN_POINT ( 'NONE',  ( 57.00000000000000000, 13.00000000000000178, -60.00402776293827145 ) ) ;
#18303 = COLOUR_RGB ( '', 0.31764706, 0.68627451, 0.89019608) ;
#18304 = DIRECTION ( 'NONE',  ( -0.000000000000000000, -1.000000000000000000, 0.000000000000000000 ) ) ;
#18305 = CARTESIAN_POINT ( 'NONE',  ( -44.99999999999977973, 146.9999999999999716, 9.500000000000000000 ) ) ;
#18306 = SURFACE_SIDE_STYLE ('',( #60843 ) ) ;
#18307 = ORIENTED_EDGE ( 'NONE', *, *, #7449, .T. ) ;
#18309 = VERTEX_POINT ( 'NONE', #20138 ) ;
#18308 = COLOUR_RGB ( '', 0.40784314, 0.44705882, 0.49803922) ;
#18310 = VECTOR ( 'NONE', #62061, 1000.000000000000000 ) ;
#18311 = FACE_OUTER_BOUND ( 'NONE', #10570, .T. ) ;
#18312 = CIRCLE ( 'NONE', #60963, 5.499999999999976907 ) ;
#18313 = DIRECTION ( 'NONE',  ( -0.000000000000000000, -0.000000000000000000, -1.000000000000000000 ) ) ;
#18314 = DIRECTION ( 'NONE',  ( 0.000000000000000000, 1.000000000000000000, 0.000000000000000000 ) ) ;
#18315 = DIRECTION ( 'NONE',  ( -1.000000000000000000, 0.000000000000000000, 0.000000000000000000 ) ) ;
#18316 = DIRECTION ( 'NONE',  ( -1.000000000000000000, 0.000000000000000000, 0.000000000000000000 ) ) ;
#18317 = ORIENTED_EDGE ( 'NONE', *, *, #63399, .T. ) ;
#18318 = CARTESIAN_POINT ( 'NONE',  ( -132.8050000000000068, -8.437984349512086979, 5.166775262442717831E-16 ) ) ;
#18319 = ORIENTED_EDGE ( 'NONE', *, *, #13330, .T. ) ;
#18320 = ORIENTED_EDGE ( 'NONE', *, *, #47663, .F. ) ;
#18321 = LINE ( 'NONE', #19337, #3193 ) ;
#18322 = LINE ( 'NONE', #6362, #36638 ) ;
#18323 = PRESENTATION_LAYER_ASSIGNMENT (  '', '', ( #37457 ) ) ;
#18324 = VERTEX_POINT ( 'NONE', #63066 ) ;
#18325 = DIRECTION ( 'NONE',  ( 0.000000000000000000, 0.000000000000000000, 1.000000000000000000 ) ) ;
#18326 = AXIS2_PLACEMENT_3D ( 'NONE', #23953, #19361, #61245 ) ;
#18327 = FACE_OUTER_BOUND ( 'NONE', #2167, .T. ) ;
#18328 = CARTESIAN_POINT ( 'NONE',  ( 5.598654528085805993, 141.2449999999999761, 7.705886871421374629 ) ) ;
#18329 = DIRECTION ( 'NONE',  ( 0.000000000000000000, 0.000000000000000000, 1.000000000000000000 ) ) ;
#18330 = EDGE_CURVE ( 'NONE', #47699, #15837, #23799, .T. ) ;
#18331 = CIRCLE ( 'NONE', #60984, 17.42000000000001236 ) ;
#18332 = ORIENTED_EDGE ( 'NONE', *, *, #55579, .F. ) ;
#18333 = DIRECTION ( 'NONE',  ( 1.156482317317873451E-16, 1.000000000000000000, -0.000000000000000000 ) ) ;
#18334 = CARTESIAN_POINT ( 'NONE',  ( -9.058813317711338797, 144.4550000000000125, 2.943386871421373563 ) ) ;
#18335 = CARTESIAN_POINT ( 'NONE',  ( -51.95499999999996987, -7.632228543268599452, 2.479861379858951054 ) ) ;
#18336 = DIRECTION ( 'NONE',  ( 0.000000000000000000, -1.000000000000000000, 0.000000000000000000 ) ) ;
#18337 = VERTEX_POINT ( 'NONE', #7103 ) ;
#18338 = CARTESIAN_POINT ( 'NONE',  ( 0.000000000000000000, 110.9429263765338192, -8.025000000000000355 ) ) ;
#18339 = CARTESIAN_POINT ( 'NONE',  ( 3.999798566743338668, 49.09558629977726696, 7.322456175549363344 ) ) ;
#18340 = LINE ( 'NONE', #7081, #61358 ) ;
#18341 = PRESENTATION_LAYER_ASSIGNMENT (  '', '', ( #44229 ) ) ;
#18342 = STYLED_ITEM ( 'NONE', ( #50655 ), #29531 ) ;
#18343 = DIRECTION ( 'NONE',  ( 1.000000000000000000, 0.000000000000000000, 0.000000000000000000 ) ) ;
#18344 = DIRECTION ( 'NONE',  ( -0.000000000000000000, 0.000000000000000000, 1.000000000000000000 ) ) ;
#18345 = ORIENTED_EDGE ( 'NONE', *, *, #6557, .T. ) ;
#18346 = DIRECTION ( 'NONE',  ( -0.000000000000000000, 1.000000000000000000, -0.000000000000000000 ) ) ;
#18347 = ORIENTED_EDGE ( 'NONE', *, *, #43370, .T. ) ;
#18348 = CARTESIAN_POINT ( 'NONE',  ( 21.50000000000000711, 21.99999999999998224, 4.000000000000000000 ) ) ;
#18349 = FACE_OUTER_BOUND ( 'NONE', #26850, .T. ) ;
#18350 = DIRECTION ( 'NONE',  ( 0.000000000000000000, 0.000000000000000000, 1.000000000000000000 ) ) ;
#18351 = CARTESIAN_POINT ( 'NONE',  ( -161.0050000000000239, 6.826472737025116366, 4.959722759717898555 ) ) ;
#18352 = ORIENTED_EDGE ( 'NONE', *, *, #24389, .F. ) ;
#18353 =( GEOMETRIC_REPRESENTATION_CONTEXT ( 3 ) GLOBAL_UNCERTAINTY_ASSIGNED_CONTEXT ( ( #41284 ) ) GLOBAL_UNIT_ASSIGNED_CONTEXT ( ( #22159, #43658, #16227 ) ) REPRESENTATION_CONTEXT ( 'NONE', 'WORKASPACE' ) );
#18354 = CARTESIAN_POINT ( 'NONE',  ( 0.000000000000000000, 2.299999999999999822, 0.000000000000000000 ) ) ;
#18355 = CARTESIAN_POINT ( 'NONE',  ( 0.000000000000000000, 114.4999999999999574, 0.000000000000000000 ) ) ;
#18356 = CARTESIAN_POINT ( 'NONE',  ( -99.05707362346618083, 0.000000000000000000, 9.524999999999991473 ) ) ;
#18357 = PRESENTATION_STYLE_ASSIGNMENT (( #61930 ) ) ;
#18358 =( BOUNDED_CURVE ( )  B_SPLINE_CURVE ( 2, ( #18148, #35014, #56465, #66686, #2612, #67727, #66325, #29742, #41025, #61718, #50508 ),
 .UNSPECIFIED., .F., .F. ) 
 B_SPLINE_CURVE_WITH_KNOTS ( ( 3, 2, 2, 2, 2, 3 ),
 ( 0.8043478260869565410, 0.8065217391304347894, 0.8086956521739130377, 0.8108695652173912860, 0.8130434782608695343, 0.8152173913043477826 ),
 .UNSPECIFIED. ) 
 CURVE ( )  GEOMETRIC_REPRESENTATION_ITEM ( )  RATIONAL_B_SPLINE_CURVE ( ( 1.000000000000000000, 0.9510565162951535312, 1.000000000000000000, 0.9510565162951535312, 1.000000000000000000, 0.9510565162951535312, 1.000000000000000000, 0.9510565162951535312, 1.000000000000000000, 0.9510565162951535312, 1.000000000000000000 ) ) 
 REPRESENTATION_ITEM ( '' )  );
#18359 = ORIENTED_EDGE ( 'NONE', *, *, #50683, .T. ) ;
#18360 = VERTEX_POINT ( 'NONE', #16980 ) ;
#18361 = DIRECTION ( 'NONE',  ( 1.000000000000000000, -0.000000000000000000, -0.000000000000000000 ) ) ;
#18362 = CARTESIAN_POINT ( 'NONE',  ( -78.05499999999997840, -9.827790563157499189E-16, -8.024999999999991473 ) ) ;
#18363 = ORIENTED_EDGE ( 'NONE', *, *, #702, .F. ) ;
#18364 = EDGE_CURVE ( 'NONE', #17866, #6972, #28532, .T. ) ;
#18365 = SURFACE_SIDE_STYLE ('',( #19018 ) ) ;
#18366 = CIRCLE ( 'NONE', #57668, 0.5000000000000004441 ) ;
#18368 = MECHANICAL_DESIGN_GEOMETRIC_PRESENTATION_REPRESENTATION (  '', ( #42003 ), #69418 ) ;
#18367 = MECHANICAL_DESIGN_GEOMETRIC_PRESENTATION_REPRESENTATION (  '', ( #52065 ), #15014 ) ;
#18369 = ADVANCED_FACE ( 'NONE', ( #17681 ), #44093, .T. ) ;
#18370 =( GEOMETRIC_REPRESENTATION_CONTEXT ( 3 ) GLOBAL_UNCERTAINTY_ASSIGNED_CONTEXT ( ( #26230 ) ) GLOBAL_UNIT_ASSIGNED_CONTEXT ( ( #29303, #20132, #30332 ) ) REPRESENTATION_CONTEXT ( 'NONE', 'WORKASPACE' ) );
#18371 =( NAMED_UNIT ( * ) SI_UNIT ( $, .STERADIAN. ) SOLID_ANGLE_UNIT ( ) );
#18372 = EDGE_LOOP ( 'NONE', ( #47195, #44774, #51521, #49585 ) ) ;
#18373 = LINE ( 'NONE', #54922, #64097 ) ;
#18375 = CARTESIAN_POINT ( 'NONE',  ( -23.21231517720797655, 117.4999999999999716, -9.500000000000000000 ) ) ;
#18374 = SURFACE_SIDE_STYLE ('',( #45135 ) ) ;
#18376 = AXIS2_PLACEMENT_3D ( 'NONE', #69096, #58184, #42404 ) ;
#18377 = CARTESIAN_POINT ( 'NONE',  ( -5.598654528085806881, 142.7449999999999761, -7.705886871421374629 ) ) ;
#18378 = CARTESIAN_POINT ( 'NONE',  ( -107.6949999999999932, -8.437984349512085203, 5.166775262442717831E-16 ) ) ;
#18379 = EDGE_CURVE ( 'NONE', #42065, #60451, #5688, .T. ) ;
#18380 = COLOUR_RGB ( '', 0.09019608, 0.27058824, 0.51372549) ;
#18381 = DIRECTION ( 'NONE',  ( -1.000000000000000000, -0.000000000000000000, -0.000000000000000000 ) ) ;
#18383 = CARTESIAN_POINT ( 'NONE',  ( -19.33438955202580090, 11.73703352805583933, 2.513953393961228855 ) ) ;
#18382 = CARTESIAN_POINT ( 'NONE',  ( 0.000000000000000000, 0.000000000000000000, 0.000000000000000000 ) ) ;
#18384 = ADVANCED_FACE ( 'NONE', ( #11679 ), #62923, .T. ) ;
#18385 = CARTESIAN_POINT ( 'NONE',  ( -146.5429263765338135, 9.058813317711329915, 2.943386871421369566 ) ) ;
#18386 = STYLED_ITEM ( 'NONE', ( #11896 ), #30884 ) ;
#18387 = CARTESIAN_POINT ( 'NONE',  ( -169.9449999999999932, -9.827790563157499189E-16, -8.024999999999991473 ) ) ;
#18388 = AXIS2_PLACEMENT_3D ( 'NONE', #64313, #16513, #27348 ) ;
#18389 = CARTESIAN_POINT ( 'NONE',  ( -195.0000000000000000, 0.000000000000000000, 9.524999999999991473 ) ) ;
#18390 = PRESENTATION_STYLE_ASSIGNMENT (( #28904 ) ) ;
#18391 = ORIENTED_EDGE ( 'NONE', *, *, #52659, .F. ) ;
#18392 = CARTESIAN_POINT ( 'NONE',  ( -6.826472737025120807, 128.1070736234661638, 4.959722759717906548 ) ) ;
#18393 = ORIENTED_EDGE ( 'NONE', *, *, #66055, .T. ) ;
#18394 = AXIS2_PLACEMENT_3D ( 'NONE', #23880, #49950, #17919 ) ;
#18395 = LINE ( 'NONE', #50748, #33627 ) ;
#18396 = DIRECTION ( 'NONE',  ( -1.000000000000000000, 0.000000000000000000, 0.000000000000000000 ) ) ;
#18397 = EDGE_LOOP ( 'NONE', ( #22267, #16310, #68659, #60128 ) ) ;
#18398 = CARTESIAN_POINT ( 'NONE',  ( -163.7049999999999841, 2.607480562269072433, 8.024999999999991473 ) ) ;
#18399 = COLOUR_RGB ( '', 0.40784314, 0.44705882, 0.49803922) ;
#18400 = ORIENTED_EDGE ( 'NONE', *, *, #30301, .F. ) ;
#18401 = DIRECTION ( 'NONE',  ( 1.000000000000000000, -0.000000000000000000, 0.000000000000000000 ) ) ;
#18402 = FILL_AREA_STYLE_COLOUR ( '', #34117 ) ;
#18403 = AXIS2_PLACEMENT_3D ( 'NONE', #44311, #48542, #31968 ) ;
#18404 = DIRECTION ( 'NONE',  ( 0.000000000000000000, 1.000000000000000000, 0.000000000000000000 ) ) ;
#18405 = CARTESIAN_POINT ( 'NONE',  ( -74.99999999999998579, 50.00000000000000000, -9.500000000000000000 ) ) ;
#18406 = CARTESIAN_POINT ( 'NONE',  ( 9.058813317711337021, 111.5449999999999875, 2.943386871421375783 ) ) ;
#18407 = EDGE_CURVE ( 'NONE', #38702, #28358, #11445, .T. ) ;
#18408 = STYLED_ITEM ( 'NONE', ( #30250 ), #47148 ) ;
#18409 = VERTEX_POINT ( 'NONE', #12354 ) ;
#18410 = CARTESIAN_POINT ( 'NONE',  ( 4.250000000000001776, 21.74999999999998579, 4.000000000000000000 ) ) ;
#18411 = CARTESIAN_POINT ( 'NONE',  ( 8.102448949553181734, 116.1049999999999756, -5.886773742842746238 ) ) ;
#18412 = CARTESIAN_POINT ( 'NONE',  ( -84.05499999999999261, -9.827790563157499189E-16, -8.024999999999991473 ) ) ;
#18413 = EDGE_CURVE ( 'NONE', #51444, #13259, #50709, .T. ) ;
#18414 = CARTESIAN_POINT ( 'NONE',  ( 9.058813317711337021, 124.6549999999999869, 2.943386871421375783 ) ) ;
#18415 = CARTESIAN_POINT ( 'NONE',  ( 20.30121256018846765, 114.9093931177592509, 10.36597400192487939 ) ) ;
#18416 = VECTOR ( 'NONE', #68662, 1000.000000000000000 ) ;
#18417 = CARTESIAN_POINT ( 'NONE',  ( -100.9429263765338050, 0.000000000000000000, 9.524999999999991473 ) ) ;
#18418 = FILL_AREA_STYLE_COLOUR ( '', #51482 ) ;
#18419 = FILL_AREA_STYLE_COLOUR ( '', #26090 ) ;
#18420 = ORIENTED_EDGE ( 'NONE', *, *, #56359, .F. ) ;
#18422 = CARTESIAN_POINT ( 'NONE',  ( 74.50000000000000000, 19.30628705663858113, -6.500000000000000000 ) ) ;
#18421 = PRESENTATION_LAYER_ASSIGNMENT (  '', '', ( #39791 ) ) ;
#18423 = CARTESIAN_POINT ( 'NONE',  ( -50.84499999999997044, -7.632228543268599452, 2.479861379858951054 ) ) ;
#18424 = VERTEX_POINT ( 'NONE', #55638 ) ;
#18425 = CARTESIAN_POINT ( 'NONE',  ( 6.000000000000017764, 43.00000000000000000, 29.49447654986459710 ) ) ;
#18426 = AXIS2_PLACEMENT_3D ( 'NONE', #41732, #42439, #16038 ) ;
#18427 = DIRECTION ( 'NONE',  ( -0.000000000000000000, -0.000000000000000000, 1.000000000000000000 ) ) ;
#18428 = DIRECTION ( 'NONE',  ( 1.000000000000000000, 0.000000000000000000, 0.000000000000000000 ) ) ;
#18429 = COLOUR_RGB ( '', 0.08235294, 0.09019608, 0.10196078) ;
#18430 = EDGE_LOOP ( 'NONE', ( #23006, #62549, #44403, #57093 ) ) ;
#18431 = CARTESIAN_POINT ( 'NONE',  ( -50.49993558012277362, -12.27943627009380201, 1.315570835516365777 ) ) ;
#18432 = CARTESIAN_POINT ( 'NONE',  ( -51.44499999999999318, 0.000000000000000000, 8.024999999999991473 ) ) ;
#18433 = DIRECTION ( 'NONE',  ( 0.000000000000000000, 1.000000000000000000, 0.000000000000000000 ) ) ;
#18434 = ORIENTED_EDGE ( 'NONE', *, *, #23598, .F. ) ;
#18435 = EDGE_CURVE ( 'NONE', #5753, #17573, #22650, .T. ) ;
#18436 = TOROIDAL_SURFACE ( 'NONE', #30762, 0.5000000000000000000, 0.2500000000000000000 ) ;
#18437 = CARTESIAN_POINT ( 'NONE',  ( -74.10613849977178802, 9.348154474468920228, 6.165151716360274925 ) ) ;
#18438 = CARTESIAN_POINT ( 'NONE',  ( -100.1049999999999898, -6.826472737025115478, 4.959722759717900331 ) ) ;
#18439 = ORIENTED_EDGE ( 'NONE', *, *, #57041, .T. ) ;
#18440 = EDGE_CURVE ( 'NONE', #65168, #43714, #41770, .T. ) ;
#18441 = DIRECTION ( 'NONE',  ( -0.000000000000000000, -0.000000000000000000, -1.000000000000000000 ) ) ;
#18442 = CYLINDRICAL_SURFACE ( 'NONE', #46635, 0.2500000000000002220 ) ;
#18443 = CARTESIAN_POINT ( 'NONE',  ( -149.3070736234662093, -10.01517768586948698, 6.132527647946031529E-16 ) ) ;
#18444 = FILL_AREA_STYLE_COLOUR ( '', #41865 ) ;
#18445 = CARTESIAN_POINT ( 'NONE',  ( 5.598654528085805993, 144.2449999999999761, 7.705886871421374629 ) ) ;
#18446 = CARTESIAN_POINT ( 'NONE',  ( -88.25707362346616947, 5.598654528085800663, -7.705886871421367523 ) ) ;
#18447 = AXIS2_PLACEMENT_3D ( 'NONE', #26217, #10064, #31488 ) ;
#18448 = AXIS2_PLACEMENT_3D ( 'NONE', #40594, #35300, #41295 ) ;
#18449 = EDGE_CURVE ( 'NONE', #21270, #34770, #26027, .T. ) ;
#18450 = LINE ( 'NONE', #39935, #57652 ) ;
#18451 = EDGE_CURVE ( 'NONE', #50178, #58809, #50727, .T. ) ;
#18452 = CARTESIAN_POINT ( 'NONE',  ( 36.00000000000002132, 0.000000000000000000, -77.00402776293825013 ) ) ;
#18453 = CIRCLE ( 'NONE', #63338, 8.499999999999992895 ) ;
#18454 = CARTESIAN_POINT ( 'NONE',  ( -124.4049999999999869, -2.607480562269069768, 8.024999999999991473 ) ) ;
#18455 = DIRECTION ( 'NONE',  ( 0.000000000000000000, 0.000000000000000000, 1.000000000000000000 ) ) ;
#18456 = DIRECTION ( 'NONE',  ( -7.816271194327172234E-17, 0.000000000000000000, -1.000000000000000000 ) ) ;
#18457 = CARTESIAN_POINT ( 'NONE',  ( -9.058813317711337021, 113.0449999999999875, -2.943386871421374895 ) ) ;
#18458 = CARTESIAN_POINT ( 'NONE',  ( -134.8449999999999989, -7.632228543268599452, 2.479861379858951054 ) ) ;
#18459 = EDGE_CURVE ( 'NONE', #36655, #54902, #56330, .T. ) ;
#18460 =( GEOMETRIC_REPRESENTATION_CONTEXT ( 3 ) GLOBAL_UNCERTAINTY_ASSIGNED_CONTEXT ( ( #52311 ) ) GLOBAL_UNIT_ASSIGNED_CONTEXT ( ( #21671, #32556, #43533 ) ) REPRESENTATION_CONTEXT ( 'NONE', 'WORKASPACE' ) );
#18461 = CARTESIAN_POINT ( 'NONE',  ( -124.6449999999999960, 4.716976649647091513, -6.492361379858946790 ) ) ;
#18462 = LINE ( 'NONE', #34611, #42604 ) ;
#18463 = ORIENTED_EDGE ( 'NONE', *, *, #48019, .T. ) ;
#18464 = CARTESIAN_POINT ( 'NONE',  ( -146.1570736234662036, -9.058813317711329915, -2.943386871421370898 ) ) ;
#18465 = DIRECTION ( 'NONE',  ( 0.000000000000000000, 1.000000000000000000, 0.000000000000000000 ) ) ;
#18466 = EDGE_CURVE ( 'NONE', #60291, #69646, #5808, .T. ) ;
#18467 = CARTESIAN_POINT ( 'NONE',  ( -180.5929263765338249, -3.094860106618431139, -9.524999999999991473 ) ) ;
#18468 = CARTESIAN_POINT ( 'NONE',  ( -52.34499999999997755, 7.632228543268599452, -2.479861379858951942 ) ) ;
#18469 = PRESENTATION_LAYER_ASSIGNMENT (  '', '', ( #19557 ) ) ;
#18470 =( NAMED_UNIT ( * ) SI_UNIT ( $, .STERADIAN. ) SOLID_ANGLE_UNIT ( ) );
#18471 = CARTESIAN_POINT ( 'NONE',  ( 60.00000000000000000, 1.797044900979284448E-15, 11.50000000000000000 ) ) ;
#18472 = VECTOR ( 'NONE', #1138, 1000.000000000000000 ) ;
#18473 = CARTESIAN_POINT ( 'NONE',  ( 4.000000000000029310, 34.36176364315826248, 80.00402776293826435 ) ) ;
#18474 = PRODUCT_DEFINITION_CONTEXT ( 'detailed design', #21288, 'design' ) ;
#18475 = CARTESIAN_POINT ( 'NONE',  ( -91.94292637653380496, 0.000000000000000000, 9.524999999999991473 ) ) ;
#18476 = SHAPE_DEFINITION_REPRESENTATION ( #31602, #14155 ) ;
#18477 = CARTESIAN_POINT ( 'NONE',  ( -18.25000000000000711, 33.74999999999999289, 4.000000000000000000 ) ) ;
#18478 =( BOUNDED_CURVE ( )  B_SPLINE_CURVE ( 2, ( #47956, #48270, #22195, #26076, #27098, #69354, #327, #21861, #16939, #43373, #47610 ),
 .UNSPECIFIED., .F., .F. ) 
 B_SPLINE_CURVE_WITH_KNOTS ( ( 3, 2, 2, 2, 2, 3 ),
 ( 0.3804347826086866280, 0.3826086956521648208, 0.3847826086956430136, 0.3869565217391212619, 0.3891304347825994547, 0.3913043478260777031 ),
 .UNSPECIFIED. ) 
 CURVE ( )  GEOMETRIC_REPRESENTATION_ITEM ( )  RATIONAL_B_SPLINE_CURVE ( ( 1.000000000000203615, 0.9510565162949498053, 1.000000000000000000, 0.9510565162951535312, 1.000000000000000000, 0.9510565162951535312, 1.000000000000000000, 0.9510565162951535312, 1.000000000000000000, 0.9510565162953622531, 0.9999999999997912781 ) ) 
 REPRESENTATION_ITEM ( '' )  );
#18479 = LINE ( 'NONE', #45595, #40607 ) ;
#18480 = CARTESIAN_POINT ( 'NONE',  ( -9.250000000000003553, 25.24999999999998934, -4.000000000000000000 ) ) ;
#18481 = DIRECTION ( 'NONE',  ( -1.000000000000000000, 0.000000000000000000, 0.000000000000000000 ) ) ;
#18482 =( NAMED_UNIT ( * ) SI_UNIT ( $, .STERADIAN. ) SOLID_ANGLE_UNIT ( ) );
#18483 = AXIS2_PLACEMENT_3D ( 'NONE', #45762, #51355, #40475 ) ;
#18484 = ORIENTED_EDGE ( 'NONE', *, *, #22651, .T. ) ;
#18485 = SURFACE_SIDE_STYLE ('',( #38935 ) ) ;
#18486 = DIRECTION ( 'NONE',  ( 1.000000000000000000, 0.000000000000000000, -0.000000000000000000 ) ) ;
#18487 = DIRECTION ( 'NONE',  ( 8.659560562354722084E-17, -0.7071067811865647812, 0.7071067811865302533 ) ) ;
#18488 = ORIENTED_EDGE ( 'NONE', *, *, #43516, .F. ) ;
#18489 = DIRECTION ( 'NONE',  ( -0.000000000000000000, -0.000000000000000000, 1.000000000000000000 ) ) ;
#18490 = CARTESIAN_POINT ( 'NONE',  ( 4.716976649647096842, 125.8570736234661496, 6.492361379858953896 ) ) ;
#18491 = ADVANCED_FACE ( 'NONE', ( #2455 ), #25005, .F. ) ;
#18492 = TOROIDAL_SURFACE ( 'NONE', #53297, 12.50000000000000000, 0.5000000000000000000 ) ;
#18493 = FILL_AREA_STYLE ('',( #14596 ) ) ;
#18494 = PRESENTATION_STYLE_ASSIGNMENT (( #66314 ) ) ;
#18495 = CARTESIAN_POINT ( 'NONE',  ( 15.98999599679679839, 146.4999999999999716, -9.500000000000000000 ) ) ;
#18496 = ORIENTED_EDGE ( 'NONE', *, *, #52902, .T. ) ;
#18497 = VECTOR ( 'NONE', #66182, 1000.000000000000000 ) ;
#18498 = DIRECTION ( 'NONE',  ( 1.000000000000000000, -7.709882115452468306E-16, -0.000000000000000000 ) ) ;
#18499 = CARTESIAN_POINT ( 'NONE',  ( 6.000000000000017764, 43.00000000000000000, 28.38386403503541899 ) ) ;
#18500 = FILL_AREA_STYLE_COLOUR ( '', #3634 ) ;
#18501 =( GEOMETRIC_REPRESENTATION_CONTEXT ( 3 ) GLOBAL_UNCERTAINTY_ASSIGNED_CONTEXT ( ( #5801 ) ) GLOBAL_UNIT_ASSIGNED_CONTEXT ( ( #32473, #54286, #60585 ) ) REPRESENTATION_CONTEXT ( 'NONE', 'WORKASPACE' ) );
#18502 = CARTESIAN_POINT ( 'NONE',  ( -73.55707362346616662, -1.166476076187852838E-15, -9.524999999999991473 ) ) ;
#18503 = CARTESIAN_POINT ( 'NONE',  ( -82.34499999999998465, 7.632228543268599452, -2.479861379858951942 ) ) ;
#18504 = ORIENTED_EDGE ( 'NONE', *, *, #58628, .T. ) ;
#18505 = EDGE_CURVE ( 'NONE', #17255, #11384, #68716, .T. ) ;
#18506 = ORIENTED_EDGE ( 'NONE', *, *, #64312, .F. ) ;
#18507 = CARTESIAN_POINT ( 'NONE',  ( -76.79292637653379927, -3.094860106618429807, 9.524999999999991473 ) ) ;
#18508 = DIRECTION ( 'NONE',  ( -0.7071067811865426878, 0.000000000000000000, -0.7071067811865524577 ) ) ;
#18509 = MECHANICAL_DESIGN_GEOMETRIC_PRESENTATION_REPRESENTATION (  '', ( #30837 ), #9551 ) ;
#18510 = ADVANCED_FACE ( 'NONE', ( #30259 ), #8150, .T. ) ;
#18511 =( GEOMETRIC_REPRESENTATION_CONTEXT ( 3 ) GLOBAL_UNCERTAINTY_ASSIGNED_CONTEXT ( ( #8125 ) ) GLOBAL_UNIT_ASSIGNED_CONTEXT ( ( #40651, #29726, #68399 ) ) REPRESENTATION_CONTEXT ( 'NONE', 'WORKASPACE' ) );
#18512 = VERTEX_POINT ( 'NONE', #19730 ) ;
#18513 = EDGE_CURVE ( 'NONE', #38684, #27999, #2091, .T. ) ;
#18514 = SURFACE_STYLE_USAGE ( .BOTH. , #67383 ) ;
#18515 = VERTEX_POINT ( 'NONE', #51399 ) ;
#18516 = CARTESIAN_POINT ( 'NONE',  ( -137.9929263765338590, 8.102448949553172852, -5.886773742842744461 ) ) ;
#18517 =( LENGTH_UNIT ( ) NAMED_UNIT ( * ) SI_UNIT ( .MILLI., .METRE. ) );
#18518 = CYLINDRICAL_SURFACE ( 'NONE', #45741, 0.5000000000000004441 ) ;
#18519 = STYLED_ITEM ( 'NONE', ( #44126 ), #37898 ) ;
#18520 = CARTESIAN_POINT ( 'NONE',  ( -174.6570736234662036, 9.058813317711329915, 2.943386871421369566 ) ) ;
#18521 = PRESENTATION_STYLE_ASSIGNMENT (( #19546 ) ) ;
#18522 = CARTESIAN_POINT ( 'NONE',  ( 9.058813317711338797, 114.8449999999999847, -2.943386871421372675 ) ) ;
#18523 = CARTESIAN_POINT ( 'NONE',  ( -117.8070736234661950, 10.01517768586948698, -1.839758294383808571E-15 ) ) ;
#18524 = CARTESIAN_POINT ( 'NONE',  ( -1.745454270669494212, 2.292880170259729233, 7.000000000000000000 ) ) ;
#18525 = ADVANCED_FACE ( 'NONE', ( #45121 ), #19013, .T. ) ;
#18526 = VECTOR ( 'NONE', #45664, 1000.000000000000000 ) ;
#18527 = DIRECTION ( 'NONE',  ( 0.000000000000000000, 0.000000000000000000, 1.000000000000000000 ) ) ;
#18528 = ORIENTED_EDGE ( 'NONE', *, *, #9158, .T. ) ;
#18529 = CARTESIAN_POINT ( 'NONE',  ( 69.99999999999998579, 1.000000000000007772, -3.000000000000000000 ) ) ;
#18530 = CARTESIAN_POINT ( 'NONE',  ( -34.99999999999999289, 99.99999999999998579, -9.500000000000000000 ) ) ;
#18531 = ADVANCED_FACE ( 'NONE', ( #45476 ), #46155, .F. ) ;
#18532 = CARTESIAN_POINT ( 'NONE',  ( 27.00000000000001776, 43.00000000000000000, -36.50000000000000000 ) ) ;
#18533 = SURFACE_SIDE_STYLE ('',( #66715 ) ) ;
#18534 = ORIENTED_EDGE ( 'NONE', *, *, #53199, .F. ) ;
#18535 = CARTESIAN_POINT ( 'NONE',  ( -163.4050000000000011, -2.607480562269069768, 8.024999999999991473 ) ) ;
#18536 = FACE_OUTER_BOUND ( 'NONE', #63436, .T. ) ;
#18537 = CARTESIAN_POINT ( 'NONE',  ( 22.75000000000000711, 36.75000000000000000, -4.000000000000000000 ) ) ;
#18538 = CARTESIAN_POINT ( 'NONE',  ( -165.8949999999999818, 6.826472737025116366, 4.959722759717898555 ) ) ;
#18539 = CARTESIAN_POINT ( 'NONE',  ( -159.1449999999999818, -4.716976649647092401, 6.492361379858946790 ) ) ;
#18540 = EDGE_LOOP ( 'NONE', ( #47202, #8464, #23519, #43647 ) ) ;
#18541 = MECHANICAL_DESIGN_GEOMETRIC_PRESENTATION_REPRESENTATION (  '', ( #11798 ), #28602 ) ;
#18542 = DIRECTION ( 'NONE',  ( 0.000000000000000000, 0.000000000000000000, -1.000000000000000000 ) ) ;
#18543 = VECTOR ( 'NONE', #25459, 1000.000000000000000 ) ;
#18544 = FACE_OUTER_BOUND ( 'NONE', #17265, .T. ) ;
#18545 = CARTESIAN_POINT ( 'NONE',  ( -122.8429263765338106, 9.058813317711329915, -2.943386871421373119 ) ) ;
#18546 = CARTESIAN_POINT ( 'NONE',  ( -73.10499999999996135, -6.826472737025115478, 4.959722759717900331 ) ) ;
#18547 = CARTESIAN_POINT ( 'NONE',  ( 1.000000000000000000, 43.00000000000000000, 35.50000000000000000 ) ) ;
#18548 = DIRECTION ( 'NONE',  ( 5.782411586589351722E-16, 1.000000000000000000, -0.000000000000000000 ) ) ;
#18549 = VECTOR ( 'NONE', #45043, 1000.000000000000000 ) ;
#18550 = CARTESIAN_POINT ( 'NONE',  ( -68.54499999999998749, -7.632228543268600340, -2.479861379858950166 ) ) ;
#18551 = CARTESIAN_POINT ( 'NONE',  ( -3.094860106618432471, 146.7049999999999841, -9.525000000000000355 ) ) ;
#18552 = ADVANCED_FACE ( 'NONE', ( #9553 ), #31664, .F. ) ;
#18553 =( NAMED_UNIT ( * ) SI_UNIT ( $, .STERADIAN. ) SOLID_ANGLE_UNIT ( ) );
#18554 = AXIS2_PLACEMENT_3D ( 'NONE', #64329, #20743, #20381 ) ;
#18555 = CIRCLE ( 'NONE', #43319, 0.2500000000000002220 ) ;
#18556 = CARTESIAN_POINT ( 'NONE',  ( -155.7570736234661979, -5.598654528085801552, 7.705886871421367523 ) ) ;
#18557 = EDGE_CURVE ( 'NONE', #47468, #58906, #19318, .T. ) ;
#18558 = UNCERTAINTY_MEASURE_WITH_UNIT (LENGTH_MEASURE( 1.000000000000000082E-05 ), #33255, 'distance_accuracy_value', 'NONE');
#18559 = CARTESIAN_POINT ( 'NONE',  ( 10.00000000000001954, 43.00000000000000000, 28.00000000000000355 ) ) ;
#18560 = CARTESIAN_POINT ( 'NONE',  ( -19.89974874213239886, 114.9999999999999574, -10.50000000000000000 ) ) ;
#18561 = SURFACE_STYLE_USAGE ( .BOTH. , #17542 ) ;
#18562 = DIRECTION ( 'NONE',  ( -3.552713678800500929E-15, 0.000000000000000000, 1.000000000000000000 ) ) ;
#18563 = DIRECTION ( 'NONE',  ( 1.000000000000000000, -1.445602896647339656E-16, 0.000000000000000000 ) ) ;
#18564 = AXIS2_PLACEMENT_3D ( 'NONE', #39472, #38789, #45460 ) ;
#18565 = CARTESIAN_POINT ( 'NONE',  ( 1.804495846578303864, 51.08602766979955589, 7.112547338523483198 ) ) ;
#18566 = ORIENTED_EDGE ( 'NONE', *, *, #31777, .F. ) ;
#18567 = ORIENTED_EDGE ( 'NONE', *, *, #13497, .T. ) ;
#18569 = CARTESIAN_POINT ( 'NONE',  ( -155.0929263765342228, 3.094860106624684803, 9.524999999995451105 ) ) ;
#18568 = VECTOR ( 'NONE', #59646, 1000.000000000000000 ) ;
#18570 = AXIS2_PLACEMENT_3D ( 'NONE', #46975, #51502, #19486 ) ;
#18571 = CARTESIAN_POINT ( 'NONE',  ( 57.24999999999999289, 27.74999999999998934, -4.000000000000000000 ) ) ;
#18572 = CARTESIAN_POINT ( 'NONE',  ( 4.683753779217433078, -5.887500484252664812, 0.4948905776603311213 ) ) ;
#18573 = DIRECTION ( 'NONE',  ( -0.000000000000000000, -1.000000000000000000, -0.000000000000000000 ) ) ;
#18574 = VERTEX_POINT ( 'NONE', #58077 ) ;
#18575 = EDGE_LOOP ( 'NONE', ( #59972, #38810, #12011, #38539 ) ) ;
#18576 = DIRECTION ( 'NONE',  ( -1.000000000000000000, 0.000000000000000000, 0.000000000000000000 ) ) ;
#18577 = CARTESIAN_POINT ( 'NONE',  ( 52.75000000000000000, 24.74999999999998224, -3.750000000000000000 ) ) ;
#18578 = ORIENTED_EDGE ( 'NONE', *, *, #27388, .F. ) ;
#18579 = CARTESIAN_POINT ( 'NONE',  ( -145.0429263765338135, -9.058813317711329915, -2.943386871421370898 ) ) ;
#18580 = EDGE_LOOP ( 'NONE', ( #68713, #150, #67267, #64712 ) ) ;
#18581 = EDGE_CURVE ( 'NONE', #62518, #64181, #58644, .T. ) ;
#18582 = CARTESIAN_POINT ( 'NONE',  ( -115.3449999999999847, 7.632228543268599452, -2.479861379858951942 ) ) ;
#18583 = EDGE_LOOP ( 'NONE', ( #33606, #17545, #45797, #30336, #57862 ) ) ;
#18584 = COLOUR_RGB ( '', 0.31764706, 0.68627451, 0.89019608) ;
#18585 = ORIENTED_EDGE ( 'NONE', *, *, #49144, .F. ) ;
#18586 = AXIS2_PLACEMENT_3D ( 'NONE', #12534, #50543, #2265 ) ;
#18587 = CARTESIAN_POINT ( 'NONE',  ( -74.09989551642895833, 9.371898184802235576, -6.142471281331790323 ) ) ;
#18588 = CARTESIAN_POINT ( 'NONE',  ( 3.000000000000030198, 35.42594141563417054, 80.00402776293826435 ) ) ;
#18589 = CARTESIAN_POINT ( 'NONE',  ( -12.48200500612924024, -11.19251907289281966, 4.331800619050086176 ) ) ;
#18590 = EDGE_CURVE ( 'NONE', #29672, #14650, #20446, .T. ) ;
#18591 = SURFACE_STYLE_FILL_AREA ( #18234 ) ;
#18592 = EDGE_LOOP ( 'NONE', ( #20820, #56751, #58637, #26030 ) ) ;
#18593 = CARTESIAN_POINT ( 'NONE',  ( -7.632228543268607446, 144.5429263765338135, -2.479861379858953718 ) ) ;
#18594 = CARTESIAN_POINT ( 'NONE',  ( -54.23019297999671551, -9.137952730704812510, -3.992206423876322852 ) ) ;
#18595 = DIRECTION ( 'NONE',  ( 0.000000000000000000, 0.000000000000000000, 1.000000000000000000 ) ) ;
#18596 = CYLINDRICAL_SURFACE ( 'NONE', #55352, 3.499999999999999556 ) ;
#18597 = ADVANCED_FACE ( 'NONE', ( #20425 ), #41927, .F. ) ;
#18598 = CARTESIAN_POINT ( 'NONE',  ( 0.000000000000000000, 0.000000000000000000, 42.50000000000000000 ) ) ;
#18599 = ORIENTED_EDGE ( 'NONE', *, *, #64407, .T. ) ;
#18600 = DIRECTION ( 'NONE',  ( -0.07898106964430649801, -0.9968761159932768567, 0.000000000000000000 ) ) ;
#18601 = ORIENTED_EDGE ( 'NONE', *, *, #11585, .F. ) ;
#18602 = SURFACE_STYLE_FILL_AREA ( #29109 ) ;
#18603 = CIRCLE ( 'NONE', #57928, 0.5000000000000004441 ) ;
#18604 = FILL_AREA_STYLE_COLOUR ( '', #43593 ) ;
#18605 = SURFACE_STYLE_FILL_AREA ( #13652 ) ;
#18606 = FACE_OUTER_BOUND ( 'NONE', #44775, .T. ) ;
#18607 = AXIS2_PLACEMENT_3D ( 'NONE', #11504, #59685, #1235 ) ;
#18608 = CARTESIAN_POINT ( 'NONE',  ( -136.5549999999999784, 0.000000000000000000, 8.024999999999991473 ) ) ;
#18609 = DIRECTION ( 'NONE',  ( 0.000000000000000000, 0.000000000000000000, 1.000000000000000000 ) ) ;
#18610 = DIRECTION ( 'NONE',  ( 1.000000000000000000, 0.000000000000000000, 0.000000000000000000 ) ) ;
#18611 = ORIENTED_EDGE ( 'NONE', *, *, #17309, .T. ) ;
#18612 = DIRECTION ( 'NONE',  ( -1.000000000000000000, -5.782411586589331015E-16, 0.000000000000000000 ) ) ;
#18613 = CARTESIAN_POINT ( 'NONE',  ( -45.00000000000000000, 0.000000000000000000, 0.000000000000000000 ) ) ;
#18614 = DIRECTION ( 'NONE',  ( -1.000000000000000000, 0.000000000000000000, 0.000000000000000000 ) ) ;
#18615 = ORIENTED_EDGE ( 'NONE', *, *, #5086, .T. ) ;
#18616 = VERTEX_POINT ( 'NONE', #57721 ) ;
#18617 =( NAMED_UNIT ( * ) PLANE_ANGLE_UNIT ( ) SI_UNIT ( $, .RADIAN. ) );
#18618 = CARTESIAN_POINT ( 'NONE',  ( -30.43796409298414574, -8.467951584774601415, -0.8043461282435629967 ) ) ;
#18619 = ADVANCED_FACE ( 'NONE', ( #58403 ), #21456, .T. ) ;
#18620 = CARTESIAN_POINT ( 'NONE',  ( -48.35499999999998266, -4.716976649647093289, -6.492361379858945902 ) ) ;
#18622 = ORIENTED_EDGE ( 'NONE', *, *, #4922, .T. ) ;
#18621 = AXIS2_PLACEMENT_3D ( 'NONE', #59057, #27014, #48550 ) ;
#18623 = CARTESIAN_POINT ( 'NONE',  ( -183.8050000000000068, -8.437984349512085203, 5.166775262442717831E-16 ) ) ;
#18624 = DIRECTION ( 'NONE',  ( -0.000000000000000000, 1.000000000000000000, -0.000000000000000000 ) ) ;
#18625 = CARTESIAN_POINT ( 'NONE',  ( -57.95707362346616520, 9.058813317711329915, -2.943386871421373119 ) ) ;
#18626 = CARTESIAN_POINT ( 'NONE',  ( -183.1450000000000102, -4.716976649647092401, 6.492361379858946790 ) ) ;
#18627 = CYLINDRICAL_SURFACE ( 'NONE', #45507, 13.99999999999999822 ) ;
#18628 = COLOUR_RGB ( '', 0.31764706, 0.68627451, 0.89019608) ;
#18629 = ORIENTED_EDGE ( 'NONE', *, *, #37126, .F. ) ;
#18630 = CARTESIAN_POINT ( 'NONE',  ( -161.3070736234661808, -10.01517768586948698, 6.132527647946031529E-16 ) ) ;
#18631 = CIRCLE ( 'NONE', #57946, 5.500000000000005329 ) ;
#18632 = CARTESIAN_POINT ( 'NONE',  ( -105.0549999999999926, -9.827790563157499189E-16, -8.024999999999991473 ) ) ;
#18633 = CARTESIAN_POINT ( 'NONE',  ( -27.86759363617253271, -7.579901266040472763, -0.06752590370637777395 ) ) ;
#18634 = CARTESIAN_POINT ( 'NONE',  ( -74.99999999999998579, 50.00000000000000000, 11.50000000000003730 ) ) ;
#18635 = FILL_AREA_STYLE_COLOUR ( '', #16907 ) ;
#18636 = CARTESIAN_POINT ( 'NONE',  ( -104.2449999999999903, -4.716976649647093289, -6.492361379858945902 ) ) ;
#18637 = CARTESIAN_POINT ( 'NONE',  ( -8.102448949553181734, 114.0049999999999812, -5.886773742842749790 ) ) ;
#18638 = CARTESIAN_POINT ( 'NONE',  ( -79.04499999999998749, 7.632228543268600340, 2.479861379858949277 ) ) ;
#18639 = FACE_OUTER_BOUND ( 'NONE', #58589, .T. ) ;
#18640 = DIRECTION ( 'NONE',  ( 0.000000000000000000, 1.000000000000000000, 0.000000000000000000 ) ) ;
#18641 = UNCERTAINTY_MEASURE_WITH_UNIT (LENGTH_MEASURE( 1.000000000000000082E-05 ), #2813, 'distance_accuracy_value', 'NONE');
#18642 = FILL_AREA_STYLE ('',( #19995 ) ) ;
#18643 = CARTESIAN_POINT ( 'NONE',  ( 6.000000000000017764, 43.00000000000000000, -29.49447654986460776 ) ) ;
#18644 = EDGE_LOOP ( 'NONE', ( #39989, #53640, #12264, #33143 ) ) ;
#18645 = CARTESIAN_POINT ( 'NONE',  ( -115.6429263765338078, -5.598654528085801552, 7.705886871421367523 ) ) ;
#18646 = CARTESIAN_POINT ( 'NONE',  ( -141.1449999999999818, -4.716976649647092401, 6.492361379858946790 ) ) ;
#18647 = DIRECTION ( 'NONE',  ( 0.000000000000000000, 0.000000000000000000, 1.000000000000000000 ) ) ;
#18648 = PRESENTATION_LAYER_ASSIGNMENT (  '', '', ( #15317 ) ) ;
#18649 = CARTESIAN_POINT ( 'NONE',  ( 15.98999599679679839, 146.9999999999999716, -9.500000000000000000 ) ) ;
#18650 = AXIS2_PLACEMENT_3D ( 'NONE', #18061, #8211, #29657 ) ;
#18651 = STYLED_ITEM ( 'NONE', ( #15168 ), #662 ) ;
#18652 = ORIENTED_EDGE ( 'NONE', *, *, #42966, .T. ) ;
#18653 = ORIENTED_EDGE ( 'NONE', *, *, #12368, .T. ) ;
#18654 = CIRCLE ( 'NONE', #15323, 0.5000000000000004441 ) ;
#18655 = FACE_OUTER_BOUND ( 'NONE', #16260, .T. ) ;
#18656 = CARTESIAN_POINT ( 'NONE',  ( 4.041451884327379673, -7.000000000000002665, 7.500000000000000000 ) ) ;
#18657 = SURFACE_STYLE_USAGE ( .BOTH. , #12664 ) ;
#18658 = DIRECTION ( 'NONE',  ( 0.000000000000000000, 0.000000000000000000, -1.000000000000000000 ) ) ;
#18659 = SURFACE_STYLE_USAGE ( .BOTH. , #750 ) ;
#18660 = EDGE_LOOP ( 'NONE', ( #48393, #32256, #47596, #52051 ) ) ;
#18661 = CARTESIAN_POINT ( 'NONE',  ( -130.8549999999999898, 4.716976649647094177, 6.492361379858945902 ) ) ;
#18662 = ORIENTED_EDGE ( 'NONE', *, *, #4119, .F. ) ;
#18663 = CIRCLE ( 'NONE', #43430, 0.2500000000000002220 ) ;
#18664 = ORIENTED_EDGE ( 'NONE', *, *, #14094, .T. ) ;
#18665 = CARTESIAN_POINT ( 'NONE',  ( 11.00000000000001776, 26.00000000000000355, -20.50000000000000355 ) ) ;
#18666 = CARTESIAN_POINT ( 'NONE',  ( -83.39292637653379359, 8.102448949553176405, 5.886773742842740909 ) ) ;
#18667 = ORIENTED_EDGE ( 'NONE', *, *, #41571, .F. ) ;
#18668 = ADVANCED_FACE ( 'NONE', ( #31304 ), #16004, .T. ) ;
#18669 = MECHANICAL_DESIGN_GEOMETRIC_PRESENTATION_REPRESENTATION (  '', ( #44522 ), #53469 ) ;
#18670 = DIRECTION ( 'NONE',  ( -1.000000000000000000, 0.000000000000000000, 0.000000000000000000 ) ) ;
#18671 = CARTESIAN_POINT ( 'NONE',  ( 9.058813317711337021, 144.5449999999999875, 2.943386871421375783 ) ) ;
#18672 = CARTESIAN_POINT ( 'NONE',  ( 24.00000000000000000, 1.000000000000000000, 3.000000000000000000 ) ) ;
#18673 = VERTEX_POINT ( 'NONE', #57368 ) ;
#18674 = FACE_OUTER_BOUND ( 'NONE', #27324, .T. ) ;
#18675 = CARTESIAN_POINT ( 'NONE',  ( -3.094860106618434248, 138.9049999999999727, 9.525000000000000355 ) ) ;
#18676 = CARTESIAN_POINT ( 'NONE',  ( -49.85499999999998266, 4.716976649647094177, 6.492361379858945902 ) ) ;
#18677 = CARTESIAN_POINT ( 'NONE',  ( 41.84210526315787604, 107.2928455055531600, -3.500000000000000888 ) ) ;
#18678 = ORIENTED_EDGE ( 'NONE', *, *, #36100, .T. ) ;
#18679 = CARTESIAN_POINT ( 'NONE',  ( -6.826472737025120807, 117.9929263765338021, 4.959722759717906548 ) ) ;
#18680 = UNCERTAINTY_MEASURE_WITH_UNIT (LENGTH_MEASURE( 1.000000000000000082E-05 ), #52584, 'distance_accuracy_value', 'NONE');
#18681 = CARTESIAN_POINT ( 'NONE',  ( -60.00000000000000000, -2.024042244987997205E-14, 11.50000000000000000 ) ) ;
#18682 = EDGE_CURVE ( 'NONE', #15447, #4771, #51215, .T. ) ;
#18683 = DIRECTION ( 'NONE',  ( -0.8660254037844384856, 0.5000000000000003331, 0.000000000000000000 ) ) ;
#18684 = ORIENTED_EDGE ( 'NONE', *, *, #42869, .F. ) ;
#18685 = ADVANCED_FACE ( 'NONE', ( #21111 ), #42609, .F. ) ;
#18686 = CARTESIAN_POINT ( 'NONE',  ( 41.40606286463611241, 107.1009606408074006, 3.493716402184701586 ) ) ;
#18687 = ORIENTED_EDGE ( 'NONE', *, *, #61385, .T. ) ;
#18688 = CARTESIAN_POINT ( 'NONE',  ( -117.4429263765338050, -1.166476076187852838E-15, -9.524999999999991473 ) ) ;
#18689 = CARTESIAN_POINT ( 'NONE',  ( 20.40110905463057023, 114.8435661791816358, 10.33328836125512851 ) ) ;
#18690 = CARTESIAN_POINT ( 'NONE',  ( -49.75000000000000000, 0.000000000000000000, -7.000000000000000000 ) ) ;
#18691 = CARTESIAN_POINT ( 'NONE',  ( -159.3549999999999898, -4.716976649647093289, -6.492361379858945902 ) ) ;
#18693 = ORIENTED_EDGE ( 'NONE', *, *, #21567, .F. ) ;
#18692 = EDGE_CURVE ( 'NONE', #41694, #62679, #43651, .T. ) ;
#18694 = UNCERTAINTY_MEASURE_WITH_UNIT (LENGTH_MEASURE( 1.000000000000000082E-05 ), #60906, 'distance_accuracy_value', 'NONE');
#18695 = EDGE_CURVE ( 'NONE', #1012, #33055, #59412, .T. ) ;
#18696 = CARTESIAN_POINT ( 'NONE',  ( 45.00000000000000000, 9.999999999999992895, -5.999999999999999112 ) ) ;
#18697 =( LENGTH_UNIT ( ) NAMED_UNIT ( * ) SI_UNIT ( .MILLI., .METRE. ) );
#18698 = ORIENTED_EDGE ( 'NONE', *, *, #61318, .F. ) ;
#18699 = ORIENTED_EDGE ( 'NONE', *, *, #40697, .T. ) ;
#18700 = CARTESIAN_POINT ( 'NONE',  ( -18.25000000000000711, 33.74999999999999289, 3.750000000000000000 ) ) ;
#18701 = CIRCLE ( 'NONE', #60220, 113.0000000000000142 ) ;
#18702 = DIRECTION ( 'NONE',  ( 0.000000000000000000, 0.000000000000000000, -1.000000000000000000 ) ) ;
#18703 = CARTESIAN_POINT ( 'NONE',  ( -79.25499999999999545, -4.716976649647092401, 6.492361379858946790 ) ) ;
#18704 = ORIENTED_EDGE ( 'NONE', *, *, #51965, .T. ) ;
#18705 = AXIS2_PLACEMENT_3D ( 'NONE', #23848, #45354, #67112 ) ;
#18706 = CIRCLE ( 'NONE', #1807, 0.5000000000000004441 ) ;
#18707 = DIRECTION ( 'NONE',  ( 0.000000000000000000, 0.000000000000000000, 1.000000000000000000 ) ) ;
#18708 = DIRECTION ( 'NONE',  ( 0.000000000000000000, 0.000000000000000000, 1.000000000000000000 ) ) ;
#18709 = CARTESIAN_POINT ( 'NONE',  ( 35.99999999999999289, 5.000000000000000000, 37.00402776293825724 ) ) ;
#18710 = ORIENTED_EDGE ( 'NONE', *, *, #38841, .F. ) ;
#18711 = CARTESIAN_POINT ( 'NONE',  ( 32.00000000000000711, 43.00000000000000000, -36.50000000000000000 ) ) ;
#18712 = AXIS2_PLACEMENT_3D ( 'NONE', #50504, #66321, #61383 ) ;
#18713 = CARTESIAN_POINT ( 'NONE',  ( -5.598654528085806881, 136.7449999999999761, -7.705886871421374629 ) ) ;
#18714 = CARTESIAN_POINT ( 'NONE',  ( -105.8949999999999676, 6.826472737025116366, 4.959722759717898555 ) ) ;
#18715 = DIRECTION ( 'NONE',  ( 0.000000000000000000, -1.000000000000000000, -0.000000000000000000 ) ) ;
#18716 = UNCERTAINTY_MEASURE_WITH_UNIT (LENGTH_MEASURE( 1.000000000000000082E-05 ), #55486, 'distance_accuracy_value', 'NONE');
#18717 = CARTESIAN_POINT ( 'NONE',  ( -96.20707362346723812, 3.094860106636315056, 9.524999999987000976 ) ) ;
#18718 = CARTESIAN_POINT ( 'NONE',  ( -147.5929263765338249, -3.094860106618431139, -9.524999999999991473 ) ) ;
#18719 = CARTESIAN_POINT ( 'NONE',  ( -167.5449999999999875, -7.632228543268600340, -2.479861379858950166 ) ) ;
#18720 = DIRECTION ( 'NONE',  ( -7.080503983578803083E-17, -1.000000000000000000, 0.000000000000000000 ) ) ;
#18721 = CARTESIAN_POINT ( 'NONE',  ( 0.000000000000000000, -2.500000000000000000, 9.000000000000000000 ) ) ;
#18722 = EDGE_LOOP ( 'NONE', ( #16709, #45351, #39758, #33398 ) ) ;
#18723 = CARTESIAN_POINT ( 'NONE',  ( -9.250000000000003553, 27.74999999999998934, 3.750000000000000000 ) ) ;
#18724 = ORIENTED_EDGE ( 'NONE', *, *, #44771, .T. ) ;
#18725 = PLANE ( 'NONE',  #67528 ) ;
#18726 = LINE ( 'NONE', #29266, #24769 ) ;
#18727 = CARTESIAN_POINT ( 'NONE',  ( 22.00000000000002132, 60.69879356856722552, 69.02971849933236115 ) ) ;
#18728 = CARTESIAN_POINT ( 'NONE',  ( -7.632228543268608334, 142.9570736234661581, 2.479861379858952830 ) ) ;
#18729 = COLOUR_RGB ( '', 0.72549020, 0.75294118, 0.79215686) ;
#18730 = VERTEX_POINT ( 'NONE', #947 ) ;
#18731 = CARTESIAN_POINT ( 'NONE',  ( -160.4049999999999727, -2.607480562269069768, 8.024999999999991473 ) ) ;
#18732 =( GEOMETRIC_REPRESENTATION_CONTEXT ( 3 ) GLOBAL_UNCERTAINTY_ASSIGNED_CONTEXT ( ( #30409 ) ) GLOBAL_UNIT_ASSIGNED_CONTEXT ( ( #29378, #28684, #44924 ) ) REPRESENTATION_CONTEXT ( 'NONE', 'WORKASPACE' ) );
#18733 = ORIENTED_EDGE ( 'NONE', *, *, #66192, .F. ) ;
#18734 = SURFACE_STYLE_FILL_AREA ( #52511 ) ;
#18735 = EDGE_LOOP ( 'NONE', ( #61132, #65004, #60925 ) ) ;
#18736 = ADVANCED_FACE ( 'NONE', ( #22153 ), #23199, .T. ) ;
#18737 = AXIS2_PLACEMENT_3D ( 'NONE', #67731, #30073, #2954 ) ;
#18738 = FACE_OUTER_BOUND ( 'NONE', #43448, .T. ) ;
#18739 = DIRECTION ( 'NONE',  ( 1.000000000000000000, 0.000000000000000000, -0.000000000000000000 ) ) ;
#18740 = CARTESIAN_POINT ( 'NONE',  ( 6.826472737025121695, 159.6070736234661069, -4.959722759717905660 ) ) ;
#18741 = EDGE_CURVE ( 'NONE', #31383, #48589, #10908, .T. ) ;
#18742 = ORIENTED_EDGE ( 'NONE', *, *, #32914, .T. ) ;
#18743 = DIRECTION ( 'NONE',  ( -0.000000000000000000, -0.000000000000000000, 1.000000000000000000 ) ) ;
#18744 = DIRECTION ( 'NONE',  ( 1.000000000000000000, 0.000000000000000000, 0.000000000000000000 ) ) ;
#18745 = CARTESIAN_POINT ( 'NONE',  ( -78.50499999999999545, -6.826472737025113702, -4.959722759717900331 ) ) ;
#18746 =( BOUNDED_CURVE ( )  B_SPLINE_CURVE ( 3, ( #28937, #50429, #45187, #18425 ),
 .UNSPECIFIED., .F., .F. ) 
 B_SPLINE_CURVE_WITH_KNOTS ( ( 4, 4 ),
 ( 3.874630939427412102, 4.712388980384682569 ),
 .UNSPECIFIED. ) 
 CURVE ( )  GEOMETRIC_REPRESENTATION_ITEM ( )  RATIONAL_B_SPLINE_CURVE ( ( 1.000000000000000000, 0.9423636384284016509, 0.9423636384284016509, 1.000000000000000000 ) ) 
 REPRESENTATION_ITEM ( '' )  );
#18747 = CARTESIAN_POINT ( 'NONE',  ( -3.094860106618434248, 138.9049999999999727, 9.525000000000000355 ) ) ;
#18748 = UNCERTAINTY_MEASURE_WITH_UNIT (LENGTH_MEASURE( 1.000000000000000082E-05 ), #40131, 'distance_accuracy_value', 'NONE');
#18749 = CARTESIAN_POINT ( 'NONE',  ( 22.99999999999999289, 5.000000000000000000, -37.00402776293825013 ) ) ;
#18750 = FILL_AREA_STYLE ('',( #55694 ) ) ;
#18751 = CIRCLE ( 'NONE', #33363, 0.2500000000000002220 ) ;
#18752 = CARTESIAN_POINT ( 'NONE',  ( 20.68758241885016247, 114.6823486699484107, 10.00000000000000178 ) ) ;
#18753 = EDGE_CURVE ( 'NONE', #13980, #9643, #42989, .T. ) ;
#18754 = PRESENTATION_STYLE_ASSIGNMENT (( #45538 ) ) ;
#18755 = ORIENTED_EDGE ( 'NONE', *, *, #35808, .F. ) ;
#18756 = SURFACE_STYLE_FILL_AREA ( #25079 ) ;
#18757 = CARTESIAN_POINT ( 'NONE',  ( -49.79499999999998039, 2.607480562269068880, -8.024999999999993250 ) ) ;
#18758 = ORIENTED_EDGE ( 'NONE', *, *, #40448, .F. ) ;
#18759 = CARTESIAN_POINT ( 'NONE',  ( 39.49999999999999289, 16.24999999999997513, 3.750000000000000000 ) ) ;
#18760 = CARTESIAN_POINT ( 'NONE',  ( 6.418790567836325955, 2.472216779103306283, -2.882328613363592584 ) ) ;
#18761 = CARTESIAN_POINT ( 'NONE',  ( -85.94292637653380496, 0.000000000000000000, 9.524999999999991473 ) ) ;
#18762 = ADVANCED_FACE ( 'NONE', ( #54498 ), #11592, .T. ) ;
#18763 = DIRECTION ( 'NONE',  ( -0.000000000000000000, 1.000000000000000000, 0.000000000000000000 ) ) ;
#18764 = ORIENTED_EDGE ( 'NONE', *, *, #13406, .F. ) ;
#18765 = CARTESIAN_POINT ( 'NONE',  ( -49.66358509493214513, -12.70625710064021874, 2.845334328481897046 ) ) ;
#18766 = CARTESIAN_POINT ( 'NONE',  ( -54.14499999999999602, -4.716976649647092401, 6.492361379858946790 ) ) ;
#18767 = PRESENTATION_STYLE_ASSIGNMENT (( #50785 ) ) ;
#18768 = ORIENTED_EDGE ( 'NONE', *, *, #22695, .T. ) ;
#18769 = SURFACE_SIDE_STYLE ('',( #4289 ) ) ;
#18770 = CARTESIAN_POINT ( 'NONE',  ( -103.7049999999999983, 2.607480562269073321, 8.024999999999991473 ) ) ;
#18771 = ORIENTED_EDGE ( 'NONE', *, *, #11527, .T. ) ;
#18772 = DIRECTION ( 'NONE',  ( 0.000000000000000000, 0.000000000000000000, 1.000000000000000000 ) ) ;
#18773 = CARTESIAN_POINT ( 'NONE',  ( 0.000000000000000000, 0.000000000000000000, 4.000000000000000000 ) ) ;
#18774 = CARTESIAN_POINT ( 'NONE',  ( -145.4070736234661467, 3.094860106618428031, -9.524999999999993250 ) ) ;
#18775 = DIRECTION ( 'NONE',  ( 1.000000000000000000, 0.000000000000000000, 0.000000000000000000 ) ) ;
#18776 = CARTESIAN_POINT ( 'NONE',  ( -3.094860106618432471, 139.5949999999999420, -9.525000000000000355 ) ) ;
#18777 = CARTESIAN_POINT ( 'NONE',  ( -88.85707362346617799, -5.598654528085803328, -7.705886871421366635 ) ) ;
#18778 =( NAMED_UNIT ( * ) SI_UNIT ( $, .STERADIAN. ) SOLID_ANGLE_UNIT ( ) );
#18779 = FACE_OUTER_BOUND ( 'NONE', #21484, .T. ) ;
#18780 = FILL_AREA_STYLE_COLOUR ( '', #51581 ) ;
#18781 = PRESENTATION_STYLE_ASSIGNMENT (( #23036 ) ) ;
#18782 = CARTESIAN_POINT ( 'NONE',  ( -122.9049999999999727, 2.607480562269068880, -8.024999999999993250 ) ) ;
#18783 = MECHANICAL_DESIGN_GEOMETRIC_PRESENTATION_REPRESENTATION (  '', ( #8695 ), #68261 ) ;
#18784 = CARTESIAN_POINT ( 'NONE',  ( 24.16400019955192136, 24.76135179078163162, -27.27460947215016773 ) ) ;
#18785 = LINE ( 'NONE', #19111, #52314 ) ;
#18786 = CARTESIAN_POINT ( 'NONE',  ( -131.2450000000000045, -4.716976649647093289, -6.492361379858945902 ) ) ;
#18787 = CARTESIAN_POINT ( 'NONE',  ( -116.5450000000000017, -7.632228543268600340, -2.479861379858950166 ) ) ;
#18788 = CARTESIAN_POINT ( 'NONE',  ( 4.041451884327376121, 7.000000000000007105, 7.500000000000000000 ) ) ;
#18789 = EDGE_LOOP ( 'NONE', ( #10920, #27179, #11043, #33829 ) ) ;
#18790 = EDGE_CURVE ( 'NONE', #27898, #68919, #5854, .T. ) ;
#18791 = CARTESIAN_POINT ( 'NONE',  ( -45.50000000000000000, 7.893193270153692431, -6.500000000000000000 ) ) ;
#18792 = CARTESIAN_POINT ( 'NONE',  ( -120.5929263765346064, -3.094860106631942553, -9.524999999990175326 ) ) ;
#18793 = CARTESIAN_POINT ( 'NONE',  ( -170.0929263765338249, 3.094860106618433360, 9.524999999999991473 ) ) ;
#18794 = PRESENTATION_STYLE_ASSIGNMENT (( #8946 ) ) ;
#18795 = CARTESIAN_POINT ( 'NONE',  ( -49.49499999999997613, 6.826472737025113702, -4.959722759717902107 ) ) ;
#18796 = TOROIDAL_SURFACE ( 'NONE', #36822, 0.5000000000000000000, 0.2500000000000000000 ) ;
#18797 = LINE ( 'NONE', #13513, #62404 ) ;
#18798 = DIRECTION ( 'NONE',  ( 0.000000000000000000, -0.000000000000000000, 1.000000000000000000 ) ) ;
#18799 = CARTESIAN_POINT ( 'NONE',  ( -4.750000000000002665, 22.24999999999998579, -4.000000000000000000 ) ) ;
#18800 = ORIENTED_EDGE ( 'NONE', *, *, #26210, .F. ) ;
#18801 = CARTESIAN_POINT ( 'NONE',  ( -89.84292637653381064, 9.058813317711329915, -2.943386871421373119 ) ) ;
#18802 = APPLICATION_PROTOCOL_DEFINITION ( 'draft international standard', 'automotive_design', 1998, #28885 ) ;
#18803 = DIRECTION ( 'NONE',  ( -1.000000000000000000, 0.000000000000000000, 1.300977106640434891E-16 ) ) ;
#18804 = PLANE ( 'NONE',  #68719 ) ;
#18805 = LINE ( 'NONE', #62745, #66269 ) ;
#18806 = SURFACE_STYLE_FILL_AREA ( #8277 ) ;
#18807 = CARTESIAN_POINT ( 'NONE',  ( -78.20707362346617231, 3.094860106618433360, 9.524999999999991473 ) ) ;
#18808 = EDGE_CURVE ( 'NONE', #68902, #64181, #48933, .T. ) ;
#18809 = EDGE_CURVE ( 'NONE', #20280, #25670, #16902, .T. ) ;
#18810 = VERTEX_POINT ( 'NONE', #38382 ) ;
#18811 = CARTESIAN_POINT ( 'NONE',  ( -75.46551724137930250, 63.49197145334878201, -9.500000000000000000 ) ) ;
#18812 =( NAMED_UNIT ( * ) SI_UNIT ( $, .STERADIAN. ) SOLID_ANGLE_UNIT ( ) );
#18813 = VERTEX_POINT ( 'NONE', #64372 ) ;
#18814 = CARTESIAN_POINT ( 'NONE',  ( -7.632228543268607446, 133.6570736234661467, -2.479861379858953718 ) ) ;
#18815 = CARTESIAN_POINT ( 'NONE',  ( 2.607480562269071989, 131.7070736234661865, 8.025000000000002132 ) ) ;
#18816 = EDGE_CURVE ( 'NONE', #1577, #2723, #28080, .T. ) ;
#18817 = EDGE_CURVE ( 'NONE', #55142, #59244, #37695, .T. ) ;
#18818 = COLOUR_RGB ( '', 0.40784314, 0.44705882, 0.49803922) ;
#18819 = DIRECTION ( 'NONE',  ( -1.000000000000000000, 0.000000000000000000, 0.000000000000000000 ) ) ;
#18820 = CARTESIAN_POINT ( 'NONE',  ( 74.54138597727603610, 19.45803563998442343, -6.486986334521338549 ) ) ;
#18821 = DIRECTION ( 'NONE',  ( -1.000000000000000000, 0.000000000000000000, 0.000000000000000000 ) ) ;
#18822 = ORIENTED_EDGE ( 'NONE', *, *, #48508, .T. ) ;
#18823 = DIRECTION ( 'NONE',  ( 0.000000000000000000, -0.9984713486292863260, 0.05527174654752588928 ) ) ;
#18824 = FILL_AREA_STYLE_COLOUR ( '', #7504 ) ;
#18825 = DIRECTION ( 'NONE',  ( 0.000000000000000000, 0.000000000000000000, 1.000000000000000000 ) ) ;
#18826 = ADVANCED_FACE ( 'NONE', ( #32347 ), #427, .T. ) ;
#18827 = CARTESIAN_POINT ( 'NONE',  ( -15.00000000000000000, -12.00000000000000000, 5.000000000000000000 ) ) ;
#18828 = CARTESIAN_POINT ( 'NONE',  ( -85.19500000000000739, 8.437984349512085203, -1.550032578732815448E-15 ) ) ;
#18829 = ORIENTED_EDGE ( 'NONE', *, *, #41490, .F. ) ;
#18830 = CARTESIAN_POINT ( 'NONE',  ( -74.75000000000000000, 4.336808689942018722E-16, 5.000000000000001776 ) ) ;
#18831 = ADVANCED_FACE ( 'NONE', ( #29125 ), #2000, .F. ) ;
#18832 = EDGE_LOOP ( 'NONE', ( #3477, #13904, #10557, #66868 ) ) ;
#18833 =( NAMED_UNIT ( * ) SI_UNIT ( $, .STERADIAN. ) SOLID_ANGLE_UNIT ( ) );
#18834 = SURFACE_STYLE_USAGE ( .BOTH. , #62088 ) ;
#18835 =( NAMED_UNIT ( * ) SI_UNIT ( $, .STERADIAN. ) SOLID_ANGLE_UNIT ( ) );
#18836 = EDGE_LOOP ( 'NONE', ( #32960, #41112, #10940, #47069 ) ) ;
#18837 = DIRECTION ( 'NONE',  ( 1.000000000000000000, 0.000000000000000000, 0.000000000000000000 ) ) ;
#18838 = ORIENTED_EDGE ( 'NONE', *, *, #8749, .T. ) ;
#18839 = CARTESIAN_POINT ( 'NONE',  ( -165.3570736234661922, 5.598654528085804216, 7.705886871421366635 ) ) ;
#18840 = CARTESIAN_POINT ( 'NONE',  ( -5.598654528085808657, 110.6449999999999960, 7.705886871421373741 ) ) ;
#18841 = CARTESIAN_POINT ( 'NONE',  ( -115.2570736234661695, 5.598654528085800663, -7.705886871421367523 ) ) ;
#18842 = FACE_OUTER_BOUND ( 'NONE', #15557, .T. ) ;
#18843 = ORIENTED_EDGE ( 'NONE', *, *, #59212, .F. ) ;
#18844 = CARTESIAN_POINT ( 'NONE',  ( 4.716976649647099507, 122.6429263765338220, -6.492361379858953008 ) ) ;
#18845 = DIRECTION ( 'NONE',  ( -0.000000000000000000, -1.000000000000000000, 0.000000000000000000 ) ) ;
#18846 = DIRECTION ( 'NONE',  ( -1.000000000000000000, 0.000000000000000000, 0.000000000000000000 ) ) ;
#18847 = CARTESIAN_POINT ( 'NONE',  ( -146.6049999999999329, 6.826472737025113702, -4.959722759717902107 ) ) ;
#18848 = SURFACE_STYLE_FILL_AREA ( #4058 ) ;
#18849 = CARTESIAN_POINT ( 'NONE',  ( -162.1449999999999818, -4.716976649647092401, 6.492361379858946790 ) ) ;
#18850 = CARTESIAN_POINT ( 'NONE',  ( -146.9949999999999761, -6.826472737025113702, 4.959722759717902107 ) ) ;
#18851 = ORIENTED_EDGE ( 'NONE', *, *, #19194, .F. ) ;
#18852 =( BOUNDED_CURVE ( )  B_SPLINE_CURVE ( 3, ( #68696, #31731, #20495, #63411 ),
 .UNSPECIFIED., .F., .F. ) 
 B_SPLINE_CURVE_WITH_KNOTS ( ( 4, 4 ),
 ( 1.570796326794891007, 3.141592653589793116 ),
 .UNSPECIFIED. ) 
 CURVE ( )  GEOMETRIC_REPRESENTATION_ITEM ( )  RATIONAL_B_SPLINE_CURVE ( ( 1.000000000000000000, 0.8047378541243637162, 0.8047378541243637162, 1.000000000000000000 ) ) 
 REPRESENTATION_ITEM ( '' )  );
#18853 = EDGE_CURVE ( 'NONE', #15803, #29817, #8743, .T. ) ;
#18854 = CYLINDRICAL_SURFACE ( 'NONE', #34710, 0.2500000000000002220 ) ;
#18855 = DIRECTION ( 'NONE',  ( -1.000000000000000000, -0.000000000000000000, -0.000000000000000000 ) ) ;
#18856 = VECTOR ( 'NONE', #25021, 1000.000000000000000 ) ;
#18857 = DIRECTION ( 'NONE',  ( 0.000000000000000000, 0.000000000000000000, -1.000000000000000000 ) ) ;
#18858 = CARTESIAN_POINT ( 'NONE',  ( -65.30499999999999261, 8.437984349512085203, -1.550032578732815448E-15 ) ) ;
#18859 = DIRECTION ( 'NONE',  ( 1.000000000000000000, 0.000000000000000000, 0.000000000000000000 ) ) ;
#18860 = DIRECTION ( 'NONE',  ( 0.000000000000000000, -1.000000000000000000, 0.000000000000000000 ) ) ;
#18861 = VECTOR ( 'NONE', #50883, 1000.000000000000000 ) ;
#18862 = CARTESIAN_POINT ( 'NONE',  ( -69.89499999999998181, 6.826472737025115478, 4.959722759717899443 ) ) ;
#18863 = CARTESIAN_POINT ( 'NONE',  ( -3.094860106618434248, 144.9050000000000011, 9.525000000000000355 ) ) ;
#18864 = CARTESIAN_POINT ( 'NONE',  ( -1.745454270680676157, 2.292880170256995420, -7.000000000000005329 ) ) ;
#18865 = STYLED_ITEM ( 'NONE', ( #31155 ), #14060 ) ;
#18866 =( NAMED_UNIT ( * ) PLANE_ANGLE_UNIT ( ) SI_UNIT ( $, .RADIAN. ) );
#18867 = CARTESIAN_POINT ( 'NONE',  ( -160.1070736234661922, 8.102448949553172852, -5.886773742842744461 ) ) ;
#18868 = DIRECTION ( 'NONE',  ( 0.000000000000000000, 0.000000000000000000, 1.000000000000000000 ) ) ;
#18869 = EDGE_CURVE ( 'NONE', #2790, #14650, #44692, .T. ) ;
#18870 = CARTESIAN_POINT ( 'NONE',  ( -3.569376287081467591, 110.7040900683961411, 8.618005638702442184 ) ) ;
#18871 =( NAMED_UNIT ( * ) SI_UNIT ( $, .STERADIAN. ) SOLID_ANGLE_UNIT ( ) );
#18872 = EDGE_CURVE ( 'NONE', #9835, #46789, #34432, .T. ) ;
#18873 = DIRECTION ( 'NONE',  ( -0.000000000000000000, -0.000000000000000000, -1.000000000000000000 ) ) ;
#18874 = EDGE_CURVE ( 'NONE', #23615, #34272, #7367, .T. ) ;
#18875 = DIRECTION ( 'NONE',  ( -0.000000000000000000, 1.000000000000000000, -0.000000000000000000 ) ) ;
#18876 = ORIENTED_EDGE ( 'NONE', *, *, #50141, .T. ) ;
#18877 = ORIENTED_EDGE ( 'NONE', *, *, #8838, .F. ) ;
#18878 = PRESENTATION_STYLE_ASSIGNMENT (( #12922 ) ) ;
#18879 = CARTESIAN_POINT ( 'NONE',  ( 0.7093150608672396107, -2.499999999999996003, -7.000000000000007105 ) ) ;
#18880 = ADVANCED_FACE ( 'NONE', ( #61837 ), #45722, .T. ) ;
#18881 = PRESENTATION_LAYER_ASSIGNMENT (  '', '', ( #14434 ) ) ;
#18882 = FACE_OUTER_BOUND ( 'NONE', #49069, .T. ) ;
#18883 = EDGE_CURVE ( 'NONE', #10139, #12300, #24546, .T. ) ;
#18884 = ORIENTED_EDGE ( 'NONE', *, *, #19298, .T. ) ;
#18885 = EDGE_LOOP ( 'NONE', ( #15605, #18001 ) ) ;
#18886 = CYLINDRICAL_SURFACE ( 'NONE', #53410, 0.5000000000000004441 ) ;
#18887 = CARTESIAN_POINT ( 'NONE',  ( 36.00000000000002842, 5.000000000000000000, 77.00402776293825013 ) ) ;
#18888 = ORIENTED_EDGE ( 'NONE', *, *, #41029, .F. ) ;
#18889 =( LENGTH_UNIT ( ) NAMED_UNIT ( * ) SI_UNIT ( .MILLI., .METRE. ) );
#18890 = CARTESIAN_POINT ( 'NONE',  ( -1.445602896647333671E-14, 18.74999999999994671, 3.750000000000000000 ) ) ;
#18891 = ORIENTED_EDGE ( 'NONE', *, *, #48167, .F. ) ;
#18892 = VECTOR ( 'NONE', #67268, 1000.000000000000000 ) ;
#18893 = CARTESIAN_POINT ( 'NONE',  ( -83.15707362346617515, -9.058813317711329915, -2.943386871421370898 ) ) ;
#18894 = CARTESIAN_POINT ( 'NONE',  ( -110.8449999999999847, -7.632228543268599452, 2.479861379858951054 ) ) ;
#18895 = ORIENTED_EDGE ( 'NONE', *, *, #3619, .F. ) ;
#18896 = COLOUR_RGB ( '', 0.08235294, 0.09019608, 0.10196078) ;
#18897 =( NAMED_UNIT ( * ) SI_UNIT ( $, .STERADIAN. ) SOLID_ANGLE_UNIT ( ) );
#18898 = CARTESIAN_POINT ( 'NONE',  ( -10.75761710425530637, -11.70429995583328342, 2.651158507154013577 ) ) ;
#18899 = ORIENTED_EDGE ( 'NONE', *, *, #28439, .F. ) ;
#18900 = CARTESIAN_POINT ( 'NONE',  ( 4.716976649647096842, 145.7429263765338305, 6.492361379858953896 ) ) ;
#18901 = FILL_AREA_STYLE_COLOUR ( '', #67101 ) ;
#18902 = SURFACE_STYLE_FILL_AREA ( #7669 ) ;
#18903 = AXIS2_PLACEMENT_3D ( 'NONE', #50430, #2156, #8572 ) ;
#18904 = CIRCLE ( 'NONE', #7670, 1.000000000000000888 ) ;
#18905 = SURFACE_STYLE_FILL_AREA ( #50946 ) ;
#18906 = EDGE_LOOP ( 'NONE', ( #28676, #21423, #25300 ) ) ;
#18907 = CARTESIAN_POINT ( 'NONE',  ( -20.29261984882471381, 1.607755262496699533, 12.50000000000000000 ) ) ;
#18908 = ORIENTED_EDGE ( 'NONE', *, *, #62361, .F. ) ;
#18909 = CARTESIAN_POINT ( 'NONE',  ( -18.00000000000000711, 31.24999999999999289, 3.750000000000000000 ) ) ;
#18910 = CARTESIAN_POINT ( 'NONE',  ( 32.00000000000001421, 42.00000000000000000, 36.50000000000000000 ) ) ;
#18911 = CARTESIAN_POINT ( 'NONE',  ( 0.000000000000000000, -1.999999999999999556, 0.000000000000000000 ) ) ;
#18913 = CIRCLE ( 'NONE', #25651, 0.5000000000000006661 ) ;
#18912 = DIRECTION ( 'NONE',  ( 0.000000000000000000, 0.000000000000000000, -1.000000000000000000 ) ) ;
#18914 = CARTESIAN_POINT ( 'NONE',  ( -132.8050000000000068, -8.437984349512085203, 5.166775262442717831E-16 ) ) ;
#18915 = DIRECTION ( 'NONE',  ( 1.000000000000000000, 0.000000000000000000, 0.000000000000000000 ) ) ;
#18916 = EDGE_CURVE ( 'NONE', #53591, #31626, #57549, .T. ) ;
#18917 = B_SPLINE_CURVE_WITH_KNOTS ( 'NONE', 3,
 ( #41516, #56973, #45761, #29543, #57315, #51012, #3096, #8459 ),
 .UNSPECIFIED., .F., .F.,
 ( 4, 2, 2, 4 ),
 ( 0.01183260977662614448, 0.01392219916432753390, 0.01496699385817822948, 0.01601178855202892506 ),
 .UNSPECIFIED. ) ;
#18918 = CARTESIAN_POINT ( 'NONE',  ( 36.00000000000002842, 5.000000000000000000, 32.00402776293825724 ) ) ;
#18919 = ORIENTED_EDGE ( 'NONE', *, *, #33928, .F. ) ;
#18920 = CYLINDRICAL_SURFACE ( 'NONE', #6274, 0.5000000000000004441 ) ;
#18921 = STYLED_ITEM ( 'NONE', ( #63573 ), #1027 ) ;
#18922 = CARTESIAN_POINT ( 'NONE',  ( 5.590169943749474513, 0.000000000000000000, 0.000000000000000000 ) ) ;
#18923 = DIRECTION ( 'NONE',  ( 0.000000000000000000, -1.000000000000000000, 0.000000000000000000 ) ) ;
#18924 = ORIENTED_EDGE ( 'NONE', *, *, #381, .F. ) ;
#18925 = ORIENTED_EDGE ( 'NONE', *, *, #17957, .T. ) ;
#18926 = CARTESIAN_POINT ( 'NONE',  ( -20.17806131642189271, 115.4772719928210876, 10.00000000000000178 ) ) ;
#18927 = LINE ( 'NONE', #56581, #15502 ) ;
#18928 = CARTESIAN_POINT ( 'NONE',  ( -51.05499999999999261, -9.827790563157499189E-16, -8.024999999999991473 ) ) ;
#18929 = VERTEX_POINT ( 'NONE', #36201 ) ;
#18930 = CARTESIAN_POINT ( 'NONE',  ( -123.0570736234661808, 0.000000000000000000, 9.524999999999991473 ) ) ;
#18931 = CARTESIAN_POINT ( 'NONE',  ( -182.0049999999999670, 6.826472737025116366, 4.959722759717898555 ) ) ;
#18932 = FACE_OUTER_BOUND ( 'NONE', #52756, .T. ) ;
#18933 = B_SPLINE_CURVE_WITH_KNOTS ( 'NONE', 3,
 ( #40783, #29501, #57271, #3057, #66807, #61488 ),
 .UNSPECIFIED., .F., .F.,
 ( 4, 2, 4 ),
 ( 0.004189585287972436706, 0.006269578072783809838, 0.008349570857595182971 ),
 .UNSPECIFIED. ) ;
#18934 = CARTESIAN_POINT ( 'NONE',  ( -51.95707362346615810, 9.058813317711329915, -2.943386871421373119 ) ) ;
#18935 = PLANE ( 'NONE',  #58800 ) ;
#18936 = DIRECTION ( 'NONE',  ( 0.000000000000000000, 1.000000000000000000, 0.000000000000000000 ) ) ;
#18937 = EDGE_LOOP ( 'NONE', ( #44741, #2687, #54664, #29933 ) ) ;
#18939 = CARTESIAN_POINT ( 'NONE',  ( -74.99999999999998579, 50.00000000000000000, 12.00000000000000000 ) ) ;
#18938 = AXIS2_PLACEMENT_3D ( 'NONE', #33924, #66280, #67326 ) ;
#18940 =( LENGTH_UNIT ( ) NAMED_UNIT ( * ) SI_UNIT ( .MILLI., .METRE. ) );
#18941 = CARTESIAN_POINT ( 'NONE',  ( -100.8549999999999898, 4.716976649647094177, 6.492361379858945902 ) ) ;
#18942 = DIRECTION ( 'NONE',  ( 0.000000000000000000, 1.000000000000000000, 0.000000000000000000 ) ) ;
#18943 = CARTESIAN_POINT ( 'NONE',  ( 22.00000000000000355, 42.00000000000000000, -75.00000000000001421 ) ) ;
#18944 = AXIS2_PLACEMENT_3D ( 'NONE', #50034, #65492, #54589 ) ;
#18945 = CARTESIAN_POINT ( 'NONE',  ( -99.14499999999998181, -4.716976649647092401, 6.492361379858946790 ) ) ;
#18946 = CARTESIAN_POINT ( 'NONE',  ( -1.166476076187854022E-15, 118.0549999999999926, 9.525000000000000355 ) ) ;
#18947 = CARTESIAN_POINT ( 'NONE',  ( -70.94499999999997897, -9.827790563157499189E-16, -8.024999999999991473 ) ) ;
#18948 = AXIS2_PLACEMENT_3D ( 'NONE', #37620, #12191, #60052 ) ;
#18949 = DIRECTION ( 'NONE',  ( 0.000000000000000000, -0.000000000000000000, 1.000000000000000000 ) ) ;
#18950 = SURFACE_STYLE_USAGE ( .BOTH. , #2382 ) ;
#18951 = COLOUR_RGB ( '', 0.31764706, 0.68627451, 0.89019608) ;
#18952 = CARTESIAN_POINT ( 'NONE',  ( 71.99999999999998579, 119.9999999999997868, 9.500000000000000000 ) ) ;
#18953 = DIRECTION ( 'NONE',  ( -1.000000000000000000, -0.000000000000000000, -0.000000000000000000 ) ) ;
#18954 = ORIENTED_EDGE ( 'NONE', *, *, #38156, .F. ) ;
#18955 = EDGE_CURVE ( 'NONE', #54121, #44684, #12645, .T. ) ;
#18956 = CARTESIAN_POINT ( 'NONE',  ( -111.7429263765338163, -5.598654528085803328, -7.705886871421366635 ) ) ;
#18957 = CARTESIAN_POINT ( 'NONE',  ( -139.9449999999999932, -9.827790563157499189E-16, -8.024999999999991473 ) ) ;
#18958 = SURFACE_STYLE_USAGE ( .BOTH. , #41864 ) ;
#18959 = PRESENTATION_LAYER_ASSIGNMENT (  '', '', ( #52689 ) ) ;
#18960 = EDGE_CURVE ( 'NONE', #6374, #8081, #47469, .T. ) ;
#18961 = CYLINDRICAL_SURFACE ( 'NONE', #28020, 113.0000000000000142 ) ;
#18962 = DIRECTION ( 'NONE',  ( -0.000000000000000000, -0.000000000000000000, -1.000000000000000000 ) ) ;
#18963 = VERTEX_POINT ( 'NONE', #68190 ) ;
#18964 = PRESENTATION_LAYER_ASSIGNMENT (  '', '', ( #3164 ) ) ;
#18965 = EDGE_LOOP ( 'NONE', ( #45425, #44569, #17742, #33221 ) ) ;
#18966 = CARTESIAN_POINT ( 'NONE',  ( -62.99292637653378080, 8.102448949553172852, -5.886773742842744461 ) ) ;
#18967 = CARTESIAN_POINT ( 'NONE',  ( 25.75000000000001066, 19.24999999999997868, -3.750000000000000000 ) ) ;
#18968 = DIRECTION ( 'NONE',  ( -1.000000000000000000, -0.000000000000000000, 0.000000000000000000 ) ) ;
#18969 = FILL_AREA_STYLE ('',( #66497 ) ) ;
#18970 = EDGE_CURVE ( 'NONE', #28845, #59451, #29462, .T. ) ;
#18971 = ORIENTED_EDGE ( 'NONE', *, *, #17731, .T. ) ;
#18972 = CARTESIAN_POINT ( 'NONE',  ( -133.1049999999999898, -6.826472737025113702, 4.959722759717902107 ) ) ;
#18973 = ORIENTED_EDGE ( 'NONE', *, *, #3789, .T. ) ;
#18974 =( LENGTH_UNIT ( ) NAMED_UNIT ( * ) SI_UNIT ( .MILLI., .METRE. ) );
#18975 = CARTESIAN_POINT ( 'NONE',  ( -123.2070736234661581, 3.094860106618433360, 9.524999999999991473 ) ) ;
#18976 = ORIENTED_EDGE ( 'NONE', *, *, #33222, .T. ) ;
#18977 = CARTESIAN_POINT ( 'NONE',  ( 57.00000000000000000, 0.000000000000000000, 60.00402776293825724 ) ) ;
#18978 = DIRECTION ( 'NONE',  ( -1.000000000000000000, 0.000000000000000000, 0.000000000000000000 ) ) ;
#18979 = ORIENTED_EDGE ( 'NONE', *, *, #33147, .F. ) ;
#18980 = CARTESIAN_POINT ( 'NONE',  ( 71.50000000000000000, 35.92875272052971525, -7.000000000000000000 ) ) ;
#18981 = SURFACE_SIDE_STYLE ('',( #8800 ) ) ;
#18982 = CARTESIAN_POINT ( 'NONE',  ( 3.094860106618431583, 141.0949999999999989, 9.525000000000000355 ) ) ;
#18983 = SURFACE_SIDE_STYLE ('',( #45775 ) ) ;
#18984 = ORIENTED_EDGE ( 'NONE', *, *, #61694, .F. ) ;
#18985 = SURFACE_STYLE_USAGE ( .BOTH. , #2060 ) ;
#18986 = CARTESIAN_POINT ( 'NONE',  ( -9.058813317711337021, 141.1549999999999727, -2.943386871421374895 ) ) ;
#18987 = CARTESIAN_POINT ( 'NONE',  ( -49.70499999999996987, 2.607480562269072433, 8.024999999999991473 ) ) ;
#18988 = CIRCLE ( 'NONE', #47178, 25.00000000000001421 ) ;
#18989 = ORIENTED_EDGE ( 'NONE', *, *, #21152, .T. ) ;
#18990 = CARTESIAN_POINT ( 'NONE',  ( -7.632228543268608334, 111.8429263765338106, 2.479861379858952830 ) ) ;
#18991 = CARTESIAN_POINT ( 'NONE',  ( 57.00000000000000000, 5.000000000000000000, -60.00402776293825724 ) ) ;
#18992 = CARTESIAN_POINT ( 'NONE',  ( -45.50000000000000000, 9.708372675170618749, -6.000000000000000000 ) ) ;
#18993 = AXIS2_PLACEMENT_3D ( 'NONE', #26551, #48764, #10744 ) ;
#18994 = DIRECTION ( 'NONE',  ( 0.000000000000000000, 1.000000000000000000, 0.000000000000000000 ) ) ;
#18995 = ORIENTED_EDGE ( 'NONE', *, *, #53531, .F. ) ;
#18996 = AXIS2_PLACEMENT_3D ( 'NONE', #69159, #30808, #19904 ) ;
#18997 = CARTESIAN_POINT ( 'NONE',  ( 41.30869453359411381, 107.2693964154586155, 3.464738947915712686 ) ) ;
#18998 = VERTEX_POINT ( 'NONE', #4125 ) ;
#18999 = DIRECTION ( 'NONE',  ( 0.000000000000000000, -0.000000000000000000, -1.000000000000000000 ) ) ;
#19000 = CIRCLE ( 'NONE', #26866, 15.00000000000000000 ) ;
#19001 = CARTESIAN_POINT ( 'NONE',  ( 3.999798566743339556, 49.09558629977726696, 2.000000000000000000 ) ) ;
#19002 = CARTESIAN_POINT ( 'NONE',  ( 48.00000000000000000, 14.49137674618942562, 9.500000000000000000 ) ) ;
#19003 = CARTESIAN_POINT ( 'NONE',  ( -162.8050000000000068, -8.437984349512085203, 5.166775262442717831E-16 ) ) ;
#19004 = ORIENTED_EDGE ( 'NONE', *, *, #40105, .T. ) ;
#19005 = ADVANCED_FACE ( 'NONE', ( #15774 ), #37254, .F. ) ;
#19006 = AXIS2_PLACEMENT_3D ( 'NONE', #32143, #15641, #58528 ) ;
#19007 = CARTESIAN_POINT ( 'NONE',  ( 8.000000000000000000, 5.000000000000000000, -72.00402776293825013 ) ) ;
#19008 = CARTESIAN_POINT ( 'NONE',  ( -57.11974195712091529, -8.499999999999996447, 7.999999999999981348 ) ) ;
#19009 =( NAMED_UNIT ( * ) PLANE_ANGLE_UNIT ( ) SI_UNIT ( $, .RADIAN. ) );
#19010 = ORIENTED_EDGE ( 'NONE', *, *, #27572, .T. ) ;
#19011 = FACE_OUTER_BOUND ( 'NONE', #47572, .T. ) ;
#19012 = ORIENTED_EDGE ( 'NONE', *, *, #52231, .F. ) ;
#19013 = CYLINDRICAL_SURFACE ( 'NONE', #8030, 1.000000000000000000 ) ;
#19014 = CYLINDRICAL_SURFACE ( 'NONE', #14265, 0.5000000000000004441 ) ;
#19015 = CARTESIAN_POINT ( 'NONE',  ( -44.91955507865309727, -12.15949886118714396, 3.183039689081057944 ) ) ;
#19016 = CARTESIAN_POINT ( 'NONE',  ( -80.00500000000000966, 6.826472737025116366, 4.959722759717898555 ) ) ;
#19017 = ORIENTED_EDGE ( 'NONE', *, *, #9517, .T. ) ;
#19018 = SURFACE_STYLE_FILL_AREA ( #40179 ) ;
#19019 =( GEOMETRIC_REPRESENTATION_CONTEXT ( 3 ) GLOBAL_UNCERTAINTY_ASSIGNED_CONTEXT ( ( #5257 ) ) GLOBAL_UNIT_ASSIGNED_CONTEXT ( ( #33574, #55732, #55011 ) ) REPRESENTATION_CONTEXT ( 'NONE', 'WORKASPACE' ) );
#19020 = CARTESIAN_POINT ( 'NONE',  ( -151.5570736234661808, -1.166476076187852838E-15, -9.524999999999991473 ) ) ;
#19021 =( REPRESENTATION_RELATIONSHIP ('NONE','NONE', #5102, #21315 ) REPRESENTATION_RELATIONSHIP_WITH_TRANSFORMATION ( #67343 )SHAPE_REPRESENTATION_RELATIONSHIP( ) );
#19022 = CARTESIAN_POINT ( 'NONE',  ( -75.00000000000000000, 8.706976341191499102, -5.725845108612586998 ) ) ;
#19023 = EDGE_LOOP ( 'NONE', ( #65383, #63571, #24588, #65047 ) ) ;
#19024 = FILL_AREA_STYLE ('',( #35589 ) ) ;
#19026 = DIRECTION ( 'NONE',  ( -0.000000000000000000, -1.000000000000000000, -0.000000000000000000 ) ) ;
#19025 = CARTESIAN_POINT ( 'NONE',  ( 28.00000000000000000, 38.70020753820971748, -89.00000000000000000 ) ) ;
#19027 = CARTESIAN_POINT ( 'NONE',  ( 0.000000000000000000, 139.4449999999999932, -9.525000000000000355 ) ) ;
#19028 = CARTESIAN_POINT ( 'NONE',  ( -108.4449999999999790, 0.000000000000000000, 8.024999999999991473 ) ) ;
#19029 = EDGE_CURVE ( 'NONE', #10674, #29467, #2692, .T. ) ;
#19030 = FILL_AREA_STYLE ('',( #57036 ) ) ;
#19031 = SURFACE_STYLE_USAGE ( .BOTH. , #6757 ) ;
#19032 = STYLED_ITEM ( 'NONE', ( #34337 ), #1136 ) ;
#19033 = CIRCLE ( 'NONE', #57206, 0.5000000000000003331 ) ;
#19035 = DIRECTION ( 'NONE',  ( -0.000000000000000000, -1.000000000000000000, -0.000000000000000000 ) ) ;
#19034 = FACE_BOUND ( 'NONE', #14427, .T. ) ;
#19036 = AXIS2_PLACEMENT_3D ( 'NONE', #59110, #53503, #15543 ) ;
#19037 = CARTESIAN_POINT ( 'NONE',  ( -140.5429263765338135, 9.058813317711329915, 2.943386871421369566 ) ) ;
#19038 = CARTESIAN_POINT ( 'NONE',  ( -166.3449999999999989, 7.632228543268599452, -2.479861379858951942 ) ) ;
#19039 = COLOUR_RGB ( '', 0.40784314, 0.44705882, 0.49803922) ;
#19040 = EDGE_CURVE ( 'NONE', #2945, #62845, #7029, .T. ) ;
#19041 = DIRECTION ( 'NONE',  ( -0.000000000000000000, 1.000000000000000000, -0.000000000000000000 ) ) ;
#19042 = AXIS2_PLACEMENT_3D ( 'NONE', #43369, #65451, #28122 ) ;
#19043 = FACE_OUTER_BOUND ( 'NONE', #33859, .T. ) ;
#19044 = ORIENTED_EDGE ( 'NONE', *, *, #16794, .T. ) ;
#19045 = CARTESIAN_POINT ( 'NONE',  ( -17.75000000000000711, 30.99999999999999289, 4.000000000000000000 ) ) ;
#19046 = ORIENTED_EDGE ( 'NONE', *, *, #44618, .T. ) ;
#19047 = EDGE_CURVE ( 'NONE', #37864, #9427, #29523, .T. ) ;
#19048 = FILL_AREA_STYLE_COLOUR ( '', #33022 ) ;
#19049 =( BOUNDED_CURVE ( )  B_SPLINE_CURVE ( 2, ( #7540, #795, #60994, #1152, #65239, #22689, #17092, #28969, #12813, #6480, #27919 ),
 .UNSPECIFIED., .F., .F. ) 
 B_SPLINE_CURVE_WITH_KNOTS ( ( 3, 2, 2, 2, 2, 3 ),
 ( 0.2717391304347761549, 0.2739130434782543477, 0.2760869565217325960, 0.2782608695652108444, 0.2804347826086890372, 0.2826086956521672300 ),
 .UNSPECIFIED. ) 
 CURVE ( )  GEOMETRIC_REPRESENTATION_ITEM ( )  RATIONAL_B_SPLINE_CURVE ( ( 1.000000000000144995, 0.9510565162950085361, 1.000000000000000000, 0.9510565162951535312, 1.000000000000000000, 0.9510565162951535312, 1.000000000000000000, 0.9510565162951535312, 1.000000000000000000, 0.9510565162953035223, 0.9999999999998500089 ) ) 
 REPRESENTATION_ITEM ( '' )  );
#19050 = ADVANCED_FACE ( 'NONE', ( #63249 ), #57597, .F. ) ;
#19051 = CIRCLE ( 'NONE', #34785, 14.49999999999999822 ) ;
#19052 = CARTESIAN_POINT ( 'NONE',  ( -9.827790563157511022E-16, 118.4429263765338192, 8.025000000000000355 ) ) ;
#19053 = CARTESIAN_POINT ( 'NONE',  ( -111.0570736234661808, 0.000000000000000000, 9.524999999999991473 ) ) ;
#19054 = AXIS2_PLACEMENT_3D ( 'NONE', #15804, #47501, #63623 ) ;
#19055 = DIRECTION ( 'NONE',  ( 0.000000000000000000, 0.000000000000000000, -1.000000000000000000 ) ) ;
#19056 = EDGE_CURVE ( 'NONE', #13795, #10407, #22751, .T. ) ;
#19057 = EDGE_LOOP ( 'NONE', ( #25761, #14412, #104, #38411 ) ) ;
#19058 = CARTESIAN_POINT ( 'NONE',  ( -162.6550000000000011, -7.632228543268600340, -2.479861379858950166 ) ) ;
#19059 = ORIENTED_EDGE ( 'NONE', *, *, #31288, .T. ) ;
#19060 = PRESENTATION_STYLE_ASSIGNMENT (( #45523 ) ) ;
#19061 = DIRECTION ( 'NONE',  ( -0.000000000000000000, 1.000000000000000000, -0.000000000000000000 ) ) ;
#19062 = ORIENTED_EDGE ( 'NONE', *, *, #1085, .T. ) ;
#19063 = B_SPLINE_CURVE_WITH_KNOTS ( 'NONE', 3,
 ( #68653, #63007, #25377, #57750, #63363, #42640 ),
 .UNSPECIFIED., .F., .F.,
 ( 4, 2, 4 ),
 ( -1.190210691535116941E-05, 0.001159215856766632581, 0.002330333820448616568 ),
 .UNSPECIFIED. ) ;
#19064 = AXIS2_PLACEMENT_3D ( 'NONE', #57384, #14836, #45816 ) ;
#19065 = DIRECTION ( 'NONE',  ( -0.000000000000000000, -0.000000000000000000, -1.000000000000000000 ) ) ;
#19066 = CARTESIAN_POINT ( 'NONE',  ( 7.632228543268608334, 159.4570736234661581, -2.479861379858951942 ) ) ;
#19067 = CONICAL_SURFACE ( 'NONE', #49438, 3.499999999999997780, 0.7853981633974452814 ) ;
#19068 = ORIENTED_EDGE ( 'NONE', *, *, #10415, .T. ) ;
#19069 = DIRECTION ( 'NONE',  ( 0.000000000000000000, 0.000000000000000000, 1.000000000000000000 ) ) ;
#19070 = CARTESIAN_POINT ( 'NONE',  ( -10.01517768586949408, 114.3049999999999926, -6.132527647946036459E-16 ) ) ;
#19071 = CARTESIAN_POINT ( 'NONE',  ( -75.65499999999998693, -7.632228543268600340, -2.479861379858950166 ) ) ;
#19072 = DIRECTION ( 'NONE',  ( -1.000000000000000000, 0.000000000000000000, 0.000000000000000000 ) ) ;
#19073 = ORIENTED_EDGE ( 'NONE', *, *, #11431, .F. ) ;
#19074 = CARTESIAN_POINT ( 'NONE',  ( 8.102448949553183510, 143.1049999999999329, -5.886773742842746238 ) ) ;
#19075 = AXIS2_PLACEMENT_3D ( 'NONE', #13327, #2014, #66459 ) ;
#19076 = PLANE ( 'NONE',  #8563 ) ;
#19077 = PRESENTATION_STYLE_ASSIGNMENT (( #13461 ) ) ;
#19078 = CARTESIAN_POINT ( 'NONE',  ( -41.49999999999997868, 10.49999999999998046, -3.000000000000000000 ) ) ;
#19079 = CYLINDRICAL_SURFACE ( 'NONE', #12633, 10.00000000000000000 ) ;
#19080 = ORIENTED_EDGE ( 'NONE', *, *, #30641, .T. ) ;
#19081 = DIRECTION ( 'NONE',  ( -0.000000000000000000, -0.000000000000000000, -1.000000000000000000 ) ) ;
#19082 = CARTESIAN_POINT ( 'NONE',  ( 60.00000000000000000, 1.797044900979284448E-15, -10.00000000000000000 ) ) ;
#19084 = CARTESIAN_POINT ( 'NONE',  ( -48.89499999999999602, 6.826472737025116366, 4.959722759717898555 ) ) ;
#19083 = STYLED_ITEM ( 'NONE', ( #28792 ), #59292 ) ;
#19085 = VERTEX_POINT ( 'NONE', #46418 ) ;
#19086 = LINE ( 'NONE', #40238, #19967 ) ;
#19087 = CARTESIAN_POINT ( 'NONE',  ( -44.99999999999999289, 7.768687147774684831, -6.500000000000010658 ) ) ;
#19088 = PRESENTATION_LAYER_ASSIGNMENT (  '', '', ( #39373 ) ) ;
#19089 = DIRECTION ( 'NONE',  ( 0.000000000000000000, 0.000000000000000000, 1.000000000000000000 ) ) ;
#19090 = VERTEX_POINT ( 'NONE', #67843 ) ;
#19091 = CARTESIAN_POINT ( 'NONE',  ( -55.49499999999999034, 6.826472737025113702, -4.959722759717902107 ) ) ;
#19092 = DIRECTION ( 'NONE',  ( -1.000000000000000000, 0.000000000000000000, 0.000000000000000000 ) ) ;
#19093 = ORIENTED_EDGE ( 'NONE', *, *, #60685, .T. ) ;
#19094 = PLANE ( 'NONE',  #51611 ) ;
#19095 = CARTESIAN_POINT ( 'NONE',  ( -101.7549999999999812, 4.716976649647091513, -6.492361379858946790 ) ) ;
#19096 = ORIENTED_EDGE ( 'NONE', *, *, #13683, .T. ) ;
#19097 = FACE_OUTER_BOUND ( 'NONE', #40957, .T. ) ;
#19098 = PRESENTATION_LAYER_ASSIGNMENT (  '', '', ( #28063 ) ) ;
#19099 = DIRECTION ( 'NONE',  ( 0.000000000000000000, 0.000000000000000000, -1.000000000000000000 ) ) ;
#19100 = CIRCLE ( 'NONE', #58435, 0.5000000000000004441 ) ;
#19101 = CARTESIAN_POINT ( 'NONE',  ( -140.9070736234661183, -3.094860106618429807, 9.524999999999991473 ) ) ;
#19102 = CARTESIAN_POINT ( 'NONE',  ( 5.598654528085809545, 142.1449999999999818, -7.705886871421373741 ) ) ;
#19103 = CARTESIAN_POINT ( 'NONE',  ( -79.10707362346616378, 8.102448949553171076, -5.886773742842744461 ) ) ;
#19104 = AXIS2_PLACEMENT_3D ( 'NONE', #15222, #41958, #28027 ) ;
#19105 = CARTESIAN_POINT ( 'NONE',  ( 30.50000000000001066, 16.24999999999997513, -3.750000000000000000 ) ) ;
#19106 =( LENGTH_UNIT ( ) NAMED_UNIT ( * ) SI_UNIT ( .MILLI., .METRE. ) );
#19107 = AXIS2_PLACEMENT_3D ( 'NONE', #23067, #18127, #49797 ) ;
#19108 = LINE ( 'NONE', #7876, #28997 ) ;
#19109 = CARTESIAN_POINT ( 'NONE',  ( -116.7549999999999812, 4.716976649647091513, -6.492361379858946790 ) ) ;
#19110 = CARTESIAN_POINT ( 'NONE',  ( 24.50574400633172090, 25.15110077572983371, -27.39850243389338402 ) ) ;
#19111 = CARTESIAN_POINT ( 'NONE',  ( 20.71231517720798010, 146.9999999999999716, -7.500000000000000000 ) ) ;
#19112 = CARTESIAN_POINT ( 'NONE',  ( -139.3449999999999989, 7.632228543268599452, -2.479861379858951942 ) ) ;
#19113 = PRESENTATION_LAYER_ASSIGNMENT (  '', '', ( #68557 ) ) ;
#19114 = EDGE_CURVE ( 'NONE', #31521, #330, #19638, .T. ) ;
#19115 = STYLED_ITEM ( 'NONE', ( #58010 ), #15619 ) ;
#19116 = CARTESIAN_POINT ( 'NONE',  ( -123.8949999999999818, 6.826472737025115478, 4.959722759717899443 ) ) ;
#19117 = CARTESIAN_POINT ( 'NONE',  ( -45.50000000000000000, 9.708372675170618749, -6.500000000000000000 ) ) ;
#19118 = ORIENTED_EDGE ( 'NONE', *, *, #59734, .T. ) ;
#19119 = TOROIDAL_SURFACE ( 'NONE', #59597, 22.50000000000000000, 0.5000000000000000000 ) ;
#19120 = ADVANCED_FACE ( 'NONE', ( #30517, #62879 ), #53716, .F. ) ;
#19121 = DIRECTION ( 'NONE',  ( 0.000000000000000000, -0.000000000000000000, -1.000000000000000000 ) ) ;
#19122 = MECHANICAL_DESIGN_GEOMETRIC_PRESENTATION_REPRESENTATION (  '', ( #43888 ), #61786 ) ;
#19123 = ADVANCED_FACE ( 'NONE', ( #21357 ), #66585, .F. ) ;
#19124 = CARTESIAN_POINT ( 'NONE',  ( -121.3429263765338106, -9.058813317711329915, 2.943386871421371787 ) ) ;
#19125 = CARTESIAN_POINT ( 'NONE',  ( -168.7429263765338305, -5.598654528085803328, -7.705886871421366635 ) ) ;
#19126 = VECTOR ( 'NONE', #13239, 1000.000000000000000 ) ;
#19127 = CARTESIAN_POINT ( 'NONE',  ( 30.99999999999998579, 5.000000000000000000, -72.00402776293822171 ) ) ;
#19128 = EDGE_CURVE ( 'NONE', #25427, #2048, #5506, .T. ) ;
#19129 = EDGE_CURVE ( 'NONE', #39359, #68708, #35089, .T. ) ;
#19130 = EDGE_CURVE ( 'NONE', #11319, #56584, #9956, .T. ) ;
#19131 = CARTESIAN_POINT ( 'NONE',  ( -18.25000000000000711, 33.74999999999999289, -3.750000000000000000 ) ) ;
#19132 = PLANE ( 'NONE',  #29354 ) ;
#19133 = ORIENTED_EDGE ( 'NONE', *, *, #25182, .T. ) ;
#19134 = AXIS2_PLACEMENT_3D ( 'NONE', #58652, #7190, #56613 ) ;
#19135 = PRODUCT_DEFINITION_CONTEXT ( 'detailed design', #15477, 'design' ) ;
#19136 = EDGE_CURVE ( 'NONE', #4855, #3314, #60936, .T. ) ;
#19137 = CARTESIAN_POINT ( 'NONE',  ( -89.99292637653380211, 8.102448949553171076, -5.886773742842744461 ) ) ;
#19138 = CARTESIAN_POINT ( 'NONE',  ( -53.60138881051016568, -9.947368421052624754, -2.000000000000000000 ) ) ;
#19139 = DIRECTION ( 'NONE',  ( -0.000000000000000000, -0.000000000000000000, -1.000000000000000000 ) ) ;
#19140 = EDGE_CURVE ( 'NONE', #12632, #42104, #7656, .T. ) ;
#19141 = CIRCLE ( 'NONE', #58483, 4.999999999999997335 ) ;
#19143 = FILL_AREA_STYLE_COLOUR ( '', #12417 ) ;
#19142 =( BOUNDED_SURFACE ( )  B_SPLINE_SURFACE ( 3, 2, ( 
 ( #13326, #12279, #39076 ),
 ( #2743, #61181, #60471 ),
 ( #23538, #50981, #18633 ),
 ( #66458, #8429, #8064 ),
 ( #28810, #55560, #23892 ),
 ( #29517, #24238, #39766 ) ),
 .UNSPECIFIED., .F., .F., .F. ) 
 B_SPLINE_SURFACE_WITH_KNOTS ( ( 4, 2, 4 ),
 ( 3, 3 ),
 ( 0.000000000000000000, 0.001858233469841190193, 0.003716466939682380385 ),
 ( 0.000000000000000000, 1.000000000000000000 ),
 .UNSPECIFIED. ) 
 GEOMETRIC_REPRESENTATION_ITEM ( )  RATIONAL_B_SPLINE_SURFACE ( (
 ( 1.000000000000000000, 0.7071067811865475727, 1.000000000000000000),
 ( 1.000000000000000000, 0.7208066020895490533, 1.000000000000000000),
 ( 1.000000000000000000, 0.7349590933757870204, 1.000000000000000000),
 ( 1.000000000000000000, 0.7642326935828396284, 1.000000000000000000),
 ( 1.000000000000000000, 0.7794396215065395594, 1.000000000000000000),
 ( 1.000000000000000000, 0.7942671885213410388, 1.000000000000000000) ) ) 
 REPRESENTATION_ITEM ( '' )  SURFACE ( )  );
#19144 = CARTESIAN_POINT ( 'NONE',  ( -162.7429263765338021, -5.598654528085803328, -7.705886871421366635 ) ) ;
#19145 = DIRECTION ( 'NONE',  ( 0.000000000000000000, 0.000000000000000000, -1.000000000000000000 ) ) ;
#19146 = ORIENTED_EDGE ( 'NONE', *, *, #25197, .T. ) ;
#19147 = CARTESIAN_POINT ( 'NONE',  ( -136.6429263765338078, -5.598654528085801552, 7.705886871421367523 ) ) ;
#19148 = DIRECTION ( 'NONE',  ( -0.000000000000000000, -0.000000000000000000, -1.000000000000000000 ) ) ;
#19149 = DIRECTION ( 'NONE',  ( 0.000000000000000000, 0.000000000000000000, -1.000000000000000000 ) ) ;
#19150 = COLOUR_RGB ( '', 0.09019608, 0.27058824, 0.51372549) ;
#19151 = VERTEX_POINT ( 'NONE', #54741 ) ;
#19152 = CARTESIAN_POINT ( 'NONE',  ( -64.94292637653380496, 0.000000000000000000, 9.524999999999991473 ) ) ;
#19153 = COLOUR_RGB ( '', 0.09019608, 0.27058824, 0.51372549) ;
#19154 = CARTESIAN_POINT ( 'NONE',  ( 4.716976649647096842, 137.8570736234661638, 6.492361379858953896 ) ) ;
#19155 = AXIS2_PLACEMENT_3D ( 'NONE', #12386, #16677, #27522 ) ;
#19156 = ORIENTED_EDGE ( 'NONE', *, *, #59554, .F. ) ;
#19157 = CARTESIAN_POINT ( 'NONE',  ( -70.75000000000000000, -4.000000000000000000, 24.00000000000000000 ) ) ;
#19158 = DIRECTION ( 'NONE',  ( 0.000000000000000000, -1.000000000000000000, 0.000000000000000000 ) ) ;
#19159 = TOROIDAL_SURFACE ( 'NONE', #7924, 1.000000000000000000, 0.5000000000000000000 ) ;
#19160 = DIRECTION ( 'NONE',  ( 0.000000000000000000, 1.000000000000000000, 0.000000000000000000 ) ) ;
#19161 = ORIENTED_EDGE ( 'NONE', *, *, #38326, .T. ) ;
#19162 = CARTESIAN_POINT ( 'NONE',  ( -94.19292637653380496, -10.01517768586948698, 6.132527647946031529E-16 ) ) ;
#19163 = DIRECTION ( 'NONE',  ( 1.000000000000000000, -0.000000000000000000, -0.000000000000000000 ) ) ;
#19164 = STYLED_ITEM ( 'NONE', ( #54833 ), #17719 ) ;
#19165 = CARTESIAN_POINT ( 'NONE',  ( -86.09499999999997044, -2.607480562269071545, -8.024999999999991473 ) ) ;
#19166 = VERTEX_POINT ( 'NONE', #33318 ) ;
#19167 = EDGE_CURVE ( 'NONE', #40156, #18929, #51984, .T. ) ;
#19168 = AXIS2_PLACEMENT_3D ( 'NONE', #20626, #18300, #39783 ) ;
#19169 = UNCERTAINTY_MEASURE_WITH_UNIT (LENGTH_MEASURE( 1.000000000000000082E-05 ), #18171, 'distance_accuracy_value', 'NONE');
#19170 = EDGE_LOOP ( 'NONE', ( #58076, #377, #53853, #47878 ) ) ;
#19171 = FACE_OUTER_BOUND ( 'NONE', #12014, .T. ) ;
#19172 =( GEOMETRIC_REPRESENTATION_CONTEXT ( 3 ) GLOBAL_UNCERTAINTY_ASSIGNED_CONTEXT ( ( #45319 ) ) GLOBAL_UNIT_ASSIGNED_CONTEXT ( ( #61008, #34291, #7894 ) ) REPRESENTATION_CONTEXT ( 'NONE', 'WORKASPACE' ) );
#19173 =( LENGTH_UNIT ( ) NAMED_UNIT ( * ) SI_UNIT ( .MILLI., .METRE. ) );
#19174 = CARTESIAN_POINT ( 'NONE',  ( -23.21231517720797655, 118.4999999999999716, -7.000000000000000000 ) ) ;
#19175 = ORIENTED_EDGE ( 'NONE', *, *, #22794, .T. ) ;
#19176 = ORIENTED_EDGE ( 'NONE', *, *, #19704, .T. ) ;
#19177 = CARTESIAN_POINT ( 'NONE',  ( -68.49999999999998579, -1.919947267060472329E-14, 10.50000000000000000 ) ) ;
#19178 = SURFACE_STYLE_USAGE ( .BOTH. , #51221 ) ;
#19179 =( NAMED_UNIT ( * ) SI_UNIT ( $, .STERADIAN. ) SOLID_ANGLE_UNIT ( ) );
#19180 = CARTESIAN_POINT ( 'NONE',  ( -169.7070736234661581, -3.094860106618431139, -9.524999999999991473 ) ) ;
#19181 = COLOUR_RGB ( '', 0.31764706, 0.68627451, 0.89019608) ;
#19182 = FACE_OUTER_BOUND ( 'NONE', #51383, .T. ) ;
#19183 = CARTESIAN_POINT ( 'NONE',  ( 0.000000000000000000, 112.4449999999999932, -9.525000000000000355 ) ) ;
#19184 = CARTESIAN_POINT ( 'NONE',  ( -115.8570736234661780, -5.598654528085803328, -7.705886871421366635 ) ) ;
#19185 = CIRCLE ( 'NONE', #6852, 7.249999999999999112 ) ;
#19186 = COLOUR_RGB ( '', 0.66274510, 0.83137255, 0.94901961) ;
#19187 = ORIENTED_EDGE ( 'NONE', *, *, #63167, .T. ) ;
#19188 = DIRECTION ( 'NONE',  ( 1.000000000000000000, -0.000000000000000000, -1.300977106640434891E-16 ) ) ;
#19189 = CARTESIAN_POINT ( 'NONE',  ( -9.000000000000003553, 25.24999999999998934, -3.750000000000000000 ) ) ;
#19191 = AXIS2_PLACEMENT_3D ( 'NONE', #47859, #53426, #15463 ) ;
#19190 = FACE_OUTER_BOUND ( 'NONE', #25322, .T. ) ;
#19192 = CYLINDRICAL_SURFACE ( 'NONE', #61299, 5.000000000000004441 ) ;
#19193 = CARTESIAN_POINT ( 'NONE',  ( -150.5049999999999955, -6.826472737025115478, -4.959722759717899443 ) ) ;
#19194 = EDGE_CURVE ( 'NONE', #53011, #24720, #8328, .T. ) ;
#19195 = FACE_OUTER_BOUND ( 'NONE', #5385, .T. ) ;
#19196 = CARTESIAN_POINT ( 'NONE',  ( -7.398177350229779847, 111.8698371976141743, 3.525222019987722000 ) ) ;
#19197 = VECTOR ( 'NONE', #13355, 1000.000000000000000 ) ;
#19198 = CARTESIAN_POINT ( 'NONE',  ( -165.5949999999999704, 2.607480562269073321, 8.024999999999991473 ) ) ;
#19199 = CARTESIAN_POINT ( 'NONE',  ( -149.0949999999999704, -2.607480562269071545, -8.024999999999991473 ) ) ;
#19200 = ORIENTED_EDGE ( 'NONE', *, *, #3539, .T. ) ;
#19201 = EDGE_CURVE ( 'NONE', #48456, #37266, #5905, .T. ) ;
#19202 = COLOUR_RGB ( '', 0.31764706, 0.68627451, 0.89019608) ;
#19203 = DIRECTION ( 'NONE',  ( 0.000000000000000000, 0.000000000000000000, -1.000000000000000000 ) ) ;
#19204 = CARTESIAN_POINT ( 'NONE',  ( 9.568252947146927312, -1.861307952554195566, -1.427299755870872433 ) ) ;
#19205 = CARTESIAN_POINT ( 'NONE',  ( -64.10499999999997556, -6.826472737025115478, 4.959722759717900331 ) ) ;
#19206 = CARTESIAN_POINT ( 'NONE',  ( 48.74999999999999289, 24.74999999999998579, 4.000000000000000000 ) ) ;
#19207 = CIRCLE ( 'NONE', #14724, 0.5000000000000004441 ) ;
#19208 = CARTESIAN_POINT ( 'NONE',  ( 13.75000000000000533, 30.99999999999999289, -3.750000000000000000 ) ) ;
#19209 = CARTESIAN_POINT ( 'NONE',  ( -64.79499999999998749, 2.607480562269069324, -8.024999999999993250 ) ) ;
#19210 = CARTESIAN_POINT ( 'NONE',  ( 5.598654528085805993, 154.3549999999999898, 7.705886871421374629 ) ) ;
#19211 =( NAMED_UNIT ( * ) SI_UNIT ( $, .STERADIAN. ) SOLID_ANGLE_UNIT ( ) );
#19212 = MECHANICAL_DESIGN_GEOMETRIC_PRESENTATION_REPRESENTATION (  '', ( #10263 ), #37262 ) ;
#19213 = EDGE_CURVE ( 'NONE', #10613, #7095, #36490, .T. ) ;
#19214 = UNCERTAINTY_MEASURE_WITH_UNIT (LENGTH_MEASURE( 1.000000000000000082E-05 ), #26735, 'distance_accuracy_value', 'NONE');
#19215 = COLOUR_RGB ( '', 0.08235294, 0.09019608, 0.10196078) ;
#19216 = CARTESIAN_POINT ( 'NONE',  ( 0.000000000000000000, 42.00000000000000000, -44.99999999999999289 ) ) ;
#19217 = EDGE_CURVE ( 'NONE', #12224, #56168, #62110, .T. ) ;
#19218 = COLOUR_RGB ( '', 0.08235294, 0.09019608, 0.10196078) ;
#19219 = CARTESIAN_POINT ( 'NONE',  ( 0.000000000000000000, 2.500000000000000000, 9.000000000000001776 ) ) ;
#19220 = CYLINDRICAL_SURFACE ( 'NONE', #37247, 0.5000000000000004441 ) ;
#19221 = DIRECTION ( 'NONE',  ( -0.000000000000000000, -1.000000000000000000, -0.000000000000000000 ) ) ;
#19222 = ORIENTED_EDGE ( 'NONE', *, *, #30072, .T. ) ;
#19223 = ORIENTED_EDGE ( 'NONE', *, *, #43529, .T. ) ;
#19224 = CARTESIAN_POINT ( 'NONE',  ( -61.55707362346617373, -1.166476076187852838E-15, -9.524999999999991473 ) ) ;
#19225 = CIRCLE ( 'NONE', #31595, 7.000000000000001776 ) ;
#19226 = B_SPLINE_CURVE_WITH_KNOTS ( 'NONE', 3,
 ( #10518, #22098, #26652, #33002, #32295, #64671, #38316, #36929 ),
 .UNSPECIFIED., .F., .F.,
 ( 4, 2, 2, 4 ),
 ( 2.544316211735810720E-07, 0.002094919859796807744, 0.003142252573884624176, 0.004189585287972440175 ),
 .UNSPECIFIED. ) ;
#19227 = CARTESIAN_POINT ( 'NONE',  ( 0.000000000000000000, 0.000000000000000000, 0.000000000000000000 ) ) ;
#19228 = VECTOR ( 'NONE', #34827, 1000.000000000000000 ) ;
#19229 = AXIS2_PLACEMENT_3D ( 'NONE', #64652, #22423, #38655 ) ;
#19230 = CARTESIAN_POINT ( 'NONE',  ( 22.00000000000002132, 42.47058823529412308, 74.11764705882352189 ) ) ;
#19231 =( NAMED_UNIT ( * ) SI_UNIT ( $, .STERADIAN. ) SOLID_ANGLE_UNIT ( ) );
#19232 = ORIENTED_EDGE ( 'NONE', *, *, #19290, .T. ) ;
#19233 = VERTEX_POINT ( 'NONE', #13935 ) ;
#19234 = CARTESIAN_POINT ( 'NONE',  ( -195.0000000000000000, 6.735557395310425260E-16, -5.499999999999985789 ) ) ;
#19235 = SURFACE_STYLE_FILL_AREA ( #9419 ) ;
#19236 = VERTEX_POINT ( 'NONE', #13224 ) ;
#19237 = CARTESIAN_POINT ( 'NONE',  ( -65.84292637653379643, 9.058813317711329915, -2.943386871421373119 ) ) ;
#19238 = CARTESIAN_POINT ( 'NONE',  ( -145.4929263765338021, -8.102448949553174629, 5.886773742842742685 ) ) ;
#19239 = VERTEX_POINT ( 'NONE', #24466 ) ;
#19240 = FILL_AREA_STYLE_COLOUR ( '', #16445 ) ;
#19241 = AXIS2_PLACEMENT_3D ( 'NONE', #49464, #6881, #28306 ) ;
#19242 = DIRECTION ( 'NONE',  ( 0.000000000000000000, 0.000000000000000000, 1.000000000000000000 ) ) ;
#19243 = CARTESIAN_POINT ( 'NONE',  ( -110.2449999999999903, -4.716976649647093289, -6.492361379858945902 ) ) ;
#19244 = EDGE_LOOP ( 'NONE', ( #49834, #19456, #51765, #29443 ) ) ;
#19245 = EDGE_CURVE ( 'NONE', #47861, #1828, #50881, .T. ) ;
#19246 = AXIS2_PLACEMENT_3D ( 'NONE', #12484, #38933, #49801 ) ;
#19247 =( NAMED_UNIT ( * ) PLANE_ANGLE_UNIT ( ) SI_UNIT ( $, .RADIAN. ) );
#19248 = FILL_AREA_STYLE ('',( #29095 ) ) ;
#19249 = CARTESIAN_POINT ( 'NONE',  ( -179.3070736234661524, -10.01517768586948698, 6.132527647946031529E-16 ) ) ;
#19250 = VERTEX_POINT ( 'NONE', #39655 ) ;
#19251 = CARTESIAN_POINT ( 'NONE',  ( 7.632228543268607446, 143.0429263765338135, 2.479861379858954606 ) ) ;
#19252 = DIRECTION ( 'NONE',  ( -0.07898106964430656740, -0.9968761159932768567, 0.000000000000000000 ) ) ;
#19253 = FACE_OUTER_BOUND ( 'NONE', #44944, .T. ) ;
#19254 = COLOUR_RGB ( '', 0.31764706, 0.68627451, 0.89019608) ;
#19255 = CARTESIAN_POINT ( 'NONE',  ( 2.000000000000008882, 26.00000000000000355, -24.00000000000000355 ) ) ;
#19256 = ORIENTED_EDGE ( 'NONE', *, *, #39187, .T. ) ;
#19257 = AXIS2_PLACEMENT_3D ( 'NONE', #14120, #3145, #35579 ) ;
#19258 =( NAMED_UNIT ( * ) SI_UNIT ( $, .STERADIAN. ) SOLID_ANGLE_UNIT ( ) );
#19259 = VERTEX_POINT ( 'NONE', #56137 ) ;
#19260 = DIRECTION ( 'NONE',  ( 1.000000000000000000, 0.000000000000000000, 0.000000000000000000 ) ) ;
#19261 = CARTESIAN_POINT ( 'NONE',  ( -60.00000000000000000, -2.024042244987997205E-14, -9.500000000000000000 ) ) ;
#19262 = CARTESIAN_POINT ( 'NONE',  ( 41.49999999999998579, 106.9282032302754999, -3.500000000000000000 ) ) ;
#19263 = CARTESIAN_POINT ( 'NONE',  ( -126.5049999999999528, -6.826472737025115478, -4.959722759717899443 ) ) ;
#19264 = LINE ( 'NONE', #4115, #5814 ) ;
#19265 = FACE_OUTER_BOUND ( 'NONE', #69061, .T. ) ;
#19266 = CIRCLE ( 'NONE', #39559, 0.2500000000000002220 ) ;
#19267 = CARTESIAN_POINT ( 'NONE',  ( 0.000000000000000000, 110.4999999999999858, -23.00000000000000000 ) ) ;
#19268 = CARTESIAN_POINT ( 'NONE',  ( -8.437984349512095861, 120.6929263765338050, -5.166775262442723748E-16 ) ) ;
#19269 = ORIENTED_EDGE ( 'NONE', *, *, #43256, .T. ) ;
#19270 = STYLED_ITEM ( 'NONE', ( #17409 ), #24302 ) ;
#19271 = ORIENTED_EDGE ( 'NONE', *, *, #62164, .F. ) ;
#19272 = FILL_AREA_STYLE_COLOUR ( '', #44098 ) ;
#19273 = CARTESIAN_POINT ( 'NONE',  ( 45.65811388300841855, 10.21937129433612057, 6.292893218813452982 ) ) ;
#19274 = DIRECTION ( 'NONE',  ( -1.000000000000000000, 0.000000000000000000, 0.000000000000000000 ) ) ;
#19275 = EDGE_CURVE ( 'NONE', #16904, #51850, #34380, .T. ) ;
#19276 = CARTESIAN_POINT ( 'NONE',  ( -49.85499999999998266, 4.716976649647094177, 6.492361379858945902 ) ) ;
#19277 = VERTEX_POINT ( 'NONE', #1921 ) ;
#19278 = CARTESIAN_POINT ( 'NONE',  ( 0.000000000000000000, 0.000000000000000000, 12.50000000000000000 ) ) ;
#19279 = CARTESIAN_POINT ( 'NONE',  ( -178.2549999999999955, -4.716976649647092401, 6.492361379858946790 ) ) ;
#19280 = EDGE_CURVE ( 'NONE', #13760, #12794, #61073, .T. ) ;
#19281 = CARTESIAN_POINT ( 'NONE',  ( -90.59292637653381064, -3.094860106618431139, -9.524999999999991473 ) ) ;
#19282 =( NAMED_UNIT ( * ) PLANE_ANGLE_UNIT ( ) SI_UNIT ( $, .RADIAN. ) );
#19283 = CARTESIAN_POINT ( 'NONE',  ( -56.90707362346616804, -3.094860106618429807, 9.524999999999991473 ) ) ;
#19284 = COLOUR_RGB ( '', 0.66274510, 0.83137255, 0.94901961) ;
#19285 = CARTESIAN_POINT ( 'NONE',  ( -178.6450000000000102, 4.716976649647091513, -6.492361379858946790 ) ) ;
#19286 = DIRECTION ( 'NONE',  ( 0.000000000000000000, -1.000000000000000000, 0.000000000000000000 ) ) ;
#19287 = ORIENTED_EDGE ( 'NONE', *, *, #44776, .F. ) ;
#19288 = LINE ( 'NONE', #14039, #12211 ) ;
#19289 = AXIS2_PLACEMENT_3D ( 'NONE', #4352, #5402, #36791 ) ;
#19290 = EDGE_CURVE ( 'NONE', #13063, #10616, #23898, .T. ) ;
#19291 = VECTOR ( 'NONE', #1522, 1000.000000000000000 ) ;
#19292 = LINE ( 'NONE', #24562, #66148 ) ;
#19293 = DIRECTION ( 'NONE',  ( -0.000000000000000000, -0.000000000000000000, -1.000000000000000000 ) ) ;
#19294 = CARTESIAN_POINT ( 'NONE',  ( -89.15499999999998693, 7.632228543268600340, 2.479861379858949277 ) ) ;
#19295 = DIRECTION ( 'NONE',  ( 1.000000000000000000, 0.000000000000000000, 0.000000000000000000 ) ) ;
#19296 = FACE_OUTER_BOUND ( 'NONE', #57403, .T. ) ;
#19297 = FACE_OUTER_BOUND ( 'NONE', #10597, .T. ) ;
#19298 = EDGE_CURVE ( 'NONE', #49707, #7942, #13769, .T. ) ;
#19299 = AXIS2_PLACEMENT_3D ( 'NONE', #49029, #55291, #13073 ) ;
#19300 = CARTESIAN_POINT ( 'NONE',  ( -89.09499999999998465, -2.607480562269071545, -8.024999999999991473 ) ) ;
#19301 = CARTESIAN_POINT ( 'NONE',  ( -8.102448949553181734, 120.6049999999999756, 5.886773742842747126 ) ) ;
#19302 = CARTESIAN_POINT ( 'NONE',  ( -71.84499999999999886, -7.632228543268599452, 2.479861379858951054 ) ) ;
#19303 = STYLED_ITEM ( 'NONE', ( #31878 ), #22304 ) ;
#19304 = SURFACE_STYLE_FILL_AREA ( #35153 ) ;
#19305 = EDGE_CURVE ( 'NONE', #56838, #68708, #44400, .T. ) ;
#19306 = CARTESIAN_POINT ( 'NONE',  ( -15.98999599679679839, 118.4999999999999716, -7.500000000000000000 ) ) ;
#19307 = DIRECTION ( 'NONE',  ( 0.000000000000000000, 0.000000000000000000, 1.000000000000000000 ) ) ;
#19308 = UNCERTAINTY_MEASURE_WITH_UNIT (LENGTH_MEASURE( 1.000000000000000082E-05 ), #44689, 'distance_accuracy_value', 'NONE');
#19309 = DIRECTION ( 'NONE',  ( 0.000000000000000000, -1.000000000000000000, 0.000000000000000000 ) ) ;
#19310 = ORIENTED_EDGE ( 'NONE', *, *, #33012, .T. ) ;
#19311 = CARTESIAN_POINT ( 'NONE',  ( -111.5929263765337822, -3.094860106618431139, -9.524999999999991473 ) ) ;
#19312 = EDGE_CURVE ( 'NONE', #14021, #41380, #50540, .T. ) ;
#19313 = CARTESIAN_POINT ( 'NONE',  ( -128.0949999999999704, -2.607480562269071545, -8.024999999999991473 ) ) ;
#19315 = SURFACE_STYLE_FILL_AREA ( #52739 ) ;
#19314 = TOROIDAL_SURFACE ( 'NONE', #63114, 18.99999999999998934, 1.000000000000000000 ) ;
#19316 = AXIS2_PLACEMENT_3D ( 'NONE', #10816, #26619, #10479 ) ;
#19317 = DIRECTION ( 'NONE',  ( 0.000000000000000000, -1.000000000000000000, -0.000000000000000000 ) ) ;
#19318 = CIRCLE ( 'NONE', #50774, 0.5000000000000004441 ) ;
#19320 = DIRECTION ( 'NONE',  ( -0.000000000000000000, -1.000000000000000000, -0.000000000000000000 ) ) ;
#19319 = CARTESIAN_POINT ( 'NONE',  ( -131.3929263765338078, 8.102448949553176405, 5.886773742842740909 ) ) ;
#19321 = FILL_AREA_STYLE ('',( #30917 ) ) ;
#19322 = ORIENTED_EDGE ( 'NONE', *, *, #12447, .T. ) ;
#19323 = ORIENTED_EDGE ( 'NONE', *, *, #2493, .F. ) ;
#19324 = CARTESIAN_POINT ( 'NONE',  ( 15.98999599679679839, 117.9999999999999716, -9.500000000000000000 ) ) ;
#19325 = AXIS2_PLACEMENT_3D ( 'NONE', #65222, #17420, #38886 ) ;
#19326 = DIRECTION ( 'NONE',  ( 1.000000000000000000, 0.000000000000000000, -0.000000000000000000 ) ) ;
#19327 = CARTESIAN_POINT ( 'NONE',  ( -98.45707362346617231, -9.058813317711329915, 2.943386871421371787 ) ) ;
#19328 = CIRCLE ( 'NONE', #13715, 1.000000000000000888 ) ;
#19329 = CARTESIAN_POINT ( 'NONE',  ( -45.99999999999998579, 0.000000000000000000, 0.000000000000000000 ) ) ;
#19330 = DIRECTION ( 'NONE',  ( 0.000000000000000000, 0.000000000000000000, -1.000000000000000000 ) ) ;
#19331 = ORIENTED_EDGE ( 'NONE', *, *, #65591, .T. ) ;
#19332 = CARTESIAN_POINT ( 'NONE',  ( -131.4549999999999841, 7.632228543268599452, -2.479861379858951942 ) ) ;
#19333 = VERTEX_POINT ( 'NONE', #18529 ) ;
#19334 = FACE_OUTER_BOUND ( 'NONE', #13135, .T. ) ;
#19335 = CARTESIAN_POINT ( 'NONE',  ( -119.0070736234661837, -8.102448949553172852, -5.886773742842741797 ) ) ;
#19336 = ORIENTED_EDGE ( 'NONE', *, *, #31765, .T. ) ;
#19337 = CARTESIAN_POINT ( 'NONE',  ( 61.99999999999998579, 33.74999999999999289, 4.000000000000000000 ) ) ;
#19338 = LINE ( 'NONE', #46839, #50109 ) ;
#19339 = ORIENTED_EDGE ( 'NONE', *, *, #9728, .F. ) ;
#19340 = CARTESIAN_POINT ( 'NONE',  ( 31.00000000000000711, 15.00000000000000000, -35.50000000000000000 ) ) ;
#19341 = CARTESIAN_POINT ( 'NONE',  ( -9.058813317711338797, 143.3449999999999989, 2.943386871421373563 ) ) ;
#19342 = SPHERICAL_SURFACE ( 'NONE', #11525, 1.000000000000000000 ) ;
#19343 = VERTEX_POINT ( 'NONE', #40017 ) ;
#19344 = CARTESIAN_POINT ( 'NONE',  ( -54.20707362346616520, 3.094860106618433360, 9.524999999999991473 ) ) ;
#19345 = CARTESIAN_POINT ( 'NONE',  ( 9.058813317711338797, 136.9549999999999841, -2.943386871421372675 ) ) ;
#19346 = CARTESIAN_POINT ( 'NONE',  ( 1.000000000000000000, 0.000000000000000000, -3.000000000000000000 ) ) ;
#19347 = PRODUCT_DEFINITION_SHAPE ( 'NONE', 'NONE',  #69703 ) ;
#19348 = ORIENTED_EDGE ( 'NONE', *, *, #34801, .F. ) ;
#19349 = CARTESIAN_POINT ( 'NONE',  ( -8.437984349512095861, 117.6929263765338050, -5.166775262442723748E-16 ) ) ;
#19350 = FACE_OUTER_BOUND ( 'NONE', #30285, .T. ) ;
#19351 = UNCERTAINTY_MEASURE_WITH_UNIT (LENGTH_MEASURE( 1.000000000000000082E-05 ), #59201, 'distance_accuracy_value', 'NONE');
#19352 = CIRCLE ( 'NONE', #5890, 0.5000000000000004441 ) ;
#19353 = CARTESIAN_POINT ( 'NONE',  ( -97.94292637653380496, 0.000000000000000000, 9.524999999999991473 ) ) ;
#19354 =( NAMED_UNIT ( * ) PLANE_ANGLE_UNIT ( ) SI_UNIT ( $, .RADIAN. ) );
#19355 = ORIENTED_EDGE ( 'NONE', *, *, #501, .F. ) ;
#19356 = STYLED_ITEM ( 'NONE', ( #55945 ), #22725 ) ;
#19357 = DIRECTION ( 'NONE',  ( 0.000000000000000000, 0.000000000000000000, 1.000000000000000000 ) ) ;
#19358 = VERTEX_POINT ( 'NONE', #34682 ) ;
#19359 = CARTESIAN_POINT ( 'NONE',  ( 23.50000000000001776, 15.00000000000000000, 29.68999999999999417 ) ) ;
#19360 = PLANE ( 'NONE',  #61436 ) ;
#19361 = DIRECTION ( 'NONE',  ( 0.000000000000000000, 0.000000000000000000, 1.000000000000000000 ) ) ;
#19362 = CARTESIAN_POINT ( 'NONE',  ( -159.2050000000000125, -2.607480562269071545, -8.024999999999991473 ) ) ;
#19363 = ORIENTED_EDGE ( 'NONE', *, *, #8606, .T. ) ;
#19364 = DIRECTION ( 'NONE',  ( 1.000000000000000000, 0.000000000000000000, 0.000000000000000000 ) ) ;
#19365 = UNCERTAINTY_MEASURE_WITH_UNIT (LENGTH_MEASURE( 1.000000000000000082E-05 ), #36821, 'distance_accuracy_value', 'NONE');
#19366 = VECTOR ( 'NONE', #13828, 1000.000000000000000 ) ;
#19367 = EDGE_CURVE ( 'NONE', #37693, #52614, #63222, .T. ) ;
#19368 = TOROIDAL_SURFACE ( 'NONE', #9452, 14.49999999999999822, 0.5000000000000000000 ) ;
#19369 =( NAMED_UNIT ( * ) SI_UNIT ( $, .STERADIAN. ) SOLID_ANGLE_UNIT ( ) );
#19370 = CARTESIAN_POINT ( 'NONE',  ( -54.62809784357641263, -9.152876382972518599, 4.262533829682994657 ) ) ;
#19371 = DIRECTION ( 'NONE',  ( 1.000000000000000000, 0.000000000000000000, -0.000000000000000000 ) ) ;
#19372 = ORIENTED_EDGE ( 'NONE', *, *, #27603, .T. ) ;
#19373 = CYLINDRICAL_SURFACE ( 'NONE', #66770, 8.025000000000000355 ) ;
#19374 = EDGE_CURVE ( 'NONE', #60681, #52169, #13574, .T. ) ;
#19375 = ORIENTED_EDGE ( 'NONE', *, *, #63780, .T. ) ;
#19376 = CARTESIAN_POINT ( 'NONE',  ( 0.000000000000000000, 1.000000000000000000, 3.000000000000000000 ) ) ;
#19377 = DIRECTION ( 'NONE',  ( 1.000000000000000000, -5.204170427930416550E-15, 0.000000000000000000 ) ) ;
#19378 = EDGE_CURVE ( 'NONE', #62177, #59244, #25011, .T. ) ;
#19379 = AXIS2_PLACEMENT_3D ( 'NONE', #17351, #18, #38120 ) ;
#19380 = CARTESIAN_POINT ( 'NONE',  ( -71.30499999999997840, 8.437984349512085203, -1.550032578732815448E-15 ) ) ;
#19381 = ORIENTED_EDGE ( 'NONE', *, *, #13500, .T. ) ;
#19382 = DIRECTION ( 'NONE',  ( -0.000000000000000000, -0.000000000000000000, -1.000000000000000000 ) ) ;
#19383 =( GEOMETRIC_REPRESENTATION_CONTEXT ( 3 ) GLOBAL_UNCERTAINTY_ASSIGNED_CONTEXT ( ( #56719 ) ) GLOBAL_UNIT_ASSIGNED_CONTEXT ( ( #57986, #3771, #15435 ) ) REPRESENTATION_CONTEXT ( 'NONE', 'WORKASPACE' ) );
#19384 = CARTESIAN_POINT ( 'NONE',  ( -150.5070736234661410, 8.102448949553176405, 5.886773742842740909 ) ) ;
#19385 = ORIENTED_EDGE ( 'NONE', *, *, #48971, .F. ) ;
#19386 = MECHANICAL_DESIGN_GEOMETRIC_PRESENTATION_REPRESENTATION (  '', ( #55332 ), #1357 ) ;
#19387 = CYLINDRICAL_SURFACE ( 'NONE', #57117, 4.999999999999997335 ) ;
#19388 =( NAMED_UNIT ( * ) PLANE_ANGLE_UNIT ( ) SI_UNIT ( $, .RADIAN. ) );
#19389 = CARTESIAN_POINT ( 'NONE',  ( 23.50000000000001776, 27.44010416289936316, -27.18999999999999417 ) ) ;
#19390 = PRESENTATION_LAYER_ASSIGNMENT (  '', '', ( #62055 ) ) ;
#19392 = CARTESIAN_POINT ( 'NONE',  ( 68.99999999999998579, 37.00000000000000000, 3.750000000000000000 ) ) ;
#19391 = DIRECTION ( 'NONE',  ( -0.000000000000000000, -0.000000000000000000, -1.000000000000000000 ) ) ;
#19393 = ADVANCED_FACE ( 'NONE', ( #19892 ), #47377, .T. ) ;
#19394 = CARTESIAN_POINT ( 'NONE',  ( 5.598654528085809545, 136.1449999999999818, -7.705886871421373741 ) ) ;
#19395 = CARTESIAN_POINT ( 'NONE',  ( -101.2449999999999903, -4.716976649647093289, -6.492361379858945902 ) ) ;
#19396 = FACE_OUTER_BOUND ( 'NONE', #46735, .T. ) ;
#19397 = AXIS2_PLACEMENT_3D ( 'NONE', #3405, #61830, #13302 ) ;
#19398 =( GEOMETRIC_REPRESENTATION_CONTEXT ( 3 ) GLOBAL_UNCERTAINTY_ASSIGNED_CONTEXT ( ( #33340 ) ) GLOBAL_UNIT_ASSIGNED_CONTEXT ( ( #4079, #30469, #19587 ) ) REPRESENTATION_CONTEXT ( 'NONE', 'WORKASPACE' ) );
#19399 = CARTESIAN_POINT ( 'NONE',  ( 21.50000000000001066, 24.99999999999998579, 4.000000000000000000 ) ) ;
#19400 = UNCERTAINTY_MEASURE_WITH_UNIT (LENGTH_MEASURE( 1.000000000000000082E-05 ), #68396, 'distance_accuracy_value', 'NONE');
#19401 = FACE_OUTER_BOUND ( 'NONE', #4889, .T. ) ;
#19402 = COLOUR_RGB ( '', 0.72549020, 0.75294118, 0.79215686) ;
#19403 = CARTESIAN_POINT ( 'NONE',  ( -143.6929263765338192, 10.01517768586948698, -1.839758294383808571E-15 ) ) ;
#19404 =( LENGTH_UNIT ( ) NAMED_UNIT ( * ) SI_UNIT ( .MILLI., .METRE. ) );
#19405 = DIRECTION ( 'NONE',  ( 1.000000000000000000, 0.000000000000000000, 0.000000000000000000 ) ) ;
#19406 = CARTESIAN_POINT ( 'NONE',  ( -154.1949999999999648, 8.437984349512085203, -1.550032578732815448E-15 ) ) ;
#19407 = VECTOR ( 'NONE', #68697, 1000.000000000000000 ) ;
#19408 = ADVANCED_FACE ( 'NONE', ( #25181 ), #10060, .T. ) ;
#19409 = CARTESIAN_POINT ( 'NONE',  ( -70.75000000000000000, -3.000000000000000000, 24.00000000000000000 ) ) ;
#19410 = CIRCLE ( 'NONE', #27164, 0.2500000000000002220 ) ;
#19411 = ORIENTED_EDGE ( 'NONE', *, *, #42173, .F. ) ;
#19412 = CARTESIAN_POINT ( 'NONE',  ( 24.00000000000000355, 36.75000000000000000, 3.750000000000000000 ) ) ;
#19413 = ORIENTED_EDGE ( 'NONE', *, *, #51616, .F. ) ;
#19414 = COLOUR_RGB ( '', 0.66274510, 0.83137255, 0.94901961) ;
#19415 = EDGE_CURVE ( 'NONE', #11393, #1454, #42449, .T. ) ;
#19416 = CARTESIAN_POINT ( 'NONE',  ( 22.25000000000000711, 33.74999999999999289, 3.750000000000000000 ) ) ;
#19417 = FILL_AREA_STYLE_COLOUR ( '', #31567 ) ;
#19418 = CARTESIAN_POINT ( 'NONE',  ( 6.826472737025121695, 119.4929263765338163, -4.959722759717905660 ) ) ;
#19419 = CARTESIAN_POINT ( 'NONE',  ( -172.7070736234662718, -3.094860106620514362, -9.524999999998476241 ) ) ;
#19420 = MECHANICAL_DESIGN_GEOMETRIC_PRESENTATION_REPRESENTATION (  '', ( #63213 ), #17204 ) ;
#19421 = ORIENTED_EDGE ( 'NONE', *, *, #14563, .T. ) ;
#19422 = CARTESIAN_POINT ( 'NONE',  ( -156.6550000000000011, -7.632228543268600340, -2.479861379858950166 ) ) ;
#19423 = CIRCLE ( 'NONE', #25053, 0.5000000000000004441 ) ;
#19424 = EDGE_LOOP ( 'NONE', ( #19271, #41037, #15327 ) ) ;
#19425 = FACE_OUTER_BOUND ( 'NONE', #68057, .T. ) ;
#19426 = DIRECTION ( 'NONE',  ( -0.000000000000000000, -1.000000000000000000, -6.938893903907234689E-15 ) ) ;
#19427 = ORIENTED_EDGE ( 'NONE', *, *, #9760, .F. ) ;
#19428 = DIRECTION ( 'NONE',  ( 0.000000000000000000, 0.000000000000000000, -1.000000000000000000 ) ) ;
#19429 = CARTESIAN_POINT ( 'NONE',  ( 57.00000000000000000, 0.9999999999999991118, -80.00402776293826435 ) ) ;
#19430 = CARTESIAN_POINT ( 'NONE',  ( 2.607480562269071989, 158.7070736234661865, 8.025000000000002132 ) ) ;
#19431 = AXIS2_PLACEMENT_3D ( 'NONE', #60137, #64379, #638 ) ;
#19432 = ORIENTED_EDGE ( 'NONE', *, *, #25487, .F. ) ;
#19433 = CARTESIAN_POINT ( 'NONE',  ( -52.00000000000000000, -1.926070501056209087E-14, -11.50000000000000000 ) ) ;
#19434 = DIRECTION ( 'NONE',  ( -0.000000000000000000, -0.000000000000000000, -1.000000000000000000 ) ) ;
#19435 = CARTESIAN_POINT ( 'NONE',  ( -70.85499999999998977, 4.716976649647094177, 6.492361379858945902 ) ) ;
#19436 =( NAMED_UNIT ( * ) SI_UNIT ( $, .STERADIAN. ) SOLID_ANGLE_UNIT ( ) );
#19437 = ORIENTED_EDGE ( 'NONE', *, *, #57297, .F. ) ;
#19438 = CARTESIAN_POINT ( 'NONE',  ( 5.598654528085809545, 134.2549999999999955, -7.705886871421373741 ) ) ;
#19439 = UNCERTAINTY_MEASURE_WITH_UNIT (LENGTH_MEASURE( 1.000000000000000082E-05 ), #37249, 'distance_accuracy_value', 'NONE');
#19440 = FACE_OUTER_BOUND ( 'NONE', #62542, .T. ) ;
#19441 =( LENGTH_UNIT ( ) NAMED_UNIT ( * ) SI_UNIT ( .MILLI., .METRE. ) );
#19442 = EDGE_CURVE ( 'NONE', #21468, #38966, #62797, .T. ) ;
#19443 = LINE ( 'NONE', #56380, #60889 ) ;
#19444 = ORIENTED_EDGE ( 'NONE', *, *, #69110, .T. ) ;
#19445 = AXIS2_PLACEMENT_3D ( 'NONE', #21591, #53603, #424 ) ;
#19446 = CARTESIAN_POINT ( 'NONE',  ( -53.99499999999998323, -6.826472737025115478, 4.959722759717900331 ) ) ;
#19447 = ORIENTED_EDGE ( 'NONE', *, *, #29555, .F. ) ;
#19448 = CARTESIAN_POINT ( 'NONE',  ( 31.53557424407129517, 42.85561152959481035, 45.52242327283500600 ) ) ;
#19449 = VECTOR ( 'NONE', #64621, 1000.000000000000000 ) ;
#19450 = PLANE ( 'NONE',  #68353 ) ;
#19451 = CARTESIAN_POINT ( 'NONE',  ( -45.50000000000000000, -2.024042244987997205E-14, -10.00000000000000000 ) ) ;
#19452 = EDGE_CURVE ( 'NONE', #59074, #9325, #14899, .T. ) ;
#19453 = ORIENTED_EDGE ( 'NONE', *, *, #55112, .T. ) ;
#19454 = DIRECTION ( 'NONE',  ( 0.5000000000000001110, 0.8660254037844384856, 0.000000000000000000 ) ) ;
#19455 = CARTESIAN_POINT ( 'NONE',  ( 71.50000000000000000, 14.49137674618942562, -7.500000000000000000 ) ) ;
#19456 = ORIENTED_EDGE ( 'NONE', *, *, #29275, .T. ) ;
#19457 = ADVANCED_FACE ( 'NONE', ( #36103 ), #47031, .T. ) ;
#19458 = CARTESIAN_POINT ( 'NONE',  ( -100.8549999999999898, 4.716976649647094177, 6.492361379858945902 ) ) ;
#19459 = ORIENTED_EDGE ( 'NONE', *, *, #7955, .F. ) ;
#19460 = FACE_OUTER_BOUND ( 'NONE', #41898, .T. ) ;
#19461 = CARTESIAN_POINT ( 'NONE',  ( 8.750000000000001776, 25.24999999999998934, -3.750000000000000000 ) ) ;
#19462 = CARTESIAN_POINT ( 'NONE',  ( -140.6070736234661922, -8.102448949553172852, 5.886773742842742685 ) ) ;
#19463 =( GEOMETRIC_REPRESENTATION_CONTEXT ( 3 ) GLOBAL_UNCERTAINTY_ASSIGNED_CONTEXT ( ( #17983 ) ) GLOBAL_UNIT_ASSIGNED_CONTEXT ( ( #57353, #5253, #14805 ) ) REPRESENTATION_CONTEXT ( 'NONE', 'WORKASPACE' ) );
#19464 = DIRECTION ( 'NONE',  ( 0.000000000000000000, 0.000000000000000000, 1.000000000000000000 ) ) ;
#19465 = CARTESIAN_POINT ( 'NONE',  ( 8.102448949553181734, 144.9949999999999761, -5.886773742842746238 ) ) ;
#19466 = CARTESIAN_POINT ( 'NONE',  ( -79.40707362346617515, 3.094860106618428031, -9.524999999999993250 ) ) ;
#19467 = AXIS2_PLACEMENT_3D ( 'NONE', #6295, #6996, #49227 ) ;
#19468 = CARTESIAN_POINT ( 'NONE',  ( -92.69292637653379074, 10.01517768586948698, -1.839758294383808966E-15 ) ) ;
#19469 = STYLED_ITEM ( 'NONE', ( #12929 ), #31034 ) ;
#19470 = CARTESIAN_POINT ( 'NONE',  ( -19.48451829062191720, -11.79395247191043339, 2.235223184618424508 ) ) ;
#19472 = CARTESIAN_POINT ( 'NONE',  ( -100.6429263765337936, -5.598654528085801552, 7.705886871421367523 ) ) ;
#19471 = CARTESIAN_POINT ( 'NONE',  ( -57.11974195712093660, -8.499999999999992895, 3.000000000000000000 ) ) ;
#19473 = ADVANCED_FACE ( 'NONE', ( #26212 ), #52295, .F. ) ;
#19474 = AXIS2_PLACEMENT_3D ( 'NONE', #23232, #60842, #66121 ) ;
#19475 = CARTESIAN_POINT ( 'NONE',  ( -121.2549999999999812, -4.716976649647092401, 6.492361379858946790 ) ) ;
#19476 = CARTESIAN_POINT ( 'NONE',  ( -122.3949999999999818, -6.826472737025115478, -4.959722759717899443 ) ) ;
#19477 = CARTESIAN_POINT ( 'NONE',  ( -119.8449999999999989, -7.632228543268599452, 2.479861379858951054 ) ) ;
#19478 = ORIENTED_EDGE ( 'NONE', *, *, #60667, .F. ) ;
#19479 =( BOUNDED_CURVE ( )  B_SPLINE_CURVE ( 2, ( #9056, #14683, #47426, #52336, #36527, #51615, #67799, #36153, #58272, #68495, #57585 ),
 .UNSPECIFIED., .F., .F. ) 
 B_SPLINE_CURVE_WITH_KNOTS ( ( 3, 2, 2, 2, 2, 3 ),
 ( 0.7608695652173913526, 0.7630434782608696009, 0.7652173913043478493, 0.7673913043478260976, 0.7695652173913043459, 0.7717391304347825942 ),
 .UNSPECIFIED. ) 
 CURVE ( )  GEOMETRIC_REPRESENTATION_ITEM ( )  RATIONAL_B_SPLINE_CURVE ( ( 1.000000000000000000, 0.9510565162951535312, 1.000000000000000000, 0.9510565162951535312, 1.000000000000000000, 0.9510565162951535312, 1.000000000000000000, 0.9510565162951535312, 1.000000000000000000, 0.9510565162951535312, 1.000000000000000000 ) ) 
 REPRESENTATION_ITEM ( '' )  );
#19480 = SPHERICAL_SURFACE ( 'NONE', #2169, 0.5000000000000000000 ) ;
#19481 = PRESENTATION_STYLE_ASSIGNMENT (( #30361 ) ) ;
#19482 = DIRECTION ( 'NONE',  ( -1.000000000000000000, 0.000000000000000000, -4.625929269271509580E-16 ) ) ;
#19483 = CARTESIAN_POINT ( 'NONE',  ( -169.1929263765338192, -10.01517768586948698, 6.132527647946031529E-16 ) ) ;
#19484 = CARTESIAN_POINT ( 'NONE',  ( -48.44499999999998607, 0.000000000000000000, 8.024999999999991473 ) ) ;
#19485 = AXIS2_PLACEMENT_3D ( 'NONE', #60595, #49384, #2520 ) ;
#19486 = DIRECTION ( 'NONE',  ( 0.000000000000000000, 0.000000000000000000, -1.000000000000000000 ) ) ;
#19487 = AXIS2_PLACEMENT_3D ( 'NONE', #30833, #63204, #31872 ) ;
#19488 = STYLED_ITEM ( 'NONE', ( #55499 ), #61844 ) ;
#19489 = FILL_AREA_STYLE ('',( #40279 ) ) ;
#19490 = CARTESIAN_POINT ( 'NONE',  ( 0.000000000000000000, -7.000000000000000888, 0.000000000000000000 ) ) ;
#19491 = VERTEX_POINT ( 'NONE', #53322 ) ;
#19492 = CARTESIAN_POINT ( 'NONE',  ( -87.74292637653380211, -5.598654528085803328, -7.705886871421366635 ) ) ;
#19493 = ITEM_DEFINED_TRANSFORMATION ( 'NONE', 'NONE', #3367,  #42840 ) ;
#19494 = CARTESIAN_POINT ( 'NONE',  ( -53.60138881051015858, -9.947368421052628307, -2.264720458637549338 ) ) ;
#19495 = FACE_OUTER_BOUND ( 'NONE', #29503, .T. ) ;
#19496 = VECTOR ( 'NONE', #55271, 1000.000000000000000 ) ;
#19497 = CIRCLE ( 'NONE', #8274, 0.2500000000000002220 ) ;
#19498 = DIRECTION ( 'NONE',  ( -1.000000000000000000, 0.000000000000000000, 1.300977106640434891E-16 ) ) ;
#19499 =( NAMED_UNIT ( * ) PLANE_ANGLE_UNIT ( ) SI_UNIT ( $, .RADIAN. ) );
#19500 = FACE_OUTER_BOUND ( 'NONE', #46525, .T. ) ;
#19501 = AXIS2_PLACEMENT_3D ( 'NONE', #19416, #40558, #62332 ) ;
#19502 = VERTEX_POINT ( 'NONE', #21633 ) ;
#19503 = CARTESIAN_POINT ( 'NONE',  ( 44.25000000000000000, 19.24999999999998224, 3.750000000000000000 ) ) ;
#19504 = DIRECTION ( 'NONE',  ( -0.000000000000000000, 0.000000000000000000, -1.000000000000000000 ) ) ;
#19505 = LINE ( 'NONE', #36441, #27252 ) ;
#19506 = ORIENTED_EDGE ( 'NONE', *, *, #63387, .F. ) ;
#19507 = CARTESIAN_POINT ( 'NONE',  ( -45.91547277936962246, 9.430195807687219656, 3.611004237778671744 ) ) ;
#19508 = MECHANICAL_DESIGN_GEOMETRIC_PRESENTATION_REPRESENTATION (  '', ( #44273 ), #6002 ) ;
#19509 = PRESENTATION_STYLE_ASSIGNMENT (( #46293 ) ) ;
#19510 = CARTESIAN_POINT ( 'NONE',  ( -7.632228543268607446, 133.6570736234661467, -2.479861379858953718 ) ) ;
#19511 = DIRECTION ( 'NONE',  ( 0.000000000000000000, 0.000000000000000000, -1.000000000000000000 ) ) ;
#19512 = VECTOR ( 'NONE', #23859, 1000.000000000000000 ) ;
#19513 = EDGE_LOOP ( 'NONE', ( #35461, #1220, #34036, #2490 ) ) ;
#19514 = CARTESIAN_POINT ( 'NONE',  ( -106.2549999999999955, -4.716976649647092401, 6.492361379858946790 ) ) ;
#19515 = COLOUR_RGB ( '', 0.66274510, 0.83137255, 0.94901961) ;
#19516 = EDGE_LOOP ( 'NONE', ( #58758, #10388, #26854, #35745 ) ) ;
#19517 = COLOUR_RGB ( '', 0.08235294, 0.09019608, 0.10196078) ;
#19518 = CARTESIAN_POINT ( 'NONE',  ( 0.000000000000000000, -2.500000000000000000, 5.000000000000000000 ) ) ;
#19519 = CARTESIAN_POINT ( 'NONE',  ( 4.716976649647096842, 149.8570736234661638, 6.492361379858953896 ) ) ;
#19520 = CARTESIAN_POINT ( 'NONE',  ( 0.000000000000000000, 114.9999999999999574, 0.000000000000000000 ) ) ;
#19521 = ADVANCED_FACE ( 'NONE', ( #32517 ), #58760, .T. ) ;
#19522 = AXIS2_PLACEMENT_3D ( 'NONE', #65820, #33796, #39813 ) ;
#19523 = CARTESIAN_POINT ( 'NONE',  ( -86.54499999999998749, -7.632228543268600340, -2.479861379858950166 ) ) ;
#19524 = ORIENTED_EDGE ( 'NONE', *, *, #49507, .F. ) ;
#19525 = CIRCLE ( 'NONE', #58863, 111.0000000000000142 ) ;
#19526 = VECTOR ( 'NONE', #14192, 1000.000000000000000 ) ;
#19527 = FILL_AREA_STYLE ('',( #46674 ) ) ;
#19528 = CARTESIAN_POINT ( 'NONE',  ( -35.65778776279520912, -9.947368421052624754, 4.481646853389230856 ) ) ;
#19529 = ORIENTED_EDGE ( 'NONE', *, *, #59394, .T. ) ;
#19530 = CARTESIAN_POINT ( 'NONE',  ( 0.000000000000000000, 0.000000000000000000, -2.000000000000000000 ) ) ;
#19531 = ADVANCED_FACE ( 'NONE', ( #37875 ), #5782, .T. ) ;
#19533 = DIRECTION ( 'NONE',  ( -1.000000000000000000, 0.000000000000000000, 0.000000000000000000 ) ) ;
#19532 = VECTOR ( 'NONE', #37600, 1000.000000000000000 ) ;
#19535 = ADVANCED_FACE ( 'NONE', ( #48766 ), #17207, .F. ) ;
#19534 = LINE ( 'NONE', #41729, #44760 ) ;
#19536 = VERTEX_POINT ( 'NONE', #11774 ) ;
#19537 = FILL_AREA_STYLE_COLOUR ( '', #65560 ) ;
#19538 = ADVANCED_FACE ( 'NONE', ( #32896 ), #10746, .T. ) ;
#19539 = VERTEX_POINT ( 'NONE', #61337 ) ;
#19540 = CARTESIAN_POINT ( 'NONE',  ( -60.00000000000000000, -2.024042244987997205E-14, -7.000000000000000888 ) ) ;
#19541 = CARTESIAN_POINT ( 'NONE',  ( 0.7093150608870643081, -2.499999999999996891, 7.000000000000000888 ) ) ;
#19542 = MECHANICAL_DESIGN_GEOMETRIC_PRESENTATION_REPRESENTATION (  '', ( #48818 ), #18460 ) ;
#19543 = CIRCLE ( 'NONE', #30786, 0.2500000000000002220 ) ;
#19544 = CARTESIAN_POINT ( 'NONE',  ( -171.8070736234661808, 10.01517768586948698, -1.839758294383808571E-15 ) ) ;
#19545 = ADVANCED_FACE ( 'NONE', ( #56058 ), #12450, .T. ) ;
#19546 = SURFACE_STYLE_USAGE ( .BOTH. , #67746 ) ;
#19547 = CARTESIAN_POINT ( 'NONE',  ( 10.01517768586949408, 117.6949999999999790, 1.839758294383810543E-15 ) ) ;
#19548 = CARTESIAN_POINT ( 'NONE',  ( -107.4570736234661865, -9.058813317711329915, 2.943386871421371787 ) ) ;
#19549 = EDGE_CURVE ( 'NONE', #4398, #56593, #18450, .T. ) ;
#19550 =( NAMED_UNIT ( * ) SI_UNIT ( $, .STERADIAN. ) SOLID_ANGLE_UNIT ( ) );
#19551 = VERTEX_POINT ( 'NONE', #7201 ) ;
#19552 = DIRECTION ( 'NONE',  ( 0.000000000000000000, 0.000000000000000000, 1.000000000000000000 ) ) ;
#19553 = CARTESIAN_POINT ( 'NONE',  ( -106.2570736234661695, 5.598654528085800663, -7.705886871421367523 ) ) ;
#19555 = CYLINDRICAL_SURFACE ( 'NONE', #63867, 0.5000000000000004441 ) ;
#19554 = DIRECTION ( 'NONE',  ( -9.376883653928687363E-17, 1.000000000000000000, 0.000000000000000000 ) ) ;
#19556 = SURFACE_SIDE_STYLE ('',( #35750 ) ) ;
#19557 = STYLED_ITEM ( 'NONE', ( #39792 ), #38514 ) ;
#19558 = CARTESIAN_POINT ( 'NONE',  ( -152.3050000000000068, 8.437984349512085203, -1.550032578732815448E-15 ) ) ;
#19559 = CARTESIAN_POINT ( 'NONE',  ( -74.99999999999998579, 9.027015924850166684, 6.778771685250380763 ) ) ;
#19560 = CARTESIAN_POINT ( 'NONE',  ( -5.201328222576680815, 110.9678030318073496, -7.425688344617400460 ) ) ;
#19561 = CARTESIAN_POINT ( 'NONE',  ( -153.8949999999999818, 6.826472737025116366, 4.959722759717898555 ) ) ;
#19562 = STYLED_ITEM ( 'NONE', ( #40006 ), #36824 ) ;
#19563 = CARTESIAN_POINT ( 'NONE',  ( -143.9949999999999761, -6.826472737025113702, 4.959722759717902107 ) ) ;
#19564 = ORIENTED_EDGE ( 'NONE', *, *, #8206, .F. ) ;
#19565 = STYLED_ITEM ( 'NONE', ( #51553 ), #55902 ) ;
#19566 = CARTESIAN_POINT ( 'NONE',  ( -181.4070736234661751, 3.094860106618131823, -9.525000000000206413 ) ) ;
#19567 = DIRECTION ( 'NONE',  ( -0.000000000000000000, -1.000000000000000000, -0.000000000000000000 ) ) ;
#19568 = CARTESIAN_POINT ( 'NONE',  ( 34.99999999999999289, 113.4999999999999858, -7.000000000000000000 ) ) ;
#19569 = CIRCLE ( 'NONE', #58849, 4.000000000000000000 ) ;
#19570 = CARTESIAN_POINT ( 'NONE',  ( -64.25499999999998124, -4.716976649647092401, 6.492361379858946790 ) ) ;
#19571 = CARTESIAN_POINT ( 'NONE',  ( 48.50000000000000000, 14.49137674618942562, 10.00000000000000000 ) ) ;
#19572 = CARTESIAN_POINT ( 'NONE',  ( -154.2570736234661979, 5.598654528085800663, -7.705886871421367523 ) ) ;
#19573 = AXIS2_PLACEMENT_3D ( 'NONE', #14161, #60931, #62336 ) ;
#19574 = CARTESIAN_POINT ( 'NONE',  ( -64.49499999999997613, 6.826472737025113702, -4.959722759717902107 ) ) ;
#19575 = CARTESIAN_POINT ( 'NONE',  ( -9.058813317711337021, 159.1550000000000011, -2.943386871421374895 ) ) ;
#19576 = DIRECTION ( 'NONE',  ( 1.000000000000000000, 0.000000000000000000, 0.000000000000000000 ) ) ;
#19577 = AXIS2_PLACEMENT_3D ( 'NONE', #67998, #19783, #41277 ) ;
#19578 = DIRECTION ( 'NONE',  ( 0.000000000000000000, 0.000000000000000000, 1.000000000000000000 ) ) ;
#19579 = CARTESIAN_POINT ( 'NONE',  ( 16.00000000000002487, 123.6078173946806942, -2.103763174417413592E-14 ) ) ;
#19580 = VECTOR ( 'NONE', #12115, 1000.000000000000000 ) ;
#19581 = CARTESIAN_POINT ( 'NONE',  ( -159.6570736234661751, 9.058813317711329915, 2.943386871421369566 ) ) ;
#19582 = TOROIDAL_SURFACE ( 'NONE', #3840, 14.49999999999999822, 0.5000000000000000000 ) ;
#19583 = CARTESIAN_POINT ( 'NONE',  ( -83.49999999999998579, -2.499999999999999556, 24.00000000000000000 ) ) ;
#19584 = DIRECTION ( 'NONE',  ( 1.000000000000000000, 0.000000000000000000, 0.000000000000000000 ) ) ;
#19585 = AXIS2_PLACEMENT_3D ( 'NONE', #5351, #16313, #53566 ) ;
#19586 = DIRECTION ( 'NONE',  ( 0.2413793103448194644, 0.9704308468600220117, 0.000000000000000000 ) ) ;
#19587 =( NAMED_UNIT ( * ) SI_UNIT ( $, .STERADIAN. ) SOLID_ANGLE_UNIT ( ) );
#19588 = ORIENTED_EDGE ( 'NONE', *, *, #40363, .F. ) ;
#19590 = ORIENTED_EDGE ( 'NONE', *, *, #43009, .F. ) ;
#19589 = VECTOR ( 'NONE', #46113, 1000.000000000000000 ) ;
#19591 = DIRECTION ( 'NONE',  ( -1.000000000000000000, 0.000000000000000000, 1.300977106640434891E-16 ) ) ;
#19592 = DIRECTION ( 'NONE',  ( 1.000000000000000000, -1.189524669241239115E-16, 0.000000000000000000 ) ) ;
#19593 =( NAMED_UNIT ( * ) PLANE_ANGLE_UNIT ( ) SI_UNIT ( $, .RADIAN. ) );
#19594 = CARTESIAN_POINT ( 'NONE',  ( -45.00000000000000000, 8.553246373267509028, 6.928940927505456315 ) ) ;
#19595 = SURFACE_STYLE_USAGE ( .BOTH. , #63210 ) ;
#19596 = ORIENTED_EDGE ( 'NONE', *, *, #41034, .T. ) ;
#19597 = VERTEX_POINT ( 'NONE', #61660 ) ;
#19598 = LINE ( 'NONE', #52340, #30888 ) ;
#19599 = VECTOR ( 'NONE', #40825, 1000.000000000000000 ) ;
#19600 = ORIENTED_EDGE ( 'NONE', *, *, #9655, .T. ) ;
#19601 =( NAMED_UNIT ( * ) SI_UNIT ( $, .STERADIAN. ) SOLID_ANGLE_UNIT ( ) );
#19602 = DIRECTION ( 'NONE',  ( 0.000000000000000000, -1.000000000000000000, 0.000000000000000000 ) ) ;
#19603 = EDGE_LOOP ( 'NONE', ( #33492, #11375, #30891, #16036 ) ) ;
#19604 = EDGE_CURVE ( 'NONE', #59357, #69289, #44531, .T. ) ;
#19605 = MECHANICAL_DESIGN_GEOMETRIC_PRESENTATION_REPRESENTATION (  '', ( #38748 ), #46473 ) ;
#19606 = SURFACE_STYLE_FILL_AREA ( #46751 ) ;
#19607 = CARTESIAN_POINT ( 'NONE',  ( -106.6449999999999960, 4.716976649647091513, -6.492361379858946790 ) ) ;
#19608 = ORIENTED_EDGE ( 'NONE', *, *, #41413, .T. ) ;
#19609 = AXIS2_PLACEMENT_3D ( 'NONE', #22284, #60, #58537 ) ;
#19610 = EDGE_CURVE ( 'NONE', #63887, #13795, #60304, .T. ) ;
#19611 = PLANE ( 'NONE',  #27645 ) ;
#19612 = FILL_AREA_STYLE ('',( #36173 ) ) ;
#19613 = LINE ( 'NONE', #41111, #55315 ) ;
#19614 = ORIENTED_EDGE ( 'NONE', *, *, #60940, .T. ) ;
#19615 = CARTESIAN_POINT ( 'NONE',  ( 4.716976649647099507, 143.6429263765338078, -6.492361379858953008 ) ) ;
#19616 = CARTESIAN_POINT ( 'NONE',  ( 0.000000000000000000, 149.9999999999999716, -23.00000000000000355 ) ) ;
#19617 = SURFACE_SIDE_STYLE ('',( #18902 ) ) ;
#19618 = FACE_OUTER_BOUND ( 'NONE', #799, .T. ) ;
#19619 = VERTEX_POINT ( 'NONE', #39584 ) ;
#19620 = DIRECTION ( 'NONE',  ( 1.000000000000000000, -0.000000000000000000, 0.000000000000000000 ) ) ;
#19621 = EDGE_CURVE ( 'NONE', #44068, #44052, #10020, .T. ) ;
#19622 = EDGE_LOOP ( 'NONE', ( #19943, #30581, #4107, #53944 ) ) ;
#19623 = DIRECTION ( 'NONE',  ( 0.000000000000000000, 1.000000000000000000, 0.000000000000000000 ) ) ;
#19624 = DIRECTION ( 'NONE',  ( -1.000000000000000000, -0.000000000000000000, -0.000000000000000000 ) ) ;
#19625 = SURFACE_STYLE_FILL_AREA ( #30867 ) ;
#19626 = FACE_OUTER_BOUND ( 'NONE', #69227, .T. ) ;
#19627 = CARTESIAN_POINT ( 'NONE',  ( -122.3050000000000068, 8.437984349512085203, -1.550032578732815448E-15 ) ) ;
#19628 = LINE ( 'NONE', #9440, #29731 ) ;
#19629 = CARTESIAN_POINT ( 'NONE',  ( 0.000000000000000000, 142.0570736234661524, -8.025000000000000355 ) ) ;
#19630 = SURFACE_STYLE_USAGE ( .BOTH. , #67835 ) ;
#19631 = VECTOR ( 'NONE', #59341, 1000.000000000000000 ) ;
#19632 =( GEOMETRIC_REPRESENTATION_CONTEXT ( 3 ) GLOBAL_UNCERTAINTY_ASSIGNED_CONTEXT ( ( #29218 ) ) GLOBAL_UNIT_ASSIGNED_CONTEXT ( ( #64266, #5495, #21709 ) ) REPRESENTATION_CONTEXT ( 'NONE', 'WORKASPACE' ) );
#19633 = CARTESIAN_POINT ( 'NONE',  ( 7.750000000000000000, 33.74999999999998579, 4.000000000000000000 ) ) ;
#19634 = EDGE_CURVE ( 'NONE', #6374, #2941, #40258, .T. ) ;
#19635 = CARTESIAN_POINT ( 'NONE',  ( -74.72379611408101141, 36.27863051838266983, 9.964730096445045149 ) ) ;
#19636 = ORIENTED_EDGE ( 'NONE', *, *, #8831, .T. ) ;
#19637 = EDGE_LOOP ( 'NONE', ( #24978, #58753, #1824, #54798 ) ) ;
#19638 = LINE ( 'NONE', #14355, #54222 ) ;
#19639 = SURFACE_STYLE_USAGE ( .BOTH. , #46785 ) ;
#19641 = FILL_AREA_STYLE ('',( #67846 ) ) ;
#19640 = AXIS2_PLACEMENT_3D ( 'NONE', #2365, #40106, #56592 ) ;
#19642 = ORIENTED_EDGE ( 'NONE', *, *, #11825, .T. ) ;
#19643 = CARTESIAN_POINT ( 'NONE',  ( -123.9570736234661723, 9.058813317711329915, -2.943386871421373119 ) ) ;
#19644 = CARTESIAN_POINT ( 'NONE',  ( -180.2049999999999841, -2.607480562269071545, -8.024999999999991473 ) ) ;
#19645 = LINE ( 'NONE', #52713, #29582 ) ;
#19646 = DIRECTION ( 'NONE',  ( -0.000000000000000000, 0.000000000000000000, -1.000000000000000000 ) ) ;
#19647 = CARTESIAN_POINT ( 'NONE',  ( -60.20707362346617231, 3.094860106618433360, 9.524999999999991473 ) ) ;
#19648 = PRESENTATION_LAYER_ASSIGNMENT (  '', '', ( #55551 ) ) ;
#19649 = AXIS2_PLACEMENT_3D ( 'NONE', #65198, #17048, #10025 ) ;
#19650 = AXIS2_PLACEMENT_3D ( 'NONE', #61632, #23329, #50415 ) ;
#19651 = CARTESIAN_POINT ( 'NONE',  ( -181.6450000000000102, 4.716976649647091513, -6.492361379858946790 ) ) ;
#19652 = PRESENTATION_STYLE_ASSIGNMENT (( #67856 ) ) ;
#19653 = ORIENTED_EDGE ( 'NONE', *, *, #4793, .T. ) ;
#19654 = FILL_AREA_STYLE_COLOUR ( '', #56034 ) ;
#19655 = PRESENTATION_STYLE_ASSIGNMENT (( #67862 ) ) ;
#19656 = CARTESIAN_POINT ( 'NONE',  ( -95.45499999999998408, 7.632228543268599452, -2.479861379858951942 ) ) ;
#19657 = CARTESIAN_POINT ( 'NONE',  ( 9.385348596157497170, 154.4999999999999432, 1.684017021904244737 ) ) ;
#19658 = CARTESIAN_POINT ( 'NONE',  ( 1.000000000000000222, 1.224646799147373175E-16, -3.000000000000000000 ) ) ;
#19659 = CARTESIAN_POINT ( 'NONE',  ( 98.00000000000000000, 5.000000000000000000, -5.000000000000004441 ) ) ;
#19660 = CARTESIAN_POINT ( 'NONE',  ( -87.29499999999998749, -2.607480562269069768, 8.024999999999991473 ) ) ;
#19661 = CARTESIAN_POINT ( 'NONE',  ( -5.598654528085806881, 131.8549999999999898, -7.705886871421374629 ) ) ;
#19662 = CARTESIAN_POINT ( 'NONE',  ( -70.19499999999995055, 8.437984349512085203, -1.550032578732815448E-15 ) ) ;
#19663 = CARTESIAN_POINT ( 'NONE',  ( -75.00000000000000000, 9.298035018096992843, -6.651463925736444516 ) ) ;
#19664 = PRESENTATION_LAYER_ASSIGNMENT (  '', '', ( #33138 ) ) ;
#19665 = CARTESIAN_POINT ( 'NONE',  ( -56.45707362346616520, -9.058813317711329915, 2.943386871421371787 ) ) ;
#19666 = DIRECTION ( 'NONE',  ( 0.000000000000000000, 0.000000000000000000, 1.000000000000000000 ) ) ;
#19667 = COLOUR_RGB ( '', 0.40784314, 0.44705882, 0.49803922) ;
#19668 = ADVANCED_FACE ( 'NONE', ( #56412 ), #50124, .F. ) ;
#19669 = DIRECTION ( 'NONE',  ( 1.000000000000000000, 0.000000000000000000, 0.000000000000000000 ) ) ;
#19670 = ORIENTED_EDGE ( 'NONE', *, *, #36755, .F. ) ;
#19671 = CARTESIAN_POINT ( 'NONE',  ( -115.7929263765337993, -3.094860106618429807, 9.524999999999991473 ) ) ;
#19672 = CARTESIAN_POINT ( 'NONE',  ( -129.5949999999999989, 2.607480562269073321, 8.024999999999991473 ) ) ;
#19673 = DIRECTION ( 'NONE',  ( 0.000000000000000000, 0.000000000000000000, -1.000000000000000000 ) ) ;
#19674 = FILL_AREA_STYLE ('',( #7729 ) ) ;
#19675 = FACE_OUTER_BOUND ( 'NONE', #41938, .T. ) ;
#19676 =( NAMED_UNIT ( * ) SI_UNIT ( $, .STERADIAN. ) SOLID_ANGLE_UNIT ( ) );
#19677 = ORIENTED_EDGE ( 'NONE', *, *, #58239, .T. ) ;
#19678 = ORIENTED_EDGE ( 'NONE', *, *, #27629, .T. ) ;
#19679 = FILL_AREA_STYLE_COLOUR ( '', #46581 ) ;
#19680 =( GEOMETRIC_REPRESENTATION_CONTEXT ( 3 ) GLOBAL_UNCERTAINTY_ASSIGNED_CONTEXT ( ( #56747 ) ) GLOBAL_UNIT_ASSIGNED_CONTEXT ( ( #30334, #46599, #68705 ) ) REPRESENTATION_CONTEXT ( 'NONE', 'WORKASPACE' ) );
#19681 = AXIS2_PLACEMENT_3D ( 'NONE', #5181, #11156, #64640 ) ;
#19682 = DIRECTION ( 'NONE',  ( 0.000000000000000000, 0.000000000000000000, -1.000000000000000000 ) ) ;
#19683 = DIRECTION ( 'NONE',  ( 1.000000000000000000, 0.000000000000000000, 0.000000000000000000 ) ) ;
#19684 = SURFACE_STYLE_FILL_AREA ( #24956 ) ;
#19685 = DIRECTION ( 'NONE',  ( 0.000000000000000000, 0.000000000000000000, -1.000000000000000000 ) ) ;
#19686 = ORIENTED_EDGE ( 'NONE', *, *, #1954, .T. ) ;
#19687 = CARTESIAN_POINT ( 'NONE',  ( -127.2550000000000097, -4.716976649647092401, 6.492361379858946790 ) ) ;
#19689 = EDGE_CURVE ( 'NONE', #62580, #3143, #28260, .T. ) ;
#19688 = ORIENTED_EDGE ( 'NONE', *, *, #27279, .T. ) ;
#19690 = COLOUR_RGB ( '', 0.09019608, 0.27058824, 0.51372549) ;
#19691 = CARTESIAN_POINT ( 'NONE',  ( -119.3070736234661808, -10.01517768586948698, 6.132527647946031529E-16 ) ) ;
#19692 = ADVANCED_FACE ( 'NONE', ( #65583 ), #6837, .F. ) ;
#19693 = EDGE_LOOP ( 'NONE', ( #14599, #20063, #49852, #26184 ) ) ;
#19694 = DIRECTION ( 'NONE',  ( 0.000000000000000000, 0.000000000000000000, -1.000000000000000000 ) ) ;
#19695 = DIRECTION ( 'NONE',  ( 1.000000000000000000, 0.000000000000000000, 0.000000000000000000 ) ) ;
#19696 = VERTEX_POINT ( 'NONE', #68037 ) ;
#19697 = AXIS2_PLACEMENT_3D ( 'NONE', #542, #43234, #27658 ) ;
#19698 = CARTESIAN_POINT ( 'NONE',  ( 57.74999999999998579, 30.99999999999999289, 4.000000000000000000 ) ) ;
#19699 = CARTESIAN_POINT ( 'NONE',  ( -3.094860106618434248, 137.7950000000000159, 9.525000000000000355 ) ) ;
#19700 = SURFACE_STYLE_FILL_AREA ( #46843 ) ;
#19701 = ORIENTED_EDGE ( 'NONE', *, *, #12980, .T. ) ;
#19702 = DIRECTION ( 'NONE',  ( 0.000000000000000000, 0.000000000000000000, -1.000000000000000000 ) ) ;
#19704 = EDGE_CURVE ( 'NONE', #51470, #48074, #28361, .T. ) ;
#19703 = CARTESIAN_POINT ( 'NONE',  ( -5.598654528085808657, 150.7549999999999955, 7.705886871421373741 ) ) ;
#19705 = DIRECTION ( 'NONE',  ( -1.000000000000000000, 0.000000000000000000, 0.000000000000000000 ) ) ;
#19706 = SURFACE_STYLE_FILL_AREA ( #41897 ) ;
#19707 = EDGE_LOOP ( 'NONE', ( #39635, #11222, #42520, #24545 ) ) ;
#19708 = CARTESIAN_POINT ( 'NONE',  ( 8.437984349512095861, 113.1929263765338050, 1.550032578732817026E-15 ) ) ;
#19709 = CARTESIAN_POINT ( 'NONE',  ( 15.48999599679679662, 146.4999999999999716, 10.00000000000000000 ) ) ;
#19710 = FILL_AREA_STYLE_COLOUR ( '', #695 ) ;
#19711 = FILL_AREA_STYLE ('',( #46494 ) ) ;
#19712 = MECHANICAL_DESIGN_GEOMETRIC_PRESENTATION_REPRESENTATION (  '', ( #10727 ), #48936 ) ;
#19713 = DIRECTION ( 'NONE',  ( -0.000000000000000000, 0.000000000000000000, -1.000000000000000000 ) ) ;
#19714 = EDGE_LOOP ( 'NONE', ( #1969, #45870, #45114, #16720, #9242, #8654 ) ) ;
#19715 = AXIS2_PLACEMENT_3D ( 'NONE', #16294, #32776, #43718 ) ;
#19716 = CARTESIAN_POINT ( 'NONE',  ( -5.196152422706634688, -9.000000000000005329, 1.392304845413258052 ) ) ;
#19717 = EDGE_CURVE ( 'NONE', #4438, #2325, #25104, .T. ) ;
#19718 = ORIENTED_EDGE ( 'NONE', *, *, #46184, .T. ) ;
#19719 = CARTESIAN_POINT ( 'NONE',  ( -56.39292637653378648, 8.102448949553176405, 5.886773742842740909 ) ) ;
#19720 =( LENGTH_UNIT ( ) NAMED_UNIT ( * ) SI_UNIT ( .MILLI., .METRE. ) );
#19721 = DIRECTION ( 'NONE',  ( 0.000000000000000000, 0.000000000000000000, -1.000000000000000000 ) ) ;
#19722 = CARTESIAN_POINT ( 'NONE',  ( -150.9550000000000125, -7.632228543268599452, 2.479861379858951054 ) ) ;
#19723 = EDGE_LOOP ( 'NONE', ( #42717, #66095, #1767, #51398 ) ) ;
#19724 =( GEOMETRIC_REPRESENTATION_CONTEXT ( 3 ) GLOBAL_UNCERTAINTY_ASSIGNED_CONTEXT ( ( #46087 ) ) GLOBAL_UNIT_ASSIGNED_CONTEXT ( ( #61542, #9164, #3111 ) ) REPRESENTATION_CONTEXT ( 'NONE', 'WORKASPACE' ) );
#19725 = EDGE_CURVE ( 'NONE', #39381, #12255, #31327, .T. ) ;
#19726 = CARTESIAN_POINT ( 'NONE',  ( 30.99999999999998579, 0.000000000000000000, -72.00402776293822171 ) ) ;
#19727 = CARTESIAN_POINT ( 'NONE',  ( -71.50000000000000000, 14.49137674618942562, 7.500000000000000000 ) ) ;
#19728 = ORIENTED_EDGE ( 'NONE', *, *, #38026, .T. ) ;
#19729 = ORIENTED_EDGE ( 'NONE', *, *, #25487, .T. ) ;
#19730 = CARTESIAN_POINT ( 'NONE',  ( -70.87837837837835764, 13.70805908423323949, 10.00000000000000000 ) ) ;
#19731 = LINE ( 'NONE', #60625, #39010 ) ;
#19732 = CARTESIAN_POINT ( 'NONE',  ( -64.40499999999998693, -2.607480562269069768, 8.024999999999991473 ) ) ;
#19733 = ORIENTED_EDGE ( 'NONE', *, *, #9414, .T. ) ;
#19734 = CARTESIAN_POINT ( 'NONE',  ( -80.49999999999995737, 50.00000000000000000, 12.00000000000000000 ) ) ;
#19735 = CARTESIAN_POINT ( 'NONE',  ( -91.25707362346616947, 5.598654528085800663, -7.705886871421367523 ) ) ;
#19736 = DIRECTION ( 'NONE',  ( 0.000000000000000000, 0.000000000000000000, 1.000000000000000000 ) ) ;
#19737 = ORIENTED_EDGE ( 'NONE', *, *, #58859, .T. ) ;
#19738 = STYLED_ITEM ( 'NONE', ( #8671 ), #8539 ) ;
#19739 = CARTESIAN_POINT ( 'NONE',  ( -75.00000000000000000, 9.118333594695574362, -6.737587966311150645 ) ) ;
#19740 = LINE ( 'NONE', #25363, #21857 ) ;
#19742 = DIRECTION ( 'NONE',  ( -4.625929269271509580E-16, 0.000000000000000000, 1.000000000000000000 ) ) ;
#19741 = DIRECTION ( 'NONE',  ( -1.000000000000000000, -0.000000000000000000, -0.000000000000000000 ) ) ;
#19743 =( GEOMETRIC_REPRESENTATION_CONTEXT ( 3 ) GLOBAL_UNCERTAINTY_ASSIGNED_CONTEXT ( ( #69253 ) ) GLOBAL_UNIT_ASSIGNED_CONTEXT ( ( #40089, #62534, #50959 ) ) REPRESENTATION_CONTEXT ( 'NONE', 'WORKASPACE' ) );
#19744 = CARTESIAN_POINT ( 'NONE',  ( -3.094860106618432471, 145.5949999999999136, -9.525000000000000355 ) ) ;
#19745 = CARTESIAN_POINT ( 'NONE',  ( -94.04499999999998749, 7.632228543268600340, 2.479861379858949277 ) ) ;
#19746 = AXIS2_PLACEMENT_3D ( 'NONE', #63885, #53014, #47070 ) ;
#19747 = CIRCLE ( 'NONE', #64695, 1.000000000000000000 ) ;
#19748 = CYLINDRICAL_SURFACE ( 'NONE', #50554, 1.000000000000000888 ) ;
#19749 = EDGE_CURVE ( 'NONE', #54396, #1660, #17888, .T. ) ;
#19750 = CARTESIAN_POINT ( 'NONE',  ( -2.607480562269157254, 144.0929263765338249, -8.024999999999939959 ) ) ;
#19751 = EDGE_LOOP ( 'NONE', ( #29295, #46514, #44518, #2652 ) ) ;
#19752 = CARTESIAN_POINT ( 'NONE',  ( -145.6429263765338078, -5.598654528085801552, 7.705886871421367523 ) ) ;
#19753 = CARTESIAN_POINT ( 'NONE',  ( -160.9449999999999932, -9.827790563157499189E-16, -8.024999999999991473 ) ) ;
#19754 = AXIS2_PLACEMENT_3D ( 'NONE', #55237, #33114, #7061 ) ;
#19755 = CARTESIAN_POINT ( 'NONE',  ( 49.12162162162162105, 13.70805908423323238, 9.500000000000000000 ) ) ;
#19756 = AXIS2_PLACEMENT_3D ( 'NONE', #69623, #42593, #59763 ) ;
#19757 = COLOUR_RGB ( '', 0.09019608, 0.27058824, 0.51372549) ;
#19758 = FACE_OUTER_BOUND ( 'NONE', #35879, .T. ) ;
#19759 = DIRECTION ( 'NONE',  ( -0.000000000000000000, 1.000000000000000000, -0.000000000000000000 ) ) ;
#19760 = ORIENTED_EDGE ( 'NONE', *, *, #14128, .T. ) ;
#19761 = CARTESIAN_POINT ( 'NONE',  ( -2.607480562269073321, 129.0929263765338249, -8.025000000000000355 ) ) ;
#19762 = ORIENTED_EDGE ( 'NONE', *, *, #65536, .T. ) ;
#19763 = CIRCLE ( 'NONE', #14153, 0.2500000000000002220 ) ;
#19764 = DIRECTION ( 'NONE',  ( -0.000000000000000000, -0.000000000000000000, 1.000000000000000000 ) ) ;
#19765 = EDGE_CURVE ( 'NONE', #17222, #28040, #8905, .T. ) ;
#19766 = CARTESIAN_POINT ( 'NONE',  ( 60.00000000000000000, 115.4999999999999574, -10.50000000000000000 ) ) ;
#19767 = CARTESIAN_POINT ( 'NONE',  ( -45.00000000000000000, 7.768687147774683943, 7.000000000000000888 ) ) ;
#19768 = SPHERICAL_SURFACE ( 'NONE', #61772, 0.2500000000000000000 ) ;
#19769 = SURFACE_STYLE_USAGE ( .BOTH. , #9928 ) ;
#19770 = ORIENTED_EDGE ( 'NONE', *, *, #11086, .F. ) ;
#19771 = CARTESIAN_POINT ( 'NONE',  ( -159.0550000000000068, -9.827790563157499189E-16, -8.024999999999991473 ) ) ;
#19772 = ADVANCED_FACE ( 'NONE', ( #37453 ), #34099, .F. ) ;
#19773 = EDGE_CURVE ( 'NONE', #12357, #42679, #55557, .T. ) ;
#19774 = EDGE_LOOP ( 'NONE', ( #63790, #386, #52717 ) ) ;
#19775 = CARTESIAN_POINT ( 'NONE',  ( 9.827790563157511022E-16, 87.30187232391182306, -8.025000000000000355 ) ) ;
#19776 = DIRECTION ( 'NONE',  ( -0.000000000000000000, -1.000000000000000000, -0.000000000000000000 ) ) ;
#19777 = VERTEX_POINT ( 'NONE', #26797 ) ;
#19778 =( NAMED_UNIT ( * ) SI_UNIT ( $, .STERADIAN. ) SOLID_ANGLE_UNIT ( ) );
#19779 = CARTESIAN_POINT ( 'NONE',  ( 57.00000000000000000, 5.000000000000000000, -77.00402776293825013 ) ) ;
#19780 = CARTESIAN_POINT ( 'NONE',  ( -8.102448949553181734, 109.8949999999999818, -5.886773742842749790 ) ) ;
#19781 = PRESENTATION_LAYER_ASSIGNMENT (  '', '', ( #61349 ) ) ;
#19782 = VERTEX_POINT ( 'NONE', #7021 ) ;
#19783 = DIRECTION ( 'NONE',  ( -0.000000000000000000, -1.000000000000000000, 0.000000000000000000 ) ) ;
#19785 = EDGE_CURVE ( 'NONE', #24442, #28025, #37797, .T. ) ;
#19784 = CARTESIAN_POINT ( 'NONE',  ( -1.166476076187854022E-15, 118.0549999999999926, 9.525000000000000355 ) ) ;
#19786 = CARTESIAN_POINT ( 'NONE',  ( -76.85499999999998977, 4.716976649647094177, 6.492361379858945902 ) ) ;
#19787 = LINE ( 'NONE', #31027, #32942 ) ;
#19788 = PRODUCT_DEFINITION_SHAPE ( 'NONE', 'NONE',  #27444 ) ;
#19789 = B_SPLINE_CURVE_WITH_KNOTS ( 'NONE', 3,
 ( #52269, #62769, #4026, #48051, #57516, #42091 ),
 .UNSPECIFIED., .F., .F.,
 ( 4, 2, 4 ),
 ( 0.004189585287972442777, 0.006269578072783818512, 0.008349570857595195114 ),
 .UNSPECIFIED. ) ;
#19790 = ORIENTED_EDGE ( 'NONE', *, *, #68246, .F. ) ;
#19791 = CARTESIAN_POINT ( 'NONE',  ( 3.094860106618431583, 142.2050000000000125, 9.525000000000000355 ) ) ;
#19792 =( LENGTH_UNIT ( ) NAMED_UNIT ( * ) SI_UNIT ( .MILLI., .METRE. ) );
#19793 = ADVANCED_FACE ( 'NONE', ( #10998 ), #58503, .F. ) ;
#19794 = VECTOR ( 'NONE', #44680, 1000.000000000000114 ) ;
#19795 = CARTESIAN_POINT ( 'NONE',  ( 20.26325459587049238, 115.0245731144845394, 10.00000000000000000 ) ) ;
#19796 = DIRECTION ( 'NONE',  ( 1.000000000000000000, 0.000000000000000000, 0.000000000000000000 ) ) ;
#19797 = EDGE_LOOP ( 'NONE', ( #20194, #45525, #25456, #18629 ) ) ;
#19798 =( NAMED_UNIT ( * ) PLANE_ANGLE_UNIT ( ) SI_UNIT ( $, .RADIAN. ) );
#19799 = CARTESIAN_POINT ( 'NONE',  ( -69.50000000000000000, 50.00000000000000000, 12.00000000000000000 ) ) ;
#19800 = CARTESIAN_POINT ( 'NONE',  ( -178.7050000000000125, 2.607480562269073321, 8.024999999999991473 ) ) ;
#19801 = ORIENTED_EDGE ( 'NONE', *, *, #13865, .T. ) ;
#19802 =( BOUNDED_CURVE ( )  B_SPLINE_CURVE ( 2, ( #57993, #30882, #63596, #4478, #42889, #3778, #15440, #52380, #15102, #37258, #42528 ),
 .UNSPECIFIED., .F., .F. ) 
 B_SPLINE_CURVE_WITH_KNOTS ( ( 3, 2, 2, 2, 2, 3 ),
 ( 0.2173913043478209184, 0.2195652173912991389, 0.2217391304347773318, 0.2239130434782555801, 0.2260869565217337729, 0.2282608695652119657 ),
 .UNSPECIFIED. ) 
 CURVE ( )  GEOMETRIC_REPRESENTATION_ITEM ( )  RATIONAL_B_SPLINE_CURVE ( ( 1.000000000000116129, 0.9510565162950372908, 1.000000000000000000, 0.9510565162951535312, 1.000000000000000000, 0.9510565162951535312, 1.000000000000000000, 0.9510565162951535312, 1.000000000000000000, 0.9510565162952754337, 0.9999999999998780975 ) ) 
 REPRESENTATION_ITEM ( '' )  );
#19803 = CARTESIAN_POINT ( 'NONE',  ( 8.601545703395382603, 111.4306875064348503, 0.4166762051479315221 ) ) ;
#19804 = CARTESIAN_POINT ( 'NONE',  ( -86.84292637653381064, 9.058813317711329915, -2.943386871421373119 ) ) ;
#19805 = PRESENTATION_STYLE_ASSIGNMENT (( #40595 ) ) ;
#19806 = ORIENTED_EDGE ( 'NONE', *, *, #31873, .T. ) ;
#19807 = DIRECTION ( 'NONE',  ( 0.000000000000000000, -1.000000000000000000, 0.000000000000000000 ) ) ;
#19808 = ORIENTED_EDGE ( 'NONE', *, *, #60737, .F. ) ;
#19809 = DIRECTION ( 'NONE',  ( 1.000000000000000000, 0.000000000000000000, 0.000000000000000000 ) ) ;
#19810 = AXIS2_PLACEMENT_3D ( 'NONE', #38341, #64691, #22122 ) ;
#19811 = FILL_AREA_STYLE_COLOUR ( '', #33680 ) ;
#19812 = CARTESIAN_POINT ( 'NONE',  ( -101.6049999999999898, 6.826472737025113702, -4.959722759717902107 ) ) ;
#19813 = ORIENTED_EDGE ( 'NONE', *, *, #58070, .T. ) ;
#19814 = EDGE_CURVE ( 'NONE', #52933, #47797, #53829, .T. ) ;
#19815 =( GEOMETRIC_REPRESENTATION_CONTEXT ( 3 ) GLOBAL_UNCERTAINTY_ASSIGNED_CONTEXT ( ( #65127 ) ) GLOBAL_UNIT_ASSIGNED_CONTEXT ( ( #45550, #24046, #3228 ) ) REPRESENTATION_CONTEXT ( 'NONE', 'WORKASPACE' ) );
#19816 = CARTESIAN_POINT ( 'NONE',  ( -141.6570736234662036, 9.058813317711329915, 2.943386871421369566 ) ) ;
#19817 = EDGE_CURVE ( 'NONE', #24442, #28382, #7736, .T. ) ;
#19818 = CARTESIAN_POINT ( 'NONE',  ( -8.102448949553179958, 148.8950000000000102, -5.886773742842749790 ) ) ;
#19819 = CARTESIAN_POINT ( 'NONE',  ( -73.40707362346617515, 3.094860106618428031, -9.524999999999993250 ) ) ;
#19820 = CARTESIAN_POINT ( 'NONE',  ( -92.84292637653379643, 9.058813317711329915, -2.943386871421373119 ) ) ;
#19821 = ORIENTED_EDGE ( 'NONE', *, *, #20950, .F. ) ;
#19822 = CARTESIAN_POINT ( 'NONE',  ( -83.99999999999997158, 50.00000000000000000, 11.50000000000000000 ) ) ;
#19823 = CARTESIAN_POINT ( 'NONE',  ( -17.50859832773041447, -11.19035067480616874, 4.337450031442691589 ) ) ;
#19825 = CARTESIAN_POINT ( 'NONE',  ( -100.3429263765337964, -9.058813317711329915, 2.943386871421371787 ) ) ;
#19824 = DIRECTION ( 'NONE',  ( -1.000000000000000000, 0.000000000000000000, 0.000000000000000000 ) ) ;
#19826 = CARTESIAN_POINT ( 'NONE',  ( -123.5049999999999955, -6.826472737025115478, -4.959722759717899443 ) ) ;
#19827 = DIRECTION ( 'NONE',  ( 0.000000000000000000, -1.000000000000000000, 0.000000000000000000 ) ) ;
#19828 = CARTESIAN_POINT ( 'NONE',  ( 5.598654528085805993, 114.2449999999999903, 7.705886871421374629 ) ) ;
#19829 = CARTESIAN_POINT ( 'NONE',  ( -125.9949999999999903, -6.826472737025115478, 4.959722759717900331 ) ) ;
#19830 = CARTESIAN_POINT ( 'NONE',  ( -111.0570736234661808, 0.000000000000000000, 9.524999999999991473 ) ) ;
#19831 = ORIENTED_EDGE ( 'NONE', *, *, #35373, .F. ) ;
#19832 = SURFACE_SIDE_STYLE ('',( #25454 ) ) ;
#19833 = FILL_AREA_STYLE ('',( #55743 ) ) ;
#19834 = DIRECTION ( 'NONE',  ( -0.000000000000000000, -0.000000000000000000, -1.000000000000000000 ) ) ;
#19835 = CARTESIAN_POINT ( 'NONE',  ( -170.3929263765337794, 8.102448949553176405, 5.886773742842740909 ) ) ;
#19836 = SHAPE_REPRESENTATION_RELATIONSHIP ( 'NONE' , 'NONE' ,  #15001, #55567 ) ;
#19837 = SURFACE_STYLE_FILL_AREA ( #69422 ) ;
#19838 = EDGE_CURVE ( 'NONE', #55848, #33948, #55192, .T. ) ;
#19839 = AXIS2_PLACEMENT_3D ( 'NONE', #27807, #49311, #61235 ) ;
#19840 = DIRECTION ( 'NONE',  ( -1.000000000000000000, 0.000000000000000000, 0.000000000000000000 ) ) ;
#19841 = DIRECTION ( 'NONE',  ( 6.938893903907222067E-15, 0.000000000000000000, 1.000000000000000000 ) ) ;
#19842 = ORIENTED_EDGE ( 'NONE', *, *, #43771, .T. ) ;
#19843 = CARTESIAN_POINT ( 'NONE',  ( -86.99292637653378790, 8.102448949553171076, -5.886773742842744461 ) ) ;
#19844 = ITEM_DEFINED_TRANSFORMATION ( 'NONE', 'NONE', #29264,  #42840 ) ;
#19845 = SURFACE_SIDE_STYLE ('',( #8956 ) ) ;
#19846 = EDGE_CURVE ( 'NONE', #67406, #50331, #41150, .T. ) ;
#19847 = CARTESIAN_POINT ( 'NONE',  ( 27.00000000000001776, 15.00000000000000000, 34.49999999999998579 ) ) ;
#19848 = CARTESIAN_POINT ( 'NONE',  ( 2.607480562269075985, 123.9070736234661467, -8.025000000000000355 ) ) ;
#19849 = LINE ( 'NONE', #52920, #31409 ) ;
#19850 = CIRCLE ( 'NONE', #64755, 7.500000000000000000 ) ;
#19851 = CARTESIAN_POINT ( 'NONE',  ( -156.2070736234664992, 3.094860106624047091, 9.524999999995914735 ) ) ;
#19852 = ADVANCED_FACE ( 'NONE', ( #67859 ), #24572, .T. ) ;
#19853 = VERTEX_POINT ( 'NONE', #35838 ) ;
#19854 = DIRECTION ( 'NONE',  ( -0.000000000000000000, -1.000000000000000000, 0.000000000000000000 ) ) ;
#19855 = EDGE_LOOP ( 'NONE', ( #65090, #37079, #48128, #18225 ) ) ;
#19856 = CARTESIAN_POINT ( 'NONE',  ( -102.4429263765338050, -1.166476076187852838E-15, -9.524999999999991473 ) ) ;
#19857 = CARTESIAN_POINT ( 'NONE',  ( 8.000000000000000000, 0.000000000000000000, 72.00402776293825013 ) ) ;
#19858 = CARTESIAN_POINT ( 'NONE',  ( 2.607480562269076430, 135.9070736234661467, -8.025000000000000355 ) ) ;
#19859 = FILL_AREA_STYLE_COLOUR ( '', #32661 ) ;
#19860 = VERTEX_POINT ( 'NONE', #28806 ) ;
#19861 = SURFACE_STYLE_USAGE ( .BOTH. , #55770 ) ;
#19862 = CARTESIAN_POINT ( 'NONE',  ( -102.3549999999999898, -4.716976649647093289, -6.492361379858945902 ) ) ;
#19863 = ORIENTED_EDGE ( 'NONE', *, *, #36940, .T. ) ;
#19864 = CARTESIAN_POINT ( 'NONE',  ( 75.00000000000000000, 20.36037961002804053, -6.000000000000000000 ) ) ;
#19865 = EDGE_CURVE ( 'NONE', #49361, #61387, #45255, .T. ) ;
#19866 = CARTESIAN_POINT ( 'NONE',  ( -103.8570736234661780, -5.598654528085803328, -7.705886871421366635 ) ) ;
#19867 =( LENGTH_UNIT ( ) NAMED_UNIT ( * ) SI_UNIT ( .MILLI., .METRE. ) );
#19868 = ORIENTED_EDGE ( 'NONE', *, *, #53472, .F. ) ;
#19869 = CARTESIAN_POINT ( 'NONE',  ( -5.196152422706636465, -1.107695154586736175, -9.000000000000003553 ) ) ;
#19870 = CARTESIAN_POINT ( 'NONE',  ( -71.24499999999999034, -4.716976649647093289, -6.492361379858945902 ) ) ;
#19871 = ORIENTED_EDGE ( 'NONE', *, *, #14642, .F. ) ;
#19872 = DIRECTION ( 'NONE',  ( 0.6216216216216311485, 0.7833176619561784682, 0.000000000000000000 ) ) ;
#19873 = DIRECTION ( 'NONE',  ( 1.000000000000000000, 0.000000000000000000, 0.000000000000000000 ) ) ;
#19874 = UNCERTAINTY_MEASURE_WITH_UNIT (LENGTH_MEASURE( 1.000000000000000082E-05 ), #37048, 'distance_accuracy_value', 'NONE');
#19875 = ORIENTED_EDGE ( 'NONE', *, *, #49254, .F. ) ;
#19876 = DIRECTION ( 'NONE',  ( 0.000000000000000000, 1.000000000000000000, 0.000000000000000000 ) ) ;
#19877 =( GEOMETRIC_REPRESENTATION_CONTEXT ( 3 ) GLOBAL_UNCERTAINTY_ASSIGNED_CONTEXT ( ( #60066 ) ) GLOBAL_UNIT_ASSIGNED_CONTEXT ( ( #42293, #4934, #26033 ) ) REPRESENTATION_CONTEXT ( 'NONE', 'WORKASPACE' ) );
#19878 = PLANE ( 'NONE',  #4409 ) ;
#19879 = VERTEX_POINT ( 'NONE', #18274 ) ;
#19880 = SURFACE_SIDE_STYLE ('',( #15673 ) ) ;
#19881 = ORIENTED_EDGE ( 'NONE', *, *, #69082, .T. ) ;
#19882 = CARTESIAN_POINT ( 'NONE',  ( -138.4429263765337907, -1.166476076187852838E-15, -9.524999999999991473 ) ) ;
#19883 = FACE_OUTER_BOUND ( 'NONE', #12260, .T. ) ;
#19884 = CARTESIAN_POINT ( 'NONE',  ( -168.0570736234661808, 0.000000000000000000, 9.524999999999991473 ) ) ;
#19885 = ADVANCED_FACE ( 'NONE', ( #39760 ), #29514, .T. ) ;
#19886 = DIRECTION ( 'NONE',  ( -1.000000000000000000, 0.000000000000000000, 0.000000000000000000 ) ) ;
#19887 =( BOUNDED_CURVE ( )  B_SPLINE_CURVE ( 2, ( #10870, #58714, #58359, #41882, #47882, #10184, #48546, #63300, #48198, #15824, #4892 ),
 .UNSPECIFIED., .F., .F. ) 
 B_SPLINE_CURVE_WITH_KNOTS ( ( 3, 2, 2, 2, 2, 3 ),
 ( 0.3260869565217315302, 0.3282608695652097230, 0.3304347826086879159, 0.3326086956521662197, 0.3347826086956444125, 0.3369565217391226053 ),
 .UNSPECIFIED. ) 
 CURVE ( )  GEOMETRIC_REPRESENTATION_ITEM ( )  RATIONAL_B_SPLINE_CURVE ( ( 1.000000000000171196, 0.9510565162949823348, 1.000000000000000000, 0.9510565162951535312, 1.000000000000000000, 0.9510565162951535312, 1.000000000000000000, 0.9510565162951535312, 1.000000000000000000, 0.9510565162953297236, 0.9999999999998238076 ) ) 
 REPRESENTATION_ITEM ( '' )  );
#19888 = CARTESIAN_POINT ( 'NONE',  ( -101.4570736234661723, -9.058813317711329915, 2.943386871421371787 ) ) ;
#19889 = CARTESIAN_POINT ( 'NONE',  ( 4.716976649647099507, 113.6429263765338078, -6.492361379858953008 ) ) ;
#19890 = PRESENTATION_STYLE_ASSIGNMENT (( #57902 ) ) ;
#19891 = ORIENTED_EDGE ( 'NONE', *, *, #4252, .F. ) ;
#19892 = FACE_OUTER_BOUND ( 'NONE', #56235, .T. ) ;
#19893 = CARTESIAN_POINT ( 'NONE',  ( -105.6570736234661751, 9.058813317711329915, 2.943386871421369566 ) ) ;
#19895 = CARTESIAN_POINT ( 'NONE',  ( -24.00000000000000000, -2.250452076942884869E-15, 4.000000000000000000 ) ) ;
#19894 = CARTESIAN_POINT ( 'NONE',  ( 44.28021770739998431, 9.999999999999980460, 3.500000000000000000 ) ) ;
#19896 = DIRECTION ( 'NONE',  ( -1.000000000000000000, 0.000000000000000000, 0.000000000000000000 ) ) ;
#19897 = AXIS2_PLACEMENT_3D ( 'NONE', #57338, #29567, #51731 ) ;
#19898 = CARTESIAN_POINT ( 'NONE',  ( -147.0549999999999784, -9.827790563157499189E-16, -8.024999999999991473 ) ) ;
#19899 = DIRECTION ( 'NONE',  ( 1.000000000000000000, 0.000000000000000000, 0.000000000000000000 ) ) ;
#19900 =( NAMED_UNIT ( * ) SI_UNIT ( $, .STERADIAN. ) SOLID_ANGLE_UNIT ( ) );
#19901 = CARTESIAN_POINT ( 'NONE',  ( -157.6449999999999818, 4.716976649647091513, -6.492361379858946790 ) ) ;
#19902 = CARTESIAN_POINT ( 'NONE',  ( -149.9949999999999193, -6.826472737025113702, 4.959722759717902107 ) ) ;
#19903 = ORIENTED_EDGE ( 'NONE', *, *, #43278, .T. ) ;
#19904 = DIRECTION ( 'NONE',  ( 0.6216216216216311485, 0.7833176619561784682, 0.000000000000000000 ) ) ;
#19905 = CARTESIAN_POINT ( 'NONE',  ( 40.99999999999997868, 9.999999999999978684, 3.500000000000000000 ) ) ;
#19906 = SURFACE_SIDE_STYLE ('',( #31850 ) ) ;
#19907 = UNCERTAINTY_MEASURE_WITH_UNIT (LENGTH_MEASURE( 1.000000000000000082E-05 ), #5522, 'distance_accuracy_value', 'NONE');
#19908 = CARTESIAN_POINT ( 'NONE',  ( -60.05499999999998550, -9.827790563157499189E-16, -8.024999999999991473 ) ) ;
#19909 = DIRECTION ( 'NONE',  ( -0.000000000000000000, 0.000000000000000000, -1.000000000000000000 ) ) ;
#19910 = DIRECTION ( 'NONE',  ( -1.189524669241239115E-16, -1.000000000000000000, -0.000000000000000000 ) ) ;
#19911 = CARTESIAN_POINT ( 'NONE',  ( -60.44499999999998607, 0.000000000000000000, 8.024999999999991473 ) ) ;
#19912 = CARTESIAN_POINT ( 'NONE',  ( 3.094860106618435136, 158.4049999999999727, -9.525000000000000355 ) ) ;
#19913 = DIRECTION ( 'NONE',  ( -1.000000000000000000, 4.336808689941999001E-16, 0.000000000000000000 ) ) ;
#19914 = EDGE_CURVE ( 'NONE', #63360, #42940, #48613, .T. ) ;
#19915 = SURFACE_STYLE_FILL_AREA ( #9036 ) ;
#19916 = UNCERTAINTY_MEASURE_WITH_UNIT (LENGTH_MEASURE( 1.000000000000000082E-05 ), #35677, 'distance_accuracy_value', 'NONE');
#19917 = CARTESIAN_POINT ( 'NONE',  ( 16.00000000000006040, 33.38418848238413261, 102.4884788884474318 ) ) ;
#19918 = SPHERICAL_SURFACE ( 'NONE', #48451, 0.2500000000000000000 ) ;
#19919 = FILL_AREA_STYLE ('',( #46727 ) ) ;
#19920 = CARTESIAN_POINT ( 'NONE',  ( 22.00000000000002132, 42.47058823529412308, 74.11764705882352189 ) ) ;
#19921 = VECTOR ( 'NONE', #67121, 1000.000000000000000 ) ;
#19922 = PRESENTATION_LAYER_ASSIGNMENT (  '', '', ( #21092 ) ) ;
#19923 = DIRECTION ( 'NONE',  ( -0.000000000000000000, -0.000000000000000000, -1.000000000000000000 ) ) ;
#19924 = EDGE_CURVE ( 'NONE', #37240, #55900, #19288, .T. ) ;
#19925 = DIRECTION ( 'NONE',  ( -1.000000000000000000, -0.000000000000000000, -0.000000000000000000 ) ) ;
#19926 = CARTESIAN_POINT ( 'NONE',  ( 36.00000000000002132, 5.000000000000000000, -77.00402776293825013 ) ) ;
#19927 = CARTESIAN_POINT ( 'NONE',  ( -5.196152422706636465, -1.107695154586736175, -9.000000000000003553 ) ) ;
#19928 = VERTEX_POINT ( 'NONE', #56943 ) ;
#19929 = ORIENTED_EDGE ( 'NONE', *, *, #61932, .F. ) ;
#19930 = ADVANCED_FACE ( 'NONE', ( #8758 ), #26302, .T. ) ;
#19931 = CARTESIAN_POINT ( 'NONE',  ( 1.400957079523477589, -2.390838073347307802, -7.000000000000005329 ) ) ;
#19932 = EDGE_CURVE ( 'NONE', #44394, #42499, #36913, .T. ) ;
#19933 = CARTESIAN_POINT ( 'NONE',  ( -20.57648123223228254, 114.4999999999999574, 10.27659574468085069 ) ) ;
#19934 = CARTESIAN_POINT ( 'NONE',  ( 0.000000000000000000, 0.000000000000000000, 0.2499999999999924227 ) ) ;
#19935 = PRESENTATION_LAYER_ASSIGNMENT (  '', '', ( #51396 ) ) ;
#19936 = DIRECTION ( 'NONE',  ( 1.156482317317873451E-16, -1.000000000000000000, 0.000000000000000000 ) ) ;
#19937 = ORIENTED_EDGE ( 'NONE', *, *, #44120, .F. ) ;
#19938 = EDGE_LOOP ( 'NONE', ( #10895, #33215, #9178, #24433, #59255, #57963 ) ) ;
#19939 = DIRECTION ( 'NONE',  ( -0.000000000000000000, 1.000000000000000000, 0.000000000000000000 ) ) ;
#19941 = EDGE_CURVE ( 'NONE', #2274, #50919, #14209, .T. ) ;
#19940 = AXIS2_PLACEMENT_3D ( 'NONE', #38704, #39721, #28411 ) ;
#19942 = CARTESIAN_POINT ( 'NONE',  ( 48.00000000000000000, 13.41640786499872284, -7.500000000000000000 ) ) ;
#19943 = ORIENTED_EDGE ( 'NONE', *, *, #57839, .T. ) ;
#19944 = CARTESIAN_POINT ( 'NONE',  ( -8.102448949553181734, 123.0049999999999955, -5.886773742842749790 ) ) ;
#19945 = FACE_OUTER_BOUND ( 'NONE', #29699, .T. ) ;
#19946 = CARTESIAN_POINT ( 'NONE',  ( -106.0449999999999875, 7.632228543268600340, 2.479861379858949277 ) ) ;
#19947 = ORIENTED_EDGE ( 'NONE', *, *, #3300, .T. ) ;
#19948 = SURFACE_STYLE_USAGE ( .BOTH. , #41808 ) ;
#19949 = PRESENTATION_STYLE_ASSIGNMENT (( #30148 ) ) ;
#19950 = ORIENTED_EDGE ( 'NONE', *, *, #53672, .T. ) ;
#19951 = CARTESIAN_POINT ( 'NONE',  ( -6.826472737025120807, 150.3929263765338078, -4.959722759717907437 ) ) ;
#19952 = CARTESIAN_POINT ( 'NONE',  ( -12.16421356237309048, -4.000000000000000000, 18.58578643762690419 ) ) ;
#19953 = DIRECTION ( 'NONE',  ( -0.000000000000000000, -0.000000000000000000, -1.000000000000000000 ) ) ;
#19954 = CARTESIAN_POINT ( 'NONE',  ( 54.99999999999999289, 2.409368300552961372E-15, 6.999999999999988454 ) ) ;
#19955 = ORIENTED_EDGE ( 'NONE', *, *, #52459, .T. ) ;
#19956 =( NAMED_UNIT ( * ) PLANE_ANGLE_UNIT ( ) SI_UNIT ( $, .RADIAN. ) );
#19957 = ORIENTED_EDGE ( 'NONE', *, *, #22172, .F. ) ;
#19958 = CARTESIAN_POINT ( 'NONE',  ( 21.02379604162863558, 114.6409683457797115, 9.999999999999998224 ) ) ;
#19959 = SURFACE_STYLE_USAGE ( .BOTH. , #68181 ) ;
#19960 = CARTESIAN_POINT ( 'NONE',  ( -31.19338908182848513, -8.500000000001197265, 7.186868961050565829 ) ) ;
#19961 = CARTESIAN_POINT ( 'NONE',  ( -120.5049999999999812, -6.826472737025115478, -4.959722759717899443 ) ) ;
#19962 = CARTESIAN_POINT ( 'NONE',  ( -51.05707362346617373, 0.000000000000000000, 9.524999999999991473 ) ) ;
#19963 = MECHANICAL_DESIGN_GEOMETRIC_PRESENTATION_REPRESENTATION (  '', ( #6459 ), #33437 ) ;
#19964 = CARTESIAN_POINT ( 'NONE',  ( -74.14894044101720283, 9.184648417642964802, 6.276141209865989445 ) ) ;
#19965 = CARTESIAN_POINT ( 'NONE',  ( 24.21231517720798010, 112.9999999999999858, 7.500000000000000000 ) ) ;
#19966 = EDGE_LOOP ( 'NONE', ( #67790, #19375, #35539, #26008 ) ) ;
#19967 = VECTOR ( 'NONE', #8907, 1000.000000000000000 ) ;
#19968 = ORIENTED_EDGE ( 'NONE', *, *, #48720, .F. ) ;
#19969 = CARTESIAN_POINT ( 'NONE',  ( -17.75000000000000711, 31.24999999999999289, -3.750000000000000000 ) ) ;
#19970 = CARTESIAN_POINT ( 'NONE',  ( 4.716976649647096842, 113.8570736234661638, 6.492361379858953896 ) ) ;
#19971 = EDGE_LOOP ( 'NONE', ( #48584, #31259, #60905, #5469 ) ) ;
#19972 = SURFACE_STYLE_USAGE ( .BOTH. , #68194 ) ;
#19973 = CARTESIAN_POINT ( 'NONE',  ( -175.1050000000000182, -6.826472737025115478, 4.959722759717900331 ) ) ;
#19974 = DIRECTION ( 'NONE',  ( 0.000000000000000000, -0.1048768571002353378, -0.9944852160011111719 ) ) ;
#19975 = CARTESIAN_POINT ( 'NONE',  ( -50.75707362346618368, -5.598654528085801552, 7.705886871421367523 ) ) ;
#19976 = MECHANICAL_DESIGN_GEOMETRIC_PRESENTATION_REPRESENTATION (  '', ( #50332 ), #68311 ) ;
#19977 = CARTESIAN_POINT ( 'NONE',  ( -176.3949999999999818, -6.826472737025113702, -4.959722759717900331 ) ) ;
#19978 = DIRECTION ( 'NONE',  ( 0.000000000000000000, 1.000000000000000000, 0.000000000000000000 ) ) ;
#19979 = ORIENTED_EDGE ( 'NONE', *, *, #66213, .T. ) ;
#19980 = DIRECTION ( 'NONE',  ( 0.000000000000000000, 0.000000000000000000, 1.000000000000000000 ) ) ;
#19981 = CARTESIAN_POINT ( 'NONE',  ( -11.02915983529077337, 11.60772081924744015, -3.055653888425151177 ) ) ;
#19982 = CARTESIAN_POINT ( 'NONE',  ( -89.75499999999998124, 4.716976649647091513, -6.492361379858946790 ) ) ;
#19983 = CARTESIAN_POINT ( 'NONE',  ( 72.00000000000000000, 35.92875272052971525, 7.000000000000000000 ) ) ;
#19984 = DIRECTION ( 'NONE',  ( -0.000000000000000000, 1.000000000000000000, 0.000000000000000000 ) ) ;
#19985 = MECHANICAL_DESIGN_GEOMETRIC_PRESENTATION_REPRESENTATION (  '', ( #64927 ), #60404 ) ;
#19986 = CARTESIAN_POINT ( 'NONE',  ( -86.69499999999999318, -8.437984349512086979, 5.166775262442717831E-16 ) ) ;
#19987 = CARTESIAN_POINT ( 'NONE',  ( 3.094860106618435136, 125.4050000000000011, -9.525000000000000355 ) ) ;
#19988 = CARTESIAN_POINT ( 'NONE',  ( -65.99499999999996191, -6.826472737025115478, 4.959722759717900331 ) ) ;
#19989 = CARTESIAN_POINT ( 'NONE',  ( -74.99999999999998579, 50.00000000000000000, 9.500000000000000000 ) ) ;
#19990 = ADVANCED_FACE ( 'NONE', ( #42537 ), #48159, .T. ) ;
#19991 = CARTESIAN_POINT ( 'NONE',  ( 15.98999599679679839, 118.4999999999999716, -10.00000000000000000 ) ) ;
#19992 =( LENGTH_UNIT ( ) NAMED_UNIT ( * ) SI_UNIT ( .MILLI., .METRE. ) );
#19993 = UNCERTAINTY_MEASURE_WITH_UNIT (LENGTH_MEASURE( 1.000000000000000082E-05 ), #3942, 'distance_accuracy_value', 'NONE');
#19994 = EDGE_CURVE ( 'NONE', #25847, #5343, #4137, .T. ) ;
#19995 = FILL_AREA_STYLE_COLOUR ( '', #52812 ) ;
#19996 = EDGE_CURVE ( 'NONE', #6652, #25552, #21214, .T. ) ;
#19997 = VERTEX_POINT ( 'NONE', #25605 ) ;
#19998 = CARTESIAN_POINT ( 'NONE',  ( -105.8929263765337794, -8.102448949553172852, -5.886773742842741797 ) ) ;
#19999 = CARTESIAN_POINT ( 'NONE',  ( -125.3949999999999818, -6.826472737025115478, -4.959722759717899443 ) ) ;
#20000 = CARTESIAN_POINT ( 'NONE',  ( -2.607480562269158586, 146.4070736234661751, 8.024999999999939959 ) ) ;
#20001 = EDGE_CURVE ( 'NONE', #41724, #26112, #60523, .T. ) ;
#20002 = ADVANCED_FACE ( 'NONE', ( #11168 ), #43922, .F. ) ;
#20003 = SURFACE_STYLE_USAGE ( .BOTH. , #52412 ) ;
#20004 = ADVANCED_FACE ( 'NONE', ( #37961 ), #60386, .T. ) ;
#20006 = DIRECTION ( 'NONE',  ( -0.000000000000000000, 1.000000000000000000, 1.224646799147353207E-16 ) ) ;
#20005 = LINE ( 'NONE', #25978, #64479 ) ;
#20007 = SURFACE_STYLE_USAGE ( .BOTH. , #24950 ) ;
#20008 = ORIENTED_EDGE ( 'NONE', *, *, #10985, .F. ) ;
#20009 = CIRCLE ( 'NONE', #23382, 1.000000000000000888 ) ;
#20010 = ORIENTED_EDGE ( 'NONE', *, *, #35035, .T. ) ;
#20011 = CARTESIAN_POINT ( 'NONE',  ( -80.49999999999998579, 50.00000000000000000, 6.499999999999999112 ) ) ;
#20012 = CARTESIAN_POINT ( 'NONE',  ( 31.00000000000002132, 42.00000000000000711, 75.00000000000000000 ) ) ;
#20013 = UNCERTAINTY_MEASURE_WITH_UNIT (LENGTH_MEASURE( 1.000000000000000082E-05 ), #7308, 'distance_accuracy_value', 'NONE');
#20014 = ADVANCED_FACE ( 'NONE', ( #16497 ), #6933, .F. ) ;
#20015 = DIRECTION ( 'NONE',  ( 0.000000000000000000, 0.000000000000000000, 1.000000000000000000 ) ) ;
#20016 = CARTESIAN_POINT ( 'NONE',  ( 3.000000000000030198, 34.36176364315826248, 80.00402776293826435 ) ) ;
#20017 = STYLED_ITEM ( 'NONE', ( #12020 ), #50999 ) ;
#20018 = CARTESIAN_POINT ( 'NONE',  ( -47.50000000000000000, 99.99999999999992895, -9.500000000000000000 ) ) ;
#20019 = ORIENTED_EDGE ( 'NONE', *, *, #60264, .F. ) ;
#20020 = CARTESIAN_POINT ( 'NONE',  ( -119.7549999999999812, 4.716976649647091513, -6.492361379858946790 ) ) ;
#20021 = ORIENTED_EDGE ( 'NONE', *, *, #6491, .T. ) ;
#20022 =( NAMED_UNIT ( * ) SI_UNIT ( $, .STERADIAN. ) SOLID_ANGLE_UNIT ( ) );
#20023 = CARTESIAN_POINT ( 'NONE',  ( -125.6070736234661922, -8.102448949553172852, 5.886773742842742685 ) ) ;
#20024 = ORIENTED_EDGE ( 'NONE', *, *, #41194, .T. ) ;
#20025 = DIRECTION ( 'NONE',  ( -0.000000000000000000, -0.000000000000000000, 1.000000000000000000 ) ) ;
#20026 = VERTEX_POINT ( 'NONE', #54076 ) ;
#20027 = COLOUR_RGB ( '', 0.66274510, 0.83137255, 0.94901961) ;
#20028 = LINE ( 'NONE', #51721, #24174 ) ;
#20029 = CARTESIAN_POINT ( 'NONE',  ( -8.102448949553181734, 151.8950000000000102, -5.886773742842749790 ) ) ;
#20030 = PRESENTATION_LAYER_ASSIGNMENT (  '', '', ( #40299 ) ) ;
#20031 = ORIENTED_EDGE ( 'NONE', *, *, #47050, .T. ) ;
#20032 = DIRECTION ( 'NONE',  ( -0.000000000000000000, 0.000000000000000000, -1.000000000000000000 ) ) ;
#20033 = CARTESIAN_POINT ( 'NONE',  ( -3.094860106618434248, 153.9049999999999727, 9.525000000000000355 ) ) ;
#20034 = ORIENTED_EDGE ( 'NONE', *, *, #48539, .T. ) ;
#20035 = CARTESIAN_POINT ( 'NONE',  ( -7.632228543268607446, 114.5429263765338277, -2.479861379858953718 ) ) ;
#20036 = PRESENTATION_STYLE_ASSIGNMENT (( #61552 ) ) ;
#20037 = UNCERTAINTY_MEASURE_WITH_UNIT (LENGTH_MEASURE( 1.000000000000000082E-05 ), #52264, 'distance_accuracy_value', 'NONE');
#20038 = STYLED_ITEM ( 'NONE', ( #34774 ), #68155 ) ;
#20039 = CARTESIAN_POINT ( 'NONE',  ( -98.09292637653487645, 3.094860106636583286, 9.524999999986803800 ) ) ;
#20040 = CARTESIAN_POINT ( 'NONE',  ( -23.71231517720798010, 117.4999999999999716, 7.500000000000000000 ) ) ;
#20041 = CARTESIAN_POINT ( 'NONE',  ( 0.000000000000000000, 2.500000000000000000, 0.000000000000000000 ) ) ;
#20042 = EDGE_LOOP ( 'NONE', ( #64355, #20839, #46260, #66445 ) ) ;
#20043 = CARTESIAN_POINT ( 'NONE',  ( 28.58578643762692550, 34.36176364315826248, 80.00402776293826435 ) ) ;
#20044 = ORIENTED_EDGE ( 'NONE', *, *, #34625, .T. ) ;
#20045 = CARTESIAN_POINT ( 'NONE',  ( -55.49292637653380211, -8.102448949553172852, 5.886773742842742685 ) ) ;
#20046 = SURFACE_STYLE_USAGE ( .BOTH. , #30242 ) ;
#20047 = CARTESIAN_POINT ( 'NONE',  ( -155.4549999999999841, 7.632228543268599452, -2.479861379858951942 ) ) ;
#20048 = ORIENTED_EDGE ( 'NONE', *, *, #45575, .T. ) ;
#20049 = CYLINDRICAL_SURFACE ( 'NONE', #63232, 17.00000000000000000 ) ;
#20050 = UNCERTAINTY_MEASURE_WITH_UNIT (LENGTH_MEASURE( 1.000000000000000082E-05 ), #46675, 'distance_accuracy_value', 'NONE');
#20051 = EDGE_CURVE ( 'NONE', #66072, #39399, #27922, .T. ) ;
#20052 =( GEOMETRIC_REPRESENTATION_CONTEXT ( 3 ) GLOBAL_UNCERTAINTY_ASSIGNED_CONTEXT ( ( #4554 ) ) GLOBAL_UNIT_ASSIGNED_CONTEXT ( ( #42301, #69328, #26722 ) ) REPRESENTATION_CONTEXT ( 'NONE', 'WORKASPACE' ) );
#20053 = FACE_OUTER_BOUND ( 'NONE', #28230, .T. ) ;
#20054 = CARTESIAN_POINT ( 'NONE',  ( -51.84221223720477667, -9.947368421052630083, 4.481646853389225527 ) ) ;
#20055 = CARTESIAN_POINT ( 'NONE',  ( -69.44292637653380496, -1.166476076187852838E-15, -9.524999999999991473 ) ) ;
#20056 = CARTESIAN_POINT ( 'NONE',  ( 0.000000000000000000, 146.9429263765338192, -8.025000000000000355 ) ) ;
#20057 = ORIENTED_EDGE ( 'NONE', *, *, #66120, .T. ) ;
#20058 = EDGE_LOOP ( 'NONE', ( #56042, #65324, #66114, #55127 ) ) ;
#20059 = CARTESIAN_POINT ( 'NONE',  ( 22.84125995469108972, 24.77021312349235771, 27.27736960510218367 ) ) ;
#20060 = VECTOR ( 'NONE', #56134, 1000.000000000000000 ) ;
#20061 = FILL_AREA_STYLE ('',( #29589 ) ) ;
#20062 = CARTESIAN_POINT ( 'NONE',  ( -61.85499999999998266, 4.716976649647094177, 6.492361379858945902 ) ) ;
#20063 = ORIENTED_EDGE ( 'NONE', *, *, #45689, .F. ) ;
#20064 =( NAMED_UNIT ( * ) PLANE_ANGLE_UNIT ( ) SI_UNIT ( $, .RADIAN. ) );
#20065 = DIRECTION ( 'NONE',  ( 1.000000000000000000, 0.000000000000000000, -1.300977106640434891E-16 ) ) ;
#20066 = AXIS2_PLACEMENT_3D ( 'NONE', #37267, #58667, #62895 ) ;
#20067 = PRESENTATION_LAYER_ASSIGNMENT (  '', '', ( #50407 ) ) ;
#20068 = CARTESIAN_POINT ( 'NONE',  ( -124.7929263765345524, -3.094860106605926031, 9.525000000009075762 ) ) ;
#20069 = CARTESIAN_POINT ( 'NONE',  ( 9.250000000000003553, 27.74999999999998934, -3.750000000000000000 ) ) ;
#20070 = MECHANICAL_DESIGN_GEOMETRIC_PRESENTATION_REPRESENTATION (  '', ( #50410 ), #47080 ) ;
#20071 = ORIENTED_EDGE ( 'NONE', *, *, #60357, .T. ) ;
#20072 = CARTESIAN_POINT ( 'NONE',  ( -74.99999999999998579, 8.681192140609642394, -5.652915417256433983 ) ) ;
#20073 = DIRECTION ( 'NONE',  ( 0.000000000000000000, -1.000000000000000000, 0.000000000000000000 ) ) ;
#20074 = TOROIDAL_SURFACE ( 'NONE', #29040, 1.000000000000000000, 0.5000000000000000000 ) ;
#20075 = ADVANCED_FACE ( 'NONE', ( #54751 ), #11867, .T. ) ;
#20076 = CARTESIAN_POINT ( 'NONE',  ( -5.598654528085808657, 149.6450000000000102, 7.705886871421373741 ) ) ;
#20077 = CARTESIAN_POINT ( 'NONE',  ( -92.84499999999998465, -7.632228543268599452, 2.479861379858951054 ) ) ;
#20078 = DIRECTION ( 'NONE',  ( -0.000000000000000000, -1.000000000000000000, 0.000000000000000000 ) ) ;
#20079 = UNCERTAINTY_MEASURE_WITH_UNIT (LENGTH_MEASURE( 1.000000000000000082E-05 ), #41639, 'distance_accuracy_value', 'NONE');
#20080 = EDGE_CURVE ( 'NONE', #59688, #52874, #22064, .T. ) ;
#20081 = CARTESIAN_POINT ( 'NONE',  ( -71.99292637653380211, 8.102448949553172852, -5.886773742842744461 ) ) ;
#20082 = ORIENTED_EDGE ( 'NONE', *, *, #62254, .F. ) ;
#20083 = CARTESIAN_POINT ( 'NONE',  ( -132.4429263765338192, -1.166476076187852838E-15, -9.524999999999991473 ) ) ;
#20084 = SURFACE_SIDE_STYLE ('',( #53834 ) ) ;
#20085 = CARTESIAN_POINT ( 'NONE',  ( 36.00000000000002842, 5.000000000000000000, 29.00402776293825724 ) ) ;
#20086 = CARTESIAN_POINT ( 'NONE',  ( -161.0949999999999420, -2.607480562269071545, -8.024999999999991473 ) ) ;
#20087 = DIRECTION ( 'NONE',  ( -1.239088197126289584E-16, 0.000000000000000000, -1.000000000000000000 ) ) ;
#20088 = DIRECTION ( 'NONE',  ( 0.000000000000000000, 0.000000000000000000, -1.000000000000000000 ) ) ;
#20089 = ADVANCED_FACE ( 'NONE', ( #28008 ), #43720, .T. ) ;
#20090 = CARTESIAN_POINT ( 'NONE',  ( -132.7429263765338021, -5.598654528085803328, -7.705886871421366635 ) ) ;
#20091 = ORIENTED_EDGE ( 'NONE', *, *, #11050, .T. ) ;
#20092 = ORIENTED_EDGE ( 'NONE', *, *, #33674, .T. ) ;
#20093 = ADVANCED_FACE ( 'NONE', ( #44276 ), #18854, .T. ) ;
#20094 = CARTESIAN_POINT ( 'NONE',  ( -2.607480562269032909, 118.2929263765338135, 8.025000000000032330 ) ) ;
#20095 = FACE_OUTER_BOUND ( 'NONE', #69214, .T. ) ;
#20096 =( LENGTH_UNIT ( ) NAMED_UNIT ( * ) SI_UNIT ( .MILLI., .METRE. ) );
#20097 = AXIS2_PLACEMENT_3D ( 'NONE', #46697, #63168, #15005 ) ;
#20098 = ORIENTED_EDGE ( 'NONE', *, *, #16824, .F. ) ;
#20099 = CARTESIAN_POINT ( 'NONE',  ( -155.6049999999999329, 6.826472737025113702, -4.959722759717902107 ) ) ;
#20100 = ORIENTED_EDGE ( 'NONE', *, *, #53682, .T. ) ;
#20101 = CARTESIAN_POINT ( 'NONE',  ( 0.000000000000000000, 42.00000000000000000, -44.99999999999999289 ) ) ;
#20102 = CARTESIAN_POINT ( 'NONE',  ( 185.0000000000000000, 0.000000000000000000, 0.000000000000000000 ) ) ;
#20103 = ORIENTED_EDGE ( 'NONE', *, *, #48985, .T. ) ;
#20104 = AXIS2_PLACEMENT_3D ( 'NONE', #2914, #65946, #61348 ) ;
#20105 = CIRCLE ( 'NONE', #44916, 5.000000000000004441 ) ;
#20106 = LINE ( 'NONE', #63391, #42819 ) ;
#20107 = CARTESIAN_POINT ( 'NONE',  ( 22.00000000000002132, 50.00000000000000000, 46.00000000000000000 ) ) ;
#20108 = AXIS2_PLACEMENT_3D ( 'NONE', #64591, #22362, #818 ) ;
#20109 = CARTESIAN_POINT ( 'NONE',  ( -3.094860106618434248, 119.7949999999999733, 9.525000000000000355 ) ) ;
#20110 = ORIENTED_EDGE ( 'NONE', *, *, #41018, .F. ) ;
#20111 = CARTESIAN_POINT ( 'NONE',  ( -66.05707362346618083, 0.000000000000000000, 9.524999999999991473 ) ) ;
#20112 = CARTESIAN_POINT ( 'NONE',  ( -10.01517768586949408, 117.3049999999999784, -6.132527647946036459E-16 ) ) ;
#20113 = CARTESIAN_POINT ( 'NONE',  ( -69.50499999999996703, -6.826472737025113702, -4.959722759717900331 ) ) ;
#20114 = CARTESIAN_POINT ( 'NONE',  ( -81.05707362346618083, 0.000000000000000000, 9.524999999999991473 ) ) ;
#20115 = EDGE_LOOP ( 'NONE', ( #48275, #42459, #51044, #69294 ) ) ;
#20116 = CARTESIAN_POINT ( 'NONE',  ( -3.094860106618432471, 140.7049999999999557, -9.525000000000000355 ) ) ;
#20117 = UNCERTAINTY_MEASURE_WITH_UNIT (LENGTH_MEASURE( 1.000000000000000082E-05 ), #9395, 'distance_accuracy_value', 'NONE');
#20118 = FILL_AREA_STYLE_COLOUR ( '', #46668 ) ;
#20119 = CARTESIAN_POINT ( 'NONE',  ( 6.000000000000017764, 43.00000000000000000, 29.49447654986459710 ) ) ;
#20120 = CARTESIAN_POINT ( 'NONE',  ( -34.99999999999999289, 99.99999999999998579, 7.500000000000000000 ) ) ;
#20121 = CARTESIAN_POINT ( 'NONE',  ( 3.414213562373098032, 42.99999999999999289, -79.58981420056515788 ) ) ;
#20122 = ORIENTED_EDGE ( 'NONE', *, *, #9938, .T. ) ;
#20123 = AXIS2_PLACEMENT_3D ( 'NONE', #63438, #16661, #16321 ) ;
#20124 = LINE ( 'NONE', #29746, #36764 ) ;
#20125 = DIRECTION ( 'NONE',  ( 0.000000000000000000, 0.000000000000000000, 1.000000000000000000 ) ) ;
#20126 = LINE ( 'NONE', #25421, #62071 ) ;
#20127 = CARTESIAN_POINT ( 'NONE',  ( -46.79499999999996618, 2.607480562269068880, -8.024999999999993250 ) ) ;
#20128 = VERTEX_POINT ( 'NONE', #24830 ) ;
#20129 = CARTESIAN_POINT ( 'NONE',  ( 6.780819373525680760, 111.6853910234447369, -4.862369566202438875 ) ) ;
#20130 = PRESENTATION_LAYER_ASSIGNMENT (  '', '', ( #61642 ) ) ;
#20131 = ADVANCED_FACE ( 'NONE', ( #28721 ), #29782, .T. ) ;
#20132 =( NAMED_UNIT ( * ) PLANE_ANGLE_UNIT ( ) SI_UNIT ( $, .RADIAN. ) );
#20133 = ORIENTED_EDGE ( 'NONE', *, *, #55015, .F. ) ;
#20134 = CARTESIAN_POINT ( 'NONE',  ( 60.00000000000000000, 1.797044900979284448E-15, 11.50000000000000000 ) ) ;
#20135 = PRESENTATION_STYLE_ASSIGNMENT (( #69393 ) ) ;
#20136 = ORIENTED_EDGE ( 'NONE', *, *, #37448, .F. ) ;
#20137 = STYLED_ITEM ( 'NONE', ( #41317 ), #68959 ) ;
#20138 = CARTESIAN_POINT ( 'NONE',  ( 7.400000000000003908, 11.99999999999999289, 4.000000000000000000 ) ) ;
#20139 = DIRECTION ( 'NONE',  ( 0.000000000000000000, 1.000000000000000000, 0.000000000000000000 ) ) ;
#20140 = CARTESIAN_POINT ( 'NONE',  ( -94.25499999999999545, -4.716976649647092401, 6.492361379858946790 ) ) ;
#20141 = ORIENTED_EDGE ( 'NONE', *, *, #57202, .F. ) ;
#20142 = CARTESIAN_POINT ( 'NONE',  ( 3.999798566743339556, 8.867945265733707672, -2.000000000000000000 ) ) ;
#20143 = CARTESIAN_POINT ( 'NONE',  ( -74.50000000000000000, 7.768687147774688384, -6.500000000000000000 ) ) ;
#20144 = CARTESIAN_POINT ( 'NONE',  ( -132.8070736234661808, 10.01517768586948698, -1.839758294383808571E-15 ) ) ;
#20145 =( GEOMETRIC_REPRESENTATION_CONTEXT ( 3 ) GLOBAL_UNCERTAINTY_ASSIGNED_CONTEXT ( ( #53028 ) ) GLOBAL_UNIT_ASSIGNED_CONTEXT ( ( #57161, #3670, #2243 ) ) REPRESENTATION_CONTEXT ( 'NONE', 'WORKASPACE' ) );
#20146 = TOROIDAL_SURFACE ( 'NONE', #59453, 17.00000000000000355, 1.000000000000000000 ) ;
#20147 = CARTESIAN_POINT ( 'NONE',  ( -1.166476076187854022E-15, 149.9449999999999932, 9.525000000000000355 ) ) ;
#20148 = CARTESIAN_POINT ( 'NONE',  ( -72.65707362346617515, 9.058813317711329915, 2.943386871421369566 ) ) ;
#20149 = PRODUCT_RELATED_PRODUCT_CATEGORY ( 'part', '', ( #64784 ) ) ;
#20150 = EDGE_CURVE ( 'NONE', #61901, #7256, #40710, .T. ) ;
#20151 = VECTOR ( 'NONE', #40984, 1000.000000000000000 ) ;
#20152 = DIRECTION ( 'NONE',  ( -1.000000000000000000, 0.000000000000000000, 0.000000000000000000 ) ) ;
#20153 = ORIENTED_EDGE ( 'NONE', *, *, #56873, .F. ) ;
#20154 = FACE_OUTER_BOUND ( 'NONE', #55251, .T. ) ;
#20155 = CARTESIAN_POINT ( 'NONE',  ( -19.73763835060324823, -11.89250300617436551, 1.631536037870932043 ) ) ;
#20156 = CARTESIAN_POINT ( 'NONE',  ( -7.441974819423173848, 2.003239292658529180, 1.110121504110835877 ) ) ;
#20157 = MECHANICAL_DESIGN_GEOMETRIC_PRESENTATION_REPRESENTATION (  '', ( #43807 ), #49405 ) ;
#20158 = ADVANCED_FACE ( 'NONE', ( #55471 ), #45305, .T. ) ;
#20159 = CARTESIAN_POINT ( 'NONE',  ( -107.6049999999999756, 6.826472737025113702, -4.959722759717902107 ) ) ;
#20160 = EDGE_CURVE ( 'NONE', #58710, #51275, #29235, .T. ) ;
#20161 = DIRECTION ( 'NONE',  ( -1.000000000000000000, -0.000000000000000000, -0.000000000000000000 ) ) ;
#20162 = CARTESIAN_POINT ( 'NONE',  ( 9.058813317711338797, 123.8449999999999847, -2.943386871421372675 ) ) ;
#20163 = CARTESIAN_POINT ( 'NONE',  ( -126.2950000000000017, -2.607480562269069768, 8.024999999999991473 ) ) ;
#20164 = AXIS2_PLACEMENT_3D ( 'NONE', #2765, #14061, #40129 ) ;
#20165 = CARTESIAN_POINT ( 'NONE',  ( -111.6570736234661751, 9.058813317711329915, 2.943386871421369566 ) ) ;
#20166 = MECHANICAL_DESIGN_GEOMETRIC_PRESENTATION_REPRESENTATION (  '', ( #25794 ), #20216 ) ;
#20167 = CIRCLE ( 'NONE', #27973, 1.000000000000000888 ) ;
#20168 = LINE ( 'NONE', #63090, #43813 ) ;
#20169 = VECTOR ( 'NONE', #7146, 1000.000000000000114 ) ;
#20170 = PRESENTATION_STYLE_ASSIGNMENT (( #14560 ) ) ;
#20171 = EDGE_CURVE ( 'NONE', #17220, #26318, #10046, .T. ) ;
#20172 = VERTEX_POINT ( 'NONE', #67407 ) ;
#20173 = CYLINDRICAL_SURFACE ( 'NONE', #67614, 9.524999999999991473 ) ;
#20174 = CIRCLE ( 'NONE', #57225, 0.2500000000000002220 ) ;
#20175 = CARTESIAN_POINT ( 'NONE',  ( -176.3929263765338078, 8.102448949553176405, 5.886773742842740909 ) ) ;
#20176 = EDGE_CURVE ( 'NONE', #17419, #55126, #38138, .T. ) ;
#20177 = DIRECTION ( 'NONE',  ( 0.000000000000000000, 1.000000000000000000, 0.000000000000000000 ) ) ;
#20178 = EDGE_CURVE ( 'NONE', #27375, #27464, #20939, .T. ) ;
#20179 = CARTESIAN_POINT ( 'NONE',  ( -20.99077900071323199, 114.7777241159145518, -10.00000000000000000 ) ) ;
#20180 = CARTESIAN_POINT ( 'NONE',  ( 48.25000000000000000, 21.74999999999998579, -4.000000000000000000 ) ) ;
#20181 = ORIENTED_EDGE ( 'NONE', *, *, #52972, .T. ) ;
#20182 = CARTESIAN_POINT ( 'NONE',  ( -81.14292637653380780, 5.598654528085800663, -7.705886871421367523 ) ) ;
#20183 = ITEM_DEFINED_TRANSFORMATION ( 'NONE', 'NONE', #49587,  #42840 ) ;
#20184 = CARTESIAN_POINT ( 'NONE',  ( -71.50000000000000000, 14.49137674618942562, -7.000000000000000000 ) ) ;
#20185 = DIRECTION ( 'NONE',  ( 0.000000000000000000, -1.000000000000000000, 0.000000000000000000 ) ) ;
#20186 = EDGE_CURVE ( 'NONE', #44405, #13586, #66199, .T. ) ;
#20187 = FACE_OUTER_BOUND ( 'NONE', #64015, .T. ) ;
#20188 =( NAMED_UNIT ( * ) SI_UNIT ( $, .STERADIAN. ) SOLID_ANGLE_UNIT ( ) );
#20189 = CYLINDRICAL_SURFACE ( 'NONE', #68487, 8.025000000000000355 ) ;
#20190 = CARTESIAN_POINT ( 'NONE',  ( -157.5570736234661808, -1.166476076187852838E-15, -9.524999999999991473 ) ) ;
#20191 = VERTEX_POINT ( 'NONE', #50892 ) ;
#20192 = CARTESIAN_POINT ( 'NONE',  ( -135.7429263765338021, -5.598654528085803328, -7.705886871421366635 ) ) ;
#20193 = DIRECTION ( 'NONE',  ( -0.000000000000000000, -0.000000000000000000, -1.000000000000000000 ) ) ;
#20194 = ORIENTED_EDGE ( 'NONE', *, *, #68767, .T. ) ;
#20195 =( NAMED_UNIT ( * ) SI_UNIT ( $, .STERADIAN. ) SOLID_ANGLE_UNIT ( ) );
#20196 = STYLED_ITEM ( 'NONE', ( #16381 ), #1450 ) ;
#20197 = AXIS2_PLACEMENT_3D ( 'NONE', #6635, #45030, #2722 ) ;
#20198 =( BOUNDED_CURVE ( )  B_SPLINE_CURVE ( 2, ( #41340, #52242, #57486, #32138, #57851, #31785, #36431, #15994, #31086, #63794, #9315 ),
 .UNSPECIFIED., .F., .F. ) 
 B_SPLINE_CURVE_WITH_KNOTS ( ( 3, 2, 2, 2, 2, 3 ),
 ( 0.1304347826086926510, 0.1326086956521708715, 0.1347826086956490643, 0.1369565217391272849, 0.1391304347826055055, 0.1413043478260836983 ),
 .UNSPECIFIED. ) 
 CURVE ( )  GEOMETRIC_REPRESENTATION_ITEM ( )  RATIONAL_B_SPLINE_CURVE ( ( 1.000000000000067502, 0.9510565162950860296, 1.000000000000000000, 0.9510565162951535312, 1.000000000000000000, 0.9510565162951535312, 1.000000000000000000, 0.9510565162951535312, 1.000000000000000000, 0.9510565162952266949, 0.9999999999999268363 ) ) 
 REPRESENTATION_ITEM ( '' )  );
#20199 = CARTESIAN_POINT ( 'NONE',  ( 23.50000000000001776, 15.00000000000000000, 29.68999999999999417 ) ) ;
#20200 = CARTESIAN_POINT ( 'NONE',  ( 4.716976649647096842, 134.8570736234661638, 6.492361379858953896 ) ) ;
#20201 = DIRECTION ( 'NONE',  ( 0.000000000000000000, 0.000000000000000000, -1.000000000000000000 ) ) ;
#20202 = ORIENTED_EDGE ( 'NONE', *, *, #58785, .F. ) ;
#20203 = DIRECTION ( 'NONE',  ( -0.000000000000000000, 1.000000000000000000, -0.000000000000000000 ) ) ;
#20204 = CARTESIAN_POINT ( 'NONE',  ( -99.95499999999998408, -7.632228543268599452, 2.479861379858951054 ) ) ;
#20205 = UNCERTAINTY_MEASURE_WITH_UNIT (LENGTH_MEASURE( 1.000000000000000082E-05 ), #22211, 'distance_accuracy_value', 'NONE');
#20206 = DIRECTION ( 'NONE',  ( 1.000000000000000000, 0.000000000000000000, 0.000000000000000000 ) ) ;
#20207 = ORIENTED_EDGE ( 'NONE', *, *, #10585, .F. ) ;
#20208 = CARTESIAN_POINT ( 'NONE',  ( 35.99999999999999289, 5.000000000000000000, -37.00402776293825724 ) ) ;
#20209 = CARTESIAN_POINT ( 'NONE',  ( 12.00000000000001776, 15.00000000000000000, -60.00402776293827145 ) ) ;
#20210 = CARTESIAN_POINT ( 'NONE',  ( 8.082903768654761123, 1.417096231345241097, 9.294316082458970795E-16 ) ) ;
#20211 =( GEOMETRIC_REPRESENTATION_CONTEXT ( 3 ) GLOBAL_UNCERTAINTY_ASSIGNED_CONTEXT ( ( #53942 ) ) GLOBAL_UNIT_ASSIGNED_CONTEXT ( ( #29352, #61366, #7908 ) ) REPRESENTATION_CONTEXT ( 'NONE', 'WORKASPACE' ) );
#20212 = CIRCLE ( 'NONE', #1066, 5.000000000000004441 ) ;
#20213 = ORIENTED_EDGE ( 'NONE', *, *, #66636, .T. ) ;
#20214 = CARTESIAN_POINT ( 'NONE',  ( 44.99999999999977973, 149.4999999999999716, -10.00000000000000000 ) ) ;
#20215 = CARTESIAN_POINT ( 'NONE',  ( -68.24499999999999034, -4.716976649647093289, -6.492361379858945902 ) ) ;
#20217 = ORIENTED_EDGE ( 'NONE', *, *, #47839, .T. ) ;
#20216 =( GEOMETRIC_REPRESENTATION_CONTEXT ( 3 ) GLOBAL_UNCERTAINTY_ASSIGNED_CONTEXT ( ( #37767 ) ) GLOBAL_UNIT_ASSIGNED_CONTEXT ( ( #39524, #49713, #65884 ) ) REPRESENTATION_CONTEXT ( 'NONE', 'WORKASPACE' ) );
#20218 = SURFACE_STYLE_FILL_AREA ( #68094 ) ;
#20219 = CARTESIAN_POINT ( 'NONE',  ( 23.21231517720797655, 117.9999999999999716, 10.00000000000000000 ) ) ;
#20220 = DIRECTION ( 'NONE',  ( -1.000000000000000000, 0.000000000000000000, 0.000000000000000000 ) ) ;
#20221 = AXIS2_PLACEMENT_3D ( 'NONE', #44635, #66379, #45672 ) ;
#20222 = ORIENTED_EDGE ( 'NONE', *, *, #6663, .T. ) ;
#20223 = LINE ( 'NONE', #9706, #67370 ) ;
#20224 = DIRECTION ( 'NONE',  ( 0.000000000000000000, 1.000000000000000000, -0.000000000000000000 ) ) ;
#20225 = VECTOR ( 'NONE', #15039, 1000.000000000000000 ) ;
#20226 = DIRECTION ( 'NONE',  ( 0.000000000000000000, 1.000000000000000000, 0.000000000000000000 ) ) ;
#20227 = DIRECTION ( 'NONE',  ( 1.000000000000000000, 0.000000000000000000, 0.000000000000000000 ) ) ;
#20228 = ORIENTED_EDGE ( 'NONE', *, *, #12369, .F. ) ;
#20229 = DIRECTION ( 'NONE',  ( 0.000000000000000000, 0.000000000000000000, 1.000000000000000000 ) ) ;
#20230 = TOROIDAL_SURFACE ( 'NONE', #7884, 4.750000000000000000, 0.2500000000000000000 ) ;
#20231 = ORIENTED_EDGE ( 'NONE', *, *, #45843, .F. ) ;
#20232 = CARTESIAN_POINT ( 'NONE',  ( -195.0000000000000000, 1.166476076187852838E-15, -9.524999999999991473 ) ) ;
#20234 = VECTOR ( 'NONE', #19984, 1000.000000000000000 ) ;
#20233 = DIRECTION ( 'NONE',  ( -1.000000000000000000, -0.000000000000000000, -0.000000000000000000 ) ) ;
#20235 = CARTESIAN_POINT ( 'NONE',  ( -171.5070736234661979, 8.102448949553176405, 5.886773742842740909 ) ) ;
#20236 =( GEOMETRIC_REPRESENTATION_CONTEXT ( 3 ) GLOBAL_UNCERTAINTY_ASSIGNED_CONTEXT ( ( #41179 ) ) GLOBAL_UNIT_ASSIGNED_CONTEXT ( ( #12292, #44719, #16924 ) ) REPRESENTATION_CONTEXT ( 'NONE', 'WORKASPACE' ) );
#20237 = CARTESIAN_POINT ( 'NONE',  ( -5.598654528085806881, 124.7449999999999903, -7.705886871421374629 ) ) ;
#20238 = CARTESIAN_POINT ( 'NONE',  ( -103.7070736234661865, -3.094860106618431139, -9.524999999999991473 ) ) ;
#20239 = EDGE_CURVE ( 'NONE', #35855, #68529, #47042, .T. ) ;
#20240 = FILL_AREA_STYLE_COLOUR ( '', #62158 ) ;
#20241 = SURFACE_SIDE_STYLE ('',( #30093 ) ) ;
#20242 = ORIENTED_EDGE ( 'NONE', *, *, #21529, .F. ) ;
#20243 = CIRCLE ( 'NONE', #52865, 15.00000000000000000 ) ;
#20244 = PRESENTATION_STYLE_ASSIGNMENT (( #68447 ) ) ;
#20246 = DIRECTION ( 'NONE',  ( 1.000000000000000000, 0.000000000000000000, 0.000000000000000000 ) ) ;
#20245 = LINE ( 'NONE', #53643, #15551 ) ;
#20247 =( NAMED_UNIT ( * ) PLANE_ANGLE_UNIT ( ) SI_UNIT ( $, .RADIAN. ) );
#20248 = EDGE_CURVE ( 'NONE', #18094, #40178, #25528, .T. ) ;
#20249 = CARTESIAN_POINT ( 'NONE',  ( -152.1549999999999727, 7.632228543268600340, 2.479861379858949277 ) ) ;
#20250 = CARTESIAN_POINT ( 'NONE',  ( 23.21231517720797655, 117.4999999999999716, 7.000000000000000000 ) ) ;
#20251 = CARTESIAN_POINT ( 'NONE',  ( -148.4929263765337737, -8.102448949553174629, 5.886773742842742685 ) ) ;
#20252 = CARTESIAN_POINT ( 'NONE',  ( -158.6949999999999648, -8.437984349512085203, 5.166775262442717831E-16 ) ) ;
#20253 = CARTESIAN_POINT ( 'NONE',  ( -149.8449999999999989, -7.632228543268599452, 2.479861379858951054 ) ) ;
#20254 = ORIENTED_EDGE ( 'NONE', *, *, #25372, .T. ) ;
#20255 = DIRECTION ( 'NONE',  ( 0.000000000000000000, 0.000000000000000000, -1.000000000000000000 ) ) ;
#20256 = CARTESIAN_POINT ( 'NONE',  ( -71.49999999999998579, 50.00000000000000000, 7.000000000000000000 ) ) ;
#20257 = FACE_OUTER_BOUND ( 'NONE', #12846, .T. ) ;
#20258 = CARTESIAN_POINT ( 'NONE',  ( -65.90499999999998693, 2.607480562269068880, -8.024999999999993250 ) ) ;
#20259 = CARTESIAN_POINT ( 'NONE',  ( 13.75000000000000355, 28.24999999999998934, -4.000000000000000000 ) ) ;
#20260 = EDGE_CURVE ( 'NONE', #30333, #23187, #25921, .T. ) ;
#20261 = CARTESIAN_POINT ( 'NONE',  ( -59.09499999999997044, -2.607480562269071545, -8.024999999999991473 ) ) ;
#20262 = CARTESIAN_POINT ( 'NONE',  ( 5.598654528085805993, 157.3549999999999898, 7.705886871421374629 ) ) ;
#20263 = CARTESIAN_POINT ( 'NONE',  ( 3.414213562373125121, 34.36176364315826248, 80.00402776293826435 ) ) ;
#20264 = DIRECTION ( 'NONE',  ( -0.000000000000000000, -0.000000000000000000, 1.000000000000000000 ) ) ;
#20265 = AXIS2_PLACEMENT_3D ( 'NONE', #10855, #1881, #38930 ) ;
#20266 = CIRCLE ( 'NONE', #38241, 0.5000000000000004441 ) ;
#20267 = FILL_AREA_STYLE ('',( #68469 ) ) ;
#20268 = DIRECTION ( 'NONE',  ( 1.000000000000000000, 5.775339657480442461E-17, -4.528264053928433241E-17 ) ) ;
#20269 = PRESENTATION_STYLE_ASSIGNMENT (( #4073 ) ) ;
#20270 = MECHANICAL_DESIGN_GEOMETRIC_PRESENTATION_REPRESENTATION (  '', ( #41660 ), #62948 ) ;
#20271 = FACE_OUTER_BOUND ( 'NONE', #46459, .T. ) ;
#20272 = CARTESIAN_POINT ( 'NONE',  ( -49.94292637653380496, 0.000000000000000000, 9.524999999999991473 ) ) ;
#20273 = MECHANICAL_DESIGN_GEOMETRIC_PRESENTATION_REPRESENTATION (  '', ( #67477 ), #65216 ) ;
#20274 = LINE ( 'NONE', #56520, #12424 ) ;
#20275 = EDGE_CURVE ( 'NONE', #16380, #26318, #42663, .T. ) ;
#20276 = MECHANICAL_DESIGN_GEOMETRIC_PRESENTATION_REPRESENTATION (  '', ( #28134 ), #50625 ) ;
#20277 = DIRECTION ( 'NONE',  ( 0.000000000000000000, 0.000000000000000000, 1.000000000000000000 ) ) ;
#20278 = DIRECTION ( 'NONE',  ( 0.000000000000000000, 0.000000000000000000, -1.000000000000000000 ) ) ;
#20279 = CARTESIAN_POINT ( 'NONE',  ( -15.48999599679678951, 146.9999999999999716, -9.500000000000000000 ) ) ;
#20280 = VERTEX_POINT ( 'NONE', #14651 ) ;
#20281 = ORIENTED_EDGE ( 'NONE', *, *, #61298, .T. ) ;
#20282 = FILL_AREA_STYLE_COLOUR ( '', #58824 ) ;
#20283 = EDGE_CURVE ( 'NONE', #64812, #7926, #22378, .T. ) ;
#20284 = AXIS2_PLACEMENT_3D ( 'NONE', #42910, #41860, #25969 ) ;
#20285 = CARTESIAN_POINT ( 'NONE',  ( 4.041451884327379673, -7.000000000000002665, 1.082903768654758903 ) ) ;
#20286 = FACE_OUTER_BOUND ( 'NONE', #45062, .T. ) ;
#20287 = VERTEX_POINT ( 'NONE', #57917 ) ;
#20288 = ORIENTED_EDGE ( 'NONE', *, *, #37950, .F. ) ;
#20289 = DIRECTION ( 'NONE',  ( 0.000000000000000000, 0.000000000000000000, -1.000000000000000000 ) ) ;
#20290 = SURFACE_STYLE_USAGE ( .BOTH. , #57953 ) ;
#20291 = SURFACE_STYLE_USAGE ( .BOTH. , #39458 ) ;
#20292 = ORIENTED_EDGE ( 'NONE', *, *, #69051, .T. ) ;
#20293 = CARTESIAN_POINT ( 'NONE',  ( -9.058813317711338797, 114.4549999999999841, 2.943386871421373563 ) ) ;
#20294 = CARTESIAN_POINT ( 'NONE',  ( 45.00000000000000000, 10.69371294336137801, 6.000000000000000888 ) ) ;
#20295 = CIRCLE ( 'NONE', #57417, 0.2500000000000002220 ) ;
#20296 =( NAMED_UNIT ( * ) PLANE_ANGLE_UNIT ( ) SI_UNIT ( $, .RADIAN. ) );
#20297 = CARTESIAN_POINT ( 'NONE',  ( -103.7949999999999733, 2.607480562269068880, -8.024999999999993250 ) ) ;
#20298 = ORIENTED_EDGE ( 'NONE', *, *, #65904, .T. ) ;
#20299 =( BOUNDED_CURVE ( )  B_SPLINE_CURVE ( 2, ( #45678, #55840, #50574, #39694, #16265, #56172, #11287, #37739, #45336, #18569, #40050 ),
 .UNSPECIFIED., .F., .F. ) 
 B_SPLINE_CURVE_WITH_KNOTS ( ( 3, 2, 2, 2, 2, 3 ),
 ( 0.2065217391304298156, 0.2086956521739080361, 0.2108695652173862567, 0.2130434782608644773, 0.2152173913043426978, 0.2173913043478209184 ),
 .UNSPECIFIED. ) 
 CURVE ( )  GEOMETRIC_REPRESENTATION_ITEM ( )  RATIONAL_B_SPLINE_CURVE ( ( 1.000000000000111910, 0.9510565162950417317, 1.000000000000000000, 0.9510565162951535312, 1.000000000000000000, 0.9510565162951535312, 1.000000000000000000, 0.9510565162951535312, 1.000000000000000000, 0.9510565162952697715, 0.9999999999998837596 ) ) 
 REPRESENTATION_ITEM ( '' )  );
#20300 = CARTESIAN_POINT ( 'NONE',  ( 15.00000000000000000, 8.000000000000000000, -3.500000000000017764 ) ) ;
#20301 = SURFACE_STYLE_FILL_AREA ( #46391 ) ;
#20302 = CIRCLE ( 'NONE', #22583, 18.99999999999998934 ) ;
#20303 = AXIS2_PLACEMENT_3D ( 'NONE', #27753, #66456, #28098 ) ;
#20304 = CARTESIAN_POINT ( 'NONE',  ( -33.89861118948982721, -9.947368421052624754, -2.000000000000000000 ) ) ;
#20305 = ORIENTED_EDGE ( 'NONE', *, *, #16490, .T. ) ;
#20306 = CARTESIAN_POINT ( 'NONE',  ( -2.607480562269075097, 154.2929263765338135, 8.025000000000000355 ) ) ;
#20307 = AXIS2_PLACEMENT_3D ( 'NONE', #63277, #58682, #216 ) ;
#20308 =( NAMED_UNIT ( * ) SI_UNIT ( $, .STERADIAN. ) SOLID_ANGLE_UNIT ( ) );
#20309 = ORIENTED_EDGE ( 'NONE', *, *, #50376, .T. ) ;
#20310 = EDGE_CURVE ( 'NONE', #68610, #11473, #49355, .T. ) ;
#20311 = CIRCLE ( 'NONE', #59626, 0.2500000000000002220 ) ;
#20312 = CARTESIAN_POINT ( 'NONE',  ( -61.55707362346617373, -1.166476076187852838E-15, -9.524999999999991473 ) ) ;
#20313 = VERTEX_POINT ( 'NONE', #5115 ) ;
#20314 = CARTESIAN_POINT ( 'NONE',  ( 10.00000000000001776, 42.74314482547740113, 27.71473342867655987 ) ) ;
#20315 = DIRECTION ( 'NONE',  ( 0.000000000000000000, 0.000000000000000000, 1.000000000000000000 ) ) ;
#20316 =( NAMED_UNIT ( * ) PLANE_ANGLE_UNIT ( ) SI_UNIT ( $, .RADIAN. ) );
#20317 = CARTESIAN_POINT ( 'NONE',  ( -33.68474050223620964, -8.999709270181368126, 5.797011693762501139 ) ) ;
#20318 = CARTESIAN_POINT ( 'NONE',  ( -128.3050000000000068, 8.437984349512085203, -1.550032578732815448E-15 ) ) ;
#20319 = SURFACE_SIDE_STYLE ('',( #57977 ) ) ;
#20320 = MECHANICAL_DESIGN_GEOMETRIC_PRESENTATION_REPRESENTATION (  '', ( #68645 ), #40590 ) ;
#20321 = DIRECTION ( 'NONE',  ( -0.000000000000000000, -0.000000000000000000, -1.000000000000000000 ) ) ;
#20322 = CARTESIAN_POINT ( 'NONE',  ( 72.00000000000000000, 35.92875272052971525, 9.500000000000000000 ) ) ;
#20323 = DIRECTION ( 'NONE',  ( -1.000000000000000000, -0.000000000000000000, -0.000000000000000000 ) ) ;
#20324 = CARTESIAN_POINT ( 'NONE',  ( 44.25000000000000000, 21.99999999999998579, -3.750000000000000000 ) ) ;
#20325 = CARTESIAN_POINT ( 'NONE',  ( -160.9429263765338192, 0.000000000000000000, 9.524999999999991473 ) ) ;
#20326 = ORIENTED_EDGE ( 'NONE', *, *, #6583, .T. ) ;
#20327 =( GEOMETRIC_REPRESENTATION_CONTEXT ( 3 ) GLOBAL_UNCERTAINTY_ASSIGNED_CONTEXT ( ( #309 ) ) GLOBAL_UNIT_ASSIGNED_CONTEXT ( ( #35446, #35079, #30125 ) ) REPRESENTATION_CONTEXT ( 'NONE', 'WORKASPACE' ) );
#20328 = VERTEX_POINT ( 'NONE', #42461 ) ;
#20329 = DIRECTION ( 'NONE',  ( -1.982541115402069054E-16, -0.000000000000000000, -1.000000000000000000 ) ) ;
#20330 = DIRECTION ( 'NONE',  ( -1.000000000000000000, 0.000000000000000000, 0.000000000000000000 ) ) ;
#20331 = CARTESIAN_POINT ( 'NONE',  ( -75.75000000000000000, -0.9999999999999995559, 7.000000000000001776 ) ) ;
#20332 = DIRECTION ( 'NONE',  ( 0.000000000000000000, 0.000000000000000000, 1.000000000000000000 ) ) ;
#20333 = VERTEX_POINT ( 'NONE', #41058 ) ;
#20334 =( LENGTH_UNIT ( ) NAMED_UNIT ( * ) SI_UNIT ( .MILLI., .METRE. ) );
#20335 = EDGE_CURVE ( 'NONE', #21181, #40347, #26565, .T. ) ;
#20336 = CARTESIAN_POINT ( 'NONE',  ( -178.5549999999999784, 0.000000000000000000, 8.024999999999991473 ) ) ;
#20337 = FACE_OUTER_BOUND ( 'NONE', #32091, .T. ) ;
#20338 = PLANE ( 'NONE',  #60496 ) ;
#20339 = CARTESIAN_POINT ( 'NONE',  ( -182.5449999999999875, -7.632228543268600340, -2.479861379858950166 ) ) ;
#20340 = CARTESIAN_POINT ( 'NONE',  ( -173.5450000000000159, -7.632228543268600340, -2.479861379858950166 ) ) ;
#20341 = AXIS2_PLACEMENT_3D ( 'NONE', #53347, #31508, #58258 ) ;
#20342 = ORIENTED_EDGE ( 'NONE', *, *, #31523, .F. ) ;
#20343 = DIRECTION ( 'NONE',  ( -0.000000000000000000, -0.000000000000000000, -1.000000000000000000 ) ) ;
#20344 = DIRECTION ( 'NONE',  ( 2.312964634635740689E-15, -1.000000000000000000, 0.000000000000000000 ) ) ;
#20345 = CARTESIAN_POINT ( 'NONE',  ( -96.80499999999999261, -8.437984349512085203, 5.166775262442717831E-16 ) ) ;
#20347 =( LENGTH_UNIT ( ) NAMED_UNIT ( * ) SI_UNIT ( .MILLI., .METRE. ) );
#20346 = STYLED_ITEM ( 'NONE', ( #15983 ), #175 ) ;
#20348 = EDGE_CURVE ( 'NONE', #28793, #38116, #44915, .T. ) ;
#20349 = CARTESIAN_POINT ( 'NONE',  ( -86.09499999999995623, -2.607480562269071545, -8.024999999999991473 ) ) ;
#20350 = CARTESIAN_POINT ( 'NONE',  ( 5.598654528085809545, 131.2549999999999955, -7.705886871421373741 ) ) ;
#20351 = CARTESIAN_POINT ( 'NONE',  ( -68.84499999999998465, -7.632228543268599452, 2.479861379858951054 ) ) ;
#20352 = CYLINDRICAL_SURFACE ( 'NONE', #51072, 3.100000000000003642 ) ;
#20353 = AXIS2_PLACEMENT_3D ( 'NONE', #1793, #51095, #66926 ) ;
#20354 = CARTESIAN_POINT ( 'NONE',  ( 4.500000000000002665, 24.99999999999998579, 4.000000000000000000 ) ) ;
#20355 = FILL_AREA_STYLE_COLOUR ( '', #42799 ) ;
#20356 = SURFACE_STYLE_USAGE ( .BOTH. , #68564 ) ;
#20357 = ORIENTED_EDGE ( 'NONE', *, *, #46346, .T. ) ;
#20358 = CARTESIAN_POINT ( 'NONE',  ( -109.7929263765338135, -3.094860106618429807, 9.524999999999991473 ) ) ;
#20359 = PRODUCT ( '7. Upper Jaw', '7. Upper Jaw', '', ( #13171 ) ) ;
#20360 = CARTESIAN_POINT ( 'NONE',  ( -128.3949999999999534, -6.826472737025115478, -4.959722759717899443 ) ) ;
#20361 = CARTESIAN_POINT ( 'NONE',  ( 0.000000000000000000, 145.0570736234661524, -8.025000000000000355 ) ) ;
#20362 = CIRCLE ( 'NONE', #10245, 0.2500000000000002220 ) ;
#20363 = CARTESIAN_POINT ( 'NONE',  ( 31.00000000000002132, 43.00000000000000000, 79.00402776293823592 ) ) ;
#20364 = AXIS2_PLACEMENT_3D ( 'NONE', #24007, #45516, #40915 ) ;
#20366 = CARTESIAN_POINT ( 'NONE',  ( -25.00000000000000000, 0.000000000000000000, 4.000000000000000000 ) ) ;
#20365 = CARTESIAN_POINT ( 'NONE',  ( -131.2429263765338021, 5.598654528085804216, 7.705886871421366635 ) ) ;
#20367 = VERTEX_POINT ( 'NONE', #9025 ) ;
#20368 = VERTEX_POINT ( 'NONE', #15019 ) ;
#20369 =( NAMED_UNIT ( * ) SI_UNIT ( $, .STERADIAN. ) SOLID_ANGLE_UNIT ( ) );
#20370 =( GEOMETRIC_REPRESENTATION_CONTEXT ( 3 ) GLOBAL_UNCERTAINTY_ASSIGNED_CONTEXT ( ( #8809 ) ) GLOBAL_UNIT_ASSIGNED_CONTEXT ( ( #68078, #3650, #7921 ) ) REPRESENTATION_CONTEXT ( 'NONE', 'WORKASPACE' ) );
#20371 = CARTESIAN_POINT ( 'NONE',  ( -134.5429263765338135, 9.058813317711329915, 2.943386871421369566 ) ) ;
#20372 = AXIS2_PLACEMENT_3D ( 'NONE', #38235, #63872, #16764 ) ;
#20373 =( REPRESENTATION_RELATIONSHIP ('NONE','NONE', #5102, #22166 ) REPRESENTATION_RELATIONSHIP_WITH_TRANSFORMATION ( #25810 )SHAPE_REPRESENTATION_RELATIONSHIP( ) );
#20374 = CARTESIAN_POINT ( 'NONE',  ( 66.49999999999998579, 36.75000000000000000, 3.750000000000000000 ) ) ;
#20375 = VECTOR ( 'NONE', #37113, 1000.000000000000000 ) ;
#20376 = CARTESIAN_POINT ( 'NONE',  ( 10.39230484541327115, -4.119968255444916849E-15, 7.500000000000000000 ) ) ;
#20377 = CARTESIAN_POINT ( 'NONE',  ( 17.25000000000000711, 24.99999999999998224, 3.750000000000000000 ) ) ;
#20378 = VERTEX_POINT ( 'NONE', #62474 ) ;
#20379 = CARTESIAN_POINT ( 'NONE',  ( -125.7550000000000097, 4.716976649647091513, -6.492361379858946790 ) ) ;
#20380 = EDGE_LOOP ( 'NONE', ( #4987, #60085, #1666, #43553 ) ) ;
#20381 = DIRECTION ( 'NONE',  ( 0.000000000000000000, -0.000000000000000000, -1.000000000000000000 ) ) ;
#20382 = CARTESIAN_POINT ( 'NONE',  ( -121.7070736234661581, -3.094860106618431139, -9.524999999999991473 ) ) ;
#20383 = VERTEX_POINT ( 'NONE', #52308 ) ;
#20384 = DIRECTION ( 'NONE',  ( 1.000000000000000000, 0.000000000000000000, 0.000000000000000000 ) ) ;
#20385 = PRESENTATION_STYLE_ASSIGNMENT (( #69283 ) ) ;
#20386 = ORIENTED_EDGE ( 'NONE', *, *, #43444, .T. ) ;
#20387 = PRESENTATION_STYLE_ASSIGNMENT (( #40840 ) ) ;
#20388 = CARTESIAN_POINT ( 'NONE',  ( 10.01517768586949231, 147.6949999999999932, 1.839758294383810543E-15 ) ) ;
#20389 = CYLINDRICAL_SURFACE ( 'NONE', #12674, 0.5000000000000004441 ) ;
#20390 = AXIS2_PLACEMENT_3D ( 'NONE', #1084, #53928, #5728 ) ;
#20391 = VERTEX_POINT ( 'NONE', #31146 ) ;
#20392 = MECHANICAL_DESIGN_GEOMETRIC_PRESENTATION_REPRESENTATION (  '', ( #37316 ), #42941 ) ;
#20393 = SURFACE_STYLE_USAGE ( .BOTH. , #10197 ) ;
#20394 = CARTESIAN_POINT ( 'NONE',  ( 3.094860106618435136, 152.4049999999999443, -9.525000000000000355 ) ) ;
#20395 = CARTESIAN_POINT ( 'NONE',  ( 192.5000000000000000, 4.592425496802570028E-16, 0.000000000000000000 ) ) ;
#20396 = ORIENTED_EDGE ( 'NONE', *, *, #40370, .T. ) ;
#20397 = CARTESIAN_POINT ( 'NONE',  ( 6.826472737025119919, 127.8929263765338220, 4.959722759717908325 ) ) ;
#20398 = CARTESIAN_POINT ( 'NONE',  ( 4.000000000000002665, 43.00000000000000000, -90.00000000000000000 ) ) ;
#20399 = CARTESIAN_POINT ( 'NONE',  ( -47.00707362346617657, -8.102448949553174629, -5.886773742842741797 ) ) ;
#20400 = PRESENTATION_LAYER_ASSIGNMENT (  '', '', ( #31588 ) ) ;
#20401 = SURFACE_STYLE_USAGE ( .BOTH. , #9530 ) ;
#20402 = DIRECTION ( 'NONE',  ( -1.300977106640434891E-16, 0.000000000000000000, -1.000000000000000000 ) ) ;
#20403 = CARTESIAN_POINT ( 'NONE',  ( 48.50000000000000000, 14.49137674618942562, 7.500000000000000000 ) ) ;
#20404 = VERTEX_POINT ( 'NONE', #67766 ) ;
#20405 = ADVANCED_FACE ( 'NONE', ( #52643 ), #4400, .F. ) ;
#20406 = DIRECTION ( 'NONE',  ( 0.000000000000000000, 0.000000000000000000, -1.000000000000000000 ) ) ;
#20407 = EDGE_LOOP ( 'NONE', ( #35403, #42842, #23723, #30877 ) ) ;
#20408 = CARTESIAN_POINT ( 'NONE',  ( -56.84292637653378932, 9.058813317711329915, -2.943386871421373119 ) ) ;
#20409 = CARTESIAN_POINT ( 'NONE',  ( -8.082903768654762899, 3.463586619550771876E-15, 1.082903768654759125 ) ) ;
#20410 = CARTESIAN_POINT ( 'NONE',  ( -156.3549999999999898, -4.716976649647093289, -6.492361379858945902 ) ) ;
#20411 = VERTEX_POINT ( 'NONE', #31494 ) ;
#20412 = PRESENTATION_STYLE_ASSIGNMENT (( #14432 ) ) ;
#20413 = EDGE_CURVE ( 'NONE', #55502, #13013, #14292, .T. ) ;
#20414 = ADVANCED_FACE ( 'NONE', ( #25874 ), #41761, .F. ) ;
#20415 = AXIS2_PLACEMENT_3D ( 'NONE', #68414, #40307, #35009 ) ;
#20416 = CIRCLE ( 'NONE', #46311, 0.4999999999999991118 ) ;
#20417 = DIRECTION ( 'NONE',  ( 1.000000000000000000, 0.000000000000000000, -1.300977106640434891E-16 ) ) ;
#20418 = DIRECTION ( 'NONE',  ( 0.000000000000000000, 0.000000000000000000, 1.000000000000000000 ) ) ;
#20419 = CARTESIAN_POINT ( 'NONE',  ( 75.00000000000000000, 19.44429231213349141, 6.999999999972111198 ) ) ;
#20420 = CARTESIAN_POINT ( 'NONE',  ( 7.632228543268607446, 146.0429263765338135, 2.479861379858954606 ) ) ;
#20421 = EDGE_LOOP ( 'NONE', ( #41793, #59416, #3113, #67996 ) ) ;
#20422 = AXIS2_PLACEMENT_3D ( 'NONE', #41804, #62852, #63223 ) ;
#20423 = ADVANCED_FACE ( 'NONE', ( #41405 ), #69101, .T. ) ;
#20424 = ORIENTED_EDGE ( 'NONE', *, *, #28901, .T. ) ;
#20425 = FACE_OUTER_BOUND ( 'NONE', #43538, .T. ) ;
#20426 = AXIS2_PLACEMENT_3D ( 'NONE', #50451, #37611, #36404 ) ;
#20427 = SURFACE_SIDE_STYLE ('',( #5964 ) ) ;
#20428 = CARTESIAN_POINT ( 'NONE',  ( -63.95499999999998408, -7.632228543268599452, 2.479861379858951054 ) ) ;
#20429 = ORIENTED_EDGE ( 'NONE', *, *, #26518, .F. ) ;
#20430 = CARTESIAN_POINT ( 'NONE',  ( 0.000000000000000000, 2.299999999999999822, 0.000000000000000000 ) ) ;
#20431 = ADVANCED_FACE ( 'NONE', ( #65597 ), #60317, .F. ) ;
#20432 = ADVANCED_FACE ( 'NONE', ( #17099 ), #32206, .F. ) ;
#20434 = EDGE_CURVE ( 'NONE', #12490, #583, #53653, .T. ) ;
#20433 = AXIS2_PLACEMENT_3D ( 'NONE', #25065, #67280, #29283 ) ;
#20435 = CARTESIAN_POINT ( 'NONE',  ( -124.3429263765337964, -9.058813317711329915, 2.943386871421371787 ) ) ;
#20436 = DIRECTION ( 'NONE',  ( 0.000000000000000000, 0.000000000000000000, -1.000000000000000000 ) ) ;
#20437 = ORIENTED_EDGE ( 'NONE', *, *, #45552, .F. ) ;
#20438 = STYLED_ITEM ( 'NONE', ( #25134 ), #54315 ) ;
#20439 = EDGE_CURVE ( 'NONE', #149, #17310, #16415, .T. ) ;
#20440 = DIRECTION ( 'NONE',  ( 0.000000000000000000, -1.000000000000000000, 0.000000000000000000 ) ) ;
#20441 = FILL_AREA_STYLE_COLOUR ( '', #49937 ) ;
#20442 = CARTESIAN_POINT ( 'NONE',  ( 22.00000000000002132, 50.00000000000000000, 59.99999999999999289 ) ) ;
#20443 = AXIS2_PLACEMENT_3D ( 'NONE', #18922, #20323, #9447 ) ;
#20444 = CARTESIAN_POINT ( 'NONE',  ( -8.102448949553181734, 145.8949999999999534, -5.886773742842749790 ) ) ;
#20445 = CARTESIAN_POINT ( 'NONE',  ( -97.19499999999997897, 8.437984349512085203, -1.550032578732815448E-15 ) ) ;
#20446 = CIRCLE ( 'NONE', #1287, 0.2500000000000002220 ) ;
#20447 =( LENGTH_UNIT ( ) NAMED_UNIT ( * ) SI_UNIT ( .MILLI., .METRE. ) );
#20448 = COLOUR_RGB ( '', 0.40784314, 0.44705882, 0.49803922) ;
#20449 = CARTESIAN_POINT ( 'NONE',  ( -40.99999999999998579, 107.7459666924148252, -3.050022167383943383 ) ) ;
#20450 = ORIENTED_EDGE ( 'NONE', *, *, #30460, .F. ) ;
#20451 = CARTESIAN_POINT ( 'NONE',  ( -131.8429263765337964, 9.058813317711329915, -2.943386871421373119 ) ) ;
#20452 = DIRECTION ( 'NONE',  ( -1.000000000000000000, -0.000000000000000000, -0.000000000000000000 ) ) ;
#20453 = CARTESIAN_POINT ( 'NONE',  ( -159.5949999999999989, 2.607480562269073321, 8.024999999999991473 ) ) ;
#20454 =( LENGTH_UNIT ( ) NAMED_UNIT ( * ) SI_UNIT ( .MILLI., .METRE. ) );
#20455 = MECHANICAL_DESIGN_GEOMETRIC_PRESENTATION_REPRESENTATION (  '', ( #50787 ), #46352 ) ;
#20456 = LINE ( 'NONE', #16511, #61775 ) ;
#20457 = CARTESIAN_POINT ( 'NONE',  ( -133.4929263765338021, -8.102448949553174629, 5.886773742842742685 ) ) ;
#20458 = ORIENTED_EDGE ( 'NONE', *, *, #67682, .T. ) ;
#20459 = ORIENTED_EDGE ( 'NONE', *, *, #49668, .T. ) ;
#20460 = CIRCLE ( 'NONE', #31701, 5.000000000000000000 ) ;
#20461 = LINE ( 'NONE', #53180, #55462 ) ;
#20462 = CONICAL_SURFACE ( 'NONE', #47480, 3.599999999999992095, 0.7853981633974375098 ) ;
#20463 = VECTOR ( 'NONE', #44381, 1000.000000000000000 ) ;
#20464 = DIRECTION ( 'NONE',  ( -1.000000000000000000, 0.000000000000000000, 0.000000000000000000 ) ) ;
#20465 = CARTESIAN_POINT ( 'NONE',  ( -45.91547277787986303, 9.430195805462179948, 6.024500123752370762 ) ) ;
#20466 = MECHANICAL_DESIGN_GEOMETRIC_PRESENTATION_REPRESENTATION (  '', ( #49701 ), #43013 ) ;
#20467 = CARTESIAN_POINT ( 'NONE',  ( -58.57530068368657794, -7.668632606274902841, -0.3315242760381541531 ) ) ;
#20468 = ORIENTED_EDGE ( 'NONE', *, *, #24503, .F. ) ;
#20469 = CARTESIAN_POINT ( 'NONE',  ( -146.4550000000000125, 7.632228543268599452, -2.479861379858951942 ) ) ;
#20470 = VERTEX_POINT ( 'NONE', #48776 ) ;
#20471 = DIRECTION ( 'NONE',  ( 0.000000000000000000, 0.000000000000000000, -1.000000000000000000 ) ) ;
#20472 = DIRECTION ( 'NONE',  ( 1.000000000000000000, -0.000000000000000000, -0.000000000000000000 ) ) ;
#20473 = CIRCLE ( 'NONE', #24933, 4.750000000000000000 ) ;
#20474 = ORIENTED_EDGE ( 'NONE', *, *, #49043, .F. ) ;
#20475 = FILL_AREA_STYLE_COLOUR ( '', #40573 ) ;
#20476 = DIRECTION ( 'NONE',  ( -0.000000000000000000, 1.000000000000000000, -0.000000000000000000 ) ) ;
#20477 = CARTESIAN_POINT ( 'NONE',  ( -5.598654528085808657, 125.6449999999999818, 7.705886871421373741 ) ) ;
#20478 = CARTESIAN_POINT ( 'NONE',  ( 0.8561458320465511473, 42.99999999999999289, -74.38749456993816978 ) ) ;
#20479 = PRESENTATION_LAYER_ASSIGNMENT (  '', '', ( #44128 ) ) ;
#20480 = VERTEX_POINT ( 'NONE', #22345 ) ;
#20481 = FILL_AREA_STYLE ('',( #26441 ) ) ;
#20482 = CARTESIAN_POINT ( 'NONE',  ( -8.102448949553179958, 120.6049999999999756, 5.886773742842747126 ) ) ;
#20483 = CARTESIAN_POINT ( 'NONE',  ( -67.55499999999999261, 0.000000000000000000, 8.024999999999991473 ) ) ;
#20484 = FILL_AREA_STYLE_COLOUR ( '', #65519 ) ;
#20485 = EDGE_LOOP ( 'NONE', ( #7088, #58479, #40835, #2336 ) ) ;
#20486 = CARTESIAN_POINT ( 'NONE',  ( 0.000000000000000000, 149.5550000000000068, -9.525000000000000355 ) ) ;
#20487 = CARTESIAN_POINT ( 'NONE',  ( 0.000000000000000000, 149.9999999999999716, 0.000000000000000000 ) ) ;
#20488 = MECHANICAL_DESIGN_GEOMETRIC_PRESENTATION_REPRESENTATION (  '', ( #30555 ), #171 ) ;
#20489 = DIRECTION ( 'NONE',  ( -0.000000000000000000, -1.000000000000000000, -0.000000000000000000 ) ) ;
#20490 = ADVANCED_FACE ( 'NONE', ( #59973 ), #43839, .T. ) ;
#20491 = DIRECTION ( 'NONE',  ( 0.000000000000000000, 0.000000000000000000, 1.000000000000000000 ) ) ;
#20492 = ADVANCED_FACE ( 'NONE', ( #39598 ), #34286, .T. ) ;
#20493 = VERTEX_POINT ( 'NONE', #62040 ) ;
#20494 = FILL_AREA_STYLE_COLOUR ( '', #21000 ) ;
#20495 = CARTESIAN_POINT ( 'NONE',  ( 74.65811388300841145, 19.88603796100278487, -6.292893218813454759 ) ) ;
#20496 = CARTESIAN_POINT ( 'NONE',  ( -8.082903768654761123, -1.417096231345241097, -1.759977097422839922E-15 ) ) ;
#20497 = CARTESIAN_POINT ( 'NONE',  ( -179.9049999999999727, 2.607480562269068880, -8.024999999999993250 ) ) ;
#20498 = ORIENTED_EDGE ( 'NONE', *, *, #21616, .T. ) ;
#20499 = CARTESIAN_POINT ( 'NONE',  ( 4.325530127497533073, 111.8337402250126900, -6.961252418569971567 ) ) ;
#20500 = EDGE_CURVE ( 'NONE', #61162, #8408, #56788, .T. ) ;
#20501 =( GEOMETRIC_REPRESENTATION_CONTEXT ( 3 ) GLOBAL_UNCERTAINTY_ASSIGNED_CONTEXT ( ( #49731 ) ) GLOBAL_UNIT_ASSIGNED_CONTEXT ( ( #25437, #54915, #10654 ) ) REPRESENTATION_CONTEXT ( 'NONE', 'WORKASPACE' ) );
#20502 = FILL_AREA_STYLE ('',( #58481 ) ) ;
#20503 = ORIENTED_EDGE ( 'NONE', *, *, #40052, .T. ) ;
#20504 = LINE ( 'NONE', #67654, #54526 ) ;
#20505 = FACE_OUTER_BOUND ( 'NONE', #91, .T. ) ;
#20506 = ORIENTED_EDGE ( 'NONE', *, *, #56629, .F. ) ;
#20507 = VECTOR ( 'NONE', #59931, 1000.000000000000000 ) ;
#20508 = CARTESIAN_POINT ( 'NONE',  ( 10.00000000000000533, 50.00000000000000000, -60.00000000000000000 ) ) ;
#20509 = CARTESIAN_POINT ( 'NONE',  ( -94.10499999999997556, -6.826472737025115478, 4.959722759717900331 ) ) ;
#20510 = ORIENTED_EDGE ( 'NONE', *, *, #35122, .T. ) ;
#20511 = FACE_OUTER_BOUND ( 'NONE', #54132, .T. ) ;
#20512 = ADVANCED_FACE ( 'NONE', ( #17775 ), #13867, .F. ) ;
#20513 = FILL_AREA_STYLE_COLOUR ( '', #25795 ) ;
#20514 = CARTESIAN_POINT ( 'NONE',  ( -135.5070736234661695, 8.102448949553176405, 5.886773742842740909 ) ) ;
#20515 = AXIS2_PLACEMENT_3D ( 'NONE', #63671, #26705, #69635 ) ;
#20516 = CONICAL_SURFACE ( 'NONE', #37445, 5.500000000000005329, 0.7853981633974309595 ) ;
#20517 = CARTESIAN_POINT ( 'NONE',  ( -1.113559396844004956, 154.5000000000000000, -9.459683423334018570 ) ) ;
#20518 = CARTESIAN_POINT ( 'NONE',  ( -72.05707362346616662, 0.000000000000000000, 9.524999999999991473 ) ) ;
#20519 = EDGE_CURVE ( 'NONE', #38534, #1374, #67330, .T. ) ;
#20520 = CARTESIAN_POINT ( 'NONE',  ( 17.00000000000000711, 24.99999999999998224, 4.000000000000000000 ) ) ;
#20521 = VERTEX_POINT ( 'NONE', #56078 ) ;
#20522 = LINE ( 'NONE', #48005, #21525 ) ;
#20523 = CARTESIAN_POINT ( 'NONE',  ( -18.30630105587923495, -11.39666211907883664, -3.764819142662532592 ) ) ;
#20525 = CARTESIAN_POINT ( 'NONE',  ( 1.000000000000000000, 42.00000000000000000, 79.00402776293826435 ) ) ;
#20524 =( LENGTH_UNIT ( ) NAMED_UNIT ( * ) SI_UNIT ( .MILLI., .METRE. ) );
#20526 = CARTESIAN_POINT ( 'NONE',  ( -111.2049999999999983, -2.607480562269071545, -8.024999999999991473 ) ) ;
#20527 = CARTESIAN_POINT ( 'NONE',  ( 22.00000000000002132, 43.00000000000000000, -29.68999999999999417 ) ) ;
#20528 = CARTESIAN_POINT ( 'NONE',  ( -8.102448949553181734, 119.4949999999999903, 5.886773742842747126 ) ) ;
#20529 = AXIS2_PLACEMENT_3D ( 'NONE', #29191, #2420, #52086 ) ;
#20530 = CARTESIAN_POINT ( 'NONE',  ( -124.1950000000000074, 8.437984349512085203, -1.550032578732815448E-15 ) ) ;
#20531 = LINE ( 'NONE', #31408, #20151 ) ;
#20532 = CARTESIAN_POINT ( 'NONE',  ( 28.00000000000000000, 43.00000000000000000, -79.00402776293826435 ) ) ;
#20533 = ORIENTED_EDGE ( 'NONE', *, *, #23124, .F. ) ;
#20534 = CARTESIAN_POINT ( 'NONE',  ( -158.9929263765338021, 8.102448949553171076, -5.886773742842744461 ) ) ;
#20535 = CARTESIAN_POINT ( 'NONE',  ( -182.0949999999999989, -2.607480562269071545, -8.024999999999991473 ) ) ;
#20536 = STYLED_ITEM ( 'NONE', ( #8645 ), #7231 ) ;
#20537 = AXIS2_PLACEMENT_3D ( 'NONE', #52475, #51408, #46881 ) ;
#20538 = PLANE ( 'NONE',  #36042 ) ;
#20539 = DIRECTION ( 'NONE',  ( 1.000000000000000000, 0.000000000000000000, 0.000000000000000000 ) ) ;
#20540 = DIRECTION ( 'NONE',  ( 0.000000000000000000, 0.000000000000000000, 1.000000000000000000 ) ) ;
#20541 = ORIENTED_EDGE ( 'NONE', *, *, #32354, .T. ) ;
#20542 = CARTESIAN_POINT ( 'NONE',  ( -78.29292637653378506, 3.094860106618428031, -9.524999999999993250 ) ) ;
#20543 = LINE ( 'NONE', #69430, #34071 ) ;
#20544 = DIRECTION ( 'NONE',  ( -1.000000000000000000, -3.469446951953611033E-15, 0.000000000000000000 ) ) ;
#20545 = EDGE_CURVE ( 'NONE', #63576, #53864, #59620, .T. ) ;
#20546 = CARTESIAN_POINT ( 'NONE',  ( 8.437984349512095861, 152.1929263765338192, 1.550032578732816828E-15 ) ) ;
#20547 = CARTESIAN_POINT ( 'NONE',  ( 6.826472737025119919, 147.0070736234661695, 4.959722759717908325 ) ) ;
#20548 = CARTESIAN_POINT ( 'NONE',  ( -181.2549999999999955, -4.716976649647092401, 6.492361379858946790 ) ) ;
#20549 = VERTEX_POINT ( 'NONE', #12820 ) ;
#20550 = CARTESIAN_POINT ( 'NONE',  ( -83.49999999999997158, 50.00000000000000000, -12.00000000000000000 ) ) ;
#20551 = FILL_AREA_STYLE_COLOUR ( '', #61013 ) ;
#20552 = VERTEX_POINT ( 'NONE', #40268 ) ;
#20553 = CARTESIAN_POINT ( 'NONE',  ( 5.196152422706631135, -1.107695154586740394, 9.000000000000001776 ) ) ;
#20554 = AXIS2_PLACEMENT_3D ( 'NONE', #8043, #61479, #50610 ) ;
#20555 = STYLED_ITEM ( 'NONE', ( #57135 ), #61294 ) ;
#20556 = B_SPLINE_CURVE_WITH_KNOTS ( 'NONE', 3,
 ( #20285, #5141, #54024, #5827, #4430, #48454, #63208, #15053 ),
 .UNSPECIFIED., .F., .F.,
 ( 4, 2, 2, 4 ),
 ( 0.004248627969284164696, 0.005296391997195108725, 0.006344156025106052754, 0.008439684080927939078 ),
 .UNSPECIFIED. ) ;
#20557 = CARTESIAN_POINT ( 'NONE',  ( 48.81081081081080697, 14.09971791521132900, -7.500000000000000000 ) ) ;
#20558 = CARTESIAN_POINT ( 'NONE',  ( -9.827790563157511022E-16, 146.5570736234661524, 8.025000000000000355 ) ) ;
#20559 = PRESENTATION_STYLE_ASSIGNMENT (( #68406 ) ) ;
#20560 = MECHANICAL_DESIGN_GEOMETRIC_PRESENTATION_REPRESENTATION (  '', ( #23919 ), #58830 ) ;
#20561 = ORIENTED_EDGE ( 'NONE', *, *, #24101, .T. ) ;
#20562 = DIRECTION ( 'NONE',  ( -0.000000000000000000, -1.000000000000000000, -0.000000000000000000 ) ) ;
#20563 = CARTESIAN_POINT ( 'NONE',  ( -92.15499999999998693, 7.632228543268600340, 2.479861379858949277 ) ) ;
#20564 = LINE ( 'NONE', #42081, #13972 ) ;
#20565 = ORIENTED_EDGE ( 'NONE', *, *, #37727, .T. ) ;
#20566 = DIRECTION ( 'NONE',  ( 0.000000000000000000, 1.000000000000000000, 0.000000000000000000 ) ) ;
#20567 = EDGE_CURVE ( 'NONE', #51461, #31418, #24619, .T. ) ;
#20568 = CARTESIAN_POINT ( 'NONE',  ( 4.716976649647099507, 143.6429263765338078, -6.492361379858953008 ) ) ;
#20569 = EDGE_CURVE ( 'NONE', #40909, #19597, #55741, .T. ) ;
#20570 = CARTESIAN_POINT ( 'NONE',  ( -45.50000000000000000, -2.024042244987997205E-14, -6.999999999999999112 ) ) ;
#20571 = AXIS2_PLACEMENT_3D ( 'NONE', #30939, #10194, #27020 ) ;
#20572 = EDGE_LOOP ( 'NONE', ( #8011, #18667, #62196, #62975 ) ) ;
#20573 = AXIS2_PLACEMENT_3D ( 'NONE', #13390, #50697, #34851 ) ;
#20574 = DIRECTION ( 'NONE',  ( 1.000000000000000000, 0.000000000000000000, 0.000000000000000000 ) ) ;
#20575 = CARTESIAN_POINT ( 'NONE',  ( -70.94499999999997897, -9.827790563157499189E-16, -8.024999999999991473 ) ) ;
#20576 = ORIENTED_EDGE ( 'NONE', *, *, #58882, .T. ) ;
#20577 = CYLINDRICAL_SURFACE ( 'NONE', #36199, 5.000000000000004441 ) ;
#20578 = PRESENTATION_LAYER_ASSIGNMENT (  '', '', ( #22850 ) ) ;
#20579 = SURFACE_STYLE_USAGE ( .BOTH. , #52948 ) ;
#20580 = EDGE_CURVE ( 'NONE', #45878, #66425, #1521, .T. ) ;
#20581 = DIRECTION ( 'NONE',  ( 0.000000000000000000, 0.000000000000000000, -1.000000000000000000 ) ) ;
#20582 = PRESENTATION_LAYER_ASSIGNMENT (  '', '', ( #17257 ) ) ;
#20583 = ORIENTED_EDGE ( 'NONE', *, *, #57927, .F. ) ;
#20584 = DIRECTION ( 'NONE',  ( -0.000000000000000000, -0.000000000000000000, -1.000000000000000000 ) ) ;
#20585 = CARTESIAN_POINT ( 'NONE',  ( 57.00000000000000000, 5.000000000000000000, -65.00402776293825013 ) ) ;
#20586 = EDGE_CURVE ( 'NONE', #51601, #20128, #8935, .T. ) ;
#20587 = MECHANICAL_DESIGN_GEOMETRIC_PRESENTATION_REPRESENTATION (  '', ( #34086 ), #1437 ) ;
#20588 = EDGE_LOOP ( 'NONE', ( #44055, #46909, #65570, #60092 ) ) ;
#20589 =( LENGTH_UNIT ( ) NAMED_UNIT ( * ) SI_UNIT ( .MILLI., .METRE. ) );
#20590 = VERTEX_POINT ( 'NONE', #61676 ) ;
#20591 = EDGE_CURVE ( 'NONE', #29559, #65168, #1866, .T. ) ;
#20592 = LINE ( 'NONE', #30783, #22948 ) ;
#20593 = DIRECTION ( 'NONE',  ( 0.000000000000000000, 0.000000000000000000, 1.000000000000000000 ) ) ;
#20594 = CARTESIAN_POINT ( 'NONE',  ( -158.9070736234661183, -3.094860106618429807, 9.524999999999991473 ) ) ;
#20595 = CARTESIAN_POINT ( 'NONE',  ( 0.000000000000000000, 118.4449999999999932, -9.525000000000000355 ) ) ;
#20596 = CARTESIAN_POINT ( 'NONE',  ( -107.7570736234661695, -5.598654528085801552, 7.705886871421367523 ) ) ;
#20597 = MECHANICAL_DESIGN_GEOMETRIC_PRESENTATION_REPRESENTATION (  '', ( #25062 ), #65486 ) ;
#20598 = SURFACE_STYLE_FILL_AREA ( #57540 ) ;
#20599 = EDGE_CURVE ( 'NONE', #5467, #11645, #50462, .T. ) ;
#20600 = CARTESIAN_POINT ( 'NONE',  ( -65.45707362346617231, -9.058813317711329915, 2.943386871421371787 ) ) ;
#20601 = VERTEX_POINT ( 'NONE', #7214 ) ;
#20602 =( BOUNDED_CURVE ( )  B_SPLINE_CURVE ( 2, ( #12257, #5597, #27045, #43993, #43324, #6633, #59778, #48579, #33724, #54493, #11240 ),
 .UNSPECIFIED., .F., .F. ) 
 B_SPLINE_CURVE_WITH_KNOTS ( ( 3, 2, 2, 2, 2, 3 ),
 ( 0.1176470588235295212, 0.1235294117647059986, 0.1294117647058824760, 0.1352941176470589257, 0.1411764705882354032, 0.1470588235294118806 ),
 .UNSPECIFIED. ) 
 CURVE ( )  GEOMETRIC_REPRESENTATION_ITEM ( )  RATIONAL_B_SPLINE_CURVE ( ( 0.9999999999999991118, 0.9510565162951544194, 1.000000000000000000, 0.9510565162951535312, 1.000000000000000000, 0.9510565162951535312, 1.000000000000000000, 0.9510565162951535312, 1.000000000000000000, 0.9510565162951526430, 1.000000000000000888 ) ) 
 REPRESENTATION_ITEM ( '' )  );
#20604 = CARTESIAN_POINT ( 'NONE',  ( 48.50000000000000000, 14.49137674618942562, 7.000000000000000000 ) ) ;
#20603 = CARTESIAN_POINT ( 'NONE',  ( -195.0000000000000000, 0.000000000000000000, 0.000000000000000000 ) ) ;
#20605 =( NAMED_UNIT ( * ) PLANE_ANGLE_UNIT ( ) SI_UNIT ( $, .RADIAN. ) );
#20606 = CARTESIAN_POINT ( 'NONE',  ( -141.8050000000000068, -8.437984349512085203, 5.166775262442717831E-16 ) ) ;
#20607 = LINE ( 'NONE', #25867, #16214 ) ;
#20608 = LINE ( 'NONE', #473, #25770 ) ;
#20609 = CARTESIAN_POINT ( 'NONE',  ( -156.7450000000000045, 4.716976649647094177, 6.492361379858945902 ) ) ;
#20610 = VECTOR ( 'NONE', #22806, 1000.000000000000000 ) ;
#20611 = AXIS2_PLACEMENT_3D ( 'NONE', #63971, #68933, #31256 ) ;
#20612 = CARTESIAN_POINT ( 'NONE',  ( -134.5449999999999875, -7.632228543268600340, -2.479861379858950166 ) ) ;
#20613 = VERTEX_POINT ( 'NONE', #50136 ) ;
#20614 = CARTESIAN_POINT ( 'NONE',  ( 12.75000000000000533, 28.24999999999998224, -4.000000000000000000 ) ) ;
#20615 = STYLED_ITEM ( 'NONE', ( #32100 ), #47057 ) ;
#20616 = DIRECTION ( 'NONE',  ( -0.000000000000000000, -0.000000000000000000, -1.000000000000000000 ) ) ;
#20617 = DIRECTION ( 'NONE',  ( 0.000000000000000000, 0.000000000000000000, 1.000000000000000000 ) ) ;
#20618 = UNCERTAINTY_MEASURE_WITH_UNIT (LENGTH_MEASURE( 1.000000000000000082E-05 ), #47102, 'distance_accuracy_value', 'NONE');
#20619 = CARTESIAN_POINT ( 'NONE',  ( -56.30499999999999972, 8.437984349512085203, -1.550032578732815448E-15 ) ) ;
#20620 = VECTOR ( 'NONE', #31784, 1000.000000000000000 ) ;
#20621 = CARTESIAN_POINT ( 'NONE',  ( 10.01517768586949231, 157.8050000000000068, 1.839758294383810543E-15 ) ) ;
#20622 = CARTESIAN_POINT ( 'NONE',  ( 3.000000000000030198, 35.42594141563417054, 80.00402776293826435 ) ) ;
#20623 = CARTESIAN_POINT ( 'NONE',  ( 41.49999999999998579, 106.9282032302754999, 4.000000000000000000 ) ) ;
#20624 = UNCERTAINTY_MEASURE_WITH_UNIT (LENGTH_MEASURE( 1.000000000000000082E-05 ), #24748, 'distance_accuracy_value', 'NONE');
#20625 =( BOUNDED_CURVE ( )  B_SPLINE_CURVE ( 2, ( #26215, #20958, #10750, #27586, #11778, #5109, #69481, #58581, #16405, #59608, #42808 ),
 .UNSPECIFIED., .F., .F. ) 
 B_SPLINE_CURVE_WITH_KNOTS ( ( 3, 2, 2, 2, 2, 3 ),
 ( 0.4117647058823530326, 0.4176470588235295378, 0.4235294117647059875, 0.4294117647058824372, 0.4352941176470589424, 0.4411764705882353921 ),
 .UNSPECIFIED. ) 
 CURVE ( )  GEOMETRIC_REPRESENTATION_ITEM ( )  RATIONAL_B_SPLINE_CURVE ( ( 0.9999999999999991118, 0.9510565162951544194, 1.000000000000000000, 0.9510565162951535312, 1.000000000000000000, 0.9510565162951535312, 1.000000000000000000, 0.9510565162951535312, 1.000000000000000000, 0.9510565162951526430, 1.000000000000000888 ) ) 
 REPRESENTATION_ITEM ( '' )  );
#20626 = CARTESIAN_POINT ( 'NONE',  ( 0.000000000000000000, 0.000000000000000000, 0.000000000000000000 ) ) ;
#20627 = AXIS2_PLACEMENT_3D ( 'NONE', #44248, #23422, #22752 ) ;
#20628 =( NAMED_UNIT ( * ) PLANE_ANGLE_UNIT ( ) SI_UNIT ( $, .RADIAN. ) );
#20629 = ADVANCED_FACE ( 'NONE', ( #45223 ), #13504, .T. ) ;
#20630 = STYLED_ITEM ( 'NONE', ( #68235 ), #30860 ) ;
#20631 = CARTESIAN_POINT ( 'NONE',  ( -81.65707362346617515, 9.058813317711329915, 2.943386871421369566 ) ) ;
#20632 = CARTESIAN_POINT ( 'NONE',  ( 92.41620014002536720, 5.000000000000000000, 29.00402776293826079 ) ) ;
#20633 = PRESENTATION_LAYER_ASSIGNMENT (  '', '', ( #46546 ) ) ;
#20634 = VECTOR ( 'NONE', #36930, 1000.000000000000000 ) ;
#20635 = FILL_AREA_STYLE_COLOUR ( '', #46231 ) ;
#20636 = SURFACE_STYLE_FILL_AREA ( #25212 ) ;
#20637 = DIRECTION ( 'NONE',  ( 0.000000000000000000, 1.000000000000000000, -0.000000000000000000 ) ) ;
#20638 = CARTESIAN_POINT ( 'NONE',  ( -0.4575609230677349926, -2.491211107078686648, -9.000000000000003553 ) ) ;
#20639 = ORIENTED_EDGE ( 'NONE', *, *, #47063, .F. ) ;
#20640 = VERTEX_POINT ( 'NONE', #24405 ) ;
#20641 = PLANE ( 'NONE',  #19487 ) ;
#20642 = VECTOR ( 'NONE', #6029, 1000.000000000000000 ) ;
#20643 = CARTESIAN_POINT ( 'NONE',  ( 6.826472737025121695, 114.6070736234661496, -4.959722759717905660 ) ) ;
#20644 = CIRCLE ( 'NONE', #2616, 1.000000000000000888 ) ;
#20645 = CIRCLE ( 'NONE', #59956, 5.000000000000000888 ) ;
#20646 = ADVANCED_FACE ( 'NONE', ( #45900 ), #32553, .T. ) ;
#20647 = FACE_OUTER_BOUND ( 'NONE', #31699, .T. ) ;
#20648 = CARTESIAN_POINT ( 'NONE',  ( 22.91454444302602411, 24.72107417156074760, -27.25824408850648695 ) ) ;
#20649 = ORIENTED_EDGE ( 'NONE', *, *, #68891, .F. ) ;
#20650 = ORIENTED_EDGE ( 'NONE', *, *, #12306, .F. ) ;
#20651 = CARTESIAN_POINT ( 'NONE',  ( -75.00000000000000000, 35.50862325381056905, -9.500000000000000000 ) ) ;
#20652 = EDGE_CURVE ( 'NONE', #53553, #69054, #20168, .T. ) ;
#20653 = COLOUR_RGB ( '', 0.09019608, 0.27058824, 0.51372549) ;
#20654 = CARTESIAN_POINT ( 'NONE',  ( -20.71938756518089875, 149.6378529145318907, 9.985383568374002650 ) ) ;
#20655 = EDGE_LOOP ( 'NONE', ( #11067, #9844, #64254, #11198 ) ) ;
#20656 = ADVANCED_FACE ( 'NONE', ( #52567 ), #19480, .F. ) ;
#20657 = CARTESIAN_POINT ( 'NONE',  ( -9.058813317711337021, 120.1549999999999869, -2.943386871421374895 ) ) ;
#20658 = CARTESIAN_POINT ( 'NONE',  ( 4.750000000000002665, 24.99999999999998579, -3.750000000000000000 ) ) ;
#20659 = ORIENTED_EDGE ( 'NONE', *, *, #40632, .F. ) ;
#20660 = PRESENTATION_LAYER_ASSIGNMENT (  '', '', ( #50988 ) ) ;
#20661 = CIRCLE ( 'NONE', #38628, 1.000000000000000888 ) ;
#20662 = CARTESIAN_POINT ( 'NONE',  ( 51.99999999999998579, 1.797044900979284448E-15, 11.50000000000000000 ) ) ;
#20663 = CARTESIAN_POINT ( 'NONE',  ( -100.6449999999999818, 4.716976649647091513, -6.492361379858946790 ) ) ;
#20664 = ORIENTED_EDGE ( 'NONE', *, *, #40930, .T. ) ;
#20665 = AXIS2_PLACEMENT_3D ( 'NONE', #43409, #12348, #17340 ) ;
#20666 = DIRECTION ( 'NONE',  ( -1.000000000000000000, 0.000000000000000000, 0.000000000000000000 ) ) ;
#20667 = CARTESIAN_POINT ( 'NONE',  ( -53.09292637653378932, 3.094860106618433360, 9.524999999999991473 ) ) ;
#20668 = ADVANCED_FACE ( 'NONE', ( #30717 ), #49414, .F. ) ;
#20669 =( LENGTH_UNIT ( ) NAMED_UNIT ( * ) SI_UNIT ( .MILLI., .METRE. ) );
#20670 = ORIENTED_EDGE ( 'NONE', *, *, #53546, .F. ) ;
#20671 = CARTESIAN_POINT ( 'NONE',  ( 2.607480562269076430, 152.7929263765338135, -8.025000000000000355 ) ) ;
#20672 = ADVANCED_FACE ( 'NONE', ( #29211 ), #66525, .F. ) ;
#20673 = DIRECTION ( 'NONE',  ( 0.000000000000000000, 0.000000000000000000, 1.000000000000000000 ) ) ;
#20674 = DIRECTION ( 'NONE',  ( -4.516179008354028246E-16, 0.000000000000000000, 1.000000000000000000 ) ) ;
#20675 = ORIENTED_EDGE ( 'NONE', *, *, #50651, .F. ) ;
#20676 =( LENGTH_UNIT ( ) NAMED_UNIT ( * ) SI_UNIT ( .MILLI., .METRE. ) );
#20677 = CARTESIAN_POINT ( 'NONE',  ( -45.89905495956738690, 9.405628579031729330, 3.000000000000000000 ) ) ;
#20678 = CARTESIAN_POINT ( 'NONE',  ( -140.8429263765338249, 9.058813317711329915, -2.943386871421373119 ) ) ;
#20679 = CARTESIAN_POINT ( 'NONE',  ( 66.49999999999998579, 34.24999999999999289, -3.750000000000000000 ) ) ;
#20680 = PRESENTATION_LAYER_ASSIGNMENT (  '', '', ( #19562 ) ) ;
#20681 = LINE ( 'NONE', #64953, #66798 ) ;
#20682 = CARTESIAN_POINT ( 'NONE',  ( -45.89905495956738690, 9.405628579031731107, -3.000000000000000444 ) ) ;
#20683 = AXIS2_PLACEMENT_3D ( 'NONE', #40323, #9356, #20229 ) ;
#20684 = CARTESIAN_POINT ( 'NONE',  ( -74.24147510199526323, 8.825811131586496217, 6.400570753484256414 ) ) ;
#20686 = FACE_OUTER_BOUND ( 'NONE', #13528, .T. ) ;
#20685 = CIRCLE ( 'NONE', #69003, 22.49999999999999645 ) ;
#20687 = CARTESIAN_POINT ( 'NONE',  ( 74.50000000000000000, 19.99999999999997868, -6.500000000000000000 ) ) ;
#20688 = CARTESIAN_POINT ( 'NONE',  ( -41.74416970038988950, -12.08331763868298658, 3.200680680164544878 ) ) ;
#20689 = VERTEX_POINT ( 'NONE', #34507 ) ;
#20690 = EDGE_LOOP ( 'NONE', ( #45694, #2892, #42647, #27887, #24871, #34820, #56678, #45780 ) ) ;
#20691 = CARTESIAN_POINT ( 'NONE',  ( 72.00000000000000000, 14.49137674618942562, 9.500000000000000000 ) ) ;
#20692 = PRESENTATION_LAYER_ASSIGNMENT (  '', '', ( #57753 ) ) ;
#20693 = ORIENTED_EDGE ( 'NONE', *, *, #5972, .T. ) ;
#20694 = CARTESIAN_POINT ( 'NONE',  ( 62.10000000000000142, 11.99999999999999822, -3.499999999999999556 ) ) ;
#20695 = CARTESIAN_POINT ( 'NONE',  ( -172.7049999999999841, 2.607480562269073321, 8.024999999999991473 ) ) ;
#20696 = CARTESIAN_POINT ( 'NONE',  ( -90.74292637653380211, -5.598654528085803328, -7.705886871421366635 ) ) ;
#20697 = EDGE_CURVE ( 'NONE', #37155, #6425, #31406, .T. ) ;
#20698 = CARTESIAN_POINT ( 'NONE',  ( -19.00000000000000000, 8.000000000000000000, 3.500000000000003997 ) ) ;
#20699 = CARTESIAN_POINT ( 'NONE',  ( -46.70707362346617231, -3.094860106618431139, -9.524999999999991473 ) ) ;
#20700 = PRESENTATION_LAYER_ASSIGNMENT (  '', '', ( #65626 ) ) ;
#20701 = CARTESIAN_POINT ( 'NONE',  ( -179.2449999999999761, -4.716976649647093289, -6.492361379858945902 ) ) ;
#20702 = EDGE_CURVE ( 'NONE', #12003, #26708, #51045, .T. ) ;
#20703 = VERTEX_POINT ( 'NONE', #62281 ) ;
#20704 = CIRCLE ( 'NONE', #21808, 1.000000000000000888 ) ;
#20705 = FILL_AREA_STYLE ('',( #4489 ) ) ;
#20706 = CARTESIAN_POINT ( 'NONE',  ( -10.51151497852317718, 11.79546843913625231, 2.227144960977124999 ) ) ;
#20707 = CARTESIAN_POINT ( 'NONE',  ( -90.95499999999999829, -7.632228543268599452, 2.479861379858951054 ) ) ;
#20708 = CYLINDRICAL_SURFACE ( 'NONE', #49986, 0.5000000000000004441 ) ;
#20709 = CIRCLE ( 'NONE', #63382, 0.5000000000000004441 ) ;
#20710 = CARTESIAN_POINT ( 'NONE',  ( -89.24499999999999034, -4.716976649647093289, -6.492361379858945902 ) ) ;
#20711 = CARTESIAN_POINT ( 'NONE',  ( -9.058813317711338797, 129.4549999999999841, 2.943386871421373563 ) ) ;
#20712 = CARTESIAN_POINT ( 'NONE',  ( -75.00000000000000000, 7.967158085982124049, -7.000000000000000888 ) ) ;
#20713 = CIRCLE ( 'NONE', #44360, 22.00000000000001421 ) ;
#20714 = COLOUR_RGB ( '', 0.31764706, 0.68627451, 0.89019608) ;
#20715 = FACE_OUTER_BOUND ( 'NONE', #53062, .T. ) ;
#20716 = DIRECTION ( 'NONE',  ( 0.000000000000000000, 0.000000000000000000, 1.000000000000000000 ) ) ;
#20717 = UNCERTAINTY_MEASURE_WITH_UNIT (LENGTH_MEASURE( 1.000000000000000082E-05 ), #1473, 'distance_accuracy_value', 'NONE');
#20718 = CARTESIAN_POINT ( 'NONE',  ( 8.000000000000000000, 33.74999999999998579, 3.750000000000000000 ) ) ;
#20719 = CARTESIAN_POINT ( 'NONE',  ( -48.29292637653378506, 3.094860106618428031, -9.524999999999993250 ) ) ;
#20720 = EDGE_LOOP ( 'NONE', ( #19421, #17332, #41465, #61809 ) ) ;
#20721 = CARTESIAN_POINT ( 'NONE',  ( -8.437984349512095861, 132.6929263765338192, -5.166775262442723748E-16 ) ) ;
#20722 = AXIS2_PLACEMENT_3D ( 'NONE', #8784, #35169, #40470 ) ;
#20723 = LINE ( 'NONE', #63626, #26966 ) ;
#20724 = EDGE_CURVE ( 'NONE', #38702, #36309, #50507, .T. ) ;
#20726 = CARTESIAN_POINT ( 'NONE',  ( -48.00000000000000000, 99.99999999999992895, 7.500000000000000000 ) ) ;
#20725 = CARTESIAN_POINT ( 'NONE',  ( 7.750000000000000000, 33.74999999999998579, 4.000000000000000000 ) ) ;
#20727 = DIRECTION ( 'NONE',  ( 0.7833176619561891263, 0.6216216216216174928, -0.000000000000000000 ) ) ;
#20728 = ORIENTED_EDGE ( 'NONE', *, *, #8684, .F. ) ;
#20729 = EDGE_LOOP ( 'NONE', ( #55048, #49718, #3973, #41193 ) ) ;
#20730 = FACE_OUTER_BOUND ( 'NONE', #66054, .T. ) ;
#20731 = AXIS2_PLACEMENT_3D ( 'NONE', #16605, #38067, #59461 ) ;
#20732 =( NAMED_UNIT ( * ) SI_UNIT ( $, .STERADIAN. ) SOLID_ANGLE_UNIT ( ) );
#20733 = MECHANICAL_DESIGN_GEOMETRIC_PRESENTATION_REPRESENTATION (  '', ( #69049 ), #57798 ) ;
#20734 =( BOUNDED_SURFACE ( )  B_SPLINE_SURFACE ( 3, 2, ( 
 ( #8894, #3570, #40938 ),
 ( #51458, #30319, #25073 ),
 ( #62362, #46580, #29658 ),
 ( #50773, #19795, #50421 ),
 ( #34572, #2145, #18415 ),
 ( #39902, #13119, #56025 ),
 ( #7841, #24027, #45536 ),
 ( #66952, #18752, #61998 ),
 ( #51127, #9947, #41628 ),
 ( #4646, #58472, #48301 ) ),
 .UNSPECIFIED., .F., .F., .F. ) 
 B_SPLINE_SURFACE_WITH_KNOTS ( ( 4, 2, 2, 2, 4 ),
 ( 3, 3 ),
 ( 0.0004231141141892710367, 0.0008386083364002310404, 0.001254102558611191152, 0.001669596780822151265, 0.002085091003033111377 ),
 ( 0.000000000000000000, 1.000000000000000000 ),
 .UNSPECIFIED. ) 
 GEOMETRIC_REPRESENTATION_ITEM ( )  RATIONAL_B_SPLINE_SURFACE ( (
 ( 1.000000000000000000, 0.7071067811865573427, 1.000000000000000000),
 ( 1.000000000000000000, 0.7275888720224806816, 1.000000000000000000),
 ( 1.000000000000000000, 0.7463828630404263365, 1.000000000000000000),
 ( 1.000000000000000000, 0.7812714640742435268, 1.000000000000000000),
 ( 1.000000000000000000, 0.7963642535525788935, 1.000000000000000000),
 ( 1.000000000000000000, 0.8224433532025096083, 1.000000000000000000),
 ( 1.000000000000000000, 0.8326146287104877475, 1.000000000000000000),
 ( 1.000000000000000000, 0.8468497872537316118, 1.000000000000000000),
 ( 1.000000000000000000, 0.8504932968929420634, 1.000000000000000000),
 ( 1.000000000000000000, 0.8505317485662416965, 1.000000000000000000) ) ) 
 REPRESENTATION_ITEM ( '' )  SURFACE ( )  );
#20735 = EDGE_CURVE ( 'NONE', #68501, #46540, #12317, .T. ) ;
#20736 = AXIS2_PLACEMENT_3D ( 'NONE', #19989, #51684, #31235 ) ;
#20737 = CARTESIAN_POINT ( 'NONE',  ( -3.000000000000000444, 0.000000000000000000, 7.500000000000000000 ) ) ;
#20738 = DIRECTION ( 'NONE',  ( -1.000000000000000000, -0.000000000000000000, -0.000000000000000000 ) ) ;
#20739 = SURFACE_STYLE_USAGE ( .BOTH. , #36253 ) ;
#20740 = VERTEX_POINT ( 'NONE', #28867 ) ;
#20741 = CARTESIAN_POINT ( 'NONE',  ( -125.4549999999999841, 7.632228543268599452, -2.479861379858951942 ) ) ;
#20742 = EDGE_LOOP ( 'NONE', ( #34763, #20458, #53178, #34084, #60857, #56738, #4930 ) ) ;
#20743 = DIRECTION ( 'NONE',  ( 0.000000000000000000, -1.000000000000000000, 0.000000000000000000 ) ) ;
#20744 = CARTESIAN_POINT ( 'NONE',  ( 4.716976649647096842, 128.8570736234661638, 6.492361379858953896 ) ) ;
#20745 = EDGE_CURVE ( 'NONE', #53126, #38818, #23951, .T. ) ;
#20746 = VERTEX_POINT ( 'NONE', #61560 ) ;
#20747 =( LENGTH_UNIT ( ) NAMED_UNIT ( * ) SI_UNIT ( .MILLI., .METRE. ) );
#20748 = DIRECTION ( 'NONE',  ( 1.000000000000000000, -0.000000000000000000, 0.000000000000000000 ) ) ;
#20749 = ORIENTED_EDGE ( 'NONE', *, *, #60564, .F. ) ;
#20750 = DIRECTION ( 'NONE',  ( 0.000000000000000000, 0.000000000000000000, -1.000000000000000000 ) ) ;
#20751 = CARTESIAN_POINT ( 'NONE',  ( 9.058813317711338797, 153.8449999999999704, -2.943386871421372675 ) ) ;
#20752 = FACE_OUTER_BOUND ( 'NONE', #31719, .T. ) ;
#20753 = STYLED_ITEM ( 'NONE', ( #46886 ), #27294 ) ;
#20754 = ORIENTED_EDGE ( 'NONE', *, *, #50683, .F. ) ;
#20755 = VECTOR ( 'NONE', #5952, 1000.000000000000000 ) ;
#20756 = CARTESIAN_POINT ( 'NONE',  ( -55.25707362346615525, 5.598654528085800663, -7.705886871421367523 ) ) ;
#20757 = CARTESIAN_POINT ( 'NONE',  ( -5.598654528085806881, 152.8549999999999898, -7.705886871421374629 ) ) ;
#20758 = CARTESIAN_POINT ( 'NONE',  ( -135.0570736234661808, 0.000000000000000000, 9.524999999999991473 ) ) ;
#20759 = DIRECTION ( 'NONE',  ( 0.000000000000000000, 0.000000000000000000, 1.000000000000000000 ) ) ;
#20760 = ORIENTED_EDGE ( 'NONE', *, *, #60080, .T. ) ;
#20761 = CARTESIAN_POINT ( 'NONE',  ( -9.827790563157511022E-16, 121.4429263765338050, 8.025000000000000355 ) ) ;
#20762 = CARTESIAN_POINT ( 'NONE',  ( -195.0000000000000000, 0.000000000000000000, 9.524999999999991473 ) ) ;
#20763 = UNCERTAINTY_MEASURE_WITH_UNIT (LENGTH_MEASURE( 1.000000000000000082E-05 ), #3119, 'distance_accuracy_value', 'NONE');
#20764 =( NAMED_UNIT ( * ) SI_UNIT ( $, .STERADIAN. ) SOLID_ANGLE_UNIT ( ) );
#20765 = CARTESIAN_POINT ( 'NONE',  ( 44.99999999999999289, 10.00436330937146145, 6.147562757269795952 ) ) ;
#20766 = EDGE_CURVE ( 'NONE', #44158, #69107, #55959, .T. ) ;
#20767 = ORIENTED_EDGE ( 'NONE', *, *, #38509, .F. ) ;
#20768 = DIRECTION ( 'NONE',  ( 0.000000000000000000, 1.000000000000000000, 0.000000000000000000 ) ) ;
#20769 = EDGE_LOOP ( 'NONE', ( #15732, #13267, #2354 ) ) ;
#20770 = CARTESIAN_POINT ( 'NONE',  ( -55.34292637653378932, -9.058813317711329915, 2.943386871421371787 ) ) ;
#20771 = AXIS2_PLACEMENT_3D ( 'NONE', #24269, #33862, #61899 ) ;
#20772 = AXIS2_PLACEMENT_3D ( 'NONE', #18495, #39624, #49816 ) ;
#20773 = CARTESIAN_POINT ( 'NONE',  ( -4.000000000000000000, -2.499999999999999556, 0.000000000000000000 ) ) ;
#20774 = CARTESIAN_POINT ( 'NONE',  ( -156.8050000000000068, -8.437984349512085203, 5.166775262442717831E-16 ) ) ;
#20775 = ORIENTED_EDGE ( 'NONE', *, *, #16800, .F. ) ;
#20776 = SURFACE_SIDE_STYLE ('',( #49236 ) ) ;
#20777 = UNCERTAINTY_MEASURE_WITH_UNIT (LENGTH_MEASURE( 1.000000000000000082E-05 ), #1128, 'distance_accuracy_value', 'NONE');
#20778 = CARTESIAN_POINT ( 'NONE',  ( -5.705565085145812176, -4.117671386636407860, 0.02778322089669425093 ) ) ;
#20779 = CARTESIAN_POINT ( 'NONE',  ( -48.50000000000000000, 14.49137674618942384, -7.500000000000000000 ) ) ;
#20780 = CARTESIAN_POINT ( 'NONE',  ( 4.716976649647096842, 145.7429263765338305, 6.492361379858953896 ) ) ;
#20781 = VERTEX_POINT ( 'NONE', #18688 ) ;
#20782 = CIRCLE ( 'NONE', #3869, 8.999999999999994671 ) ;
#20783 = ORIENTED_EDGE ( 'NONE', *, *, #1587, .F. ) ;
#20784 = DIRECTION ( 'NONE',  ( 0.000000000000000000, 0.000000000000000000, -1.000000000000000000 ) ) ;
#20785 = CARTESIAN_POINT ( 'NONE',  ( -1.000000000000028644, 0.000000000000000000, 11.99999999999999645 ) ) ;
#20786 = CARTESIAN_POINT ( 'NONE',  ( -70.55499999999999261, 0.000000000000000000, 8.024999999999991473 ) ) ;
#20788 = ORIENTED_EDGE ( 'NONE', *, *, #40060, .F. ) ;
#20787 = MECHANICAL_DESIGN_GEOMETRIC_PRESENTATION_REPRESENTATION (  '', ( #33135 ), #29752 ) ;
#20789 = DIRECTION ( 'NONE',  ( -0.000000000000000000, -0.000000000000000000, -1.000000000000000000 ) ) ;
#20790 = CARTESIAN_POINT ( 'NONE',  ( 54.50000000000002132, 2.470600640510325790E-15, 12.00000000000000000 ) ) ;
#20791 = AXIS2_PLACEMENT_3D ( 'NONE', #67444, #31450, #26179 ) ;
#20792 = FILL_AREA_STYLE_COLOUR ( '', #36302 ) ;
#20793 = DIRECTION ( 'NONE',  ( 0.000000000000000000, 0.000000000000000000, -1.000000000000000000 ) ) ;
#20794 = ORIENTED_EDGE ( 'NONE', *, *, #32984, .T. ) ;
#20795 = DIRECTION ( 'NONE',  ( -0.000000000000000000, -1.000000000000000000, -0.000000000000000000 ) ) ;
#20796 = AXIS2_PLACEMENT_3D ( 'NONE', #20623, #62483, #42136 ) ;
#20797 = CARTESIAN_POINT ( 'NONE',  ( 7.750000000000001776, 31.24999999999998579, -4.000000000000000000 ) ) ;
#20798 = DIRECTION ( 'NONE',  ( -0.000000000000000000, -0.000000000000000000, 1.000000000000000000 ) ) ;
#20799 = SURFACE_STYLE_FILL_AREA ( #68993 ) ;
#20800 = CARTESIAN_POINT ( 'NONE',  ( -119.3949999999999676, -6.826472737025113702, -4.959722759717900331 ) ) ;
#20801 = CARTESIAN_POINT ( 'NONE',  ( -3.094860106618432471, 148.5949999999999704, -9.525000000000000355 ) ) ;
#20802 = CARTESIAN_POINT ( 'NONE',  ( -86.69499999999999318, -8.437984349512085203, 5.166775262442717831E-16 ) ) ;
#20803 =( LENGTH_UNIT ( ) NAMED_UNIT ( * ) SI_UNIT ( .MILLI., .METRE. ) );
#20804 = CARTESIAN_POINT ( 'NONE',  ( 66.24999999999998579, 34.24999999999999289, -3.750000000000000000 ) ) ;
#20805 = UNCERTAINTY_MEASURE_WITH_UNIT (LENGTH_MEASURE( 1.000000000000000082E-05 ), #34571, 'distance_accuracy_value', 'NONE');
#20806 = DIRECTION ( 'NONE',  ( 0.000000000000000000, 0.000000000000000000, 1.000000000000000000 ) ) ;
#20807 = AXIS2_PLACEMENT_3D ( 'NONE', #14026, #62882, #52377 ) ;
#20808 = VERTEX_POINT ( 'NONE', #13387 ) ;
#20809 = CARTESIAN_POINT ( 'NONE',  ( -129.4429263765338192, -1.166476076187852838E-15, -9.524999999999991473 ) ) ;
#20810 = SHAPE_REPRESENTATION_RELATIONSHIP ( 'NONE' , 'NONE' ,  #46015, #57167 ) ;
#20811 = LINE ( 'NONE', #52830, #34356 ) ;
#20812 = CARTESIAN_POINT ( 'NONE',  ( -157.7950000000000159, 2.607480562269068880, -8.024999999999993250 ) ) ;
#20813 = PRESENTATION_STYLE_ASSIGNMENT (( #36327 ) ) ;
#20814 =( GEOMETRIC_REPRESENTATION_CONTEXT ( 3 ) GLOBAL_UNCERTAINTY_ASSIGNED_CONTEXT ( ( #16507 ) ) GLOBAL_UNIT_ASSIGNED_CONTEXT ( ( #48435, #59262, #31855 ) ) REPRESENTATION_CONTEXT ( 'NONE', 'WORKASPACE' ) );
#20815 = ADVANCED_FACE ( 'NONE', ( #34848 ), #24294, .T. ) ;
#20816 = DIRECTION ( 'NONE',  ( -1.000000000000000000, -0.000000000000000000, -0.000000000000000000 ) ) ;
#20817 = COLOUR_RGB ( '', 0.72549020, 0.75294118, 0.79215686) ;
#20818 = SURFACE_SIDE_STYLE ('',( #69007 ) ) ;
#20819 = EDGE_LOOP ( 'NONE', ( #49510, #25854, #9611, #51129, #1396 ) ) ;
#20820 = ORIENTED_EDGE ( 'NONE', *, *, #30147, .F. ) ;
#20821 = LINE ( 'NONE', #4243, #18416 ) ;
#20822 = CARTESIAN_POINT ( 'NONE',  ( -143.2429263765338021, 5.598654528085804216, 7.705886871421366635 ) ) ;
#20823 = CARTESIAN_POINT ( 'NONE',  ( -45.00000000000000000, 9.609776836748578077, 6.329322064279326199 ) ) ;
#20824 = CARTESIAN_POINT ( 'NONE',  ( 34.99999999999992895, 109.9999999999999858, -9.500000000000000000 ) ) ;
#20825 = ORIENTED_EDGE ( 'NONE', *, *, #52921, .F. ) ;
#20826 = CARTESIAN_POINT ( 'NONE',  ( -148.8549999999999898, 4.716976649647094177, 6.492361379858945902 ) ) ;
#20827 = EDGE_CURVE ( 'NONE', #5819, #13735, #29924, .T. ) ;
#20828 = ORIENTED_EDGE ( 'NONE', *, *, #50526, .F. ) ;
#20829 = CARTESIAN_POINT ( 'NONE',  ( 27.00000000000001776, -60.04052944165106709, -35.50000000000000000 ) ) ;
#20830 = CARTESIAN_POINT ( 'NONE',  ( 10.00000000000001954, 43.00000000000000000, -29.68999999999999417 ) ) ;
#20832 = ORIENTED_EDGE ( 'NONE', *, *, #40446, .T. ) ;
#20831 = ADVANCED_FACE ( 'NONE', ( #40863 ), #24254, .T. ) ;
#20833 = AXIS2_PLACEMENT_3D ( 'NONE', #53212, #58473, #16629 ) ;
#20834 = EDGE_CURVE ( 'NONE', #23161, #21193, #22433, .T. ) ;
#20835 = CARTESIAN_POINT ( 'NONE',  ( -13.50000000000000533, 30.74999999999999289, -3.750000000000000000 ) ) ;
#20836 = CARTESIAN_POINT ( 'NONE',  ( 10.01517768586949231, 117.6949999999999790, 1.839758294383810543E-15 ) ) ;
#20837 = DIRECTION ( 'NONE',  ( 0.000000000000000000, -0.7071067811865469066, -0.7071067811865482389 ) ) ;
#20838 = CIRCLE ( 'NONE', #10740, 0.5000000000000004441 ) ;
#20839 = ORIENTED_EDGE ( 'NONE', *, *, #39057, .F. ) ;
#20840 = DIRECTION ( 'NONE',  ( -0.000000000000000000, -0.000000000000000000, -1.000000000000000000 ) ) ;
#20842 = EDGE_CURVE ( 'NONE', #30586, #50171, #29098, .T. ) ;
#20841 = CARTESIAN_POINT ( 'NONE',  ( 9.058813317711338797, 121.9549999999999841, -2.943386871421372675 ) ) ;
#20843 = CARTESIAN_POINT ( 'NONE',  ( -67.85499999999998977, 4.716976649647094177, 6.492361379858945902 ) ) ;
#20844 = CIRCLE ( 'NONE', #47862, 0.2500000000000002220 ) ;
#20845 = CARTESIAN_POINT ( 'NONE',  ( -157.9429263765338192, 0.000000000000000000, 9.524999999999991473 ) ) ;
#20846 = ORIENTED_EDGE ( 'NONE', *, *, #65904, .F. ) ;
#20847 = CARTESIAN_POINT ( 'NONE',  ( -1.166476076187854022E-15, 151.0550000000000068, 9.525000000000000355 ) ) ;
#20848 = UNCERTAINTY_MEASURE_WITH_UNIT (LENGTH_MEASURE( 1.000000000000000082E-05 ), #64198, 'distance_accuracy_value', 'NONE');
#20849 = CARTESIAN_POINT ( 'NONE',  ( 22.00000000000000355, 43.00000000000000000, -75.00000000000001421 ) ) ;
#20850 = EDGE_CURVE ( 'NONE', #9272, #61826, #68481, .T. ) ;
#20851 = SURFACE_STYLE_USAGE ( .BOTH. , #52182 ) ;
#20852 = DIRECTION ( 'NONE',  ( 1.000000000000000000, 0.000000000000000000, 0.000000000000000000 ) ) ;
#20853 = VERTEX_POINT ( 'NONE', #18649 ) ;
#20854 = LINE ( 'NONE', #52872, #66496 ) ;
#20855 = CARTESIAN_POINT ( 'NONE',  ( -183.8050000000000068, -8.437984349512085203, 5.166775262442717831E-16 ) ) ;
#20856 = VERTEX_POINT ( 'NONE', #29165 ) ;
#20857 = DIRECTION ( 'NONE',  ( 0.000000000000000000, 0.000000000000000000, 1.000000000000000000 ) ) ;
#20858 = COLOUR_RGB ( '', 0.66274510, 0.83137255, 0.94901961) ;
#20859 = CARTESIAN_POINT ( 'NONE',  ( 0.000000000000000000, 111.9999999999999858, 0.000000000000000000 ) ) ;
#20860 = EDGE_LOOP ( 'NONE', ( #42481, #42232, #14027, #30313 ) ) ;
#20861 = CARTESIAN_POINT ( 'NONE',  ( -121.5570736234661808, -1.166476076187852838E-15, -9.524999999999991473 ) ) ;
#20862 = FACE_OUTER_BOUND ( 'NONE', #42694, .T. ) ;
#20863 = ORIENTED_EDGE ( 'NONE', *, *, #1631, .T. ) ;
#20864 = CARTESIAN_POINT ( 'NONE',  ( 0.000000000000000000, 0.000000000000000000, 0.000000000000000000 ) ) ;
#20865 = FILL_AREA_STYLE_COLOUR ( '', #50519 ) ;
#20866 = CARTESIAN_POINT ( 'NONE',  ( -91.70499999999998408, 2.607480562269073321, 8.024999999999991473 ) ) ;
#20867 = EDGE_LOOP ( 'NONE', ( #56275, #68341, #25591 ) ) ;
#20868 = FACE_OUTER_BOUND ( 'NONE', #43404, .T. ) ;
#20869 = CIRCLE ( 'NONE', #9683, 3.000000000000000444 ) ;
#20870 = CARTESIAN_POINT ( 'NONE',  ( -133.5570736234661808, -1.166476076187852838E-15, -9.524999999999991473 ) ) ;
#20871 = CIRCLE ( 'NONE', #53451, 0.5000000000000004441 ) ;
#20872 = CARTESIAN_POINT ( 'NONE',  ( 5.598654528085805993, 150.2449999999999761, 7.705886871421374629 ) ) ;
#20873 = CARTESIAN_POINT ( 'NONE',  ( -65.30707362346618083, -10.01517768586948698, 6.132527647946031529E-16 ) ) ;
#20874 = CARTESIAN_POINT ( 'NONE',  ( -81.14292637653380780, 5.598654528085800663, -7.705886871421367523 ) ) ;
#20875 = ORIENTED_EDGE ( 'NONE', *, *, #27572, .F. ) ;
#20876 = FACE_OUTER_BOUND ( 'NONE', #11671, .T. ) ;
#20877 = PRESENTATION_STYLE_ASSIGNMENT (( #52212 ) ) ;
#20878 = CARTESIAN_POINT ( 'NONE',  ( -111.8049999999999784, -8.437984349512085203, 5.166775262442717831E-16 ) ) ;
#20879 = CARTESIAN_POINT ( 'NONE',  ( -9.058813317711337021, 116.0449999999999875, -2.943386871421374895 ) ) ;
#20880 = CARTESIAN_POINT ( 'NONE',  ( -125.2449999999999903, -4.716976649647093289, -6.492361379858945902 ) ) ;
#20881 = AXIS2_PLACEMENT_3D ( 'NONE', #23501, #930, #11925 ) ;
#20882 = VECTOR ( 'NONE', #12350, 1000.000000000000000 ) ;
#20883 = CARTESIAN_POINT ( 'NONE',  ( 17.15973193263811680, -3.000000000000000000, 2.000000000000000000 ) ) ;
#20884 = AXIS2_PLACEMENT_3D ( 'NONE', #6978, #17885, #23170 ) ;
#20885 = FILL_AREA_STYLE_COLOUR ( '', #27849 ) ;
#20886 = ORIENTED_EDGE ( 'NONE', *, *, #30898, .F. ) ;
#20887 = CIRCLE ( 'NONE', #55671, 0.9999999999999986677 ) ;
#20888 = CARTESIAN_POINT ( 'NONE',  ( -165.8929263765338078, -8.102448949553172852, -5.886773742842741797 ) ) ;
#20889 = SURFACE_SIDE_STYLE ('',( #25801 ) ) ;
#20890 = EDGE_CURVE ( 'NONE', #28212, #12977, #60622, .T. ) ;
#20891 = LINE ( 'NONE', #68747, #23662 ) ;
#20892 = SURFACE_STYLE_FILL_AREA ( #25807 ) ;
#20893 = DIRECTION ( 'NONE',  ( -0.000000000000000000, 1.000000000000000000, -0.000000000000000000 ) ) ;
#20894 = ORIENTED_EDGE ( 'NONE', *, *, #34383, .F. ) ;
#20895 = CARTESIAN_POINT ( 'NONE',  ( -71.99292637653381632, 8.102448949553171076, -5.886773742842744461 ) ) ;
#20896 = ITEM_DEFINED_TRANSFORMATION ( 'NONE', 'NONE', #39413,  #42840 ) ;
#20898 = EDGE_CURVE ( 'NONE', #55490, #41057, #39334, .T. ) ;
#20897 = LINE ( 'NONE', #52581, #50948 ) ;
#20899 = COLOUR_RGB ( '', 0.08235294, 0.09019608, 0.10196078) ;
#20900 = SURFACE_STYLE_USAGE ( .BOTH. , #32462 ) ;
#20901 = DIRECTION ( 'NONE',  ( 1.000000000000000000, -0.000000000000000000, 0.000000000000000000 ) ) ;
#20902 = LINE ( 'NONE', #59550, #42666 ) ;
#20903 = ADVANCED_FACE ( 'NONE', ( #51347 ), #18961, .T. ) ;
#20904 = AXIS2_PLACEMENT_3D ( 'NONE', #24535, #41125, #46049 ) ;
#20905 = CARTESIAN_POINT ( 'NONE',  ( -182.9049999999999727, 2.607480562269069324, -8.024999999999993250 ) ) ;
#20906 = ORIENTED_EDGE ( 'NONE', *, *, #41645, .T. ) ;
#20907 = FACE_OUTER_BOUND ( 'NONE', #11485, .T. ) ;
#20908 =( NAMED_UNIT ( * ) PLANE_ANGLE_UNIT ( ) SI_UNIT ( $, .RADIAN. ) );
#20909 = EDGE_CURVE ( 'NONE', #27901, #54497, #66845, .T. ) ;
#20910 = CARTESIAN_POINT ( 'NONE',  ( 13.50000000000000355, 28.24999999999998934, -3.750000000000000000 ) ) ;
#20912 = ORIENTED_EDGE ( 'NONE', *, *, #4778, .F. ) ;
#20911 = MECHANICAL_DESIGN_GEOMETRIC_PRESENTATION_REPRESENTATION (  '', ( #5166 ), #44553 ) ;
#20913 = AXIS2_PLACEMENT_3D ( 'NONE', #41902, #5245, #68954 ) ;
#20914 = CARTESIAN_POINT ( 'NONE',  ( -110.5429263765337993, 9.058813317711329915, 2.943386871421369566 ) ) ;
#20915 = AXIS2_PLACEMENT_3D ( 'NONE', #65006, #12934, #28044 ) ;
#20916 =( LENGTH_UNIT ( ) NAMED_UNIT ( * ) SI_UNIT ( .MILLI., .METRE. ) );
#20917 = CARTESIAN_POINT ( 'NONE',  ( -4.716976649647097730, 139.3570736234661638, -6.492361379858953896 ) ) ;
#20918 = VERTEX_POINT ( 'NONE', #67170 ) ;
#20920 = EDGE_CURVE ( 'NONE', #8229, #25042, #67369, .T. ) ;
#20919 = CARTESIAN_POINT ( 'NONE',  ( -100.8570736234661780, -5.598654528085803328, -7.705886871421366635 ) ) ;
#20921 = CARTESIAN_POINT ( 'NONE',  ( -95.60499999999997556, 6.826472737025113702, -4.959722759717902107 ) ) ;
#20922 = UNCERTAINTY_MEASURE_WITH_UNIT (LENGTH_MEASURE( 1.000000000000000082E-05 ), #37755, 'distance_accuracy_value', 'NONE');
#20923 = DIRECTION ( 'NONE',  ( 0.000000000000000000, -0.6691306063588592368, -0.7431448254773934670 ) ) ;
#20924 = VERTEX_POINT ( 'NONE', #51000 ) ;
#20925 = CARTESIAN_POINT ( 'NONE',  ( 3.109477999331718312, -1.987149502472170370, -9.000000000000005329 ) ) ;
#20926 =( GEOMETRIC_REPRESENTATION_CONTEXT ( 3 ) GLOBAL_UNCERTAINTY_ASSIGNED_CONTEXT ( ( #41205 ) ) GLOBAL_UNIT_ASSIGNED_CONTEXT ( ( #36626, #4896, #31264 ) ) REPRESENTATION_CONTEXT ( 'NONE', 'WORKASPACE' ) );
#20927 = DIRECTION ( 'NONE',  ( 0.6402681315062923595, 0.000000000000000000, 0.7681514953298217430 ) ) ;
#20928 = CARTESIAN_POINT ( 'NONE',  ( 14.09999999999999609, 11.99999999999999289, 3.500000000000004885 ) ) ;
#20929 = CARTESIAN_POINT ( 'NONE',  ( 10.00000000000002132, 43.00000000000000000, 90.00000000000000000 ) ) ;
#20930 = STYLED_ITEM ( 'NONE', ( #56393 ), #1457 ) ;
#20931 = ORIENTED_EDGE ( 'NONE', *, *, #60425, .T. ) ;
#20932 = CARTESIAN_POINT ( 'NONE',  ( -76.94499999999997897, -9.827790563157499189E-16, -8.024999999999991473 ) ) ;
#20933 = EDGE_LOOP ( 'NONE', ( #54475, #60231, #68976, #32346 ) ) ;
#20934 = VECTOR ( 'NONE', #42424, 1000.000000000000114 ) ;
#20935 = CARTESIAN_POINT ( 'NONE',  ( 8.750000000000001776, 25.24999999999998934, 4.000000000000000000 ) ) ;
#20936 = CARTESIAN_POINT ( 'NONE',  ( -120.9570736234661865, 9.058813317711329915, -2.943386871421373119 ) ) ;
#20937 = ORIENTED_EDGE ( 'NONE', *, *, #24599, .F. ) ;
#20938 = PLANE ( 'NONE',  #958 ) ;
#20939 = B_SPLINE_CURVE_WITH_KNOTS ( 'NONE', 3,
 ( #35416, #23449, #44956, #66362, #56866, #2276, #8680, #55814 ),
 .UNSPECIFIED., .F., .F.,
 ( 4, 2, 2, 4 ),
 ( 2.544313220891868126E-07, 0.002693395767724533589, 0.004039966435925756300, 0.005386537104126978143 ),
 .UNSPECIFIED. ) ;
#20940 = PRESENTATION_STYLE_ASSIGNMENT (( #68794 ) ) ;
#20941 = CARTESIAN_POINT ( 'NONE',  ( -74.99999999999998579, 8.062885929673678120, 5.900610682603717017 ) ) ;
#20942 = EDGE_LOOP ( 'NONE', ( #37427, #62579, #4032, #48731 ) ) ;
#20943 = CARTESIAN_POINT ( 'NONE',  ( -9.566487832665403701, 1.863712308906138704, -1.430357023834059271 ) ) ;
#20944 = ORIENTED_EDGE ( 'NONE', *, *, #12714, .T. ) ;
#20945 = LINE ( 'NONE', #37865, #14499 ) ;
#20946 = CARTESIAN_POINT ( 'NONE',  ( 4.500000000000002665, 22.24999999999998579, 3.750000000000000000 ) ) ;
#20947 = CARTESIAN_POINT ( 'NONE',  ( -156.5070736234661126, 8.102448949553176405, 5.886773742842740909 ) ) ;
#20948 = CARTESIAN_POINT ( 'NONE',  ( -8.102448949553179958, 119.4949999999999903, 5.886773742842747126 ) ) ;
#20949 = CARTESIAN_POINT ( 'NONE',  ( -107.1570736234661751, -9.058813317711329915, -2.943386871421370898 ) ) ;
#20950 = EDGE_CURVE ( 'NONE', #62934, #25473, #48338, .T. ) ;
#20951 = CARTESIAN_POINT ( 'NONE',  ( -1.113559396844004956, 154.5000000000000000, -9.459683423334018570 ) ) ;
#20952 = PRODUCT_DEFINITION_SHAPE ( 'NONE', 'NONE',  #7683 ) ;
#20953 = ORIENTED_EDGE ( 'NONE', *, *, #32512, .T. ) ;
#20954 = FILL_AREA_STYLE_COLOUR ( '', #33984 ) ;
#20956 = SURFACE_STYLE_FILL_AREA ( #48077 ) ;
#20955 = DIRECTION ( 'NONE',  ( 0.000000000000000000, -1.000000000000000000, 0.000000000000000000 ) ) ;
#20958 = CARTESIAN_POINT ( 'NONE',  ( -2.607480562269115509, 130.2070736234661865, -8.024999999999970157 ) ) ;
#20957 = CIRCLE ( 'NONE', #60257, 0.2500000000000002220 ) ;
#20959 = CARTESIAN_POINT ( 'NONE',  ( -144.0549999999999784, -9.827790563157499189E-16, -8.024999999999991473 ) ) ;
#20960 = FACE_OUTER_BOUND ( 'NONE', #51442, .T. ) ;
#20961 = MECHANICAL_DESIGN_GEOMETRIC_PRESENTATION_REPRESENTATION (  '', ( #23220 ), #10856 ) ;
#20962 = DIRECTION ( 'NONE',  ( 0.000000000000000000, 1.000000000000000000, 0.000000000000000000 ) ) ;
#20963 = CARTESIAN_POINT ( 'NONE',  ( -157.3449999999999989, 7.632228543268599452, -2.479861379858951942 ) ) ;
#20964 = CARTESIAN_POINT ( 'NONE',  ( -140.5450000000000159, -7.632228543268600340, -2.479861379858950166 ) ) ;
#20965 = ORIENTED_EDGE ( 'NONE', *, *, #57927, .T. ) ;
#20966 = CARTESIAN_POINT ( 'NONE',  ( -9.250000000000003553, 27.74999999999998934, -4.000000000000000000 ) ) ;
#20967 = CARTESIAN_POINT ( 'NONE',  ( 20.71231517720797655, 149.4999999999999716, -10.00000000000000000 ) ) ;
#20968 = CARTESIAN_POINT ( 'NONE',  ( -57.80499999999998550, -8.437984349512085203, 5.166775262442717831E-16 ) ) ;
#20969 = DIRECTION ( 'NONE',  ( -1.000000000000000000, 0.000000000000000000, 0.000000000000000000 ) ) ;
#20970 = EDGE_CURVE ( 'NONE', #21622, #50178, #8449, .T. ) ;
#20971 = AXIS2_PLACEMENT_3D ( 'NONE', #8299, #35375, #24112 ) ;
#20972 = EDGE_CURVE ( 'NONE', #67683, #54091, #62236, .T. ) ;
#20973 = CARTESIAN_POINT ( 'NONE',  ( 0.000000000000000000, 87.30187232391182306, 0.000000000000000000 ) ) ;
#20974 = DIRECTION ( 'NONE',  ( -1.000000000000000000, 0.000000000000000000, 0.000000000000000000 ) ) ;
#20975 =( NAMED_UNIT ( * ) SI_UNIT ( $, .STERADIAN. ) SOLID_ANGLE_UNIT ( ) );
#20976 = DIRECTION ( 'NONE',  ( -1.000000000000000000, -2.255140518769849223E-17, 5.551115123125782702E-17 ) ) ;
#20977 = ADVANCED_FACE ( 'NONE', ( #26321 ), #31957, .T. ) ;
#20978 = CARTESIAN_POINT ( 'NONE',  ( -89.90707362346732623, -3.094860106599338412, 9.525000000013864820 ) ) ;
#20979 = LINE ( 'NONE', #19920, #9041 ) ;
#20980 = DIRECTION ( 'NONE',  ( -1.156482317317873451E-16, 1.000000000000000000, 0.000000000000000000 ) ) ;
#20981 = CARTESIAN_POINT ( 'NONE',  ( -4.716976649647098618, 139.1429263765338078, 6.492361379858953008 ) ) ;
#20982 = CARTESIAN_POINT ( 'NONE',  ( -78.44292637653380496, -1.166476076187852838E-15, -9.524999999999991473 ) ) ;
#20983 = EDGE_CURVE ( 'NONE', #59410, #41519, #61768, .T. ) ;
#20984 = LINE ( 'NONE', #16082, #38536 ) ;
#20985 = VERTEX_POINT ( 'NONE', #57307 ) ;
#20986 = CARTESIAN_POINT ( 'NONE',  ( 4.716976649647099507, 117.7570736234661553, -6.492361379858953008 ) ) ;
#20988 = EDGE_CURVE ( 'NONE', #65204, #29181, #2217, .T. ) ;
#20987 = CARTESIAN_POINT ( 'NONE',  ( 9.250000000000003553, 0.000000000000000000, 3.750000000000000000 ) ) ;
#20989 = CARTESIAN_POINT ( 'NONE',  ( 22.49408850561247775, 25.15120473151022296, -27.39855116598959128 ) ) ;
#20990 = DIRECTION ( 'NONE',  ( 0.000000000000000000, 0.000000000000000000, -1.000000000000000000 ) ) ;
#20991 = EDGE_LOOP ( 'NONE', ( #54591, #1771, #27409, #35582 ) ) ;
#20992 = ORIENTED_EDGE ( 'NONE', *, *, #18282, .F. ) ;
#20993 = COLOUR_RGB ( '', 0.09019608, 0.27058824, 0.51372549) ;
#20994 = CARTESIAN_POINT ( 'NONE',  ( 13.75000000000000533, 30.99999999999999289, -3.750000000000000000 ) ) ;
#20995 = CARTESIAN_POINT ( 'NONE',  ( 3.249999999999998668, 36.74999999999999289, -3.750000000000000000 ) ) ;
#20996 = FACE_BOUND ( 'NONE', #44565, .T. ) ;
#20997 = ORIENTED_EDGE ( 'NONE', *, *, #1281, .T. ) ;
#20998 = CARTESIAN_POINT ( 'NONE',  ( 8.102448949553183510, 119.1049999999999756, -5.886773742842746238 ) ) ;
#20999 = PRESENTATION_STYLE_ASSIGNMENT (( #69523 ) ) ;
#21000 = COLOUR_RGB ( '', 0.72549020, 0.75294118, 0.79215686) ;
#21001 = AXIS2_PLACEMENT_3D ( 'NONE', #49148, #17487, #23413 ) ;
#21002 = CARTESIAN_POINT ( 'NONE',  ( 17.75000000000000711, 30.74999999999999289, 3.750000000000000000 ) ) ;
#21003 = CARTESIAN_POINT ( 'NONE',  ( -105.5949999999999989, 2.607480562269073321, 8.024999999999991473 ) ) ;
#21004 = ORIENTED_EDGE ( 'NONE', *, *, #26606, .T. ) ;
#21005 = DIRECTION ( 'NONE',  ( 0.000000000000000000, 1.000000000000000000, 0.000000000000000000 ) ) ;
#21006 = DIRECTION ( 'NONE',  ( 0.000000000000000000, 1.000000000000000000, 0.000000000000000000 ) ) ;
#21007 =( NAMED_UNIT ( * ) PLANE_ANGLE_UNIT ( ) SI_UNIT ( $, .RADIAN. ) );
#21008 = EDGE_LOOP ( 'NONE', ( #15697, #64650 ) ) ;
#21009 = CARTESIAN_POINT ( 'NONE',  ( -7.632228543268607446, 153.5429263765338419, -2.479861379858953718 ) ) ;
#21010 =( BOUNDED_CURVE ( )  B_SPLINE_CURVE ( 2, ( #58844, #714, #12031, #54242, #43065, #6744, #5696, #48679, #11335, #59514, #65498 ),
 .UNSPECIFIED., .F., .F. ) 
 B_SPLINE_CURVE_WITH_KNOTS ( ( 3, 2, 2, 2, 2, 3 ),
 ( 0.6764705882352939348, 0.6823529411764703845, 0.6882352941176468342, 0.6941176470588232839, 0.6999999999999997335, 0.7058823529411762943 ),
 .UNSPECIFIED. ) 
 CURVE ( )  GEOMETRIC_REPRESENTATION_ITEM ( )  RATIONAL_B_SPLINE_CURVE ( ( 1.000000000000001776, 0.9510565162951516438, 1.000000000000000000, 0.9510565162951535312, 1.000000000000000000, 0.9510565162951535312, 1.000000000000000000, 0.9510565162951535312, 1.000000000000000000, 0.9510565162951554186, 0.9999999999999981126 ) ) 
 REPRESENTATION_ITEM ( '' )  );
#21011 = FILL_AREA_STYLE ('',( #9782 ) ) ;
#21012 = VECTOR ( 'NONE', #49653, 1000.000000000000000 ) ;
#21013 = CARTESIAN_POINT ( 'NONE',  ( -20.83091330386927353, 149.9514755777528023, -9.751095921151032186 ) ) ;
#21014 = CARTESIAN_POINT ( 'NONE',  ( 21.02379601146600763, 114.6388938931947763, -10.00000000000000000 ) ) ;
#21015 = ORIENTED_EDGE ( 'NONE', *, *, #6120, .F. ) ;
#21016 = CARTESIAN_POINT ( 'NONE',  ( 6.826472737025121695, 128.4929263765338021, -4.959722759717905660 ) ) ;
#21017 = DIRECTION ( 'NONE',  ( -1.000000000000000000, -0.000000000000000000, -0.000000000000000000 ) ) ;
#21018 = FILL_AREA_STYLE_COLOUR ( '', #11633 ) ;
#21019 = CARTESIAN_POINT ( 'NONE',  ( -60.00000000000000000, -2.024042244987997205E-14, 12.00000000000000000 ) ) ;
#21020 = FACE_OUTER_BOUND ( 'NONE', #48040, .T. ) ;
#21021 = LINE ( 'NONE', #53390, #21816 ) ;
#21022 = EDGE_CURVE ( 'NONE', #19333, #40281, #31452, .T. ) ;
#21023 = CARTESIAN_POINT ( 'NONE',  ( 6.826472737025119919, 115.8929263765338220, 4.959722759717908325 ) ) ;
#21024 = DIRECTION ( 'NONE',  ( -1.000000000000000000, 0.000000000000000000, 0.000000000000000000 ) ) ;
#21025 = ORIENTED_EDGE ( 'NONE', *, *, #23410, .F. ) ;
#21026 = ORIENTED_EDGE ( 'NONE', *, *, #8594, .F. ) ;
#21027 = CARTESIAN_POINT ( 'NONE',  ( -11.74999999999999645, -0.9999999999999995559, 19.00000000000000000 ) ) ;
#21028 = FACE_OUTER_BOUND ( 'NONE', #33152, .T. ) ;
#21029 = VERTEX_POINT ( 'NONE', #9832 ) ;
#21030 =( NAMED_UNIT ( * ) PLANE_ANGLE_UNIT ( ) SI_UNIT ( $, .RADIAN. ) );
#21031 = CARTESIAN_POINT ( 'NONE',  ( -166.7049999999999557, 2.607480562269073321, 8.024999999999991473 ) ) ;
#21032 = FILL_AREA_STYLE ('',( #47838 ) ) ;
#21033 = DIRECTION ( 'NONE',  ( 0.000000000000000000, 1.000000000000000000, 0.000000000000000000 ) ) ;
#21034 = CARTESIAN_POINT ( 'NONE',  ( -180.2949999999999591, -2.607480562269069768, 8.024999999999991473 ) ) ;
#21035 = CARTESIAN_POINT ( 'NONE',  ( -166.6449999999999818, 4.716976649647091513, -6.492361379858946790 ) ) ;
#21036 = ORIENTED_EDGE ( 'NONE', *, *, #51331, .T. ) ;
#21037 =( NAMED_UNIT ( * ) PLANE_ANGLE_UNIT ( ) SI_UNIT ( $, .RADIAN. ) );
#21038 = EDGE_CURVE ( 'NONE', #7265, #38885, #20723, .T. ) ;
#21039 = DIRECTION ( 'NONE',  ( -0.000000000000000000, -0.000000000000000000, -1.000000000000000000 ) ) ;
#21040 = DIRECTION ( 'NONE',  ( -1.000000000000000000, -1.073081856240828566E-16, 0.000000000000000000 ) ) ;
#21041 = ADVANCED_FACE ( 'NONE', ( #52742 ), #36237, .F. ) ;
#21042 = CARTESIAN_POINT ( 'NONE',  ( -80.30499999999999261, 8.437984349512085203, -1.550032578732815448E-15 ) ) ;
#21043 = LINE ( 'NONE', #11173, #19631 ) ;
#21044 = DIRECTION ( 'NONE',  ( 0.000000000000000000, 0.000000000000000000, -1.000000000000000000 ) ) ;
#21045 = CARTESIAN_POINT ( 'NONE',  ( -74.49999999999998579, 36.50926243676796190, -10.00000000000000000 ) ) ;
#21046 = AXIS2_PLACEMENT_3D ( 'NONE', #37867, #94, #59237 ) ;
#21047 = EDGE_CURVE ( 'NONE', #34213, #52924, #29186, .T. ) ;
#21048 = CARTESIAN_POINT ( 'NONE',  ( -80.84499999999998465, -7.632228543268599452, 2.479861379858951054 ) ) ;
#21049 = ADVANCED_FACE ( 'NONE', ( #15806 ), #56094, .T. ) ;
#21050 = CARTESIAN_POINT ( 'NONE',  ( -8.102448949553181734, 129.0049999999999670, -5.886773742842749790 ) ) ;
#21051 = VECTOR ( 'NONE', #7445, 1000.000000000000000 ) ;
#21052 = CARTESIAN_POINT ( 'NONE',  ( -15.98999599679679839, 146.4999999999999716, -7.500000000000000000 ) ) ;
#21053 = DIRECTION ( 'NONE',  ( 1.000000000000000000, 0.000000000000000000, 0.000000000000000000 ) ) ;
#21054 = LINE ( 'NONE', #59348, #16981 ) ;
#21055 = DIRECTION ( 'NONE',  ( 7.080503983578803083E-17, -1.000000000000000000, -0.000000000000000000 ) ) ;
#21056 = ORIENTED_EDGE ( 'NONE', *, *, #1051, .F. ) ;
#21057 = ADVANCED_FACE ( 'NONE', ( #1542 ), #17789, .F. ) ;
#21058 = SURFACE_STYLE_USAGE ( .BOTH. , #3442 ) ;
#21059 = STYLED_ITEM ( 'NONE', ( #12462 ), #67433 ) ;
#21060 = EDGE_CURVE ( 'NONE', #24259, #51230, #60665, .T. ) ;
#21061 = DIRECTION ( 'NONE',  ( -0.000000000000000000, -0.000000000000000000, -1.000000000000000000 ) ) ;
#21062 = SURFACE_STYLE_USAGE ( .BOTH. , #21757 ) ;
#21063 = CARTESIAN_POINT ( 'NONE',  ( -4.716976649647098618, 137.2570736234661695, 6.492361379858953008 ) ) ;
#21064 = ORIENTED_EDGE ( 'NONE', *, *, #10238, .F. ) ;
#21065 = ORIENTED_EDGE ( 'NONE', *, *, #1860, .F. ) ;
#21066 = CARTESIAN_POINT ( 'NONE',  ( 74.50000000000000000, 20.36037961002804053, -6.500000000000000000 ) ) ;
#21067 =( LENGTH_UNIT ( ) NAMED_UNIT ( * ) SI_UNIT ( .MILLI., .METRE. ) );
#21068 =( LENGTH_UNIT ( ) NAMED_UNIT ( * ) SI_UNIT ( .MILLI., .METRE. ) );
#21069 = DIRECTION ( 'NONE',  ( 0.000000000000000000, 0.000000000000000000, -1.000000000000000000 ) ) ;
#21070 = FACE_OUTER_BOUND ( 'NONE', #14588, .T. ) ;
#21071 = VERTEX_POINT ( 'NONE', #13176 ) ;
#21072 = CARTESIAN_POINT ( 'NONE',  ( -125.9049999999999869, 2.607480562269069324, -8.024999999999993250 ) ) ;
#21073 = ORIENTED_EDGE ( 'NONE', *, *, #20599, .F. ) ;
#21074 = LINE ( 'NONE', #241, #65687 ) ;
#21075 = FACE_OUTER_BOUND ( 'NONE', #916, .T. ) ;
#21076 = EDGE_LOOP ( 'NONE', ( #26789, #40669 ) ) ;
#21077 = DIRECTION ( 'NONE',  ( -0.000000000000000000, -1.000000000000000000, -0.000000000000000000 ) ) ;
#21078 = ORIENTED_EDGE ( 'NONE', *, *, #41194, .F. ) ;
#21079 = EDGE_CURVE ( 'NONE', #36379, #59308, #25838, .T. ) ;
#21080 = CARTESIAN_POINT ( 'NONE',  ( 34.99999999999992895, 112.9999999999999858, 9.500000000000000000 ) ) ;
#21081 = CARTESIAN_POINT ( 'NONE',  ( -8.102448949553181734, 152.4949999999999477, 5.886773742842747126 ) ) ;
#21082 = ORIENTED_EDGE ( 'NONE', *, *, #20586, .F. ) ;
#21083 = DIRECTION ( 'NONE',  ( -0.000000000000000000, 0.000000000000000000, -1.000000000000000000 ) ) ;
#21084 = CARTESIAN_POINT ( 'NONE',  ( 3.094860106618431583, 151.2049999999999841, 9.525000000000000355 ) ) ;
#21085 = CARTESIAN_POINT ( 'NONE',  ( 62.24999999999998579, 33.74999999999999289, 3.750000000000000000 ) ) ;
#21086 = VECTOR ( 'NONE', #8681, 1000.000000000000114 ) ;
#21087 = CARTESIAN_POINT ( 'NONE',  ( 5.885195493260862776, 2.499999999999998668, 3.806542393196804763 ) ) ;
#21088 = EDGE_LOOP ( 'NONE', ( #67722, #12931, #21491, #48543, #41082, #18704 ) ) ;
#21089 = CARTESIAN_POINT ( 'NONE',  ( -7.632228543268607446, 129.5429263765338135, -2.479861379858953718 ) ) ;
#21090 = DIRECTION ( 'NONE',  ( 1.000000000000000000, 0.000000000000000000, 0.000000000000000000 ) ) ;
#21091 = CIRCLE ( 'NONE', #16659, 0.2500000000000002220 ) ;
#21092 = STYLED_ITEM ( 'NONE', ( #50966 ), #65643 ) ;
#21093 =( NAMED_UNIT ( * ) PLANE_ANGLE_UNIT ( ) SI_UNIT ( $, .RADIAN. ) );
#21094 = FILL_AREA_STYLE ('',( #32675 ) ) ;
#21095 = VERTEX_POINT ( 'NONE', #28995 ) ;
#21096 = DIRECTION ( 'NONE',  ( 0.000000000000000000, 0.000000000000000000, -1.000000000000000000 ) ) ;
#21097 = ORIENTED_EDGE ( 'NONE', *, *, #53475, .T. ) ;
#21098 = CARTESIAN_POINT ( 'NONE',  ( -61.49292637653379501, -8.102448949553172852, 5.886773742842742685 ) ) ;
#21099 = CARTESIAN_POINT ( 'NONE',  ( 0.000000000000000000, 0.000000000000000000, 0.000000000000000000 ) ) ;
#21100 = DIRECTION ( 'NONE',  ( -0.000000000000000000, -0.000000000000000000, 1.000000000000000000 ) ) ;
#21101 = CIRCLE ( 'NONE', #35720, 9.999999999999998224 ) ;
#21102 = CARTESIAN_POINT ( 'NONE',  ( -144.9550000000000125, -7.632228543268599452, 2.479861379858951054 ) ) ;
#21103 = CARTESIAN_POINT ( 'NONE',  ( -6.667623377008405683, -2.231456886122025196, -6.451337545287480602 ) ) ;
#21104 = LINE ( 'NONE', #33054, #21652 ) ;
#21105 = SURFACE_SIDE_STYLE ('',( #4926 ) ) ;
#21106 = CARTESIAN_POINT ( 'NONE',  ( 0.000000000000000000, 0.000000000000000000, 52.50000000000000000 ) ) ;
#21107 = PRESENTATION_STYLE_ASSIGNMENT (( #37341 ) ) ;
#21108 = DIRECTION ( 'NONE',  ( 0.000000000000000000, 1.000000000000000000, -0.000000000000000000 ) ) ;
#21109 = VERTEX_POINT ( 'NONE', #44562 ) ;
#21110 = ORIENTED_EDGE ( 'NONE', *, *, #64809, .F. ) ;
#21111 = FACE_OUTER_BOUND ( 'NONE', #38322, .T. ) ;
#21112 = STYLED_ITEM ( 'NONE', ( #4370 ), #41361 ) ;
#21113 = DIRECTION ( 'NONE',  ( 0.000000000000000000, 0.000000000000000000, -1.000000000000000000 ) ) ;
#21114 = CARTESIAN_POINT ( 'NONE',  ( -68.30499999999997840, 8.437984349512085203, -1.550032578732815448E-15 ) ) ;
#21115 = ORIENTED_EDGE ( 'NONE', *, *, #55617, .T. ) ;
#21116 = FILL_AREA_STYLE ('',( #43333 ) ) ;
#21117 = CARTESIAN_POINT ( 'NONE',  ( -29.23998778563472811, -8.499999999999996447, 0.5867931367521921349 ) ) ;
#21118 = CARTESIAN_POINT ( 'NONE',  ( -1.000000000000028644, 0.000000000000000000, 0.000000000000000000 ) ) ;
#21119 = CARTESIAN_POINT ( 'NONE',  ( 11.00000000000001776, 26.00000000000000355, -27.50000000000000355 ) ) ;
#21120 = CARTESIAN_POINT ( 'NONE',  ( 57.74999999999999289, 28.24999999999998934, -3.750000000000000000 ) ) ;
#21121 = ORIENTED_EDGE ( 'NONE', *, *, #20920, .F. ) ;
#21122 = ADVANCED_FACE ( 'NONE', ( #27945 ), #23741, .F. ) ;
#21123 = CARTESIAN_POINT ( 'NONE',  ( -15.98999599679679839, 118.4999999999999716, 7.500000000000000000 ) ) ;
#21124 = CARTESIAN_POINT ( 'NONE',  ( 3.673940397442060361E-16, -2.500000000000000000, -3.000000000000000444 ) ) ;
#21125 = CARTESIAN_POINT ( 'NONE',  ( 69.74999999999998579, 36.75000000000000000, -3.000000000000000000 ) ) ;
#21126 = EDGE_CURVE ( 'NONE', #28845, #38442, #5548, .T. ) ;
#21127 = CARTESIAN_POINT ( 'NONE',  ( -119.2449999999999903, -4.716976649647093289, -6.492361379858945902 ) ) ;
#21128 = CARTESIAN_POINT ( 'NONE',  ( -5.598654528085808657, 152.6449999999999818, 7.705886871421373741 ) ) ;
#21129 = CARTESIAN_POINT ( 'NONE',  ( -90.44499999999997897, 0.000000000000000000, 8.024999999999991473 ) ) ;
#21130 = DIRECTION ( 'NONE',  ( -0.000000000000000000, 0.000000000000000000, -1.000000000000000000 ) ) ;
#21131 =( BOUNDED_SURFACE ( )  B_SPLINE_SURFACE ( 3, 2, ( 
 ( #31467, #16723, #52954 ),
 ( #69135, #20941, #23348 ),
 ( #55715, #44852, #50788 ),
 ( #66253, #61325, #2538 ),
 ( #13136, #50110, #59939 ),
 ( #18437, #39922, #66619 ),
 ( #12433, #45554, #12792 ),
 ( #60293, #24048, #22667 ),
 ( #60972, #56044, #18081 ),
 ( #2165, #28242, #1838 ),
 ( #39569, #34258, #17417 ),
 ( #49408, #34589, #23697 ),
 ( #17749, #7522, #7857 ),
 ( #44170, #50437, #33224 ),
 ( #6817, #29310, #45198 ),
 ( #28948, #66974, #38547 ),
 ( #11756, #49753, #54662 ),
 ( #6465, #27899, #38882 ) ),
 .UNSPECIFIED., .F., .F., .T. ) 
 B_SPLINE_SURFACE_WITH_KNOTS ( ( 4, 2, 2, 2, 2, 2, 2, 2, 4 ),
 ( 3, 3 ),
 ( 0.0008275086428995133761, 0.0009765612317269614347, 0.001125613820554409493, 0.001274666409381857660, 0.001423718998209305611, 0.001721824175864201728, 0.002019929353519097845, 0.002616139708828890513, 0.003212350064138682747 ),
 ( 0.000000000000000000, 1.000000000000000000 ),
 .UNSPECIFIED. ) 
 GEOMETRIC_REPRESENTATION_ITEM ( )  RATIONAL_B_SPLINE_SURFACE ( (
 ( 1.000000000000000000, 0.2907356542125049681, 1.000000000000000000),
 ( 1.000000000000000000, 0.2907339171233887520, 1.000000000000000000),
 ( 1.000000000000000000, 0.2933218126492017630, 1.000000000000000000),
 ( 1.000000000000000000, 0.3027174795993979872, 1.000000000000000000),
 ( 1.000000000000000000, 0.3096405143333775256, 1.000000000000000000),
 ( 1.000000000000000000, 0.3258903432231474162, 1.000000000000000000),
 ( 1.000000000000000000, 0.3352112554374609976, 1.000000000000000000),
 ( 1.000000000000000000, 0.3552330613601621945, 1.000000000000000000),
 ( 1.000000000000000000, 0.3657822831407469000, 1.000000000000000000),
 ( 1.000000000000000000, 0.3977110304216009973, 1.000000000000000000),
 ( 1.000000000000000000, 0.4197187326556824361, 1.000000000000000000),
 ( 1.000000000000000000, 0.4623670587024229506, 1.000000000000000000),
 ( 1.000000000000000000, 0.4829316641227751616, 1.000000000000000000),
 ( 1.000000000000000000, 0.5424860661042288923, 1.000000000000000000),
 ( 1.000000000000000000, 0.5795047887218846006, 1.000000000000000000),
 ( 1.000000000000000000, 0.6470713767466169664, 1.000000000000000000),
 ( 1.000000000000000000, 0.6780453138456912221, 1.000000000000000000),
 ( 1.000000000000000000, 0.7071067811865469066, 1.000000000000000000) ) ) 
 REPRESENTATION_ITEM ( '' )  SURFACE ( )  );
#21132 = CYLINDRICAL_SURFACE ( 'NONE', #60644, 0.5000000000000004441 ) ;
#21133 = ORIENTED_EDGE ( 'NONE', *, *, #48401, .T. ) ;
#21134 = CARTESIAN_POINT ( 'NONE',  ( -137.9929263765338305, 8.102448949553171076, -5.886773742842744461 ) ) ;
#21135 = DIRECTION ( 'NONE',  ( 0.000000000000000000, 0.000000000000000000, 1.000000000000000000 ) ) ;
#21136 = CARTESIAN_POINT ( 'NONE',  ( -146.5449999999999875, -7.632228543268600340, -2.479861379858950166 ) ) ;
#21137 = DIRECTION ( 'NONE',  ( -0.000000000000000000, -1.000000000000000000, -0.000000000000000000 ) ) ;
#21138 = EDGE_CURVE ( 'NONE', #51968, #5374, #12372, .T. ) ;
#21139 = CARTESIAN_POINT ( 'NONE',  ( 48.00000000000000000, 99.99999999999992895, 7.000000000000000000 ) ) ;
#21140 = CARTESIAN_POINT ( 'NONE',  ( 66.74999999999998579, 36.75000000000000000, -3.750000000000000000 ) ) ;
#21141 = VERTEX_POINT ( 'NONE', #56807 ) ;
#21142 = VECTOR ( 'NONE', #68748, 1000.000000000000000 ) ;
#21143 = ORIENTED_EDGE ( 'NONE', *, *, #29790, .F. ) ;
#21144 = LINE ( 'NONE', #52501, #26276 ) ;
#21145 = CARTESIAN_POINT ( 'NONE',  ( -143.6929263765337907, 10.01517768586948698, -1.839758294383808966E-15 ) ) ;
#21146 = CARTESIAN_POINT ( 'NONE',  ( -45.78727775085652496, 8.937790484662075485, 6.368793980437917668 ) ) ;
#21147 = LINE ( 'NONE', #69688, #33676 ) ;
#21148 =( GEOMETRIC_REPRESENTATION_CONTEXT ( 3 ) GLOBAL_UNCERTAINTY_ASSIGNED_CONTEXT ( ( #58601 ) ) GLOBAL_UNIT_ASSIGNED_CONTEXT ( ( #50971, #55185, #6645 ) ) REPRESENTATION_CONTEXT ( 'NONE', 'WORKASPACE' ) );
#21149 = CARTESIAN_POINT ( 'NONE',  ( -58.24585058642980329, -8.499999999999992895, 0.6021708693608249785 ) ) ;
#21150 = ORIENTED_EDGE ( 'NONE', *, *, #38950, .F. ) ;
#21151 = CARTESIAN_POINT ( 'NONE',  ( -149.3049999999999784, 8.437984349512086979, -1.550032578732815448E-15 ) ) ;
#21152 = EDGE_CURVE ( 'NONE', #37052, #35876, #33151, .T. ) ;
#21153 = EDGE_LOOP ( 'NONE', ( #60619, #4897, #842, #18678 ) ) ;
#21154 = FACE_OUTER_BOUND ( 'NONE', #68511, .T. ) ;
#21155 = VERTEX_POINT ( 'NONE', #62746 ) ;
#21156 = DIRECTION ( 'NONE',  ( 0.000000000000000000, 0.000000000000000000, -1.000000000000000000 ) ) ;
#21157 = EDGE_CURVE ( 'NONE', #55864, #52256, #45599, .T. ) ;
#21158 = CARTESIAN_POINT ( 'NONE',  ( -3.094860106618432471, 118.5949999999999847, -9.525000000000000355 ) ) ;
#21159 = DIRECTION ( 'NONE',  ( -0.000000000000000000, -0.000000000000000000, -1.000000000000000000 ) ) ;
#21160 = ORIENTED_EDGE ( 'NONE', *, *, #21157, .F. ) ;
#21161 = SURFACE_SIDE_STYLE ('',( #41988 ) ) ;
#21162 = CARTESIAN_POINT ( 'NONE',  ( -3.094860106618432471, 125.7049999999999841, -9.525000000000000355 ) ) ;
#21163 = CARTESIAN_POINT ( 'NONE',  ( -68.60499999999997556, 6.826472737025113702, -4.959722759717902107 ) ) ;
#21164 = CIRCLE ( 'NONE', #16733, 0.2500000000000002220 ) ;
#21165 = CARTESIAN_POINT ( 'NONE',  ( -117.7449999999999903, 4.716976649647094177, 6.492361379858945902 ) ) ;
#21166 = CARTESIAN_POINT ( 'NONE',  ( -41.01803665359474138, 107.7206116573237722, -3.151333386623310862 ) ) ;
#21167 = ORIENTED_EDGE ( 'NONE', *, *, #18449, .T. ) ;
#21168 = CARTESIAN_POINT ( 'NONE',  ( -9.058813317711338797, 144.4550000000000125, 2.943386871421373563 ) ) ;
#21169 = CARTESIAN_POINT ( 'NONE',  ( -183.0000000000000284, -1.154738647139537111, 9.454745033939424559 ) ) ;
#21170 = CIRCLE ( 'NONE', #39183, 9.000000000000000000 ) ;
#21171 = LINE ( 'NONE', #57789, #51909 ) ;
#21172 = CARTESIAN_POINT ( 'NONE',  ( -35.00000000000003553, 10.49999999999998224, -3.500000000000000000 ) ) ;
#21173 = EDGE_LOOP ( 'NONE', ( #54125, #3947, #55431 ) ) ;
#21174 = DIRECTION ( 'NONE',  ( -1.000000000000000000, 0.000000000000000000, 0.000000000000000000 ) ) ;
#21175 = SURFACE_STYLE_USAGE ( .BOTH. , #64452 ) ;
#21176 = CARTESIAN_POINT ( 'NONE',  ( -178.1049999999999329, -6.826472737025115478, 4.959722759717900331 ) ) ;
#21177 = VERTEX_POINT ( 'NONE', #41342 ) ;
#21178 = DIRECTION ( 'NONE',  ( 0.000000000000000000, 1.000000000000000000, 0.000000000000000000 ) ) ;
#21179 = CARTESIAN_POINT ( 'NONE',  ( -45.00000000000000000, 0.000000000000000000, 9.525000000000000355 ) ) ;
#21180 = FACE_OUTER_BOUND ( 'NONE', #5416, .T. ) ;
#21181 = VERTEX_POINT ( 'NONE', #57855 ) ;
#21182 = VECTOR ( 'NONE', #60654, 1000.000000000000000 ) ;
#21183 = CIRCLE ( 'NONE', #30153, 5.000000000000000000 ) ;
#21184 = DIRECTION ( 'NONE',  ( -1.000000000000000000, 0.000000000000000000, 0.000000000000000000 ) ) ;
#21185 = CARTESIAN_POINT ( 'NONE',  ( -90.35499999999998977, -4.716976649647093289, -6.492361379858945902 ) ) ;
#21186 = ORIENTED_EDGE ( 'NONE', *, *, #51951, .T. ) ;
#21187 = CARTESIAN_POINT ( 'NONE',  ( 179.4098300562505415, 5.000000000000010658, 0.000000000000000000 ) ) ;
#21188 = ADVANCED_FACE ( 'NONE', ( #68394 ), #25470, .T. ) ;
#21189 = AXIS2_PLACEMENT_3D ( 'NONE', #2184, #7877, #28262 ) ;
#21190 = CARTESIAN_POINT ( 'NONE',  ( -128.0070736234661979, -8.102448949553172852, -5.886773742842741797 ) ) ;
#21191 = FACE_OUTER_BOUND ( 'NONE', #25312, .T. ) ;
#21192 = CARTESIAN_POINT ( 'NONE',  ( -70.25707362346616947, 5.598654528085800663, -7.705886871421367523 ) ) ;
#21193 = VERTEX_POINT ( 'NONE', #40289 ) ;
#21194 = DIRECTION ( 'NONE',  ( -0.000000000000000000, -1.000000000000000000, -0.000000000000000000 ) ) ;
#21195 =( NAMED_UNIT ( * ) SI_UNIT ( $, .STERADIAN. ) SOLID_ANGLE_UNIT ( ) );
#21196 = COLOUR_RGB ( '', 0.09019608, 0.27058824, 0.51372549) ;
#21198 = SURFACE_SIDE_STYLE ('',( #15285 ) ) ;
#21197 = FACE_OUTER_BOUND ( 'NONE', #30847, .T. ) ;
#21199 = CARTESIAN_POINT ( 'NONE',  ( -114.8049999999999926, -8.437984349512085203, 5.166775262442717831E-16 ) ) ;
#21200 = EDGE_CURVE ( 'NONE', #54121, #30484, #64106, .T. ) ;
#21201 = CARTESIAN_POINT ( 'NONE',  ( -5.598654528085808657, 122.6449999999999960, 7.705886871421373741 ) ) ;
#21202 = CARTESIAN_POINT ( 'NONE',  ( -116.5450000000000017, -7.632228543268600340, -2.479861379858950166 ) ) ;
#21203 = EDGE_CURVE ( 'NONE', #30380, #39136, #15831, .T. ) ;
#21205 = DIRECTION ( 'NONE',  ( 1.000000000000000000, 0.000000000000000000, -1.300977106640434891E-16 ) ) ;
#21204 = CARTESIAN_POINT ( 'NONE',  ( -118.4929263765338021, -8.102448949553174629, 5.886773742842742685 ) ) ;
#21206 = ADVANCED_FACE ( 'NONE', ( #61696 ), #52583, .F. ) ;
#21207 = EDGE_LOOP ( 'NONE', ( #9713, #8389, #14864, #24559 ) ) ;
#21208 = VECTOR ( 'NONE', #48859, 1000.000000000000000 ) ;
#21209 = CARTESIAN_POINT ( 'NONE',  ( -159.1429263765338078, 5.598654528085800663, -7.705886871421367523 ) ) ;
#21210 = CARTESIAN_POINT ( 'NONE',  ( -183.1450000000000102, -4.716976649647092401, 6.492361379858946790 ) ) ;
#21211 = PRESENTATION_LAYER_ASSIGNMENT (  '', '', ( #12207 ) ) ;
#21212 = ADVANCED_FACE ( 'NONE', ( #14237 ), #7914, .F. ) ;
#21213 =( NAMED_UNIT ( * ) SI_UNIT ( $, .STERADIAN. ) SOLID_ANGLE_UNIT ( ) );
#21214 = CIRCLE ( 'NONE', #41440, 0.2500000000000002220 ) ;
#21215 = AXIS2_PLACEMENT_3D ( 'NONE', #41522, #62935, #42936 ) ;
#21216 = CARTESIAN_POINT ( 'NONE',  ( -20.44241585271047867, 115.3856657692246444, -10.00000000000000000 ) ) ;
#21217 = CARTESIAN_POINT ( 'NONE',  ( 33.00000000000002132, 13.00000000000000178, 79.00402776293826435 ) ) ;
#21218 = ORIENTED_EDGE ( 'NONE', *, *, #17548, .T. ) ;
#21219 = CARTESIAN_POINT ( 'NONE',  ( -80.84292637653379643, 9.058813317711329915, -2.943386871421373119 ) ) ;
#21220 = CARTESIAN_POINT ( 'NONE',  ( 54.99999999999999289, 2.409368300552961372E-15, -11.50000000000001066 ) ) ;
#21221 = CARTESIAN_POINT ( 'NONE',  ( 0.000000000000000000, 139.0570736234661808, -8.025000000000000355 ) ) ;
#21222 = DIRECTION ( 'NONE',  ( -0.000000000000000000, -1.000000000000000000, 0.000000000000000000 ) ) ;
#21223 = CIRCLE ( 'NONE', #35859, 2.500000000000000000 ) ;
#21224 = VECTOR ( 'NONE', #2103, 1000.000000000000000 ) ;
#21225 = CARTESIAN_POINT ( 'NONE',  ( -178.2549999999999955, -4.716976649647092401, 6.492361379858946790 ) ) ;
#21226 = ORIENTED_EDGE ( 'NONE', *, *, #14084, .T. ) ;
#21227 = DIRECTION ( 'NONE',  ( -0.000000000000000000, -0.000000000000000000, -1.000000000000000000 ) ) ;
#21228 = SURFACE_STYLE_USAGE ( .BOTH. , #37829 ) ;
#21229 = DIRECTION ( 'NONE',  ( 1.084202172485504434E-16, 1.000000000000000000, 0.000000000000000000 ) ) ;
#21230 =( GEOMETRIC_REPRESENTATION_CONTEXT ( 3 ) GLOBAL_UNCERTAINTY_ASSIGNED_CONTEXT ( ( #42602 ) ) GLOBAL_UNIT_ASSIGNED_CONTEXT ( ( #5705, #11342, #47668 ) ) REPRESENTATION_CONTEXT ( 'NONE', 'WORKASPACE' ) );
#21231 = CARTESIAN_POINT ( 'NONE',  ( 4.716976649647099507, 141.7570736234661410, -6.492361379858953008 ) ) ;
#21232 = STYLED_ITEM ( 'NONE', ( #12108 ), #19668 ) ;
#21233 = ORIENTED_EDGE ( 'NONE', *, *, #11517, .T. ) ;
#21234 = PLANE ( 'NONE',  #17040 ) ;
#21235 = CARTESIAN_POINT ( 'NONE',  ( -93.05499999999997840, -9.827790563157499189E-16, -8.024999999999991473 ) ) ;
#21236 = MECHANICAL_DESIGN_GEOMETRIC_PRESENTATION_REPRESENTATION (  '', ( #20137 ), #69552 ) ;
#21237 = ORIENTED_EDGE ( 'NONE', *, *, #55188, .F. ) ;
#21238 = CARTESIAN_POINT ( 'NONE',  ( -71.74137931034481142, 36.89918356738973415, -9.500000000000000000 ) ) ;
#21239 = DIRECTION ( 'NONE',  ( 0.7833176619561811327, -0.6216216216216277068, -4.313366480807242114E-15 ) ) ;
#21240 = FILL_AREA_STYLE_COLOUR ( '', #60074 ) ;
#21241 = CARTESIAN_POINT ( 'NONE',  ( -75.75000000000000000, -0.9999999999999995559, 19.00000000000000000 ) ) ;
#21242 = CARTESIAN_POINT ( 'NONE',  ( 0.000000000000000000, -2.500000000000000000, 9.000000000000000000 ) ) ;
#21243 = VERTEX_POINT ( 'NONE', #51879 ) ;
#21244 = FACE_OUTER_BOUND ( 'NONE', #42672, .T. ) ;
#21245 = CARTESIAN_POINT ( 'NONE',  ( -69.59499999999999886, 2.607480562269073321, 8.024999999999991473 ) ) ;
#21246 = VERTEX_POINT ( 'NONE', #21221 ) ;
#21247 = FILL_AREA_STYLE ('',( #49396 ) ) ;
#21248 = CARTESIAN_POINT ( 'NONE',  ( -125.6070736234661780, -8.102448949553174629, 5.886773742842742685 ) ) ;
#21249 = VECTOR ( 'NONE', #4310, 1000.000000000000000 ) ;
#21250 = EDGE_LOOP ( 'NONE', ( #15499, #57146, #59399, #63516 ) ) ;
#21251 = DIRECTION ( 'NONE',  ( 0.000000000000000000, -0.000000000000000000, 1.000000000000000000 ) ) ;
#21252 = FILL_AREA_STYLE ('',( #16034 ) ) ;
#21253 = VERTEX_POINT ( 'NONE', #4710 ) ;
#21254 = CARTESIAN_POINT ( 'NONE',  ( -7.794228634059947147, 2.500000000000000000, -4.500000000000000000 ) ) ;
#21256 = ORIENTED_EDGE ( 'NONE', *, *, #21828, .F. ) ;
#21255 = EDGE_CURVE ( 'NONE', #64131, #65411, #50654, .T. ) ;
#21257 = AXIS2_PLACEMENT_3D ( 'NONE', #68125, #30443, #51943 ) ;
#21258 = CARTESIAN_POINT ( 'NONE',  ( -159.5929263765341659, -3.094860106623775753, -9.524999999996111910 ) ) ;
#21259 = LINE ( 'NONE', #30784, #7487 ) ;
#21260 =( GEOMETRIC_REPRESENTATION_CONTEXT ( 3 ) GLOBAL_UNCERTAINTY_ASSIGNED_CONTEXT ( ( #4567 ) ) GLOBAL_UNIT_ASSIGNED_CONTEXT ( ( #18889, #61125, #19601 ) ) REPRESENTATION_CONTEXT ( 'NONE', 'WORKASPACE' ) );
#21261 = CARTESIAN_POINT ( 'NONE',  ( -155.7570736234661979, -5.598654528085801552, 7.705886871421367523 ) ) ;
#21262 = TOROIDAL_SURFACE ( 'NONE', #61720, 2.000000000000000000, 1.000000000000000000 ) ;
#21263 = CARTESIAN_POINT ( 'NONE',  ( -9.058813317711337021, 125.0449999999999875, -2.943386871421374895 ) ) ;
#21264 = EDGE_CURVE ( 'NONE', #39120, #33963, #41697, .T. ) ;
#21265 = CARTESIAN_POINT ( 'NONE',  ( -89.90707362346616094, -3.094860106618429807, 9.524999999999991473 ) ) ;
#21266 = AXIS2_PLACEMENT_3D ( 'NONE', #11378, #64147, #31431 ) ;
#21267 = EDGE_CURVE ( 'NONE', #19236, #25473, #10189, .T. ) ;
#21268 = CIRCLE ( 'NONE', #22441, 5.499999999999984901 ) ;
#21269 = CARTESIAN_POINT ( 'NONE',  ( -0.7418830492402813670, 154.4749711138048838, -9.478234102103829883 ) ) ;
#21270 = VERTEX_POINT ( 'NONE', #42748 ) ;
#21271 =( GEOMETRIC_REPRESENTATION_CONTEXT ( 3 ) GLOBAL_UNCERTAINTY_ASSIGNED_CONTEXT ( ( #53828 ) ) GLOBAL_UNIT_ASSIGNED_CONTEXT ( ( #15468, #69590, #54095 ) ) REPRESENTATION_CONTEXT ( 'NONE', 'WORKASPACE' ) );
#21272 = DIRECTION ( 'NONE',  ( -1.000000000000000000, 0.000000000000000000, 0.000000000000000000 ) ) ;
#21273 = EDGE_CURVE ( 'NONE', #13443, #31383, #20311, .T. ) ;
#21275 = DIRECTION ( 'NONE',  ( 0.000000000000000000, -1.000000000000000000, 0.000000000000000000 ) ) ;
#21274 = CARTESIAN_POINT ( 'NONE',  ( 0.000000000000000000, 148.0570736234661524, -8.025000000000000355 ) ) ;
#21276 = CARTESIAN_POINT ( 'NONE',  ( 12.25000000000000355, 30.74999999999998579, 3.750000000000000000 ) ) ;
#21277 = CARTESIAN_POINT ( 'NONE',  ( -136.8550000000000182, 4.716976649647094177, 6.492361379858945902 ) ) ;
#21278 = ADVANCED_FACE ( 'NONE', ( #10692 ), #21947, .F. ) ;
#21279 = CARTESIAN_POINT ( 'NONE',  ( -86.00707362346616947, -8.102448949553174629, -5.886773742842741797 ) ) ;
#21280 = CARTESIAN_POINT ( 'NONE',  ( 75.00000000000000000, 20.36037961002804408, 6.585786437626904188 ) ) ;
#21281 = CARTESIAN_POINT ( 'NONE',  ( -147.5949999999999704, 2.607480562269073321, 8.024999999999991473 ) ) ;
#21282 = EDGE_CURVE ( 'NONE', #21325, #47241, #45070, .T. ) ;
#21283 = CARTESIAN_POINT ( 'NONE',  ( -138.8949999999999250, 6.826472737025115478, 4.959722759717899443 ) ) ;
#21284 = EDGE_CURVE ( 'NONE', #41256, #66255, #26334, .T. ) ;
#21285 = ORIENTED_EDGE ( 'NONE', *, *, #4425, .F. ) ;
#21286 = AXIS2_PLACEMENT_3D ( 'NONE', #45141, #55657, #61273 ) ;
#21287 = DIRECTION ( 'NONE',  ( 0.000000000000000000, 0.000000000000000000, 1.000000000000000000 ) ) ;
#21288 = APPLICATION_CONTEXT ( 'automotive_design' ) ;
#21289 = FILL_AREA_STYLE_COLOUR ( '', #69379 ) ;
#21290 = EDGE_CURVE ( 'NONE', #7249, #37399, #47288, .T. ) ;
#21291 = SURFACE_STYLE_USAGE ( .BOTH. , #69493 ) ;
#21292 = UNCERTAINTY_MEASURE_WITH_UNIT (LENGTH_MEASURE( 1.000000000000000082E-05 ), #67821, 'distance_accuracy_value', 'NONE');
#21293 = CARTESIAN_POINT ( 'NONE',  ( -58.40499999999997982, -2.607480562269069768, 8.024999999999991473 ) ) ;
#21294 = SURFACE_STYLE_USAGE ( .BOTH. , #54349 ) ;
#21295 = PRESENTATION_LAYER_ASSIGNMENT (  '', '', ( #20137 ) ) ;
#21296 = DIRECTION ( 'NONE',  ( 0.000000000000000000, 0.000000000000000000, -1.000000000000000000 ) ) ;
#21297 = SURFACE_SIDE_STYLE ('',( #15030 ) ) ;
#21298 = FILL_AREA_STYLE ('',( #26571 ) ) ;
#21299 = CARTESIAN_POINT ( 'NONE',  ( -7.794228634059948035, -2.500000000000000000, 4.499999999999999112 ) ) ;
#21300 = AXIS2_PLACEMENT_3D ( 'NONE', #25849, #15348, #47734 ) ;
#21301 = VECTOR ( 'NONE', #45473, 1000.000000000000000 ) ;
#21302 = UNCERTAINTY_MEASURE_WITH_UNIT (LENGTH_MEASURE( 1.000000000000000082E-05 ), #23714, 'distance_accuracy_value', 'NONE');
#21303 = CARTESIAN_POINT ( 'NONE',  ( -4.299999999999981171, 26.00000000000000000, -24.00000000000001066 ) ) ;
#21304 = CARTESIAN_POINT ( 'NONE',  ( -2.081668171172168513E-14, 43.00000000000000000, -28.00000000000000000 ) ) ;
#21305 = DIRECTION ( 'NONE',  ( -0.3420201433256663814, 0.9396926207859092051, -0.000000000000000000 ) ) ;
#21306 = FACE_OUTER_BOUND ( 'NONE', #12161, .T. ) ;
#21307 = CIRCLE ( 'NONE', #846, 1.000000000000000888 ) ;
#21308 = FACE_OUTER_BOUND ( 'NONE', #33226, .T. ) ;
#21309 = VECTOR ( 'NONE', #51384, 1000.000000000000000 ) ;
#21310 = CARTESIAN_POINT ( 'NONE',  ( 26.00000000000001776, -3.148064030671221758, 29.68999999999999417 ) ) ;
#21311 = ORIENTED_EDGE ( 'NONE', *, *, #24463, .F. ) ;
#21312 = CARTESIAN_POINT ( 'NONE',  ( 16.00000000000001776, -3.148064030671221758, 29.68999999999999417 ) ) ;
#21313 = AXIS2_PLACEMENT_3D ( 'NONE', #1726, #11980, #33439 ) ;
#21314 = CARTESIAN_POINT ( 'NONE',  ( -7.632228543268607446, 118.6570736234661609, -2.479861379858953718 ) ) ;
#21315 = SHAPE_REPRESENTATION ( '6. Lower Jaw', ( #42840 ), #7944 ) ;
#21316 = ADVANCED_FACE ( 'NONE', ( #49368 ), #66357, .T. ) ;
#21318 = AXIS2_PLACEMENT_3D ( 'NONE', #5901, #22796, #576 ) ;
#21317 = CARTESIAN_POINT ( 'NONE',  ( -19.98431065987488608, 114.9999999999999574, 10.47133983857574613 ) ) ;
#21319 = SURFACE_STYLE_USAGE ( .BOTH. , #15398 ) ;
#21320 = COLOUR_RGB ( '', 0.31764706, 0.68627451, 0.89019608) ;
#21321 = CARTESIAN_POINT ( 'NONE',  ( 27.99999999999999645, 0.000000000000000000, -24.00402776293821816 ) ) ;
#21322 = VERTEX_POINT ( 'NONE', #27861 ) ;
#21323 = VERTEX_POINT ( 'NONE', #39180 ) ;
#21324 = CARTESIAN_POINT ( 'NONE',  ( -46.25707362346617657, 5.598654528085800663, -7.705886871421367523 ) ) ;
#21325 = VERTEX_POINT ( 'NONE', #7139 ) ;
#21326 = CARTESIAN_POINT ( 'NONE',  ( -9.058813317711337021, 123.1549999999999869, -2.943386871421374895 ) ) ;
#21327 =( LENGTH_UNIT ( ) NAMED_UNIT ( * ) SI_UNIT ( .MILLI., .METRE. ) );
#21328 = FILL_AREA_STYLE ('',( #69524 ) ) ;
#21329 = VECTOR ( 'NONE', #56242, 1000.000000000000000 ) ;
#21330 = DIRECTION ( 'NONE',  ( -0.000000000000000000, 0.000000000000000000, -1.000000000000000000 ) ) ;
#21331 = CARTESIAN_POINT ( 'NONE',  ( -97.79500000000000171, 2.607480562269068880, -8.024999999999993250 ) ) ;
#21332 = ORIENTED_EDGE ( 'NONE', *, *, #10702, .F. ) ;
#21333 = COLOUR_RGB ( '', 0.08235294, 0.09019608, 0.10196078) ;
#21334 = DIRECTION ( 'NONE',  ( -0.000000000000000000, -0.000000000000000000, -1.000000000000000000 ) ) ;
#21335 = DIRECTION ( 'NONE',  ( -0.000000000000000000, -0.000000000000000000, -1.000000000000000000 ) ) ;
#21336 = SURFACE_SIDE_STYLE ('',( #64939 ) ) ;
#21337 = ORIENTED_EDGE ( 'NONE', *, *, #44771, .F. ) ;
#21338 = CARTESIAN_POINT ( 'NONE',  ( -4.716976649647097730, 150.2429263765338021, -6.492361379858953896 ) ) ;
#21339 = PRESENTATION_LAYER_ASSIGNMENT (  '', '', ( #7839 ) ) ;
#21340 = SURFACE_SIDE_STYLE ('',( #45191 ) ) ;
#21341 = CARTESIAN_POINT ( 'NONE',  ( 12.25000000000000355, 30.74999999999998579, -3.750000000000000000 ) ) ;
#21342 = EDGE_CURVE ( 'NONE', #48229, #6919, #56204, .T. ) ;
#21343 = CARTESIAN_POINT ( 'NONE',  ( 20.17763807713225432, 115.4773716707933460, -10.00000000000000000 ) ) ;
#21344 = ORIENTED_EDGE ( 'NONE', *, *, #44127, .T. ) ;
#21345 = DIRECTION ( 'NONE',  ( 0.000000000000000000, 0.000000000000000000, -1.000000000000000000 ) ) ;
#21346 = CARTESIAN_POINT ( 'NONE',  ( 2.999999999999998668, 0.000000000000000000, -37.00402776293829277 ) ) ;
#21347 = CARTESIAN_POINT ( 'NONE',  ( 17.75000000000000711, 30.74999999999999289, -4.000000000000000000 ) ) ;
#21348 = CARTESIAN_POINT ( 'NONE',  ( -31.03083116351206527, -8.500000000000001776, 7.024140319044499314 ) ) ;
#21349 = FACE_OUTER_BOUND ( 'NONE', #21843, .T. ) ;
#21350 =( GEOMETRIC_REPRESENTATION_CONTEXT ( 3 ) GLOBAL_UNCERTAINTY_ASSIGNED_CONTEXT ( ( #19308 ) ) GLOBAL_UNIT_ASSIGNED_CONTEXT ( ( #44689, #17910, #41464 ) ) REPRESENTATION_CONTEXT ( 'NONE', 'WORKASPACE' ) );
#21351 = DIRECTION ( 'NONE',  ( -1.000000000000000000, -7.709882115452468306E-16, 0.000000000000000000 ) ) ;
#21352 = EDGE_CURVE ( 'NONE', #25927, #6724, #25884, .T. ) ;
#21353 = CARTESIAN_POINT ( 'NONE',  ( 0.000000000000000000, 0.000000000000000000, 0.000000000000000000 ) ) ;
#21354 = CARTESIAN_POINT ( 'NONE',  ( -6.766228288048926842, 153.8165025765505334, 5.697616492254880427 ) ) ;
#21355 = VERTEX_POINT ( 'NONE', #1799 ) ;
#21356 = ORIENTED_EDGE ( 'NONE', *, *, #53552, .F. ) ;
#21357 = FACE_OUTER_BOUND ( 'NONE', #57804, .T. ) ;
#21358 = DIRECTION ( 'NONE',  ( 1.000000000000000000, 7.709882115452468306E-16, 0.000000000000000000 ) ) ;
#21359 = CARTESIAN_POINT ( 'NONE',  ( -3.000000000000000444, 0.000000000000000000, 32.50000000000000000 ) ) ;
#21360 = DIRECTION ( 'NONE',  ( 1.000000000000000000, 0.000000000000000000, 0.000000000000000000 ) ) ;
#21361 = ORIENTED_EDGE ( 'NONE', *, *, #67206, .T. ) ;
#21362 = DIRECTION ( 'NONE',  ( -0.000000000000000000, -0.000000000000000000, 1.000000000000000000 ) ) ;
#21363 = CARTESIAN_POINT ( 'NONE',  ( -169.8550000000000182, 4.716976649647094177, 6.492361379858945902 ) ) ;
#21364 = CARTESIAN_POINT ( 'NONE',  ( 0.000000000000000000, 0.000000000000000000, 32.50000000000000000 ) ) ;
#21365 = DIRECTION ( 'NONE',  ( 0.000000000000000000, 0.000000000000000000, -1.000000000000000000 ) ) ;
#21366 = MECHANICAL_DESIGN_GEOMETRIC_PRESENTATION_REPRESENTATION (  '', ( #53905 ), #52835 ) ;
#21367 = CARTESIAN_POINT ( 'NONE',  ( -50.90707362346616094, -3.094860106618429807, 9.524999999999991473 ) ) ;
#21368 = EDGE_CURVE ( 'NONE', #56593, #39359, #7344, .T. ) ;
#21369 = CARTESIAN_POINT ( 'NONE',  ( -168.7450000000000045, 4.716976649647094177, 6.492361379858945902 ) ) ;
#21370 = MECHANICAL_DESIGN_GEOMETRIC_PRESENTATION_REPRESENTATION (  '', ( #47290 ), #58439 ) ;
#21371 = ORIENTED_EDGE ( 'NONE', *, *, #65130, .F. ) ;
#21372 = CARTESIAN_POINT ( 'NONE',  ( -37.16661851630311730, -10.79484869592797658, 3.787717863381548256 ) ) ;
#21374 = EDGE_CURVE ( 'NONE', #59919, #58485, #34217, .T. ) ;
#21373 = AXIS2_PLACEMENT_3D ( 'NONE', #41777, #41421, #19584 ) ;
#21375 = CARTESIAN_POINT ( 'NONE',  ( -11.69477403538655480, 11.39635258918007210, 3.765737026947071353 ) ) ;
#21376 = CARTESIAN_POINT ( 'NONE',  ( -85.25499999999998124, -4.716976649647092401, 6.492361379858946790 ) ) ;
#21377 = DIRECTION ( 'NONE',  ( 0.000000000000000000, 0.000000000000000000, 1.000000000000000000 ) ) ;
#21378 = CARTESIAN_POINT ( 'NONE',  ( 65.00000000000000000, 1.797044900979284448E-15, 11.50000000000003730 ) ) ;
#21379 = AXIS2_PLACEMENT_3D ( 'NONE', #33943, #50154, #7229 ) ;
#21380 = CARTESIAN_POINT ( 'NONE',  ( -74.99999999999998579, 35.99166914535020823, -9.500000000000000000 ) ) ;
#21381 = CARTESIAN_POINT ( 'NONE',  ( -77.24499999999997613, -4.716976649647093289, -6.492361379858945902 ) ) ;
#21382 = CARTESIAN_POINT ( 'NONE',  ( 9.058813317711338797, 136.9549999999999841, -2.943386871421372675 ) ) ;
#21383 =( GEOMETRIC_REPRESENTATION_CONTEXT ( 3 ) GLOBAL_UNCERTAINTY_ASSIGNED_CONTEXT ( ( #4524 ) ) GLOBAL_UNIT_ASSIGNED_CONTEXT ( ( #59042, #5213, #16514 ) ) REPRESENTATION_CONTEXT ( 'NONE', 'WORKASPACE' ) );
#21384 = MECHANICAL_DESIGN_GEOMETRIC_PRESENTATION_REPRESENTATION (  '', ( #30356 ), #66324 ) ;
#21385 = DIRECTION ( 'NONE',  ( -1.000000000000000000, 0.000000000000000000, 0.000000000000000000 ) ) ;
#21386 =( NAMED_UNIT ( * ) SI_UNIT ( $, .STERADIAN. ) SOLID_ANGLE_UNIT ( ) );
#21387 = UNCERTAINTY_MEASURE_WITH_UNIT (LENGTH_MEASURE( 1.000000000000000082E-05 ), #45938, 'distance_accuracy_value', 'NONE');
#21388 = B_SPLINE_CURVE_WITH_KNOTS ( 'NONE', 3,
 ( #15859, #41921, #41553, #9882, #32006, #20778, #36984, #58394 ),
 .UNSPECIFIED., .F., .F.,
 ( 4, 2, 2, 4 ),
 ( 2.544316211732959925E-07, 0.002094919859796807744, 0.003142252573884623743, 0.004189585287972440175 ),
 .UNSPECIFIED. ) ;
#21389 = CIRCLE ( 'NONE', #56234, 5.000000000000000000 ) ;
#21391 = SURFACE_STYLE_FILL_AREA ( #37282 ) ;
#21390 = AXIS2_PLACEMENT_3D ( 'NONE', #36842, #3715, #25206 ) ;
#21392 = VERTEX_POINT ( 'NONE', #743 ) ;
#21393 = CARTESIAN_POINT ( 'NONE',  ( -66.49999999999998579, 50.00000000000000000, 12.00000000000000000 ) ) ;
#21394 = CIRCLE ( 'NONE', #30364, 1.000000000000000888 ) ;
#21395 = SURFACE_STYLE_FILL_AREA ( #47147 ) ;
#21397 =( LENGTH_UNIT ( ) NAMED_UNIT ( * ) SI_UNIT ( .MILLI., .METRE. ) );
#21396 = FILL_AREA_STYLE_COLOUR ( '', #15042 ) ;
#21398 = FACE_OUTER_BOUND ( 'NONE', #16973, .T. ) ;
#21399 = ORIENTED_EDGE ( 'NONE', *, *, #56296, .T. ) ;
#21400 = ORIENTED_EDGE ( 'NONE', *, *, #33524, .F. ) ;
#21401 = CARTESIAN_POINT ( 'NONE',  ( -45.50000000000000000, 7.768687147774684831, -6.500000000000000000 ) ) ;
#21402 = AXIS2_PLACEMENT_3D ( 'NONE', #31208, #57265, #40421 ) ;
#21403 = EDGE_CURVE ( 'NONE', #48545, #45861, #16523, .T. ) ;
#21404 = PRESENTATION_LAYER_ASSIGNMENT (  '', '', ( #37346 ) ) ;
#21405 = DIRECTION ( 'NONE',  ( 0.000000000000000000, 0.000000000000000000, -1.000000000000000000 ) ) ;
#21406 =( BOUNDED_CURVE ( )  B_SPLINE_CURVE ( 2, ( #62576, #3447, #67883, #14062, #41867, #35525, #62917, #14763, #30915, #52414, #4158 ),
 .UNSPECIFIED., .F., .F. ) 
 B_SPLINE_CURVE_WITH_KNOTS ( ( 3, 2, 2, 2, 2, 3 ),
 ( 0.5000000000000002220, 0.5058823529411766717, 0.5117647058823531214, 0.5176470588235296821, 0.5235294117647061318, 0.5294117647058825815 ),
 .UNSPECIFIED. ) 
 CURVE ( )  GEOMETRIC_REPRESENTATION_ITEM ( )  RATIONAL_B_SPLINE_CURVE ( ( 0.9999999999999981126, 0.9510565162951554186, 1.000000000000000000, 0.9510565162951535312, 1.000000000000000000, 0.9510565162951535312, 1.000000000000000000, 0.9510565162951535312, 1.000000000000000000, 0.9510565162951516438, 1.000000000000001776 ) ) 
 REPRESENTATION_ITEM ( '' )  );
#21407 = ADVANCED_FACE ( 'NONE', ( #8541 ), #5694, .T. ) ;
#21408 = DIRECTION ( 'NONE',  ( 1.000000000000000000, 0.000000000000000000, 0.000000000000000000 ) ) ;
#21409 = CARTESIAN_POINT ( 'NONE',  ( 9.250000000000003553, 27.74999999999998934, 3.750000000000000000 ) ) ;
#21410 = ORIENTED_EDGE ( 'NONE', *, *, #65268, .T. ) ;
#21411 = CARTESIAN_POINT ( 'NONE',  ( -123.6549999999999869, -7.632228543268600340, -2.479861379858950166 ) ) ;
#21412 = ORIENTED_EDGE ( 'NONE', *, *, #25346, .T. ) ;
#21413 = FILL_AREA_STYLE_COLOUR ( '', #3856 ) ;
#21414 = ORIENTED_EDGE ( 'NONE', *, *, #2164, .T. ) ;
#21415 =( NAMED_UNIT ( * ) PLANE_ANGLE_UNIT ( ) SI_UNIT ( $, .RADIAN. ) );
#21416 = LINE ( 'NONE', #49908, #62480 ) ;
#21417 = ORIENTED_EDGE ( 'NONE', *, *, #34655, .T. ) ;
#21418 = AXIS2_PLACEMENT_3D ( 'NONE', #55317, #66577, #50071 ) ;
#21419 = VECTOR ( 'NONE', #41010, 1000.000000000000000 ) ;
#21420 = CARTESIAN_POINT ( 'NONE',  ( 9.058813317711338797, 150.8449999999999989, -2.943386871421372675 ) ) ;
#21421 = SURFACE_SIDE_STYLE ('',( #58722 ) ) ;
#21422 = VECTOR ( 'NONE', #55831, 1000.000000000000000 ) ;
#21423 = ORIENTED_EDGE ( 'NONE', *, *, #50704, .F. ) ;
#21424 = DIRECTION ( 'NONE',  ( 0.7713892158398690801, 0.000000000000000000, -0.6363636363636374638 ) ) ;
#21425 = FACE_OUTER_BOUND ( 'NONE', #33450, .T. ) ;
#21426 =( LENGTH_UNIT ( ) NAMED_UNIT ( * ) SI_UNIT ( .MILLI., .METRE. ) );
#21427 = ORIENTED_EDGE ( 'NONE', *, *, #34466, .F. ) ;
#21428 = CARTESIAN_POINT ( 'NONE',  ( -2.607480562269075097, 130.2929263765337851, 8.025000000000000355 ) ) ;
#21429 = CARTESIAN_POINT ( 'NONE',  ( 53.24999999999999289, 27.99999999999998579, 4.000000000000000000 ) ) ;
#21430 = CARTESIAN_POINT ( 'NONE',  ( -71.50000000000000000, 14.49137674618942562, 7.000000000000000000 ) ) ;
#21431 = VECTOR ( 'NONE', #38846, 1000.000000000000000 ) ;
#21432 = EDGE_CURVE ( 'NONE', #65961, #28130, #25048, .T. ) ;
#21433 = CARTESIAN_POINT ( 'NONE',  ( 7.632228543268608334, 125.3429263765338249, -2.479861379858951942 ) ) ;
#21434 = DIRECTION ( 'NONE',  ( 1.000000000000000000, 0.000000000000000000, 0.000000000000000000 ) ) ;
#21435 = ADVANCED_FACE ( 'NONE', ( #2495 ), #9231, .F. ) ;
#21436 = VERTEX_POINT ( 'NONE', #46906 ) ;
#21437 = CARTESIAN_POINT ( 'NONE',  ( -41.61274205743404053, 107.5029750606318544, -3.982828305957058390 ) ) ;
#21438 = ORIENTED_EDGE ( 'NONE', *, *, #10262, .T. ) ;
#21439 = CARTESIAN_POINT ( 'NONE',  ( -50.09292637653377511, 3.094860106618433360, 9.524999999999991473 ) ) ;
#21440 = CARTESIAN_POINT ( 'NONE',  ( 30.25000000000000711, 18.74999999999997868, 4.000000000000000000 ) ) ;
#21441 = CARTESIAN_POINT ( 'NONE',  ( -144.2050000000000125, -2.607480562269071545, -8.024999999999991473 ) ) ;
#21442 = CARTESIAN_POINT ( 'NONE',  ( 22.75000000000000711, 36.75000000000000000, 3.750000000000000000 ) ) ;
#21443 =( BOUNDED_CURVE ( )  B_SPLINE_CURVE ( 2, ( #31273, #4546, #20756, #42264, #63653, #15494, #36961, #24607, #67547, #19344, #40847 ),
 .UNSPECIFIED., .F., .F. ) 
 B_SPLINE_CURVE_WITH_KNOTS ( ( 3, 2, 2, 2, 2, 3 ),
 ( 0.9239130434782608647, 0.9260869565217391131, 0.9282608695652173614, 0.9304347826086956097, 0.9326086956521738580, 0.9347826086956522174 ),
 .UNSPECIFIED. ) 
 CURVE ( )  GEOMETRIC_REPRESENTATION_ITEM ( )  RATIONAL_B_SPLINE_CURVE ( ( 1.000000000000000000, 0.9510565162951535312, 1.000000000000000000, 0.9510565162951535312, 1.000000000000000000, 0.9510565162951535312, 1.000000000000000000, 0.9510565162951535312, 1.000000000000000000, 0.9510565162951535312, 1.000000000000000000 ) ) 
 REPRESENTATION_ITEM ( '' )  );
#21444 = LINE ( 'NONE', #43321, #63077 ) ;
#21445 = UNCERTAINTY_MEASURE_WITH_UNIT (LENGTH_MEASURE( 1.000000000000000082E-05 ), #59607, 'distance_accuracy_value', 'NONE');
#21446 = COLOUR_RGB ( '', 0.31764706, 0.68627451, 0.89019608) ;
#21447 = AXIS2_PLACEMENT_3D ( 'NONE', #24925, #41483, #3793 ) ;
#21448 = ADVANCED_FACE ( 'NONE', ( #20095 ), #45835, .T. ) ;
#21449 = DIRECTION ( 'NONE',  ( -0.7071067811865549002, 8.659560562355021605E-17, 0.7071067811865402453 ) ) ;
#21450 = CARTESIAN_POINT ( 'NONE',  ( -34.99999999999999289, 99.99999999999998579, 7.000000000000000000 ) ) ;
#21451 = SURFACE_STYLE_FILL_AREA ( #10222 ) ;
#21452 = ORIENTED_EDGE ( 'NONE', *, *, #63261, .F. ) ;
#21453 = AXIS2_PLACEMENT_3D ( 'NONE', #58596, #31853, #16066 ) ;
#21455 = EDGE_CURVE ( 'NONE', #41477, #21177, #18726, .T. ) ;
#21454 = EDGE_LOOP ( 'NONE', ( #45677, #51999, #34341, #20281 ) ) ;
#21456 = CYLINDRICAL_SURFACE ( 'NONE', #27182, 9.524999999999991473 ) ;
#21457 = DIRECTION ( 'NONE',  ( 1.000000000000000000, 0.000000000000000000, 0.000000000000000000 ) ) ;
#21458 = CARTESIAN_POINT ( 'NONE',  ( -59.15499999999998693, 7.632228543268600340, 2.479861379858949277 ) ) ;
#21459 = ORIENTED_EDGE ( 'NONE', *, *, #3368, .T. ) ;
#21460 = CARTESIAN_POINT ( 'NONE',  ( 1.000000000000000000, 1.000000000000000222, -3.000000000000000000 ) ) ;
#21461 = DIRECTION ( 'NONE',  ( 0.000000000000000000, -1.000000000000000000, 0.000000000000000000 ) ) ;
#21462 = DIRECTION ( 'NONE',  ( 0.000000000000000000, 1.000000000000000000, 0.000000000000000000 ) ) ;
#21463 =( NAMED_UNIT ( * ) PLANE_ANGLE_UNIT ( ) SI_UNIT ( $, .RADIAN. ) );
#21464 = EDGE_CURVE ( 'NONE', #46026, #47623, #57407, .T. ) ;
#21465 = CONICAL_SURFACE ( 'NONE', #28153, 6.999999999999997335, 0.7853981633974500554 ) ;
#21466 = CARTESIAN_POINT ( 'NONE',  ( 12.25000000000000355, 30.74999999999998579, 3.750000000000000000 ) ) ;
#21467 = CARTESIAN_POINT ( 'NONE',  ( -96.89292637653379359, -8.102448949553174629, -5.886773742842741797 ) ) ;
#21468 = VERTEX_POINT ( 'NONE', #2849 ) ;
#21469 = AXIS2_PLACEMENT_3D ( 'NONE', #17971, #67191, #55602 ) ;
#21470 = COLOUR_RGB ( '', 0.08235294, 0.09019608, 0.10196078) ;
#21471 = CARTESIAN_POINT ( 'NONE',  ( 22.99999999999998934, 5.000000000000000000, 37.00402776293825724 ) ) ;
#21472 = EDGE_CURVE ( 'NONE', #51817, #1374, #23679, .T. ) ;
#21473 = CYLINDRICAL_SURFACE ( 'NONE', #3440, 3.100000000000005418 ) ;
#21474 = SURFACE_STYLE_FILL_AREA ( #11609 ) ;
#21475 = MECHANICAL_DESIGN_GEOMETRIC_PRESENTATION_REPRESENTATION (  '', ( #15879 ), #50710 ) ;
#21476 = CARTESIAN_POINT ( 'NONE',  ( -107.3949999999999960, -6.826472737025113702, -4.959722759717900331 ) ) ;
#21477 = CARTESIAN_POINT ( 'NONE',  ( 10.01517768586949231, 159.6949999999999648, 1.839758294383810543E-15 ) ) ;
#21478 = CARTESIAN_POINT ( 'NONE',  ( -91.49499999999997613, 6.826472737025113702, -4.959722759717902107 ) ) ;
#21479 = CARTESIAN_POINT ( 'NONE',  ( -8.437984349512095861, 112.8070736234661382, -5.166775262442723748E-16 ) ) ;
#21480 = CIRCLE ( 'NONE', #27077, 5.249999999999997335 ) ;
#21481 = CARTESIAN_POINT ( 'NONE',  ( 3.000000000000002665, 42.00000000000000000, -89.00000000000000000 ) ) ;
#21482 = UNCERTAINTY_MEASURE_WITH_UNIT (LENGTH_MEASURE( 1.000000000000000082E-05 ), #26503, 'distance_accuracy_value', 'NONE');
#21483 = STYLED_ITEM ( 'NONE', ( #57214 ), #53990 ) ;
#21484 = EDGE_LOOP ( 'NONE', ( #18973, #4510, #4312, #57026 ) ) ;
#21485 = CARTESIAN_POINT ( 'NONE',  ( -136.4929263765338305, -8.102448949553172852, 5.886773742842742685 ) ) ;
#21486 = CARTESIAN_POINT ( 'NONE',  ( -145.6450000000000102, 4.716976649647091513, -6.492361379858946790 ) ) ;
#21487 = CARTESIAN_POINT ( 'NONE',  ( 16.00000000000001776, -3.148064030671221758, 34.68999999999999062 ) ) ;
#21488 = COLOUR_RGB ( '', 0.31764706, 0.68627451, 0.89019608) ;
#21489 = LINE ( 'NONE', #43001, #63271 ) ;
#21490 = PRESENTATION_STYLE_ASSIGNMENT (( #26742 ) ) ;
#21491 = ORIENTED_EDGE ( 'NONE', *, *, #62794, .T. ) ;
#21492 = ORIENTED_EDGE ( 'NONE', *, *, #6351, .T. ) ;
#21493 = AXIS2_PLACEMENT_3D ( 'NONE', #24417, #67013, #39612 ) ;
#21494 = CARTESIAN_POINT ( 'NONE',  ( 4.041451884327377897, -1.417096231345241097, 7.000000000000000888 ) ) ;
#21495 = UNCERTAINTY_MEASURE_WITH_UNIT (LENGTH_MEASURE( 1.000000000000000082E-05 ), #20676, 'distance_accuracy_value', 'NONE');
#21496 = EDGE_CURVE ( 'NONE', #59291, #57062, #57382, .T. ) ;
#21497 = PRESENTATION_STYLE_ASSIGNMENT (( #3543 ) ) ;
#21498 = DIRECTION ( 'NONE',  ( 0.000000000000000000, 0.000000000000000000, -1.000000000000000000 ) ) ;
#21499 = DIRECTION ( 'NONE',  ( -0.000000000000000000, -0.000000000000000000, 1.000000000000000000 ) ) ;
#21500 = EDGE_LOOP ( 'NONE', ( #15399, #448, #63056, #44263 ) ) ;
#21501 = CARTESIAN_POINT ( 'NONE',  ( -147.6549999999999727, -7.632228543268600340, -2.479861379858950166 ) ) ;
#21502 = ORIENTED_EDGE ( 'NONE', *, *, #49110, .T. ) ;
#21503 =( NAMED_UNIT ( * ) PLANE_ANGLE_UNIT ( ) SI_UNIT ( $, .RADIAN. ) );
#21504 = DIRECTION ( 'NONE',  ( 0.000000000000000000, 0.000000000000000000, 1.000000000000000000 ) ) ;
#21505 = ORIENTED_EDGE ( 'NONE', *, *, #42180, .F. ) ;
#21506 = AXIS2_PLACEMENT_3D ( 'NONE', #29258, #31698, #63370 ) ;
#21507 = CARTESIAN_POINT ( 'NONE',  ( -57.06152211476823766, -8.467913063795126760, -0.8045913523036769543 ) ) ;
#21508 = CARTESIAN_POINT ( 'NONE',  ( 39.74999999999999289, 0.000000000000000000, 3.750000000000000000 ) ) ;
#21509 = CARTESIAN_POINT ( 'NONE',  ( -3.094860106618432471, 124.5949999999999704, -9.525000000000000355 ) ) ;
#21510 = ORIENTED_EDGE ( 'NONE', *, *, #28489, .F. ) ;
#21511 = EDGE_CURVE ( 'NONE', #59375, #68323, #3394, .T. ) ;
#21512 = CARTESIAN_POINT ( 'NONE',  ( -55.00000000000000000, -2.024042244987997205E-14, 6.999999999999995559 ) ) ;
#21513 = CARTESIAN_POINT ( 'NONE',  ( -5.598654528085806881, 131.8549999999999898, -7.705886871421374629 ) ) ;
#21514 = CIRCLE ( 'NONE', #36099, 0.5000000000000004441 ) ;
#21515 = CARTESIAN_POINT ( 'NONE',  ( -68.45499999999998408, 7.632228543268599452, -2.479861379858951942 ) ) ;
#21516 = CARTESIAN_POINT ( 'NONE',  ( -124.6449999999999960, 4.716976649647091513, -6.492361379858946790 ) ) ;
#21517 = CARTESIAN_POINT ( 'NONE',  ( -41.05143861928701199, 107.9622656938500000, -3.673005875159361278 ) ) ;
#21518 = PRODUCT ( '16. Bolt M6x25', '16. Bolt M6x25', '', ( #50150 ) ) ;
#21519 = ORIENTED_EDGE ( 'NONE', *, *, #24861, .F. ) ;
#21520 = CARTESIAN_POINT ( 'NONE',  ( 9.058813317711338797, 145.9550000000000125, -2.943386871421372675 ) ) ;
#21521 = CARTESIAN_POINT ( 'NONE',  ( 15.98999599679679839, 118.4999999999999716, 10.00000000000000000 ) ) ;
#21522 = UNCERTAINTY_MEASURE_WITH_UNIT (LENGTH_MEASURE( 1.000000000000000082E-05 ), #33376, 'distance_accuracy_value', 'NONE');
#21523 = EDGE_CURVE ( 'NONE', #9623, #26861, #63048, .T. ) ;
#21524 = DIRECTION ( 'NONE',  ( 0.000000000000000000, 0.000000000000000000, 1.000000000000000000 ) ) ;
#21525 = VECTOR ( 'NONE', #54248, 1000.000000000000000 ) ;
#21526 = ADVANCED_FACE ( 'NONE', ( #14484 ), #32712, .T. ) ;
#21527 = LINE ( 'NONE', #53211, #2422 ) ;
#21528 = DIRECTION ( 'NONE',  ( 0.000000000000000000, 0.000000000000000000, 1.000000000000000000 ) ) ;
#21529 = EDGE_CURVE ( 'NONE', #32974, #19259, #26748, .T. ) ;
#21530 = SURFACE_SIDE_STYLE ('',( #43400 ) ) ;
#21531 = ORIENTED_EDGE ( 'NONE', *, *, #45154, .T. ) ;
#21532 = PRESENTATION_STYLE_ASSIGNMENT (( #65121 ) ) ;
#21533 = CARTESIAN_POINT ( 'NONE',  ( 41.49999999999998579, 108.0000000000000000, -3.000000000000000444 ) ) ;
#21534 = CARTESIAN_POINT ( 'NONE',  ( -175.5549999999999784, 0.000000000000000000, 8.024999999999991473 ) ) ;
#21535 = ORIENTED_EDGE ( 'NONE', *, *, #52845, .F. ) ;
#21536 = CARTESIAN_POINT ( 'NONE',  ( 72.00000000000000000, 36.32520566882265456, 9.500000000000000000 ) ) ;
#21537 = UNCERTAINTY_MEASURE_WITH_UNIT (LENGTH_MEASURE( 1.000000000000000082E-05 ), #31389, 'distance_accuracy_value', 'NONE');
#21538 =( GEOMETRIC_REPRESENTATION_CONTEXT ( 3 ) GLOBAL_UNCERTAINTY_ASSIGNED_CONTEXT ( ( #30633 ) ) GLOBAL_UNIT_ASSIGNED_CONTEXT ( ( #2426, #67198, #51033 ) ) REPRESENTATION_CONTEXT ( 'NONE', 'WORKASPACE' ) );
#21539 = SURFACE_SIDE_STYLE ('',( #38105 ) ) ;
#21540 = SURFACE_SIDE_STYLE ('',( #53222 ) ) ;
#21541 = FACE_OUTER_BOUND ( 'NONE', #29840, .T. ) ;
#21542 = AXIS2_PLACEMENT_3D ( 'NONE', #2923, #50824, #2579 ) ;
#21543 = ORIENTED_EDGE ( 'NONE', *, *, #57101, .T. ) ;
#21544 = EDGE_CURVE ( 'NONE', #31555, #31871, #50715, .T. ) ;
#21545 = DIRECTION ( 'NONE',  ( 1.000000000000000000, 0.000000000000000000, -1.300977106640434891E-16 ) ) ;
#21546 = FILL_AREA_STYLE ('',( #36737 ) ) ;
#21547 = CARTESIAN_POINT ( 'NONE',  ( -96.95499999999998408, -7.632228543268599452, 2.479861379858951054 ) ) ;
#21548 = ORIENTED_EDGE ( 'NONE', *, *, #4270, .T. ) ;
#21549 = LINE ( 'NONE', #43418, #63226 ) ;
#21550 = AXIS2_PLACEMENT_3D ( 'NONE', #29936, #34865, #56314 ) ;
#21551 = CARTESIAN_POINT ( 'NONE',  ( -135.6570736234661751, 9.058813317711329915, 2.943386871421369566 ) ) ;
#21552 = DIRECTION ( 'NONE',  ( 0.000000000000000000, 0.000000000000000000, 1.000000000000000000 ) ) ;
#21553 = CARTESIAN_POINT ( 'NONE',  ( -68.30707362346616662, -10.01517768586948698, 6.132527647946031529E-16 ) ) ;
#21554 =( GEOMETRIC_REPRESENTATION_CONTEXT ( 3 ) GLOBAL_UNCERTAINTY_ASSIGNED_CONTEXT ( ( #43468 ) ) GLOBAL_UNIT_ASSIGNED_CONTEXT ( ( #10217, #59404, #61477 ) ) REPRESENTATION_CONTEXT ( 'NONE', 'WORKASPACE' ) );
#21555 = EDGE_LOOP ( 'NONE', ( #53580, #49169, #13473, #58028 ) ) ;
#21556 = DIRECTION ( 'NONE',  ( -0.000000000000000000, -1.000000000000000000, -0.000000000000000000 ) ) ;
#21557 = DIRECTION ( 'NONE',  ( -0.000000000000000000, -1.000000000000000000, -0.000000000000000000 ) ) ;
#21558 = AXIS2_PLACEMENT_3D ( 'NONE', #6128, #16028, #59221 ) ;
#21560 = CARTESIAN_POINT ( 'NONE',  ( -23.71231517720798010, 117.4999999999999716, 9.500000000000000000 ) ) ;
#21559 = DIRECTION ( 'NONE',  ( -1.000000000000000000, 0.000000000000000000, 0.000000000000000000 ) ) ;
#21561 = CARTESIAN_POINT ( 'NONE',  ( -116.4549999999999841, 7.632228543268599452, -2.479861379858951942 ) ) ;
#21562 = EDGE_CURVE ( 'NONE', #37680, #5084, #4597, .T. ) ;
#21563 = CARTESIAN_POINT ( 'NONE',  ( -10.01517768586949231, 116.1949999999999932, -6.132527647946036459E-16 ) ) ;
#21564 = CARTESIAN_POINT ( 'NONE',  ( -112.7949999999999733, 2.607480562269068880, -8.024999999999993250 ) ) ;
#21565 = AXIS2_PLACEMENT_3D ( 'NONE', #2397, #45072, #56623 ) ;
#21566 = DIRECTION ( 'NONE',  ( 1.000000000000000000, 0.000000000000000000, 0.000000000000000000 ) ) ;
#21567 = EDGE_CURVE ( 'NONE', #17642, #36186, #31553, .T. ) ;
#21568 = DIRECTION ( 'NONE',  ( 0.000000000000000000, 0.000000000000000000, 1.000000000000000000 ) ) ;
#21569 = MECHANICAL_DESIGN_GEOMETRIC_PRESENTATION_REPRESENTATION (  '', ( #41789 ), #56347 ) ;
#21570 = CARTESIAN_POINT ( 'NONE',  ( -160.1929263765337907, -10.01517768586948698, 6.132527647946031529E-16 ) ) ;
#21571 = CARTESIAN_POINT ( 'NONE',  ( -175.1949999999999932, 8.437984349512085203, -1.550032578732815448E-15 ) ) ;
#21572 = AXIS2_PLACEMENT_3D ( 'NONE', #47801, #48122, #10795 ) ;
#21573 = DIRECTION ( 'NONE',  ( 0.000000000000000000, 0.000000000000000000, 1.000000000000000000 ) ) ;
#21574 = CARTESIAN_POINT ( 'NONE',  ( -46.46651340543134978, -13.74896002192117095, 0.8313647636153821407 ) ) ;
#21575 =( LENGTH_UNIT ( ) NAMED_UNIT ( * ) SI_UNIT ( .MILLI., .METRE. ) );
#21576 = ORIENTED_EDGE ( 'NONE', *, *, #25782, .T. ) ;
#21577 = VECTOR ( 'NONE', #39206, 1000.000000000000000 ) ;
#21578 = CARTESIAN_POINT ( 'NONE',  ( -79.04292637653379927, -9.058813317711329915, -2.943386871421370898 ) ) ;
#21579 = CONTEXT_DEPENDENT_SHAPE_REPRESENTATION ( #11846, #54763 ) ;
#21580 = DIRECTION ( 'NONE',  ( -1.000000000000000000, -0.000000000000000000, -0.000000000000000000 ) ) ;
#21581 = SURFACE_STYLE_USAGE ( .BOTH. , #17021 ) ;
#21582 = AXIS2_PLACEMENT_3D ( 'NONE', #7844, #44500, #23680 ) ;
#21583 = PRESENTATION_STYLE_ASSIGNMENT (( #14950 ) ) ;
#21584 = DIRECTION ( 'NONE',  ( 1.000000000000000000, 0.000000000000000000, 0.000000000000000000 ) ) ;
#21585 = DIRECTION ( 'NONE',  ( 1.387778780781444413E-14, 1.000000000000000000, 0.000000000000000000 ) ) ;
#21586 = CARTESIAN_POINT ( 'NONE',  ( -180.0550000000000068, -9.827790563157499189E-16, -8.024999999999991473 ) ) ;
#21587 = VERTEX_POINT ( 'NONE', #58446 ) ;
#21588 = FILL_AREA_STYLE_COLOUR ( '', #61677 ) ;
#21590 = EDGE_CURVE ( 'NONE', #22068, #52357, #37238, .T. ) ;
#21589 = DIRECTION ( 'NONE',  ( 0.000000000000000000, 0.000000000000000000, 1.000000000000000000 ) ) ;
#21591 = CARTESIAN_POINT ( 'NONE',  ( -43.75000000000000000, 0.000000000000000000, -5.100000000000000533 ) ) ;
#21592 = CARTESIAN_POINT ( 'NONE',  ( 41.49999999999997868, 9.999999999999978684, 3.500000000000000000 ) ) ;
#21593 = DIRECTION ( 'NONE',  ( 0.000000000000000000, 0.000000000000000000, -1.000000000000000000 ) ) ;
#21594 = CARTESIAN_POINT ( 'NONE',  ( -8.437984349512095861, 145.8070736234661808, -5.166775262442723748E-16 ) ) ;
#21595 = EDGE_LOOP ( 'NONE', ( #58148, #43700, #65472, #9186 ) ) ;
#21596 = EDGE_CURVE ( 'NONE', #3068, #10009, #31704, .T. ) ;
#21597 = LINE ( 'NONE', #43110, #55148 ) ;
#21598 = CARTESIAN_POINT ( 'NONE',  ( -93.95499999999998408, -7.632228543268599452, 2.479861379858951054 ) ) ;
#21599 = UNCERTAINTY_MEASURE_WITH_UNIT (LENGTH_MEASURE( 1.000000000000000082E-05 ), #8570, 'distance_accuracy_value', 'NONE');
#21600 = ORIENTED_EDGE ( 'NONE', *, *, #23574, .F. ) ;
#21601 = ADVANCED_FACE ( 'NONE', ( #39446 ), #668, .T. ) ;
#21602 = SURFACE_STYLE_FILL_AREA ( #16021 ) ;
#21603 = LINE ( 'NONE', #1475, #26576 ) ;
#21604 = FILL_AREA_STYLE_COLOUR ( '', #59796 ) ;
#21605 = ORIENTED_EDGE ( 'NONE', *, *, #35427, .F. ) ;
#21606 = TOROIDAL_SURFACE ( 'NONE', #58664, 4.750000000000000000, 0.2500000000000000000 ) ;
#21607 = DIRECTION ( 'NONE',  ( -0.000000000000000000, 1.000000000000000000, 0.000000000000000000 ) ) ;
#21608 = CARTESIAN_POINT ( 'NONE',  ( -65.39499999999998181, -6.826472737025115478, -4.959722759717899443 ) ) ;
#21609 = ORIENTED_EDGE ( 'NONE', *, *, #19689, .F. ) ;
#21610 = SURFACE_SIDE_STYLE ('',( #79 ) ) ;
#21611 = FILL_AREA_STYLE ('',( #26188 ) ) ;
#21612 = ORIENTED_EDGE ( 'NONE', *, *, #68089, .F. ) ;
#21613 = SURFACE_SIDE_STYLE ('',( #48394 ) ) ;
#21614 = ORIENTED_EDGE ( 'NONE', *, *, #5459, .T. ) ;
#21615 = STYLED_ITEM ( 'NONE', ( #3660 ), #23634 ) ;
#21616 = EDGE_CURVE ( 'NONE', #2945, #56729, #6009, .T. ) ;
#21617 = DIRECTION ( 'NONE',  ( -1.000000000000000000, 0.000000000000000000, 1.300977106640434891E-16 ) ) ;
#21618 = CARTESIAN_POINT ( 'NONE',  ( -125.3049999999999926, 8.437984349512085203, -1.550032578732815448E-15 ) ) ;
#21619 = ORIENTED_EDGE ( 'NONE', *, *, #56938, .T. ) ;
#21620 = VECTOR ( 'NONE', #21159, 1000.000000000000000 ) ;
#21621 = DIRECTION ( 'NONE',  ( 0.000000000000000000, 0.000000000000000000, -1.000000000000000000 ) ) ;
#21622 = VERTEX_POINT ( 'NONE', #60849 ) ;
#21623 = CARTESIAN_POINT ( 'NONE',  ( -159.4429263765338192, -1.166476076187852838E-15, -9.524999999999991473 ) ) ;
#21624 = CARTESIAN_POINT ( 'NONE',  ( 0.000000000000000000, 87.30187232391182306, 8.025000000000000355 ) ) ;
#21625 = CARTESIAN_POINT ( 'NONE',  ( -164.3070736234662093, -10.01517768586948698, 6.132527647946031529E-16 ) ) ;
#21626 = PRODUCT_DEFINITION_SHAPE ( 'NONE', 'NONE',  #69716 ) ;
#21627 = MECHANICAL_DESIGN_GEOMETRIC_PRESENTATION_REPRESENTATION (  '', ( #8183 ), #44178 ) ;
#21628 = CARTESIAN_POINT ( 'NONE',  ( -5.598654528085808657, 131.6449999999999818, 7.705886871421373741 ) ) ;
#21629 = CARTESIAN_POINT ( 'NONE',  ( -90.80707362346613820, 10.01517768586948698, -1.839758294383808571E-15 ) ) ;
#21630 = AXIS2_PLACEMENT_3D ( 'NONE', #47983, #12446, #48660 ) ;
#21631 = DIRECTION ( 'NONE',  ( -0.000000000000000000, -0.000000000000000000, 1.000000000000000000 ) ) ;
#21632 = ORIENTED_EDGE ( 'NONE', *, *, #65724, .T. ) ;
#21633 = CARTESIAN_POINT ( 'NONE',  ( 66.74999999999998579, 34.24999999999999289, 4.000000000000000000 ) ) ;
#21635 =( NAMED_UNIT ( * ) PLANE_ANGLE_UNIT ( ) SI_UNIT ( $, .RADIAN. ) );
#21634 = FILL_AREA_STYLE ('',( #55379 ) ) ;
#21636 = CARTESIAN_POINT ( 'NONE',  ( 11.00000000000001599, 43.00000000000000000, -28.38386403503541899 ) ) ;
#21637 = PRESENTATION_LAYER_ASSIGNMENT (  '', '', ( #68853 ) ) ;
#21638 = CARTESIAN_POINT ( 'NONE',  ( -136.5549999999999784, 0.000000000000000000, 8.024999999999991473 ) ) ;
#21639 = CARTESIAN_POINT ( 'NONE',  ( -85.85707362346617799, -5.598654528085803328, -7.705886871421366635 ) ) ;
#21640 =( LENGTH_UNIT ( ) NAMED_UNIT ( * ) SI_UNIT ( .MILLI., .METRE. ) );
#21641 = AXIS2_PLACEMENT_3D ( 'NONE', #6548, #27997, #49505 ) ;
#21642 = DIRECTION ( 'NONE',  ( 0.000000000000000000, 0.000000000000000000, -1.000000000000000000 ) ) ;
#21643 = CARTESIAN_POINT ( 'NONE',  ( -147.8949999999999818, 6.826472737025116366, 4.959722759717898555 ) ) ;
#21644 = CARTESIAN_POINT ( 'NONE',  ( -140.3949999999999818, -6.826472737025113702, -4.959722759717900331 ) ) ;
#21645 = ORIENTED_EDGE ( 'NONE', *, *, #18970, .T. ) ;
#21646 = CARTESIAN_POINT ( 'NONE',  ( 44.94709371290443300, 9.982364570967856565, -3.713690726390495911 ) ) ;
#21647 = DIRECTION ( 'NONE',  ( 0.000000000000000000, 0.000000000000000000, -1.000000000000000000 ) ) ;
#21648 = VECTOR ( 'NONE', #50852, 1000.000000000000000 ) ;
#21649 =( NAMED_UNIT ( * ) PLANE_ANGLE_UNIT ( ) SI_UNIT ( $, .RADIAN. ) );
#21650 = CARTESIAN_POINT ( 'NONE',  ( -52.70499999999996277, 2.607480562269073321, 8.024999999999991473 ) ) ;
#21651 = FACE_OUTER_BOUND ( 'NONE', #49177, .T. ) ;
#21652 = VECTOR ( 'NONE', #4921, 1000.000000000000000 ) ;
#21653 = CARTESIAN_POINT ( 'NONE',  ( -55.64499999999997470, 4.716976649647091513, -6.492361379858946790 ) ) ;
#21654 = FACE_OUTER_BOUND ( 'NONE', #47335, .T. ) ;
#21655 = CIRCLE ( 'NONE', #47591, 0.2500000000000002220 ) ;
#21656 = AXIS2_PLACEMENT_3D ( 'NONE', #17124, #7572, #7235 ) ;
#21657 = CARTESIAN_POINT ( 'NONE',  ( -154.7070736234665276, -3.094860106624346408, -9.524999999995696243 ) ) ;
#21658 = CARTESIAN_POINT ( 'NONE',  ( -102.4429263765338050, -1.166476076187852838E-15, -9.524999999999991473 ) ) ;
#21659 = CARTESIAN_POINT ( 'NONE',  ( 35.50000000000014921, 100.0000000000000142, 74.99999999999997158 ) ) ;
#21660 = SURFACE_STYLE_USAGE ( .BOTH. , #47407 ) ;
#21661 = MECHANICAL_DESIGN_GEOMETRIC_PRESENTATION_REPRESENTATION (  '', ( #11563 ), #25031 ) ;
#21662 = DIRECTION ( 'NONE',  ( 0.000000000000000000, 0.000000000000000000, 1.000000000000000000 ) ) ;
#21663 = CARTESIAN_POINT ( 'NONE',  ( -99.80707362346616662, 10.01517768586948698, -1.839758294383808966E-15 ) ) ;
#21664 = AXIS2_PLACEMENT_3D ( 'NONE', #29664, #7510, #23683 ) ;
#21665 = CARTESIAN_POINT ( 'NONE',  ( -13.74999999999998757, -7.950815931560351124E-15, 3.750000000000000000 ) ) ;
#21666 = CIRCLE ( 'NONE', #20571, 1.000000000000000888 ) ;
#21667 = CYLINDRICAL_SURFACE ( 'NONE', #30721, 1.000000000000000888 ) ;
#21668 = ADVANCED_FACE ( 'NONE', ( #43694 ), #17959, .T. ) ;
#21669 = DIRECTION ( 'NONE',  ( 0.000000000000000000, 0.000000000000000000, -1.000000000000000000 ) ) ;
#21670 = ORIENTED_EDGE ( 'NONE', *, *, #17948, .T. ) ;
#21671 =( LENGTH_UNIT ( ) NAMED_UNIT ( * ) SI_UNIT ( .MILLI., .METRE. ) );
#21672 = VECTOR ( 'NONE', #65741, 1000.000000000000000 ) ;
#21673 = CARTESIAN_POINT ( 'NONE',  ( 6.826472737025119919, 117.0070736234661410, 4.959722759717908325 ) ) ;
#21674 = AXIS2_PLACEMENT_3D ( 'NONE', #45462, #29922, #19357 ) ;
#21675 = CARTESIAN_POINT ( 'NONE',  ( -20.58979310427664444, 114.8389001175783051, 9.999999999999879208 ) ) ;
#21676 = CARTESIAN_POINT ( 'NONE',  ( 75.00000000000000000, 20.33294439365979756, -6.261747904192522363 ) ) ;
#21677 =( LENGTH_UNIT ( ) NAMED_UNIT ( * ) SI_UNIT ( .MILLI., .METRE. ) );
#21678 = ORIENTED_EDGE ( 'NONE', *, *, #14636, .F. ) ;
#21679 = ORIENTED_EDGE ( 'NONE', *, *, #33462, .F. ) ;
#21680 = STYLED_ITEM ( 'NONE', ( #60358 ), #7177 ) ;
#21681 = CARTESIAN_POINT ( 'NONE',  ( -17.75000000000000711, 31.24999999999999289, 4.000000000000000000 ) ) ;
#21682 = DIRECTION ( 'NONE',  ( 0.000000000000000000, 0.000000000000000000, -1.000000000000000000 ) ) ;
#21683 = AXIS2_PLACEMENT_3D ( 'NONE', #65768, #54836, #56232 ) ;
#21684 = EDGE_CURVE ( 'NONE', #38142, #32231, #38063, .T. ) ;
#21685 = ORIENTED_EDGE ( 'NONE', *, *, #5159, .F. ) ;
#21686 = CARTESIAN_POINT ( 'NONE',  ( -3.094860106618434248, 126.9049999999999869, 9.525000000000000355 ) ) ;
#21687 = SURFACE_SIDE_STYLE ('',( #48463 ) ) ;
#21688 = DIRECTION ( 'NONE',  ( -1.000000000000000000, 0.000000000000000000, 0.000000000000000000 ) ) ;
#21689 = MECHANICAL_DESIGN_GEOMETRIC_PRESENTATION_REPRESENTATION (  '', ( #28378 ), #25055 ) ;
#21690 = EDGE_CURVE ( 'NONE', #30586, #55963, #16987, .T. ) ;
#21691 = ADVANCED_FACE ( 'NONE', ( #59457 ), #2042, .F. ) ;
#21692 = CARTESIAN_POINT ( 'NONE',  ( 71.50000000000000000, 35.92875272052971525, 9.500000000000000000 ) ) ;
#21693 = CARTESIAN_POINT ( 'NONE',  ( -104.8449999999999989, -7.632228543268599452, 2.479861379858951054 ) ) ;
#21694 = ORIENTED_EDGE ( 'NONE', *, *, #35258, .T. ) ;
#21695 = AXIS2_PLACEMENT_3D ( 'NONE', #3879, #19382, #31670 ) ;
#21696 = FACE_OUTER_BOUND ( 'NONE', #51917, .T. ) ;
#21697 = ADVANCED_FACE ( 'NONE', ( #6353, #1370, #48974 ), #65453, .F. ) ;
#21698 = ORIENTED_EDGE ( 'NONE', *, *, #32010, .F. ) ;
#21699 = CARTESIAN_POINT ( 'NONE',  ( 30.25000000000000711, 18.99999999999997868, -3.750000000000000000 ) ) ;
#21700 = DIRECTION ( 'NONE',  ( 0.000000000000000000, 0.000000000000000000, 1.000000000000000000 ) ) ;
#21701 = FILL_AREA_STYLE ('',( #48476 ) ) ;
#21702 = CARTESIAN_POINT ( 'NONE',  ( 20.55652580482692926, 114.6393193824117844, -10.28299520148690682 ) ) ;
#21703 = VERTEX_POINT ( 'NONE', #7051 ) ;
#21704 = CARTESIAN_POINT ( 'NONE',  ( -165.6570736234661751, 9.058813317711329915, 2.943386871421369566 ) ) ;
#21705 = CARTESIAN_POINT ( 'NONE',  ( -45.00000000000000000, 0.000000000000000000, 8.525000000000000355 ) ) ;
#21706 = DIRECTION ( 'NONE',  ( 0.000000000000000000, 0.000000000000000000, -1.000000000000000000 ) ) ;
#21707 = STYLED_ITEM ( 'NONE', ( #36936 ), #48104 ) ;
#21708 = COLOUR_RGB ( '', 0.72549020, 0.75294118, 0.79215686) ;
#21709 =( NAMED_UNIT ( * ) SI_UNIT ( $, .STERADIAN. ) SOLID_ANGLE_UNIT ( ) );
#21710 = CARTESIAN_POINT ( 'NONE',  ( -71.99999999999998579, 64.07124727947029896, 7.500000000000000000 ) ) ;
#21711 = APPLICATION_CONTEXT ( 'automotive_design' ) ;
#21712 = SURFACE_STYLE_FILL_AREA ( #27654 ) ;
#21713 = DIRECTION ( 'NONE',  ( -5.782411586589351722E-16, 1.000000000000000000, 0.000000000000000000 ) ) ;
#21714 = CARTESIAN_POINT ( 'NONE',  ( 4.716976649647096842, 115.7429263765338163, 6.492361379858953896 ) ) ;
#21715 = CARTESIAN_POINT ( 'NONE',  ( -115.3429263765337964, -9.058813317711329915, 2.943386871421371787 ) ) ;
#21716 = EDGE_LOOP ( 'NONE', ( #33982, #21884, #3315, #48004 ) ) ;
#21717 = ORIENTED_EDGE ( 'NONE', *, *, #40052, .F. ) ;
#21718 = FACE_OUTER_BOUND ( 'NONE', #27480, .T. ) ;
#21719 = CARTESIAN_POINT ( 'NONE',  ( -58.55707362346616662, -1.166476076187852838E-15, -9.524999999999991473 ) ) ;
#21720 = DIRECTION ( 'NONE',  ( 0.000000000000000000, 0.000000000000000000, 1.000000000000000000 ) ) ;
#21721 = ORIENTED_EDGE ( 'NONE', *, *, #59099, .F. ) ;
#21722 = FACE_OUTER_BOUND ( 'NONE', #27583, .T. ) ;
#21723 = AXIS2_PLACEMENT_3D ( 'NONE', #30048, #62743, #62050 ) ;
#21724 = CARTESIAN_POINT ( 'NONE',  ( -170.4549999999999841, 7.632228543268599452, -2.479861379858951942 ) ) ;
#21725 = LINE ( 'NONE', #59016, #38615 ) ;
#21726 = CARTESIAN_POINT ( 'NONE',  ( 8.750000000000001776, 25.24999999999998934, 3.750000000000000000 ) ) ;
#21727 = CARTESIAN_POINT ( 'NONE',  ( -178.1949999999999648, 8.437984349512085203, -1.550032578732815448E-15 ) ) ;
#21728 = AXIS2_PLACEMENT_3D ( 'NONE', #50265, #66428, #23507 ) ;
#21729 = CARTESIAN_POINT ( 'NONE',  ( -164.5449999999999875, -7.632228543268600340, -2.479861379858950166 ) ) ;
#21730 = ORIENTED_EDGE ( 'NONE', *, *, #69191, .T. ) ;
#21731 = AXIS2_PLACEMENT_3D ( 'NONE', #18907, #24889, #18600 ) ;
#21732 = FILL_AREA_STYLE ('',( #205 ) ) ;
#21733 = DIRECTION ( 'NONE',  ( -0.000000000000000000, 1.000000000000000000, -0.000000000000000000 ) ) ;
#21734 = PRESENTATION_STYLE_ASSIGNMENT (( #17847 ) ) ;
#21735 = AXIS2_PLACEMENT_3D ( 'NONE', #43952, #21408, #43284 ) ;
#21736 = CARTESIAN_POINT ( 'NONE',  ( -87.35499999999998977, -4.716976649647093289, -6.492361379858945902 ) ) ;
#21737 = CARTESIAN_POINT ( 'NONE',  ( 0.4142135623730951455, 42.99999999999999289, -35.49999999999999289 ) ) ;
#21738 = LINE ( 'NONE', #63942, #66287 ) ;
#21739 = CARTESIAN_POINT ( 'NONE',  ( -75.48275862205373699, 36.00832590027795987, -9.539713814030060135 ) ) ;
#21740 = AXIS2_PLACEMENT_3D ( 'NONE', #27801, #53538, #49307 ) ;
#21741 = AXIS2_PLACEMENT_3D ( 'NONE', #46456, #58344, #30556 ) ;
#21742 = CARTESIAN_POINT ( 'NONE',  ( -76.79499999999998749, 2.607480562269069324, -8.024999999999993250 ) ) ;
#21743 = CARTESIAN_POINT ( 'NONE',  ( 5.598654528085809545, 134.2549999999999955, -7.705886871421373741 ) ) ;
#21744 = CARTESIAN_POINT ( 'NONE',  ( 7.441974819423175624, -1.110121504110839430, 0.4967607073414704866 ) ) ;
#21745 = CARTESIAN_POINT ( 'NONE',  ( -172.2570736234661695, 5.598654528085800663, -7.705886871421367523 ) ) ;
#21746 = FACE_OUTER_BOUND ( 'NONE', #27048, .T. ) ;
#21747 = SHAPE_REPRESENTATION ( '12. Washer', ( #42840 ), #24690 ) ;
#21748 = AXIS2_PLACEMENT_3D ( 'NONE', #10829, #873, #43576 ) ;
#21749 = FACE_OUTER_BOUND ( 'NONE', #609, .T. ) ;
#21750 = STYLED_ITEM ( 'NONE', ( #5458 ), #8923 ) ;
#21751 = VERTEX_POINT ( 'NONE', #60171 ) ;
#21752 = CYLINDRICAL_SURFACE ( 'NONE', #8948, 0.2500000000000002220 ) ;
#21753 = MECHANICAL_DESIGN_GEOMETRIC_PRESENTATION_REPRESENTATION (  '', ( #26369 ), #1616 ) ;
#21754 = CARTESIAN_POINT ( 'NONE',  ( -10.39230484541326938, 1.107695154586735509, -1.661048719744147042E-15 ) ) ;
#21755 = EDGE_CURVE ( 'NONE', #38501, #40909, #68641, .T. ) ;
#21757 = SURFACE_SIDE_STYLE ('',( #42240 ) ) ;
#21756 = DIRECTION ( 'NONE',  ( 0.000000000000000000, 0.000000000000000000, -1.000000000000000000 ) ) ;
#21758 = CARTESIAN_POINT ( 'NONE',  ( 0.000000000000000000, 146.9429263765338192, -8.025000000000000355 ) ) ;
#21759 = ORIENTED_EDGE ( 'NONE', *, *, #38213, .T. ) ;
#21761 = ORIENTED_EDGE ( 'NONE', *, *, #68917, .F. ) ;
#21760 = AXIS2_PLACEMENT_3D ( 'NONE', #14318, #19591, #35077 ) ;
#21762 = MECHANICAL_DESIGN_GEOMETRIC_PRESENTATION_REPRESENTATION (  '', ( #34109 ), #63343 ) ;
#21763 = CARTESIAN_POINT ( 'NONE',  ( 5.429140806177446840E-16, 13.58578643762690419, -35.91421356237308515 ) ) ;
#21764 = CARTESIAN_POINT ( 'NONE',  ( -13.75000000000000533, 30.99999999999999289, -3.750000000000000000 ) ) ;
#21765 = EDGE_CURVE ( 'NONE', #51230, #58139, #1725, .T. ) ;
#21766 = VECTOR ( 'NONE', #41219, 999.9999999999998863 ) ;
#21767 = CIRCLE ( 'NONE', #12761, 13.00000000000000178 ) ;
#21768 = FACE_OUTER_BOUND ( 'NONE', #60044, .T. ) ;
#21769 = DIRECTION ( 'NONE',  ( 0.000000000000000000, 0.000000000000000000, 1.000000000000000000 ) ) ;
#21770 =( NAMED_UNIT ( * ) PLANE_ANGLE_UNIT ( ) SI_UNIT ( $, .RADIAN. ) );
#21771 = ORIENTED_EDGE ( 'NONE', *, *, #17893, .F. ) ;
#21772 = CARTESIAN_POINT ( 'NONE',  ( -108.8049999999999784, -8.437984349512086979, 5.166775262442717831E-16 ) ) ;
#21773 = ORIENTED_EDGE ( 'NONE', *, *, #10511, .T. ) ;
#21774 = LINE ( 'NONE', #43289, #44411 ) ;
#21775 = CARTESIAN_POINT ( 'NONE',  ( 21.02379604162863558, 114.6405644170961153, -10.00000000000000000 ) ) ;
#21776 = MECHANICAL_DESIGN_GEOMETRIC_PRESENTATION_REPRESENTATION (  '', ( #61079 ), #7164 ) ;
#21777 = EDGE_LOOP ( 'NONE', ( #36801, #67462, #6034, #52017 ) ) ;
#21778 = CYLINDRICAL_SURFACE ( 'NONE', #54898, 0.9999999999999974465 ) ;
#21779 = LINE ( 'NONE', #42576, #563 ) ;
#21780 = ORIENTED_EDGE ( 'NONE', *, *, #65011, .F. ) ;
#21781 = EDGE_CURVE ( 'NONE', #6197, #34838, #47333, .T. ) ;
#21782 = COLOUR_RGB ( '', 0.09019608, 0.27058824, 0.51372549) ;
#21783 = CARTESIAN_POINT ( 'NONE',  ( -5.598654528085808657, 158.6449999999999818, 7.705886871421373741 ) ) ;
#21784 = SURFACE_STYLE_FILL_AREA ( #53773 ) ;
#21785 = AXIS2_PLACEMENT_3D ( 'NONE', #37156, #4038, #32181 ) ;
#21786 = ORIENTED_EDGE ( 'NONE', *, *, #36008, .F. ) ;
#21787 = CARTESIAN_POINT ( 'NONE',  ( 59.00000000000000000, 11.99999999999999822, -4.000000000000000000 ) ) ;
#21788 = LINE ( 'NONE', #43303, #8142 ) ;
#21789 = ADVANCED_FACE ( 'NONE', ( #23240 ), #44734, .F. ) ;
#21790 = CARTESIAN_POINT ( 'NONE',  ( -181.3429263765338249, -9.058813317711329915, 2.943386871421371787 ) ) ;
#21791 = AXIS2_PLACEMENT_3D ( 'NONE', #42322, #51786, #35607 ) ;
#21792 = EDGE_LOOP ( 'NONE', ( #23084, #66700, #25087, #26143 ) ) ;
#21793 = CARTESIAN_POINT ( 'NONE',  ( 6.826472737025121695, 122.4929263765338021, -4.959722759717905660 ) ) ;
#21794 = PLANE ( 'NONE',  #57019 ) ;
#21795 = SURFACE_STYLE_FILL_AREA ( #31642 ) ;
#21796 = VECTOR ( 'NONE', #61914, 1000.000000000000000 ) ;
#21797 = CIRCLE ( 'NONE', #34199, 5.000000000000004441 ) ;
#21798 = DIRECTION ( 'NONE',  ( 1.000000000000000000, 0.000000000000000000, 0.000000000000000000 ) ) ;
#21799 = DIRECTION ( 'NONE',  ( 0.000000000000000000, 0.000000000000000000, 1.000000000000000000 ) ) ;
#21800 = ORIENTED_EDGE ( 'NONE', *, *, #5570, .F. ) ;
#21801 = DIRECTION ( 'NONE',  ( 0.000000000000000000, -1.000000000000000000, 0.000000000000000000 ) ) ;
#21802 = ORIENTED_EDGE ( 'NONE', *, *, #455, .T. ) ;
#21803 = PRESENTATION_STYLE_ASSIGNMENT (( #54816 ) ) ;
#21804 = COLOUR_RGB ( '', 0.40784314, 0.44705882, 0.49803922) ;
#21805 = CARTESIAN_POINT ( 'NONE',  ( -139.8550000000000182, 4.716976649647094177, 6.492361379858945902 ) ) ;
#21806 = DIRECTION ( 'NONE',  ( -1.000000000000000000, -0.000000000000000000, 0.000000000000000000 ) ) ;
#21807 = SURFACE_STYLE_USAGE ( .BOTH. , #20776 ) ;
#21808 = AXIS2_PLACEMENT_3D ( 'NONE', #7287, #44949, #40023 ) ;
#21809 = PRESENTATION_LAYER_ASSIGNMENT (  '', '', ( #20536 ) ) ;
#21810 = CARTESIAN_POINT ( 'NONE',  ( -106.1929263765338050, -10.01517768586948698, 6.132527647946031529E-16 ) ) ;
#21811 = DIRECTION ( 'NONE',  ( -0.6216216216216311485, 0.7833176619561784682, 0.000000000000000000 ) ) ;
#21812 = ORIENTED_EDGE ( 'NONE', *, *, #62970, .T. ) ;
#21813 = ORIENTED_EDGE ( 'NONE', *, *, #46346, .F. ) ;
#21814 = DIRECTION ( 'NONE',  ( 0.000000000000000000, 1.000000000000000000, 0.000000000000000000 ) ) ;
#21815 = DIRECTION ( 'NONE',  ( 0.000000000000000000, 0.000000000000000000, -1.000000000000000000 ) ) ;
#21817 = CARTESIAN_POINT ( 'NONE',  ( -55.40499999999997982, -2.607480562269069768, 8.024999999999991473 ) ) ;
#21816 = VECTOR ( 'NONE', #47821, 1000.000000000000000 ) ;
#21818 = ORIENTED_EDGE ( 'NONE', *, *, #59335, .F. ) ;
#21819 = CARTESIAN_POINT ( 'NONE',  ( 60.99999999999998579, 50.00000000000000000, 7.500000000000000000 ) ) ;
#21820 = FACE_OUTER_BOUND ( 'NONE', #42837, .T. ) ;
#21821 = DIRECTION ( 'NONE',  ( -1.000000000000000000, 0.000000000000000000, 0.000000000000000000 ) ) ;
#21822 = PLANE ( 'NONE',  #35771 ) ;
#21823 = AXIS2_PLACEMENT_3D ( 'NONE', #33610, #38938, #6878 ) ;
#21824 = MECHANICAL_DESIGN_GEOMETRIC_PRESENTATION_REPRESENTATION (  '', ( #39830 ), #34171 ) ;
#21825 =( NAMED_UNIT ( * ) SI_UNIT ( $, .STERADIAN. ) SOLID_ANGLE_UNIT ( ) );
#21826 = CARTESIAN_POINT ( 'NONE',  ( -96.74292637653380211, -5.598654528085803328, -7.705886871421366635 ) ) ;
#21827 = EDGE_LOOP ( 'NONE', ( #7406, #24529, #43218, #68516, #10196, #54492, #62263, #36041 ) ) ;
#21828 = EDGE_CURVE ( 'NONE', #4257, #59022, #57436, .T. ) ;
#21829 = CARTESIAN_POINT ( 'NONE',  ( -195.0000000000000000, 9.184850993605132167E-16, -7.499999999999985789 ) ) ;
#21830 = DIRECTION ( 'NONE',  ( -0.000000000000000000, 0.000000000000000000, -1.000000000000000000 ) ) ;
#21831 = CARTESIAN_POINT ( 'NONE',  ( -15.00000000000000000, 8.000000000000000000, 3.500000000000003997 ) ) ;
#21832 = CARTESIAN_POINT ( 'NONE',  ( 0.000000000000000000, 127.0570736234661666, -8.025000000000000355 ) ) ;
#21833 = AXIS2_PLACEMENT_3D ( 'NONE', #57671, #15139, #36617 ) ;
#21834 = CARTESIAN_POINT ( 'NONE',  ( -110.2449999999999903, -4.716976649647093289, -6.492361379858945902 ) ) ;
#21835 = CARTESIAN_POINT ( 'NONE',  ( -8.102448949553181734, 154.8949999999999534, -5.886773742842749790 ) ) ;
#21836 = CARTESIAN_POINT ( 'NONE',  ( -89.54499999999998749, -7.632228543268600340, -2.479861379858950166 ) ) ;
#21837 = LINE ( 'NONE', #64393, #17397 ) ;
#21838 = FILL_AREA_STYLE ('',( #42635 ) ) ;
#21839 = LINE ( 'NONE', #654, #6951 ) ;
#21840 = AXIS2_PLACEMENT_3D ( 'NONE', #7597, #29024, #50528 ) ;
#21841 = CARTESIAN_POINT ( 'NONE',  ( 3.999798566743339556, 8.867945265733707672, -2.000000000000000000 ) ) ;
#21842 =( GEOMETRIC_REPRESENTATION_CONTEXT ( 3 ) GLOBAL_UNCERTAINTY_ASSIGNED_CONTEXT ( ( #2241 ) ) GLOBAL_UNIT_ASSIGNED_CONTEXT ( ( #47721, #36071, #63486 ) ) REPRESENTATION_CONTEXT ( 'NONE', 'WORKASPACE' ) );
#21843 = EDGE_LOOP ( 'NONE', ( #48377, #30918, #22805, #25032 ) ) ;
#21844 = CARTESIAN_POINT ( 'NONE',  ( -123.4429263765338192, -1.166476076187852838E-15, -9.524999999999991473 ) ) ;
#21845 = CIRCLE ( 'NONE', #61141, 0.5000000000000004441 ) ;
#21846 =( NAMED_UNIT ( * ) PLANE_ANGLE_UNIT ( ) SI_UNIT ( $, .RADIAN. ) );
#21847 = CARTESIAN_POINT ( 'NONE',  ( -143.6949999999999932, -8.437984349512085203, 5.166775262442717831E-16 ) ) ;
#21848 = FILL_AREA_STYLE ('',( #16255 ) ) ;
#21849 = EDGE_CURVE ( 'NONE', #44684, #46060, #3095, .T. ) ;
#21850 = VECTOR ( 'NONE', #30828, 1000.000000000000000 ) ;
#21851 = EDGE_CURVE ( 'NONE', #2677, #42412, #57, .T. ) ;
#21852 = SURFACE_STYLE_FILL_AREA ( #663 ) ;
#21853 = EDGE_LOOP ( 'NONE', ( #62611, #45085, #17485, #25262 ) ) ;
#21854 = ORIENTED_EDGE ( 'NONE', *, *, #11741, .T. ) ;
#21855 = CYLINDRICAL_SURFACE ( 'NONE', #48339, 0.2500000000000002220 ) ;
#21856 = DIRECTION ( 'NONE',  ( -0.000000000000000000, -0.000000000000000000, -1.000000000000000000 ) ) ;
#21857 = VECTOR ( 'NONE', #68636, 1000.000000000000000 ) ;
#21858 = EDGE_CURVE ( 'NONE', #64972, #42340, #25925, .T. ) ;
#21859 = CARTESIAN_POINT ( 'NONE',  ( 25.00000000000000000, 1.000000000000000888, 4.000000000000000000 ) ) ;
#21860 = CARTESIAN_POINT ( 'NONE',  ( -45.00000000000036238, 8.675277573170289358, 5.941086794573004148 ) ) ;
#21861 = CARTESIAN_POINT ( 'NONE',  ( -129.5070736234661695, 8.102448949553176405, 5.886773742842740909 ) ) ;
#21862 = CARTESIAN_POINT ( 'NONE',  ( -51.05707362346617373, 0.000000000000000000, 9.524999999999991473 ) ) ;
#21863 = DIRECTION ( 'NONE',  ( 1.000000000000000000, -1.776356839400250465E-15, 0.000000000000000000 ) ) ;
#21864 = EDGE_LOOP ( 'NONE', ( #64995, #56970, #18391, #52104 ) ) ;
#21865 = CARTESIAN_POINT ( 'NONE',  ( -138.0549999999999784, -9.827790563157499189E-16, -8.024999999999991473 ) ) ;
#21866 = AXIS2_PLACEMENT_3D ( 'NONE', #3510, #25014, #62631 ) ;
#21867 = ORIENTED_EDGE ( 'NONE', *, *, #42162, .T. ) ;
#21868 = DIRECTION ( 'NONE',  ( 1.000000000000000000, -1.776356839400250465E-15, 0.000000000000000000 ) ) ;
#21869 = DIRECTION ( 'NONE',  ( 0.000000000000000000, -0.000000000000000000, -1.000000000000000000 ) ) ;
#21870 = ORIENTED_EDGE ( 'NONE', *, *, #30307, .T. ) ;
#21871 = EDGE_CURVE ( 'NONE', #26545, #67683, #57314, .T. ) ;
#21872 =( GEOMETRIC_REPRESENTATION_CONTEXT ( 3 ) GLOBAL_UNCERTAINTY_ASSIGNED_CONTEXT ( ( #48779 ) ) GLOBAL_UNIT_ASSIGNED_CONTEXT ( ( #26672, #16527, #11209 ) ) REPRESENTATION_CONTEXT ( 'NONE', 'WORKASPACE' ) );
#21873 = CIRCLE ( 'NONE', #20772, 0.5000000000000004441 ) ;
#21874 = CARTESIAN_POINT ( 'NONE',  ( -54.73148258177010916, -9.107254030102707176, -2.000000000008438139 ) ) ;
#21875 = CARTESIAN_POINT ( 'NONE',  ( 8.102448949553183510, 126.9950000000000045, -5.886773742842746238 ) ) ;
#21876 = LINE ( 'NONE', #69028, #8178 ) ;
#21877 = ORIENTED_EDGE ( 'NONE', *, *, #62985, .F. ) ;
#21878 = CARTESIAN_POINT ( 'NONE',  ( 44.91886116991580735, 10.49999999999998224, -6.500000000000000000 ) ) ;
#21879 = CARTESIAN_POINT ( 'NONE',  ( 3.094860106618435136, 134.4049999999999727, -9.525000000000000355 ) ) ;
#21880 = CARTESIAN_POINT ( 'NONE',  ( -67.10499999999998977, -6.826472737025113702, 4.959722759717902107 ) ) ;
#21881 = CARTESIAN_POINT ( 'NONE',  ( -119.0949999999999847, -2.607480562269071545, -8.024999999999991473 ) ) ;
#21882 = EDGE_CURVE ( 'NONE', #44845, #51757, #3455, .T. ) ;
#21883 = DIRECTION ( 'NONE',  ( 1.000000000000000000, 0.000000000000000000, 0.000000000000000000 ) ) ;
#21884 = ORIENTED_EDGE ( 'NONE', *, *, #9795, .F. ) ;
#21885 = CARTESIAN_POINT ( 'NONE',  ( -10.01517768586949231, 150.3050000000000068, -6.132527647946036459E-16 ) ) ;
#21886 = TOROIDAL_SURFACE ( 'NONE', #57837, 111.0000000000000142, 1.000000000000000000 ) ;
#21887 = CARTESIAN_POINT ( 'NONE',  ( 44.99999999999998579, 119.9999999999999716, -9.500000000000000000 ) ) ;
#21888 = CARTESIAN_POINT ( 'NONE',  ( -44.99999999999977973, 146.9999999999999716, -7.500000000000000000 ) ) ;
#21889 = AXIS2_PLACEMENT_3D ( 'NONE', #57860, #20193, #52588 ) ;
#21890 = PLANE ( 'NONE',  #44470 ) ;
#21891 = EDGE_LOOP ( 'NONE', ( #4677, #45475, #18662, #49374 ) ) ;
#21892 = CARTESIAN_POINT ( 'NONE',  ( -32.97523664431077606, -9.117691409006596359, -3.352975844304635356 ) ) ;
#21894 = DIRECTION ( 'NONE',  ( 0.000000000000000000, 0.000000000000000000, -1.000000000000000000 ) ) ;
#21893 =( GEOMETRIC_REPRESENTATION_CONTEXT ( 3 ) GLOBAL_UNCERTAINTY_ASSIGNED_CONTEXT ( ( #55254 ) ) GLOBAL_UNIT_ASSIGNED_CONTEXT ( ( #37519, #64549, #32506 ) ) REPRESENTATION_CONTEXT ( 'NONE', 'WORKASPACE' ) );
#21895 = CARTESIAN_POINT ( 'NONE',  ( -173.0049999999999670, 6.826472737025116366, 4.959722759717898555 ) ) ;
#21896 = ORIENTED_EDGE ( 'NONE', *, *, #69308, .T. ) ;
#21897 = DIRECTION ( 'NONE',  ( 0.000000000000000000, 1.000000000000000000, 0.000000000000000000 ) ) ;
#21898 = MECHANICAL_DESIGN_GEOMETRIC_PRESENTATION_REPRESENTATION (  '', ( #27488 ), #28644 ) ;
#21899 = DIRECTION ( 'NONE',  ( 0.000000000000000000, -1.000000000000000000, 0.000000000000000000 ) ) ;
#21900 = CARTESIAN_POINT ( 'NONE',  ( -76.94292637653380496, 0.000000000000000000, 9.524999999999991473 ) ) ;
#21901 = EDGE_LOOP ( 'NONE', ( #42969, #37407, #67558, #596 ) ) ;
#21902 = DIRECTION ( 'NONE',  ( -0.000000000000000000, 0.000000000000000000, -1.000000000000000000 ) ) ;
#21903 = PRESENTATION_STYLE_ASSIGNMENT (( #38114 ) ) ;
#21904 = CARTESIAN_POINT ( 'NONE',  ( -87.65499999999998693, -7.632228543268600340, -2.479861379858950166 ) ) ;
#21905 = ORIENTED_EDGE ( 'NONE', *, *, #13091, .T. ) ;
#21906 = CARTESIAN_POINT ( 'NONE',  ( -87.50000000000000000, -8.499999999999989342, 1.000000000000000888 ) ) ;
#21907 = CARTESIAN_POINT ( 'NONE',  ( -5.696827471326999515, 112.0732520954904032, 5.780458086807509943 ) ) ;
#21908 = CARTESIAN_POINT ( 'NONE',  ( -60.00000000000000000, -2.024042244987997205E-14, -12.00000000000000000 ) ) ;
#21909 =( NAMED_UNIT ( * ) PLANE_ANGLE_UNIT ( ) SI_UNIT ( $, .RADIAN. ) );
#21910 = CARTESIAN_POINT ( 'NONE',  ( -63.35707362346617089, 5.598654528085804216, 7.705886871421366635 ) ) ;
#21911 = CIRCLE ( 'NONE', #30872, 0.9999999999999991118 ) ;
#21912 = EDGE_CURVE ( 'NONE', #36332, #27365, #9139, .T. ) ;
#21913 = MECHANICAL_DESIGN_GEOMETRIC_PRESENTATION_REPRESENTATION (  '', ( #43300 ), #42194 ) ;
#21914 = LINE ( 'NONE', #54246, #65085 ) ;
#21915 = ORIENTED_EDGE ( 'NONE', *, *, #22327, .T. ) ;
#21916 = DIRECTION ( 'NONE',  ( 0.000000000000000000, 0.000000000000000000, -1.000000000000000000 ) ) ;
#21917 = DIRECTION ( 'NONE',  ( 1.000000000000000000, 0.000000000000000000, 0.000000000000000000 ) ) ;
#21919 = DIRECTION ( 'NONE',  ( 0.000000000000000000, 0.000000000000000000, -1.000000000000000000 ) ) ;
#21918 =( LENGTH_UNIT ( ) NAMED_UNIT ( * ) SI_UNIT ( .MILLI., .METRE. ) );
#21920 = AXIS2_PLACEMENT_3D ( 'NONE', #49955, #12271, #7019 ) ;
#21921 = CARTESIAN_POINT ( 'NONE',  ( -105.3549999999999898, -4.716976649647093289, -6.492361379858945902 ) ) ;
#21922 = CARTESIAN_POINT ( 'NONE',  ( -9.058813317711338797, 128.3449999999999989, 2.943386871421373563 ) ) ;
#21923 = CARTESIAN_POINT ( 'NONE',  ( -120.4449999999999932, 0.000000000000000000, 8.024999999999991473 ) ) ;
#21924 = CARTESIAN_POINT ( 'NONE',  ( 21.02379604162863913, 110.4999999999999858, -9.500000000000000000 ) ) ;
#21925 = CARTESIAN_POINT ( 'NONE',  ( -8.921435019309294474E-16, -7.500000000000000888, 0.000000000000000000 ) ) ;
#21926 = EDGE_CURVE ( 'NONE', #26708, #6652, #30564, .T. ) ;
#21927 = CARTESIAN_POINT ( 'NONE',  ( -160.7929263765338135, -3.094860106618429807, 9.524999999999991473 ) ) ;
#21928 = CARTESIAN_POINT ( 'NONE',  ( -180.2949999999999591, -2.607480562269069768, 8.024999999999991473 ) ) ;
#21929 = ADVANCED_FACE ( 'NONE', ( #8458 ), #34815, .F. ) ;
#21930 = AXIS2_PLACEMENT_3D ( 'NONE', #7147, #50756, #18046 ) ;
#21931 = ADVANCED_FACE ( 'NONE', ( #61891 ), #48478, .T. ) ;
#21932 = FACE_OUTER_BOUND ( 'NONE', #22546, .T. ) ;
#21933 = MECHANICAL_DESIGN_GEOMETRIC_PRESENTATION_REPRESENTATION (  '', ( #38835 ), #65767 ) ;
#21934 = CARTESIAN_POINT ( 'NONE',  ( -40.70406133565713702, -11.89285714285713880, 3.265330863013266693 ) ) ;
#21935 = VERTEX_POINT ( 'NONE', #29894 ) ;
#21936 = DIRECTION ( 'NONE',  ( 0.000000000000000000, 0.000000000000000000, 1.000000000000000000 ) ) ;
#21937 = CARTESIAN_POINT ( 'NONE',  ( -15.98999599679679839, 146.4999999999999716, -9.500000000000000000 ) ) ;
#21938 = ORIENTED_EDGE ( 'NONE', *, *, #17680, .F. ) ;
#21939 = CARTESIAN_POINT ( 'NONE',  ( -80.24292637653380211, 5.598654528085804216, 7.705886871421366635 ) ) ;
#21940 = CONTEXT_DEPENDENT_SHAPE_REPRESENTATION ( #2862, #28369 ) ;
#21941 = MECHANICAL_DESIGN_GEOMETRIC_PRESENTATION_REPRESENTATION (  '', ( #39946 ), #29763 ) ;
#21942 = LINE ( 'NONE', #4706, #48734 ) ;
#21943 = SURFACE_STYLE_FILL_AREA ( #22978 ) ;
#21944 = EDGE_CURVE ( 'NONE', #9217, #27703, #54048, .T. ) ;
#21945 = PRESENTATION_LAYER_ASSIGNMENT (  '', '', ( #3936 ) ) ;
#21946 = FILL_AREA_STYLE_COLOUR ( '', #66315 ) ;
#21947 = PLANE ( 'NONE',  #55102 ) ;
#21948 = CARTESIAN_POINT ( 'NONE',  ( 0.000000000000000000, 109.9999999999999858, 0.000000000000000000 ) ) ;
#21949 = EDGE_CURVE ( 'NONE', #60632, #67825, #39952, .T. ) ;
#21950 = VERTEX_POINT ( 'NONE', #31251 ) ;
#21951 = CARTESIAN_POINT ( 'NONE',  ( -176.9050000000000011, 2.607480562269069324, -8.024999999999993250 ) ) ;
#21952 = ORIENTED_EDGE ( 'NONE', *, *, #69037, .F. ) ;
#21953 = DIRECTION ( 'NONE',  ( 0.000000000000000000, 0.000000000000000000, -1.000000000000000000 ) ) ;
#21954 = FACE_OUTER_BOUND ( 'NONE', #39920, .T. ) ;
#21955 = CARTESIAN_POINT ( 'NONE',  ( 48.74999999999999289, 24.74999999999998579, -3.750000000000000000 ) ) ;
#21956 = FACE_OUTER_BOUND ( 'NONE', #26755, .T. ) ;
#21957 = FACE_OUTER_BOUND ( 'NONE', #58544, .T. ) ;
#21958 = CARTESIAN_POINT ( 'NONE',  ( -6.826472737025120807, 143.1070736234661638, 4.959722759717906548 ) ) ;
#21959 = AXIS2_PLACEMENT_3D ( 'NONE', #51471, #51835, #47648 ) ;
#21960 = ORIENTED_EDGE ( 'NONE', *, *, #33208, .T. ) ;
#21961 = DIRECTION ( 'NONE',  ( 1.000000000000000000, 0.000000000000000000, -1.300977106640434891E-16 ) ) ;
#21962 = CARTESIAN_POINT ( 'NONE',  ( -90.95499999999999829, -7.632228543268599452, 2.479861379858951054 ) ) ;
#21963 = CARTESIAN_POINT ( 'NONE',  ( 21.00000000000001776, -3.148064030671221758, -29.68999999999999417 ) ) ;
#21964 = ORIENTED_EDGE ( 'NONE', *, *, #31608, .F. ) ;
#21965 = VECTOR ( 'NONE', #47768, 1000.000000000000114 ) ;
#21966 = CARTESIAN_POINT ( 'NONE',  ( -72.65707362346617515, 9.058813317711329915, 2.943386871421369566 ) ) ;
#21967 = CARTESIAN_POINT ( 'NONE',  ( -57.11974195712093660, -8.499999999999992895, 8.000000000000000000 ) ) ;
#21968 = PRESENTATION_STYLE_ASSIGNMENT (( #17053 ) ) ;
#21969 = PRESENTATION_LAYER_ASSIGNMENT (  '', '', ( #551 ) ) ;
#21970 = VERTEX_POINT ( 'NONE', #26665 ) ;
#21971 = CIRCLE ( 'NONE', #11808, 26.99999999999999645 ) ;
#21972 = SURFACE_STYLE_USAGE ( .BOTH. , #75 ) ;
#21973 = ADVANCED_FACE ( 'NONE', ( #15816 ), #3508, .T. ) ;
#21974 = CARTESIAN_POINT ( 'NONE',  ( -65.69499999999999318, -8.437984349512085203, 5.166775262442717831E-16 ) ) ;
#21975 = ORIENTED_EDGE ( 'NONE', *, *, #30713, .T. ) ;
#21976 = CARTESIAN_POINT ( 'NONE',  ( 44.99999999999977973, 149.9999999999999716, -9.500000000000000000 ) ) ;
#21977 =( NAMED_UNIT ( * ) PLANE_ANGLE_UNIT ( ) SI_UNIT ( $, .RADIAN. ) );
#21978 = CARTESIAN_POINT ( 'NONE',  ( -138.0570736234661808, 0.000000000000000000, 9.524999999999991473 ) ) ;
#21979 = ORIENTED_EDGE ( 'NONE', *, *, #9655, .F. ) ;
#21980 = SURFACE_STYLE_USAGE ( .BOTH. , #38183 ) ;
#21981 = ORIENTED_EDGE ( 'NONE', *, *, #61722, .T. ) ;
#21982 = CARTESIAN_POINT ( 'NONE',  ( 45.00000000000000000, 10.18984267075341066, -6.892226874380344093 ) ) ;
#21983 = VECTOR ( 'NONE', #21869, 1000.000000000000000 ) ;
#21984 = LINE ( 'NONE', #59228, #4429 ) ;
#21985 = CARTESIAN_POINT ( 'NONE',  ( -112.1049999999999756, -6.826472737025115478, 4.959722759717900331 ) ) ;
#21986 = EDGE_LOOP ( 'NONE', ( #33609, #37773, #5872 ) ) ;
#21987 = FACE_OUTER_BOUND ( 'NONE', #22506, .T. ) ;
#21988 = CARTESIAN_POINT ( 'NONE',  ( 31.91038605531459993, 42.48853604202995626, -45.29557250688775838 ) ) ;
#21989 = DIRECTION ( 'NONE',  ( -0.000000000000000000, -0.000000000000000000, -1.000000000000000000 ) ) ;
#21990 = DIRECTION ( 'NONE',  ( 0.000000000000000000, 1.000000000000000000, 0.000000000000000000 ) ) ;
#21991 = CARTESIAN_POINT ( 'NONE',  ( -159.0570736234661808, 0.000000000000000000, 9.524999999999991473 ) ) ;
#21992 = CARTESIAN_POINT ( 'NONE',  ( -9.058813317711338797, 134.3449999999999989, 2.943386871421373563 ) ) ;
#21993 = VECTOR ( 'NONE', #35186, 1000.000000000000000 ) ;
#21994 = CARTESIAN_POINT ( 'NONE',  ( -92.60707362346619220, -8.102448949553172852, 5.886773742842742685 ) ) ;
#21995 = AXIS2_PLACEMENT_3D ( 'NONE', #54264, #59184, #42736 ) ;
#21996 = CARTESIAN_POINT ( 'NONE',  ( -22.25000000000000711, 34.24999999999999289, 4.000000000000000000 ) ) ;
#21997 = ORIENTED_EDGE ( 'NONE', *, *, #66217, .F. ) ;
#21998 = DIRECTION ( 'NONE',  ( 0.000000000000000000, 0.000000000000000000, 1.000000000000000000 ) ) ;
#21999 = DIRECTION ( 'NONE',  ( -0.000000000000000000, -1.000000000000000000, -0.000000000000000000 ) ) ;
#22000 = SURFACE_STYLE_USAGE ( .BOTH. , #49104 ) ;
#22001 = CARTESIAN_POINT ( 'NONE',  ( -144.6549999999999727, -7.632228543268600340, -2.479861379858950166 ) ) ;
#22002 = CARTESIAN_POINT ( 'NONE',  ( -86.90707362346618936, -3.094860106618429807, 9.524999999999991473 ) ) ;
#22003 = ADVANCED_FACE ( 'NONE', ( #58033 ), #63294, .F. ) ;
#22004 = CARTESIAN_POINT ( 'NONE',  ( -146.2449999999999761, -4.716976649647093289, -6.492361379858945902 ) ) ;
#22005 = CARTESIAN_POINT ( 'NONE',  ( -136.4949999999999477, 6.826472737025113702, -4.959722759717902107 ) ) ;
#22006 = VERTEX_POINT ( 'NONE', #20737 ) ;
#22007 =( GEOMETRIC_REPRESENTATION_CONTEXT ( 3 ) GLOBAL_UNCERTAINTY_ASSIGNED_CONTEXT ( ( #9545 ) ) GLOBAL_UNIT_ASSIGNED_CONTEXT ( ( #47755, #27230, #10409 ) ) REPRESENTATION_CONTEXT ( 'NONE', 'WORKASPACE' ) );
#22008 = CYLINDRICAL_SURFACE ( 'NONE', #44709, 18.00000000000000355 ) ;
#22009 = EDGE_CURVE ( 'NONE', #22236, #38885, #32777, .T. ) ;
#22010 = UNCERTAINTY_MEASURE_WITH_UNIT (LENGTH_MEASURE( 1.000000000000000082E-05 ), #38946, 'distance_accuracy_value', 'NONE');
#22011 = CARTESIAN_POINT ( 'NONE',  ( -54.65499999999997982, -7.632228543268600340, -2.479861379858950166 ) ) ;
#22012 = PRESENTATION_STYLE_ASSIGNMENT (( #26232 ) ) ;
#22013 = CARTESIAN_POINT ( 'NONE',  ( -56.69499999999998607, -8.437984349512085203, 5.166775262442717831E-16 ) ) ;
#22014 = AXIS2_PLACEMENT_3D ( 'NONE', #50142, #55033, #19405 ) ;
#22015 = ADVANCED_FACE ( 'NONE', ( #41515 ), #15478, .T. ) ;
#22016 = CARTESIAN_POINT ( 'NONE',  ( -103.5570736234661808, -1.166476076187852838E-15, -9.524999999999991473 ) ) ;
#22017 =( NAMED_UNIT ( * ) PLANE_ANGLE_UNIT ( ) SI_UNIT ( $, .RADIAN. ) );
#22018 = CARTESIAN_POINT ( 'NONE',  ( -56.67268476622996332, -8.515503721524707359, -0.2436096942820924205 ) ) ;
#22019 = CARTESIAN_POINT ( 'NONE',  ( -109.3429263765338106, -9.058813317711329915, 2.943386871421371787 ) ) ;
#22020 = CARTESIAN_POINT ( 'NONE',  ( 5.000000000000040856, 115.6078173946806942, -15.00000000000002309 ) ) ;
#22021 = DIRECTION ( 'NONE',  ( -0.000000000000000000, 1.000000000000000000, -0.000000000000000000 ) ) ;
#22022 = CARTESIAN_POINT ( 'NONE',  ( -71.99999999999998579, 119.9999999999997868, -9.500000000000000000 ) ) ;
#22023 = EDGE_CURVE ( 'NONE', #22006, #16526, #10298, .T. ) ;
#22024 = CIRCLE ( 'NONE', #38932, 0.5000000000000004441 ) ;
#22025 = CYLINDRICAL_SURFACE ( 'NONE', #59679, 0.2500000000000002220 ) ;
#22026 = ORIENTED_EDGE ( 'NONE', *, *, #40286, .F. ) ;
#22027 = FACE_OUTER_BOUND ( 'NONE', #4450, .T. ) ;
#22028 = CONICAL_SURFACE ( 'NONE', #35493, 6.999999999999997335, 0.7853981633974500554 ) ;
#22029 = ORIENTED_EDGE ( 'NONE', *, *, #31120, .F. ) ;
#22030 = DIRECTION ( 'NONE',  ( -0.000000000000000000, 0.000000000000000000, 1.000000000000000000 ) ) ;
#22032 = CARTESIAN_POINT ( 'NONE',  ( -7.632228543268608334, 115.9570736234661581, 2.479861379858952830 ) ) ;
#22031 = AXIS2_PLACEMENT_3D ( 'NONE', #27711, #22468, #65013 ) ;
#22033 =( NAMED_UNIT ( * ) PLANE_ANGLE_UNIT ( ) SI_UNIT ( $, .RADIAN. ) );
#22034 = DIRECTION ( 'NONE',  ( 0.000000000000000000, -0.9396926207859082059, 0.3420201433256693790 ) ) ;
#22035 = EDGE_LOOP ( 'NONE', ( #49864, #11746, #65479, #507 ) ) ;
#22036 = ORIENTED_EDGE ( 'NONE', *, *, #36740, .T. ) ;
#22037 = CARTESIAN_POINT ( 'NONE',  ( -4.358330484967981810, -1.733974831985838794, -6.451150163859153963 ) ) ;
#22038 = DIRECTION ( 'NONE',  ( 0.000000000000000000, 1.000000000000000000, 0.000000000000000000 ) ) ;
#22039 = CARTESIAN_POINT ( 'NONE',  ( 3.499999999999998668, 36.99999999999999289, 3.750000000000000000 ) ) ;
#22040 = ORIENTED_EDGE ( 'NONE', *, *, #186, .T. ) ;
#22041 = CARTESIAN_POINT ( 'NONE',  ( -120.0570736234661808, 0.000000000000000000, 9.524999999999991473 ) ) ;
#22042 = CARTESIAN_POINT ( 'NONE',  ( 4.716976649647096842, 133.7429263765338021, 6.492361379858953896 ) ) ;
#22043 = EDGE_CURVE ( 'NONE', #19239, #50261, #12515, .T. ) ;
#22044 = CARTESIAN_POINT ( 'NONE',  ( -95.24499999999997613, -4.716976649647093289, -6.492361379858945902 ) ) ;
#22045 = ORIENTED_EDGE ( 'NONE', *, *, #65025, .T. ) ;
#22046 = VECTOR ( 'NONE', #3721, 1000.000000000000000 ) ;
#22047 = CARTESIAN_POINT ( 'NONE',  ( -71.75000000000000000, -4.000000000000000000, 20.00000000000000000 ) ) ;
#22048 = DIRECTION ( 'NONE',  ( -1.000000000000000000, -0.000000000000000000, -0.000000000000000000 ) ) ;
#22049 = PRESENTATION_STYLE_ASSIGNMENT (( #25918 ) ) ;
#22050 = EDGE_LOOP ( 'NONE', ( #67729, #45935, #40477, #7059 ) ) ;
#22051 = CARTESIAN_POINT ( 'NONE',  ( 4.716976649647099507, 161.6429263765338362, -6.492361379858953008 ) ) ;
#22052 = VECTOR ( 'NONE', #47819, 1000.000000000000000 ) ;
#22053 = CARTESIAN_POINT ( 'NONE',  ( 6.239160159721276244, -3.193457606803200566, 4.616329562535936848E-16 ) ) ;
#22054 = ORIENTED_EDGE ( 'NONE', *, *, #32010, .T. ) ;
#22055 = COLOUR_RGB ( '', 0.66274510, 0.83137255, 0.94901961) ;
#22056 = DIRECTION ( 'NONE',  ( -1.224646799147353207E-16, 1.000000000000000000, 0.000000000000000000 ) ) ;
#22057 = VERTEX_POINT ( 'NONE', #60411 ) ;
#22058 = DIRECTION ( 'NONE',  ( 0.000000000000000000, 1.000000000000000000, -0.000000000000000000 ) ) ;
#22059 =( GEOMETRIC_REPRESENTATION_CONTEXT ( 3 ) GLOBAL_UNCERTAINTY_ASSIGNED_CONTEXT ( ( #25703 ) ) GLOBAL_UNIT_ASSIGNED_CONTEXT ( ( #23943, #56293, #56658 ) ) REPRESENTATION_CONTEXT ( 'NONE', 'WORKASPACE' ) );
#22060 = CARTESIAN_POINT ( 'NONE',  ( -71.75000000000000000, -0.9999999999999995559, 20.00000000000000000 ) ) ;
#22061 = CARTESIAN_POINT ( 'NONE',  ( 44.91886116991580735, 9.999999999999980460, 3.201362207699192997 ) ) ;
#22062 =( LENGTH_UNIT ( ) NAMED_UNIT ( * ) SI_UNIT ( .MILLI., .METRE. ) );
#22063 = DIRECTION ( 'NONE',  ( -1.000000000000000000, 0.000000000000000000, 0.000000000000000000 ) ) ;
#22064 =( BOUNDED_CURVE ( )  B_SPLINE_CURVE ( 2, ( #27669, #880, #49866, #22420, #65334, #66018, #32278, #6564, #53729, #26972, #17178 ),
 .UNSPECIFIED., .F., .F. ) 
 B_SPLINE_CURVE_WITH_KNOTS ( ( 3, 2, 2, 2, 2, 3 ),
 ( 0.6847826086956522174, 0.6869565217391304657, 0.6891304347826087140, 0.6913043478260869623, 0.6934782608695652106, 0.6956521739130434590 ),
 .UNSPECIFIED. ) 
 CURVE ( )  GEOMETRIC_REPRESENTATION_ITEM ( )  RATIONAL_B_SPLINE_CURVE ( ( 1.000000000000000000, 0.9510565162951535312, 1.000000000000000000, 0.9510565162951535312, 1.000000000000000000, 0.9510565162951535312, 1.000000000000000000, 0.9510565162951535312, 1.000000000000000000, 0.9510565162951535312, 1.000000000000000000 ) ) 
 REPRESENTATION_ITEM ( '' )  );
#22065 = DIRECTION ( 'NONE',  ( -0.000000000000000000, -0.000000000000000000, 1.000000000000000000 ) ) ;
#22066 = CARTESIAN_POINT ( 'NONE',  ( -68.99292637653380211, 8.102448949553172852, -5.886773742842744461 ) ) ;
#22067 = CARTESIAN_POINT ( 'NONE',  ( -4.325530127497521526, 153.1662597749872816, -6.961252418570021305 ) ) ;
#22068 = VERTEX_POINT ( 'NONE', #6592 ) ;
#22069 = FILL_AREA_STYLE ('',( #16815 ) ) ;
#22070 = CARTESIAN_POINT ( 'NONE',  ( -15.75000000000000000, -4.000000000000000000, 18.00000000000000000 ) ) ;
#22071 =( LENGTH_UNIT ( ) NAMED_UNIT ( * ) SI_UNIT ( .MILLI., .METRE. ) );
#22072 = ORIENTED_EDGE ( 'NONE', *, *, #68305, .F. ) ;
#22073 = SURFACE_STYLE_USAGE ( .BOTH. , #198 ) ;
#22074 = CARTESIAN_POINT ( 'NONE',  ( -170.3049999999999784, 8.437984349512085203, -1.550032578732815448E-15 ) ) ;
#22075 = FACE_OUTER_BOUND ( 'NONE', #28007, .T. ) ;
#22076 = CYLINDRICAL_SURFACE ( 'NONE', #33604, 8.025000000000000355 ) ;
#22077 = ADVANCED_FACE ( 'NONE', ( #27700 ), #46274, .T. ) ;
#22078 = CARTESIAN_POINT ( 'NONE',  ( -170.8449999999999989, -7.632228543268599452, 2.479861379858951054 ) ) ;
#22079 = CARTESIAN_POINT ( 'NONE',  ( -167.6949999999999648, -8.437984349512086979, 5.166775262442717831E-16 ) ) ;
#22080 = ORIENTED_EDGE ( 'NONE', *, *, #14362, .T. ) ;
#22081 =( LENGTH_UNIT ( ) NAMED_UNIT ( * ) SI_UNIT ( .MILLI., .METRE. ) );
#22082 = CYLINDRICAL_SURFACE ( 'NONE', #13375, 0.2500000000000002220 ) ;
#22083 = CARTESIAN_POINT ( 'NONE',  ( -2.607480562269240298, 150.0929263765338817, -8.024999999999879563 ) ) ;
#22084 = CARTESIAN_POINT ( 'NONE',  ( -78.95499999999998408, -7.632228543268599452, 2.479861379858951054 ) ) ;
#22085 = CARTESIAN_POINT ( 'NONE',  ( 1.092332116235429474E-16, 42.58578643762690774, -35.91421356237308515 ) ) ;
#22086 = CARTESIAN_POINT ( 'NONE',  ( 24.68182447752072406, 26.35395679099813293, 27.48625690893775797 ) ) ;
#22087 = CYLINDRICAL_SURFACE ( 'NONE', #57351, 9.524999999999991473 ) ;
#22088 = EDGE_CURVE ( 'NONE', #47153, #43960, #49201, .T. ) ;
#22089 = CARTESIAN_POINT ( 'NONE',  ( -83.84499999999998465, -7.632228543268599452, 2.479861379858951054 ) ) ;
#22090 = CARTESIAN_POINT ( 'NONE',  ( 3.094860106618431583, 139.2050000000000125, 9.525000000000000355 ) ) ;
#22091 = DIRECTION ( 'NONE',  ( 0.000000000000000000, 0.000000000000000000, 1.000000000000000000 ) ) ;
#22092 = ADVANCED_FACE ( 'NONE', ( #22453 ), #28035, .T. ) ;
#22093 = CARTESIAN_POINT ( 'NONE',  ( -176.8429263765338249, 9.058813317711329915, -2.943386871421373119 ) ) ;
#22094 = UNCERTAINTY_MEASURE_WITH_UNIT (LENGTH_MEASURE( 1.000000000000000082E-05 ), #13215, 'distance_accuracy_value', 'NONE');
#22095 =( NAMED_UNIT ( * ) SI_UNIT ( $, .STERADIAN. ) SOLID_ANGLE_UNIT ( ) );
#22096 = ORIENTED_EDGE ( 'NONE', *, *, #47973, .F. ) ;
#22097 = ADVANCED_FACE ( 'NONE', ( #21768 ), #34984, .T. ) ;
#22098 = CARTESIAN_POINT ( 'NONE',  ( 7.766025168014159874, -1.733974831985843013, -0.5488498361408489234 ) ) ;
#22099 = CARTESIAN_POINT ( 'NONE',  ( 24.21231517720798010, 117.4999999999999716, 7.500000000000000000 ) ) ;
#22100 = COLOUR_RGB ( '', 0.08235294, 0.09019608, 0.10196078) ;
#22101 = EDGE_CURVE ( 'NONE', #2048, #52429, #44023, .T. ) ;
#22102 = DIRECTION ( 'NONE',  ( 1.000000000000000000, 0.000000000000000000, 0.000000000000000000 ) ) ;
#22103 = VECTOR ( 'NONE', #5336, 1000.000000000000000 ) ;
#22104 =( LENGTH_UNIT ( ) NAMED_UNIT ( * ) SI_UNIT ( .MILLI., .METRE. ) );
#22105 = COLOUR_RGB ( '', 0.72549020, 0.75294118, 0.79215686) ;
#22106 =( LENGTH_UNIT ( ) NAMED_UNIT ( * ) SI_UNIT ( .MILLI., .METRE. ) );
#22107 = EDGE_LOOP ( 'NONE', ( #50949, #1909, #46382 ) ) ;
#22108 = ORIENTED_EDGE ( 'NONE', *, *, #50065, .F. ) ;
#22109 = DIRECTION ( 'NONE',  ( 1.000000000000000000, 0.000000000000000000, 0.000000000000000000 ) ) ;
#22110 = FILL_AREA_STYLE ('',( #43946 ) ) ;
#22111 =( NAMED_UNIT ( * ) PLANE_ANGLE_UNIT ( ) SI_UNIT ( $, .RADIAN. ) );
#22112 = CARTESIAN_POINT ( 'NONE',  ( -23.71231517720798010, 117.9999999999999716, 7.000000000000000000 ) ) ;
#22113 = DIRECTION ( 'NONE',  ( 0.000000000000000000, -1.000000000000000000, -0.000000000000000000 ) ) ;
#22114 = ORIENTED_EDGE ( 'NONE', *, *, #47785, .T. ) ;
#22115 = CARTESIAN_POINT ( 'NONE',  ( -112.5549999999999926, 0.000000000000000000, 8.024999999999991473 ) ) ;
#22116 = ORIENTED_EDGE ( 'NONE', *, *, #22716, .T. ) ;
#22117 = VECTOR ( 'NONE', #44757, 1000.000000000000000 ) ;
#22118 = CARTESIAN_POINT ( 'NONE',  ( 20.44164625062140317, 115.3859073845563756, -10.00000000000000000 ) ) ;
#22119 = ORIENTED_EDGE ( 'NONE', *, *, #66890, .F. ) ;
#22120 = B_SPLINE_CURVE_WITH_KNOTS ( 'NONE', 3,
 ( #64139, #1083, #22977, #55311, #60572, #65880, #59900, #7134, #12389, #38507, #33849, #54273 ),
 .UNSPECIFIED., .F., .F.,
 ( 4, 2, 2, 2, 2, 4 ),
 ( 0.000000000000000000, 0.0001173275976309089770, 0.0002346551952618179540, 0.0004693103905236373718, 0.0009386207810472817908, 0.001877241562094575291 ),
 .UNSPECIFIED. ) ;
#22121 = CARTESIAN_POINT ( 'NONE',  ( -56.09292637653378222, 3.094860106618433360, 9.524999999999991473 ) ) ;
#22122 = DIRECTION ( 'NONE',  ( 0.000000000000000000, 0.000000000000000000, -1.000000000000000000 ) ) ;
#22123 = ORIENTED_EDGE ( 'NONE', *, *, #28580, .F. ) ;
#22124 = LINE ( 'NONE', #28764, #62446 ) ;
#22125 = CARTESIAN_POINT ( 'NONE',  ( -3.094860106618434248, 155.7950000000000159, 9.525000000000000355 ) ) ;
#22126 = SURFACE_SIDE_STYLE ('',( #28765 ) ) ;
#22127 = ORIENTED_EDGE ( 'NONE', *, *, #45632, .T. ) ;
#22128 = VERTEX_POINT ( 'NONE', #45679 ) ;
#22129 = CARTESIAN_POINT ( 'NONE',  ( -12.72792206135785520, 115.4999999999999574, 10.50000000000000000 ) ) ;
#22130 = SURFACE_SIDE_STYLE ('',( #65020 ) ) ;
#22131 = CARTESIAN_POINT ( 'NONE',  ( 4.358330484967978258, 1.733974831985841458, 6.451150163859151299 ) ) ;
#22132 = ORIENTED_EDGE ( 'NONE', *, *, #51736, .T. ) ;
#22133 = CARTESIAN_POINT ( 'NONE',  ( 8.437984349512095861, 140.1929263765337907, 1.550032578732817026E-15 ) ) ;
#22134 = LINE ( 'NONE', #49220, #15469 ) ;
#22135 = FACE_OUTER_BOUND ( 'NONE', #37888, .T. ) ;
#22136 = CARTESIAN_POINT ( 'NONE',  ( -104.8429263765338106, 9.058813317711329915, -2.943386871421373119 ) ) ;
#22137 =( NAMED_UNIT ( * ) PLANE_ANGLE_UNIT ( ) SI_UNIT ( $, .RADIAN. ) );
#22138 = ORIENTED_EDGE ( 'NONE', *, *, #14038, .T. ) ;
#22139 = ORIENTED_EDGE ( 'NONE', *, *, #58792, .T. ) ;
#22140 = CARTESIAN_POINT ( 'NONE',  ( -48.59292637653380353, -3.094860106618431139, -9.524999999999991473 ) ) ;
#22141 = FACE_OUTER_BOUND ( 'NONE', #12819, .T. ) ;
#22142 = FACE_OUTER_BOUND ( 'NONE', #53851, .T. ) ;
#22143 = CARTESIAN_POINT ( 'NONE',  ( -145.7050000000000125, 2.607480562269073321, 8.024999999999991473 ) ) ;
#22144 = CARTESIAN_POINT ( 'NONE',  ( -5.603568002170373319, -1.515110734050471919, -8.294335516573692502 ) ) ;
#22145 = SURFACE_STYLE_FILL_AREA ( #27397 ) ;
#22146 = UNCERTAINTY_MEASURE_WITH_UNIT (LENGTH_MEASURE( 1.000000000000000082E-05 ), #24735, 'distance_accuracy_value', 'NONE');
#22147 = VERTEX_POINT ( 'NONE', #19230 ) ;
#22148 = FACE_OUTER_BOUND ( 'NONE', #56676, .T. ) ;
#22149 = CYLINDRICAL_SURFACE ( 'NONE', #38427, 23.00000000000000000 ) ;
#22150 = CARTESIAN_POINT ( 'NONE',  ( 40.99999999999998579, 107.7459666690181450, 3.075798416731059692 ) ) ;
#22151 = ORIENTED_EDGE ( 'NONE', *, *, #47294, .F. ) ;
#22152 = ORIENTED_EDGE ( 'NONE', *, *, #13301, .F. ) ;
#22153 = FACE_OUTER_BOUND ( 'NONE', #9463, .T. ) ;
#22154 = AXIS2_PLACEMENT_3D ( 'NONE', #51062, #33902, #57370 ) ;
#22155 = FILL_AREA_STYLE ('',( #633 ) ) ;
#22156 = CARTESIAN_POINT ( 'NONE',  ( -53.15499999999997982, 7.632228543268600340, 2.479861379858949277 ) ) ;
#22157 = ORIENTED_EDGE ( 'NONE', *, *, #51926, .T. ) ;
#22158 = DIRECTION ( 'NONE',  ( -0.000000000000000000, -0.000000000000000000, -1.000000000000000000 ) ) ;
#22159 =( LENGTH_UNIT ( ) NAMED_UNIT ( * ) SI_UNIT ( .MILLI., .METRE. ) );
#22160 = CARTESIAN_POINT ( 'NONE',  ( 68.50000000000000000, 1.797044900979284448E-15, -9.999999999999998224 ) ) ;
#22161 = EDGE_CURVE ( 'NONE', #11645, #30516, #28749, .T. ) ;
#22162 = CARTESIAN_POINT ( 'NONE',  ( -74.99999999999998579, 50.00000000000000000, -11.50000000000000000 ) ) ;
#22163 = DIRECTION ( 'NONE',  ( 0.000000000000000000, 0.000000000000000000, 1.000000000000000000 ) ) ;
#22165 = ADVANCED_FACE ( 'NONE', ( #18882 ), #23833, .T. ) ;
#22164 = ORIENTED_EDGE ( 'NONE', *, *, #157, .F. ) ;
#22166 = SHAPE_REPRESENTATION ( '8. Upper Jaw Support', ( #42840 ), #64177 ) ;
#22167 = EDGE_CURVE ( 'NONE', #320, #21193, #63524, .T. ) ;
#22168 = CARTESIAN_POINT ( 'NONE',  ( -15.98999599679679839, 146.4999999999999716, -10.00000000000000000 ) ) ;
#22169 = DIRECTION ( 'NONE',  ( 0.000000000000000000, 0.000000000000000000, -1.000000000000000000 ) ) ;
#22170 = DIRECTION ( 'NONE',  ( 0.000000000000000000, 0.000000000000000000, -1.000000000000000000 ) ) ;
#22171 = DIRECTION ( 'NONE',  ( 1.000000000000000000, 0.000000000000000000, -0.000000000000000000 ) ) ;
#22172 = EDGE_CURVE ( 'NONE', #9835, #15666, #14827, .T. ) ;
#22173 = VECTOR ( 'NONE', #13285, 1000.000000000000000 ) ;
#22174 = EDGE_CURVE ( 'NONE', #66803, #31185, #56529, .T. ) ;
#22175 = CARTESIAN_POINT ( 'NONE',  ( -106.1949999999999932, 8.437984349512086979, -1.550032578732815448E-15 ) ) ;
#22176 = CARTESIAN_POINT ( 'NONE',  ( -8.102448949553181734, 111.6049999999999613, 5.886773742842747126 ) ) ;
#22177 = CARTESIAN_POINT ( 'NONE',  ( -90.14499999999999602, -4.716976649647092401, 6.492361379858946790 ) ) ;
#22178 = ADVANCED_FACE ( 'NONE', ( #23476 ), #18212, .T. ) ;
#22179 = CARTESIAN_POINT ( 'NONE',  ( -13.75000000000000355, 28.24999999999998934, -4.000000000000000000 ) ) ;
#22180 = CARTESIAN_POINT ( 'NONE',  ( 21.50000000000000711, 21.74999999999998224, -3.750000000000000000 ) ) ;
#22181 = DIRECTION ( 'NONE',  ( -0.000000000000000000, -0.000000000000000000, 1.000000000000000000 ) ) ;
#22182 = UNCERTAINTY_MEASURE_WITH_UNIT (LENGTH_MEASURE( 1.000000000000000082E-05 ), #62178, 'distance_accuracy_value', 'NONE');
#22183 = SURFACE_STYLE_USAGE ( .BOTH. , #69340 ) ;
#22184 = ORIENTED_EDGE ( 'NONE', *, *, #28329, .F. ) ;
#22185 = EDGE_CURVE ( 'NONE', #43827, #28053, #2438, .T. ) ;
#22186 = CARTESIAN_POINT ( 'NONE',  ( -127.6429263765337936, -5.598654528085801552, 7.705886871421367523 ) ) ;
#22187 = CARTESIAN_POINT ( 'NONE',  ( -145.9449999999999932, -9.827790563157499189E-16, -8.024999999999991473 ) ) ;
#22188 = SURFACE_SIDE_STYLE ('',( #21852 ) ) ;
#22189 = LINE ( 'NONE', #43687, #3538 ) ;
#22190 = ORIENTED_EDGE ( 'NONE', *, *, #47280, .F. ) ;
#22191 = ORIENTED_EDGE ( 'NONE', *, *, #44133, .T. ) ;
#22192 = LINE ( 'NONE', #38760, #35952 ) ;
#22193 =( LENGTH_UNIT ( ) NAMED_UNIT ( * ) SI_UNIT ( .MILLI., .METRE. ) );
#22194 = CARTESIAN_POINT ( 'NONE',  ( 68.99999999999998579, 0.000000000000000000, 3.000000000000000000 ) ) ;
#22195 = CARTESIAN_POINT ( 'NONE',  ( -130.2570736234661695, 5.598654528085800663, -7.705886871421367523 ) ) ;
#22196 = COLOUR_RGB ( '', 0.72549020, 0.75294118, 0.79215686) ;
#22197 = CARTESIAN_POINT ( 'NONE',  ( -117.2929263765346519, 3.094860106604310879, -9.525000000010253487 ) ) ;
#22198 = MECHANICAL_DESIGN_GEOMETRIC_PRESENTATION_REPRESENTATION (  '', ( #10945 ), #43589 ) ;
#22199 = CARTESIAN_POINT ( 'NONE',  ( 0.000000000000000000, 2.500000000000000000, 0.000000000000000000 ) ) ;
#22200 = ORIENTED_EDGE ( 'NONE', *, *, #25977, .F. ) ;
#22201 = CARTESIAN_POINT ( 'NONE',  ( -138.5049999999999955, -6.826472737025113702, -4.959722759717900331 ) ) ;
#22202 = VERTEX_POINT ( 'NONE', #18571 ) ;
#22203 =( GEOMETRIC_REPRESENTATION_CONTEXT ( 3 ) GLOBAL_UNCERTAINTY_ASSIGNED_CONTEXT ( ( #45951 ) ) GLOBAL_UNIT_ASSIGNED_CONTEXT ( ( #61472, #44679, #66789 ) ) REPRESENTATION_CONTEXT ( 'NONE', 'WORKASPACE' ) );
#22204 = EDGE_LOOP ( 'NONE', ( #31286, #22462, #53385, #45367 ) ) ;
#22205 = CARTESIAN_POINT ( 'NONE',  ( -0.9728900412908211282, 153.0000000000000000, -7.965808808122195828 ) ) ;
#22206 = DIRECTION ( 'NONE',  ( 1.000000000000000000, 0.000000000000000000, 0.000000000000000000 ) ) ;
#22207 = ORIENTED_EDGE ( 'NONE', *, *, #26448, .F. ) ;
#22208 = PLANE ( 'NONE',  #64096 ) ;
#22209 = DIRECTION ( 'NONE',  ( 0.000000000000000000, 1.000000000000000000, 0.000000000000000000 ) ) ;
#22210 = CARTESIAN_POINT ( 'NONE',  ( -9.058813317711338797, 128.3449999999999989, 2.943386871421373563 ) ) ;
#22211 =( LENGTH_UNIT ( ) NAMED_UNIT ( * ) SI_UNIT ( .MILLI., .METRE. ) );
#22212 = ADVANCED_FACE ( 'NONE', ( #40053 ), #35449, .T. ) ;
#22213 = ORIENTED_EDGE ( 'NONE', *, *, #33745, .F. ) ;
#22214 = CARTESIAN_POINT ( 'NONE',  ( -95.30707362346615241, -10.01517768586948698, 6.132527647946031529E-16 ) ) ;
#22215 = CARTESIAN_POINT ( 'NONE',  ( -9.058813317711338797, 132.4549999999999841, 2.943386871421373563 ) ) ;
#22216 = CARTESIAN_POINT ( 'NONE',  ( -54.05499999999999261, -9.827790563157499189E-16, -8.024999999999991473 ) ) ;
#22217 = CARTESIAN_POINT ( 'NONE',  ( -120.8949999999999960, 6.826472737025116366, 4.959722759717898555 ) ) ;
#22218 = DIRECTION ( 'NONE',  ( 0.000000000000000000, 0.000000000000000000, 1.000000000000000000 ) ) ;
#22219 = ORIENTED_EDGE ( 'NONE', *, *, #9946, .T. ) ;
#22220 = CARTESIAN_POINT ( 'NONE',  ( -5.598654528085806881, 155.8549999999999898, -7.705886871421374629 ) ) ;
#22221 = DIRECTION ( 'NONE',  ( 0.000000000000000000, 0.000000000000000000, 1.000000000000000000 ) ) ;
#22222 = UNCERTAINTY_MEASURE_WITH_UNIT (LENGTH_MEASURE( 1.000000000000000082E-05 ), #65194, 'distance_accuracy_value', 'NONE');
#22223 = COLOUR_RGB ( '', 0.72549020, 0.75294118, 0.79215686) ;
#22224 = CARTESIAN_POINT ( 'NONE',  ( -43.75000000000000000, 0.000000000000000000, -3.500000000000002220 ) ) ;
#22225 = DIRECTION ( 'NONE',  ( 1.000000000000000000, 0.000000000000000000, 0.000000000000000000 ) ) ;
#22226 =( NAMED_UNIT ( * ) SI_UNIT ( $, .STERADIAN. ) SOLID_ANGLE_UNIT ( ) );
#22227 = ORIENTED_EDGE ( 'NONE', *, *, #66552, .T. ) ;
#22228 = CARTESIAN_POINT ( 'NONE',  ( -170.0049999999999955, 6.826472737025116366, 4.959722759717898555 ) ) ;
#22229 = ORIENTED_EDGE ( 'NONE', *, *, #67935, .T. ) ;
#22230 = CARTESIAN_POINT ( 'NONE',  ( -87.65707362346617515, 9.058813317711329915, 2.943386871421369566 ) ) ;
#22231 = UNCERTAINTY_MEASURE_WITH_UNIT (LENGTH_MEASURE( 1.000000000000000082E-05 ), #10979, 'distance_accuracy_value', 'NONE');
#22232 = CARTESIAN_POINT ( 'NONE',  ( -52.94292637653380496, 0.000000000000000000, 9.524999999999991473 ) ) ;
#22233 = LINE ( 'NONE', #22940, #19496 ) ;
#22234 = FILL_AREA_STYLE ('',( #49009 ) ) ;
#22235 =( NAMED_UNIT ( * ) SI_UNIT ( $, .STERADIAN. ) SOLID_ANGLE_UNIT ( ) );
#22236 = VERTEX_POINT ( 'NONE', #61444 ) ;
#22237 = CARTESIAN_POINT ( 'NONE',  ( -45.89905495956738690, 9.405628579031734660, -3.000000000000000444 ) ) ;
#22238 = CARTESIAN_POINT ( 'NONE',  ( 57.00000000000000000, 0.9999999999999991118, 60.00402776293827145 ) ) ;
#22239 = CARTESIAN_POINT ( 'NONE',  ( -82.70499999999999829, 2.607480562269073321, 8.024999999999991473 ) ) ;
#22240 = VERTEX_POINT ( 'NONE', #2681 ) ;
#22241 = EDGE_CURVE ( 'NONE', #20689, #52764, #25903, .T. ) ;
#22242 = CARTESIAN_POINT ( 'NONE',  ( 23.21231517720797655, 117.4999999999999716, -7.000000000000000000 ) ) ;
#22243 = FILL_AREA_STYLE_COLOUR ( '', #63173 ) ;
#22244 = DIRECTION ( 'NONE',  ( -0.000000000000000000, -0.000000000000000000, 1.000000000000000000 ) ) ;
#22245 = CARTESIAN_POINT ( 'NONE',  ( -61.55707362346617373, -1.166476076187852838E-15, -9.524999999999991473 ) ) ;
#22246 = ADVANCED_FACE ( 'NONE', ( #58271 ), #4697, .T. ) ;
#22247 = VECTOR ( 'NONE', #8850, 1000.000000000000000 ) ;
#22248 = CARTESIAN_POINT ( 'NONE',  ( -81.44292637653380496, -1.166476076187852838E-15, -9.524999999999991473 ) ) ;
#22249 = ORIENTED_EDGE ( 'NONE', *, *, #39482, .T. ) ;
#22250 = SURFACE_STYLE_USAGE ( .BOTH. , #7792 ) ;
#22251 = AXIS2_PLACEMENT_3D ( 'NONE', #56470, #29380, #19873 ) ;
#22252 = PRESENTATION_STYLE_ASSIGNMENT (( #718 ) ) ;
#22253 = AXIS2_PLACEMENT_3D ( 'NONE', #30431, #62112, #40340 ) ;
#22254 = CARTESIAN_POINT ( 'NONE',  ( -100.2549999999999812, -4.716976649647092401, 6.492361379858946790 ) ) ;
#22255 = CARTESIAN_POINT ( 'NONE',  ( -8.102448949553181734, 131.4950000000000045, 5.886773742842747126 ) ) ;
#22256 = CARTESIAN_POINT ( 'NONE',  ( -119.5449999999999875, -7.632228543268600340, -2.479861379858950166 ) ) ;
#22257 = ADVANCED_FACE ( 'NONE', ( #37209 ), #64232, .T. ) ;
#22258 = AXIS2_PLACEMENT_3D ( 'NONE', #46358, #46723, #45992 ) ;
#22260 = CARTESIAN_POINT ( 'NONE',  ( 29.00000000000002842, 42.00000000000000000, 89.00000000000000000 ) ) ;
#22259 =( NAMED_UNIT ( * ) SI_UNIT ( $, .STERADIAN. ) SOLID_ANGLE_UNIT ( ) );
#22261 = EDGE_CURVE ( 'NONE', #13670, #31668, #33919, .T. ) ;
#22262 = CARTESIAN_POINT ( 'NONE',  ( -150.1429263765338078, 5.598654528085800663, -7.705886871421367523 ) ) ;
#22263 = CARTESIAN_POINT ( 'NONE',  ( -172.0450000000000159, 7.632228543268600340, 2.479861379858949277 ) ) ;
#22264 = MECHANICAL_DESIGN_GEOMETRIC_PRESENTATION_REPRESENTATION (  '', ( #31230 ), #16671 ) ;
#22265 = CARTESIAN_POINT ( 'NONE',  ( -7.632228543268607446, 148.6570736234661751, -2.479861379858953718 ) ) ;
#22266 = CARTESIAN_POINT ( 'NONE',  ( 57.00000000000000000, 0.000000000000000000, 55.00402776293825724 ) ) ;
#22267 = ORIENTED_EDGE ( 'NONE', *, *, #25332, .T. ) ;
#22268 = PLANE ( 'NONE',  #53032 ) ;
#22269 = ORIENTED_EDGE ( 'NONE', *, *, #49273, .F. ) ;
#22270 = CARTESIAN_POINT ( 'NONE',  ( -64.79292637653381348, -3.094860106618429807, 9.524999999999991473 ) ) ;
#22271 = CARTESIAN_POINT ( 'NONE',  ( 16.00000000000001776, -3.148064030671221758, 29.68999999999999417 ) ) ;
#22272 =( NAMED_UNIT ( * ) SI_UNIT ( $, .STERADIAN. ) SOLID_ANGLE_UNIT ( ) );
#22273 = CARTESIAN_POINT ( 'NONE',  ( 4.716976649647099507, 147.7570736234661695, -6.492361379858953008 ) ) ;
#22274 = DIRECTION ( 'NONE',  ( -0.000000000000000000, -0.000000000000000000, -1.000000000000000000 ) ) ;
#22275 = CARTESIAN_POINT ( 'NONE',  ( -71.18918918918917882, 14.09971791521133255, 7.500000000000000000 ) ) ;
#22276 = ORIENTED_EDGE ( 'NONE', *, *, #13911, .F. ) ;
#22277 = CARTESIAN_POINT ( 'NONE',  ( -171.5049999999999670, -6.826472737025113702, -4.959722759717900331 ) ) ;
#22278 = VERTEX_POINT ( 'NONE', #69513 ) ;
#22279 = CARTESIAN_POINT ( 'NONE',  ( -24.00000000000000355, 37.00000000000000000, -3.750000000000000000 ) ) ;
#22280 = PRESENTATION_STYLE_ASSIGNMENT (( #21228 ) ) ;
#22281 = CARTESIAN_POINT ( 'NONE',  ( -195.0000000000000000, 0.000000000000000000, 0.000000000000000000 ) ) ;
#22282 = DIRECTION ( 'NONE',  ( 0.000000000000000000, 1.000000000000000000, 0.000000000000000000 ) ) ;
#22283 = VECTOR ( 'NONE', #54552, 1000.000000000000000 ) ;
#22284 = CARTESIAN_POINT ( 'NONE',  ( -44.99999999999998579, 119.9999999999999716, -9.500000000000000000 ) ) ;
#22285 = CARTESIAN_POINT ( 'NONE',  ( -6.826472737025120807, 148.5070736234661126, -4.959722759717907437 ) ) ;
#22286 = MECHANICAL_DESIGN_GEOMETRIC_PRESENTATION_REPRESENTATION (  '', ( #859 ), #11080 ) ;
#22287 = EDGE_CURVE ( 'NONE', #44244, #16387, #56360, .T. ) ;
#22288 = ORIENTED_EDGE ( 'NONE', *, *, #41979, .F. ) ;
#22289 = CARTESIAN_POINT ( 'NONE',  ( -81.35499999999998977, -4.716976649647093289, -6.492361379858945902 ) ) ;
#22290 = UNCERTAINTY_MEASURE_WITH_UNIT (LENGTH_MEASURE( 1.000000000000000082E-05 ), #43950, 'distance_accuracy_value', 'NONE');
#22291 = DIRECTION ( 'NONE',  ( 1.000000000000000000, 0.000000000000000000, 0.000000000000000000 ) ) ;
#22292 = AXIS2_PLACEMENT_3D ( 'NONE', #10646, #15263, #36729 ) ;
#22293 = TOROIDAL_SURFACE ( 'NONE', #45921, 26.49999999999999645, 0.5000000000000000000 ) ;
#22294 = CARTESIAN_POINT ( 'NONE',  ( -34.31243252642735087, -10.02680648607962510, -3.499999999999997335 ) ) ;
#22295 = CARTESIAN_POINT ( 'NONE',  ( -114.0570736234661808, 0.000000000000000000, 9.524999999999991473 ) ) ;
#22296 = ORIENTED_EDGE ( 'NONE', *, *, #22559, .F. ) ;
#22297 = AXIS2_PLACEMENT_3D ( 'NONE', #13876, #35342, #13514 ) ;
#22298 =( LENGTH_UNIT ( ) NAMED_UNIT ( * ) SI_UNIT ( .MILLI., .METRE. ) );
#22299 = CARTESIAN_POINT ( 'NONE',  ( -60.29499999999999460, -2.607480562269069768, 8.024999999999991473 ) ) ;
#22300 = EDGE_LOOP ( 'NONE', ( #69370, #45172, #1840, #4013 ) ) ;
#22301 = B_SPLINE_CURVE_WITH_KNOTS ( 'NONE', 3,
 ( #5382, #52, #27178, #26505, #48714, #48028, #416, #744 ),
 .UNSPECIFIED., .F., .F.,
 ( 4, 2, 2, 4 ),
 ( 2.544313220903533887E-07, 0.002693395767724534023, 0.004039966435925756300, 0.005386537104126978143 ),
 .UNSPECIFIED. ) ;
#22302 = PLANE ( 'NONE',  #54184 ) ;
#22303 = COLOUR_RGB ( '', 0.09019608, 0.27058824, 0.51372549) ;
#22304 = ADVANCED_FACE ( 'NONE', ( #68493 ), #41430, .F. ) ;
#22305 = DIRECTION ( 'NONE',  ( -1.000000000000000000, 0.000000000000000000, 0.000000000000000000 ) ) ;
#22306 = CARTESIAN_POINT ( 'NONE',  ( -45.00000000000000711, 8.707403661853012622, -5.727618941854548673 ) ) ;
#22307 = ORIENTED_EDGE ( 'NONE', *, *, #54623, .T. ) ;
#22308 = SPHERICAL_SURFACE ( 'NONE', #23579, 1.000000000000000000 ) ;
#22309 = DIRECTION ( 'NONE',  ( 0.000000000000000000, 0.000000000000000000, 1.000000000000000000 ) ) ;
#22310 = EDGE_LOOP ( 'NONE', ( #14352, #28417, #66569, #18984 ) ) ;
#22311 = AXIS2_PLACEMENT_3D ( 'NONE', #16228, #26718, #27058 ) ;
#22312 = EDGE_CURVE ( 'NONE', #22382, #63620, #17343, .T. ) ;
#22313 = LINE ( 'NONE', #40519, #22418 ) ;
#22314 = LINE ( 'NONE', #31820, #23536 ) ;
#22315 = CARTESIAN_POINT ( 'NONE',  ( -116.0049999999999955, 6.826472737025116366, 4.959722759717898555 ) ) ;
#22316 = VERTEX_POINT ( 'NONE', #52335 ) ;
#22317 = ADVANCED_FACE ( 'NONE', ( #63881 ), #57948, .T. ) ;
#22318 = CARTESIAN_POINT ( 'NONE',  ( 25.00000000000000355, 37.00000000000000000, 3.000000000000000000 ) ) ;
#22319 =( LENGTH_UNIT ( ) NAMED_UNIT ( * ) SI_UNIT ( .MILLI., .METRE. ) );
#22320 = FILL_AREA_STYLE_COLOUR ( '', #34676 ) ;
#22321 = PRESENTATION_STYLE_ASSIGNMENT (( #63833 ) ) ;
#22322 = DIRECTION ( 'NONE',  ( -0.000000000000000000, -0.000000000000000000, -1.000000000000000000 ) ) ;
#22323 = CARTESIAN_POINT ( 'NONE',  ( -151.8570736234661638, -5.598654528085803328, -7.705886871421366635 ) ) ;
#22324 = EDGE_CURVE ( 'NONE', #38885, #51977, #37352, .T. ) ;
#22325 = CARTESIAN_POINT ( 'NONE',  ( 8.102448949553179958, 135.3949999999999534, 5.886773742842750679 ) ) ;
#22326 = CARTESIAN_POINT ( 'NONE',  ( -97.70707362346617231, -3.094860106618431139, -9.524999999999991473 ) ) ;
#22327 = EDGE_CURVE ( 'NONE', #48570, #6729, #8130, .T. ) ;
#22328 = PRESENTATION_LAYER_ASSIGNMENT (  '', '', ( #15626 ) ) ;
#22329 = CARTESIAN_POINT ( 'NONE',  ( 23.00000000000000000, 0.000000000000000000, -24.00402776293825013 ) ) ;
#22330 = EDGE_LOOP ( 'NONE', ( #42573, #20034, #27694, #17879 ) ) ;
#22331 =( NAMED_UNIT ( * ) PLANE_ANGLE_UNIT ( ) SI_UNIT ( $, .RADIAN. ) );
#22332 = EDGE_CURVE ( 'NONE', #44124, #64274, #60340, .T. ) ;
#22333 = SURFACE_SIDE_STYLE ('',( #5429 ) ) ;
#22334 = CIRCLE ( 'NONE', #41433, 15.00000000000000000 ) ;
#22335 = DIRECTION ( 'NONE',  ( -0.000000000000000000, 1.000000000000000000, -0.000000000000000000 ) ) ;
#22336 = CARTESIAN_POINT ( 'NONE',  ( -133.2549999999999955, -4.716976649647092401, 6.492361379858946790 ) ) ;
#22337 = CARTESIAN_POINT ( 'NONE',  ( 32.00000000000000000, 15.00000000000000000, -80.00402776293826435 ) ) ;
#22338 = DIRECTION ( 'NONE',  ( -1.000000000000000000, 0.000000000000000000, 0.000000000000000000 ) ) ;
#22339 = CARTESIAN_POINT ( 'NONE',  ( -145.3449999999999989, 7.632228543268599452, -2.479861379858951942 ) ) ;
#22340 = ADVANCED_FACE ( 'NONE', ( #64922, #49815 ), #17473, .T. ) ;
#22341 = CIRCLE ( 'NONE', #56015, 0.2500000000000002220 ) ;
#22342 = CARTESIAN_POINT ( 'NONE',  ( -132.8949999999999818, 6.826472737025115478, 4.959722759717899443 ) ) ;
#22343 = EDGE_LOOP ( 'NONE', ( #38952, #62932, #50963, #61416 ) ) ;
#22344 = PRESENTATION_LAYER_ASSIGNMENT (  '', '', ( #17868 ) ) ;
#22345 = CARTESIAN_POINT ( 'NONE',  ( 15.48999599679679662, 146.4999999999999716, 9.500000000000000000 ) ) ;
#22346 = CARTESIAN_POINT ( 'NONE',  ( 24.70577775730027881, 26.00000000000004619, -27.50000000000000711 ) ) ;
#22347 = EDGE_CURVE ( 'NONE', #38818, #21246, #43053, .T. ) ;
#22348 = CARTESIAN_POINT ( 'NONE',  ( -47.90499999999997272, 2.607480562269068880, -8.024999999999993250 ) ) ;
#22349 = CARTESIAN_POINT ( 'NONE',  ( -59.39499999999998892, -6.826472737025115478, -4.959722759717899443 ) ) ;
#22350 = CIRCLE ( 'NONE', #2031, 1.000000000000000888 ) ;
#22351 = MECHANICAL_DESIGN_GEOMETRIC_PRESENTATION_REPRESENTATION (  '', ( #52689 ), #47087 ) ;
#22352 = FILL_AREA_STYLE ('',( #808 ) ) ;
#22353 = CARTESIAN_POINT ( 'NONE',  ( 24.21231517720798010, 117.4999999999999716, -7.500000000000000000 ) ) ;
#22354 = CARTESIAN_POINT ( 'NONE',  ( 0.000000000000000000, 87.30187232391182306, 8.025000000000000355 ) ) ;
#22355 = CARTESIAN_POINT ( 'NONE',  ( -76.10707362346617799, 8.102448949553172852, -5.886773742842744461 ) ) ;
#22356 = CARTESIAN_POINT ( 'NONE',  ( -103.7929263765337851, -3.094860106618429807, 9.524999999999991473 ) ) ;
#22357 = DIRECTION ( 'NONE',  ( 2.775557561562891351E-17, -0.1585527532634897485, 0.9873505073845696423 ) ) ;
#22358 = VECTOR ( 'NONE', #7875, 1000.000000000000000 ) ;
#22359 = FACE_OUTER_BOUND ( 'NONE', #68876, .T. ) ;
#22360 = CARTESIAN_POINT ( 'NONE',  ( -163.1070736234661354, 8.102448949553172852, -5.886773742842744461 ) ) ;
#22361 = PLANE ( 'NONE',  #40502 ) ;
#22362 = DIRECTION ( 'NONE',  ( 0.000000000000000000, -1.000000000000000000, 0.000000000000000000 ) ) ;
#22363 = CONICAL_SURFACE ( 'NONE', #61649, 6.999999999999997335, 0.7853981633974500554 ) ;
#22364 = CARTESIAN_POINT ( 'NONE',  ( 27.00000000000001776, 42.00000000000000000, -34.49999999999999289 ) ) ;
#22365 = ORIENTED_EDGE ( 'NONE', *, *, #61369, .T. ) ;
#22366 =( LENGTH_UNIT ( ) NAMED_UNIT ( * ) SI_UNIT ( .MILLI., .METRE. ) );
#22367 = ORIENTED_EDGE ( 'NONE', *, *, #52052, .T. ) ;
#22368 = CARTESIAN_POINT ( 'NONE',  ( 8.437984349512095861, 123.3070736234661666, 1.550032578732817026E-15 ) ) ;
#22369 = CARTESIAN_POINT ( 'NONE',  ( 20.71231517720797299, 149.6390813561872619, 10.00000000000000000 ) ) ;
#22370 = SURFACE_STYLE_USAGE ( .BOTH. , #32561 ) ;
#22371 = SURFACE_SIDE_STYLE ('',( #49136 ) ) ;
#22372 = ORIENTED_EDGE ( 'NONE', *, *, #24509, .T. ) ;
#22374 = ORIENTED_EDGE ( 'NONE', *, *, #14385, .F. ) ;
#22373 = AXIS2_PLACEMENT_3D ( 'NONE', #67395, #51229, #66348 ) ;
#22375 = CARTESIAN_POINT ( 'NONE',  ( -116.6070736234661780, -8.102448949553174629, 5.886773742842742685 ) ) ;
#22376 = ORIENTED_EDGE ( 'NONE', *, *, #4516, .T. ) ;
#22377 = PRESENTATION_STYLE_ASSIGNMENT (( #17480 ) ) ;
#22378 = CIRCLE ( 'NONE', #33622, 0.2500000000000002220 ) ;
#22379 = PRESENTATION_LAYER_ASSIGNMENT (  '', '', ( #37041 ) ) ;
#22380 = DIRECTION ( 'NONE',  ( 1.000000000000000000, 0.000000000000000000, 0.000000000000000000 ) ) ;
#22381 = CARTESIAN_POINT ( 'NONE',  ( -86.84499999999998465, -7.632228543268599452, 2.479861379858951054 ) ) ;
#22382 = VERTEX_POINT ( 'NONE', #53679 ) ;
#22383 = CIRCLE ( 'NONE', #48288, 5.000000000000004441 ) ;
#22384 = CARTESIAN_POINT ( 'NONE',  ( 7.683128691873284843, 153.7401750098334503, -4.275384889837861024 ) ) ;
#22385 = ADVANCED_FACE ( 'NONE', ( #54025 ), #1641, .T. ) ;
#22386 = DIRECTION ( 'NONE',  ( 0.000000000000000000, -1.000000000000000000, 0.000000000000000000 ) ) ;
#22387 = DIRECTION ( 'NONE',  ( -0.000000000000000000, 0.000000000000000000, -1.000000000000000000 ) ) ;
#22388 = ORIENTED_EDGE ( 'NONE', *, *, #29743, .F. ) ;
#22389 = CARTESIAN_POINT ( 'NONE',  ( 6.826472737025119919, 160.8929263765338078, 4.959722759717908325 ) ) ;
#22390 = DIRECTION ( 'NONE',  ( 1.000000000000000000, 0.000000000000000000, 0.000000000000000000 ) ) ;
#22391 = TOROIDAL_SURFACE ( 'NONE', #56084, 18.99999999999998934, 1.000000000000000000 ) ;
#22392 = ADVANCED_FACE ( 'NONE', ( #50166 ), #67362, .F. ) ;
#22393 = EDGE_CURVE ( 'NONE', #35268, #30333, #8291, .T. ) ;
#22394 = EDGE_LOOP ( 'NONE', ( #50159, #63103, #17889, #64226 ) ) ;
#22395 = EDGE_LOOP ( 'NONE', ( #3415, #27108, #30617, #4424 ) ) ;
#22396 = CARTESIAN_POINT ( 'NONE',  ( 48.00000000000000000, 99.99999999999992895, -9.500000000000000000 ) ) ;
#22397 = CARTESIAN_POINT ( 'NONE',  ( 55.65811388300842566, 13.02565835097472657, -6.000000000000000000 ) ) ;
#22399 = MECHANICAL_DESIGN_GEOMETRIC_PRESENTATION_REPRESENTATION (  '', ( #15649 ), #58348 ) ;
#22398 = CARTESIAN_POINT ( 'NONE',  ( 39.74999999999999289, 18.74999999999997868, 3.750000000000000000 ) ) ;
#22400 = CARTESIAN_POINT ( 'NONE',  ( -177.9570736234661865, 9.058813317711329915, -2.943386871421373119 ) ) ;
#22401 = AXIS2_PLACEMENT_3D ( 'NONE', #47227, #8171, #24658 ) ;
#22402 = PLANE ( 'NONE',  #24012 ) ;
#22403 =( LENGTH_UNIT ( ) NAMED_UNIT ( * ) SI_UNIT ( .MILLI., .METRE. ) );
#22404 = CARTESIAN_POINT ( 'NONE',  ( -0.5396081309076679045, 154.1248569342653809, 9.149856934265343966 ) ) ;
#22405 = VERTEX_POINT ( 'NONE', #50499 ) ;
#22406 = MECHANICAL_DESIGN_GEOMETRIC_PRESENTATION_REPRESENTATION (  '', ( #47159 ), #60594 ) ;
#22407 = CARTESIAN_POINT ( 'NONE',  ( 3.000000000000002665, 42.00000000000000000, -80.00402776293826435 ) ) ;
#22408 = EDGE_CURVE ( 'NONE', #27227, #59919, #63156, .T. ) ;
#22409 = CYLINDRICAL_SURFACE ( 'NONE', #25592, 7.999999999999992895 ) ;
#22410 = DIRECTION ( 'NONE',  ( 0.000000000000000000, 0.000000000000000000, 1.000000000000000000 ) ) ;
#22411 = VERTEX_POINT ( 'NONE', #7243 ) ;
#22412 = CARTESIAN_POINT ( 'NONE',  ( -158.4549999999999841, 7.632228543268599452, -2.479861379858951942 ) ) ;
#22413 = CARTESIAN_POINT ( 'NONE',  ( 3.499999999999999112, 34.24999999999998579, 3.750000000000000000 ) ) ;
#22414 = CARTESIAN_POINT ( 'NONE',  ( -9.250000000000003553, 27.74999999999998934, -4.000000000000000000 ) ) ;
#22415 = CARTESIAN_POINT ( 'NONE',  ( -172.1949999999999648, 8.437984349512085203, -1.550032578732815448E-15 ) ) ;
#22416 = CARTESIAN_POINT ( 'NONE',  ( -159.2949999999999875, -2.607480562269069768, 8.024999999999991473 ) ) ;
#22417 = STYLED_ITEM ( 'NONE', ( #14264 ), #1191 ) ;
#22418 = VECTOR ( 'NONE', #54314, 1000.000000000000000 ) ;
#22419 = VERTEX_POINT ( 'NONE', #33957 ) ;
#22420 = CARTESIAN_POINT ( 'NONE',  ( -89.99292637653380211, 8.102448949553172852, -5.886773742842744461 ) ) ;
#22421 = CARTESIAN_POINT ( 'NONE',  ( 44.56131952741601765, 9.853773175805232043, 3.472780323909878675 ) ) ;
#22422 = CIRCLE ( 'NONE', #52719, 0.2500000000000002220 ) ;
#22423 = DIRECTION ( 'NONE',  ( 1.000000000000000000, 0.000000000000000000, 0.000000000000000000 ) ) ;
#22424 = CARTESIAN_POINT ( 'NONE',  ( -86.45499999999998408, 7.632228543268599452, -2.479861379858951942 ) ) ;
#22425 = CARTESIAN_POINT ( 'NONE',  ( -168.5070736234661695, 8.102448949553176405, 5.886773742842740909 ) ) ;
#22426 = SURFACE_STYLE_FILL_AREA ( #6570 ) ;
#22427 = PRESENTATION_LAYER_ASSIGNMENT (  '', '', ( #50501 ) ) ;
#22428 = CARTESIAN_POINT ( 'NONE',  ( -80.24499999999997613, -4.716976649647093289, -6.492361379858945902 ) ) ;
#22429 = CARTESIAN_POINT ( 'NONE',  ( 9.058813317711337021, 139.6550000000000011, 2.943386871421375783 ) ) ;
#22430 = B_SPLINE_CURVE_WITH_KNOTS ( 'NONE', 3,
 ( #46137, #41211, #3853, #61558, #67925, #57348, #9179, #25338 ),
 .UNSPECIFIED., .F., .F.,
 ( 4, 2, 2, 4 ),
 ( 2.544316211735830308E-07, 0.002094919859796804274, 0.003142252573884619406, 0.004189585287972434971 ),
 .UNSPECIFIED. ) ;
#22431 = EDGE_CURVE ( 'NONE', #11358, #8903, #39978, .T. ) ;
#22432 = CARTESIAN_POINT ( 'NONE',  ( 6.062177826491071286, -3.500000000000002220, 0.000000000000000000 ) ) ;
#22433 = CIRCLE ( 'NONE', #7808, 0.5000000000000004441 ) ;
#22434 = CARTESIAN_POINT ( 'NONE',  ( 1.447422522084233387, 154.2051516657656691, 9.145303841767301378 ) ) ;
#22435 = EDGE_CURVE ( 'NONE', #6981, #36954, #20473, .T. ) ;
#22436 = B_SPLINE_CURVE_WITH_KNOTS ( 'NONE', 3,
 ( #56796, #36422, #3991, #57479, #25120, #8949 ),
 .UNSPECIFIED., .F., .F.,
 ( 4, 2, 4 ),
 ( 0.000000000000000000, 0.0003110060432796291855, 0.0006220120865592583710 ),
 .UNSPECIFIED. ) ;
#22437 = AXIS2_PLACEMENT_3D ( 'NONE', #10655, #64107, #15962 ) ;
#22438 = DIRECTION ( 'NONE',  ( 0.000000000000000000, 0.000000000000000000, -1.000000000000000000 ) ) ;
#22439 = DIRECTION ( 'NONE',  ( -0.7071067811865398012, 0.000000000000000000, -0.7071067811865552333 ) ) ;
#22440 = ORIENTED_EDGE ( 'NONE', *, *, #63078, .T. ) ;
#22441 = AXIS2_PLACEMENT_3D ( 'NONE', #59160, #374, #16644 ) ;
#22442 = FILL_AREA_STYLE ('',( #49884 ) ) ;
#22443 = CARTESIAN_POINT ( 'NONE',  ( -135.0570736234661808, 0.000000000000000000, 9.524999999999991473 ) ) ;
#22444 = CIRCLE ( 'NONE', #19054, 13.50000000000000178 ) ;
#22445 = CARTESIAN_POINT ( 'NONE',  ( -12.74999999999999822, -4.000000000000000000, 0.000000000000000000 ) ) ;
#22446 = SURFACE_STYLE_FILL_AREA ( #16164 ) ;
#22447 = ORIENTED_EDGE ( 'NONE', *, *, #43278, .F. ) ;
#22448 = AXIS2_PLACEMENT_3D ( 'NONE', #9208, #30627, #52133 ) ;
#22449 = ORIENTED_EDGE ( 'NONE', *, *, #57573, .T. ) ;
#22450 = DIRECTION ( 'NONE',  ( -0.000000000000000000, -0.000000000000000000, 1.000000000000000000 ) ) ;
#22451 = DIRECTION ( 'NONE',  ( -1.000000000000000000, 0.000000000000000000, 0.000000000000000000 ) ) ;
#22452 = VECTOR ( 'NONE', #68218, 1000.000000000000000 ) ;
#22453 = FACE_OUTER_BOUND ( 'NONE', #61797, .T. ) ;
#22454 = FILL_AREA_STYLE ('',( #28036 ) ) ;
#22455 = VECTOR ( 'NONE', #20161, 1000.000000000000000 ) ;
#22456 = CYLINDRICAL_SURFACE ( 'NONE', #21735, 0.2500000000000002220 ) ;
#22457 = CARTESIAN_POINT ( 'NONE',  ( 0.000000000000000000, 140.9429263765338192, -8.025000000000000355 ) ) ;
#22458 = ORIENTED_EDGE ( 'NONE', *, *, #38319, .T. ) ;
#22459 = CARTESIAN_POINT ( 'NONE',  ( -114.6549999999999869, -7.632228543268600340, -2.479861379858950166 ) ) ;
#22460 = VERTEX_POINT ( 'NONE', #29365 ) ;
#22461 = DIRECTION ( 'NONE',  ( -0.000000000000000000, -1.000000000000000000, 0.000000000000000000 ) ) ;
#22462 = ORIENTED_EDGE ( 'NONE', *, *, #9812, .F. ) ;
#22463 = FILL_AREA_STYLE ('',( #16866 ) ) ;
#22464 = SPHERICAL_SURFACE ( 'NONE', #15333, 0.2500000000000000000 ) ;
#22465 = ORIENTED_EDGE ( 'NONE', *, *, #3539, .F. ) ;
#22466 = ADVANCED_FACE ( 'NONE', ( #23756 ), #1267, .F. ) ;
#22467 = STYLED_ITEM ( 'NONE', ( #64540 ), #1385 ) ;
#22468 = DIRECTION ( 'NONE',  ( -0.000000000000000000, 1.000000000000000000, -0.000000000000000000 ) ) ;
#22469 =( BOUNDED_CURVE ( )  B_SPLINE_CURVE ( 2, ( #32925, #1879, #59986, #22360, #44892, #38231, #33267, #39262, #23389, #27609, #50152 ),
 .UNSPECIFIED., .F., .F. ) 
 B_SPLINE_CURVE_WITH_KNOTS ( ( 3, 2, 2, 2, 2, 3 ),
 ( 0.1413043478260837538, 0.1434782608695619466, 0.1456521739130400839, 0.1478260869565182767, 0.1499999999999964140, 0.1521739130434746068 ),
 .UNSPECIFIED. ) 
 CURVE ( )  GEOMETRIC_REPRESENTATION_ITEM ( )  RATIONAL_B_SPLINE_CURVE ( ( 1.000000000000071720, 0.9510565162950815887, 1.000000000000000000, 0.9510565162951535312, 1.000000000000000000, 0.9510565162951535312, 1.000000000000000000, 0.9510565162951535312, 1.000000000000000000, 0.9510565162952360208, 0.9999999999999175104 ) ) 
 REPRESENTATION_ITEM ( '' )  );
#22470 = CARTESIAN_POINT ( 'NONE',  ( 5.598654528085809545, 157.1449999999999818, -7.705886871421373741 ) ) ;
#22471 = DIRECTION ( 'NONE',  ( -0.000000000000000000, -0.000000000000000000, -1.000000000000000000 ) ) ;
#22472 = VERTEX_POINT ( 'NONE', #7923 ) ;
#22473 = ORIENTED_EDGE ( 'NONE', *, *, #57270, .F. ) ;
#22474 = DIRECTION ( 'NONE',  ( -1.000000000000000000, 0.000000000000000000, 0.000000000000000000 ) ) ;
#22475 = CARTESIAN_POINT ( 'NONE',  ( 21.02379604162863913, 154.9999999999999716, -10.50000000000000000 ) ) ;
#22476 = EDGE_LOOP ( 'NONE', ( #25494, #24050, #20670, #64791 ) ) ;
#22477 = CARTESIAN_POINT ( 'NONE',  ( 7.632228543268607446, 134.0429263765338135, 2.479861379858954606 ) ) ;
#22478 = DIRECTION ( 'NONE',  ( 0.000000000000000000, 0.000000000000000000, 1.000000000000000000 ) ) ;
#22479 = DIRECTION ( 'NONE',  ( 0.000000000000000000, 0.000000000000000000, 1.000000000000000000 ) ) ;
#22480 = PRESENTATION_STYLE_ASSIGNMENT (( #27384 ) ) ;
#22481 = ADVANCED_FACE ( 'NONE', ( #24106 ), #24431, .T. ) ;
#22482 = CARTESIAN_POINT ( 'NONE',  ( 44.00000000000000000, 21.74999999999998579, -3.750000000000000000 ) ) ;
#22483 = ORIENTED_EDGE ( 'NONE', *, *, #38670, .T. ) ;
#22484 = AXIS2_PLACEMENT_3D ( 'NONE', #20363, #63959, #53431 ) ;
#22485 = SURFACE_STYLE_FILL_AREA ( #43635 ) ;
#22486 = VERTEX_POINT ( 'NONE', #4986 ) ;
#22487 = CARTESIAN_POINT ( 'NONE',  ( -51.89292637653380069, -8.102448949553172852, -5.886773742842741797 ) ) ;
#22488 = AXIS2_PLACEMENT_3D ( 'NONE', #21460, #58407, #42615 ) ;
#22489 = DIRECTION ( 'NONE',  ( 1.000000000000000000, 0.000000000000000000, 0.000000000000000000 ) ) ;
#22490 = CARTESIAN_POINT ( 'NONE',  ( 71.50000000000000000, 14.49137674618942562, 7.500000000000000000 ) ) ;
#22491 = CARTESIAN_POINT ( 'NONE',  ( -158.7570736234661979, -5.598654528085801552, 7.705886871421367523 ) ) ;
#22492 = CARTESIAN_POINT ( 'NONE',  ( -142.5549999999999784, 0.000000000000000000, 8.024999999999991473 ) ) ;
#22493 = DIRECTION ( 'NONE',  ( -0.000000000000000000, -0.000000000000000000, 1.000000000000000000 ) ) ;
#22494 = AXIS2_PLACEMENT_3D ( 'NONE', #68317, #31011, #46197 ) ;
#22495 = ORIENTED_EDGE ( 'NONE', *, *, #62179, .T. ) ;
#22496 = CARTESIAN_POINT ( 'NONE',  ( 18.25000000000000711, 33.99999999999999289, -3.750000000000000000 ) ) ;
#22497 = COLOUR_RGB ( '', 0.31764706, 0.68627451, 0.89019608) ;
#22498 = DIRECTION ( 'NONE',  ( 0.000000000000000000, -1.000000000000000000, 0.000000000000000000 ) ) ;
#22499 = EDGE_LOOP ( 'NONE', ( #28871, #7338, #49190, #14934 ) ) ;
#22500 = CIRCLE ( 'NONE', #31465, 0.5000000000000004441 ) ;
#22501 = ORIENTED_EDGE ( 'NONE', *, *, #10722, .T. ) ;
#22502 = CARTESIAN_POINT ( 'NONE',  ( -45.03910207541591859, 8.121286912818771242, 3.616120970039215621 ) ) ;
#22503 = EDGE_CURVE ( 'NONE', #24854, #13223, #58676, .T. ) ;
#22504 = CARTESIAN_POINT ( 'NONE',  ( -51.35707362346617089, 5.598654528085804216, 7.705886871421366635 ) ) ;
#22505 = CARTESIAN_POINT ( 'NONE',  ( -52.55499999999999261, 0.000000000000000000, 8.024999999999991473 ) ) ;
#22506 = EDGE_LOOP ( 'NONE', ( #9368, #22449, #26622, #26014, #9921, #7173 ) ) ;
#22507 = LINE ( 'NONE', #48590, #59527 ) ;
#22508 = DIRECTION ( 'NONE',  ( 0.000000000000000000, 0.000000000000000000, -1.000000000000000000 ) ) ;
#22509 = CARTESIAN_POINT ( 'NONE',  ( 0.000000000000000000, 36.74999999999999289, 4.000000000000000000 ) ) ;
#22510 = CARTESIAN_POINT ( 'NONE',  ( 23.71231517720798010, 113.4999999999999858, 9.500000000000000000 ) ) ;
#22511 = STYLED_ITEM ( 'NONE', ( #9833 ), #17576 ) ;
#22512 = DIRECTION ( 'NONE',  ( 0.000000000000000000, 1.000000000000000000, 0.000000000000000000 ) ) ;
#22513 = CARTESIAN_POINT ( 'NONE',  ( -128.5429263765338135, 9.058813317711329915, 2.943386871421369566 ) ) ;
#22514 =( GEOMETRIC_REPRESENTATION_CONTEXT ( 3 ) GLOBAL_UNCERTAINTY_ASSIGNED_CONTEXT ( ( #20013 ) ) GLOBAL_UNIT_ASSIGNED_CONTEXT ( ( #7308, #6256, #22095 ) ) REPRESENTATION_CONTEXT ( 'NONE', 'WORKASPACE' ) );
#22515 = VERTEX_POINT ( 'NONE', #31717 ) ;
#22516 = MECHANICAL_DESIGN_GEOMETRIC_PRESENTATION_REPRESENTATION (  '', ( #44980 ), #6733 ) ;
#22517 = CARTESIAN_POINT ( 'NONE',  ( -60.00000000000000000, -2.024042244987997205E-14, -6.500000000000000000 ) ) ;
#22518 = CARTESIAN_POINT ( 'NONE',  ( -7.335726704534230258, 2.464278740834323411, -5.294148637306920868 ) ) ;
#22519 = PRESENTATION_STYLE_ASSIGNMENT (( #53494 ) ) ;
#22520 = DIRECTION ( 'NONE',  ( 0.000000000000000000, 0.000000000000000000, -1.000000000000000000 ) ) ;
#22521 = CARTESIAN_POINT ( 'NONE',  ( 0.000000000000000000, 0.000000000000000000, 0.000000000000000000 ) ) ;
#22522 = CARTESIAN_POINT ( 'NONE',  ( -105.4449999999999790, 0.000000000000000000, 8.024999999999991473 ) ) ;
#22523 = CARTESIAN_POINT ( 'NONE',  ( 8.102448949553181734, 159.3949999999999534, 5.886773742842750679 ) ) ;
#22524 = CARTESIAN_POINT ( 'NONE',  ( -79.49499999999999034, 6.826472737025113702, -4.959722759717902107 ) ) ;
#22525 = FACE_OUTER_BOUND ( 'NONE', #5734, .T. ) ;
#22526 = CARTESIAN_POINT ( 'NONE',  ( 13.75000000000000533, 30.99999999999999289, 4.000000000000000000 ) ) ;
#22527 = DIRECTION ( 'NONE',  ( 0.000000000000000000, 0.000000000000000000, 1.000000000000000000 ) ) ;
#22528 = AXIS2_PLACEMENT_3D ( 'NONE', #35820, #25587, #51307 ) ;
#22529 = LINE ( 'NONE', #65437, #59545 ) ;
#22530 = VERTEX_POINT ( 'NONE', #26436 ) ;
#22531 = CARTESIAN_POINT ( 'NONE',  ( -124.7929263765337851, -3.094860106618429807, 9.524999999999991473 ) ) ;
#22532 = CARTESIAN_POINT ( 'NONE',  ( -142.7949999999999875, 2.607480562269068880, -8.024999999999993250 ) ) ;
#22533 = CARTESIAN_POINT ( 'NONE',  ( -3.414918479307655907, 7.000000000000006217, 0.7696370661449007944 ) ) ;
#22534 = AXIS2_PLACEMENT_3D ( 'NONE', #30292, #7820, #34905 ) ;
#22535 = DIRECTION ( 'NONE',  ( 0.000000000000000000, 0.000000000000000000, 1.000000000000000000 ) ) ;
#22536 = FILL_AREA_STYLE_COLOUR ( '', #24913 ) ;
#22537 = EDGE_LOOP ( 'NONE', ( #15101, #21870, #14684 ) ) ;
#22538 = ORIENTED_EDGE ( 'NONE', *, *, #53279, .F. ) ;
#22539 = AXIS2_PLACEMENT_3D ( 'NONE', #22112, #1640, #64998 ) ;
#22540 = LINE ( 'NONE', #60169, #62890 ) ;
#22541 = AXIS2_PLACEMENT_3D ( 'NONE', #18723, #34546, #7478 ) ;
#22542 = CARTESIAN_POINT ( 'NONE',  ( -172.5570736234661808, -1.166476076187852838E-15, -9.524999999999991473 ) ) ;
#22543 = PRESENTATION_LAYER_ASSIGNMENT (  '', '', ( #41664 ) ) ;
#22544 = CARTESIAN_POINT ( 'NONE',  ( -50.15707362346616094, -9.058813317711329915, -2.943386871421370898 ) ) ;
#22545 = FACE_OUTER_BOUND ( 'NONE', #15625, .T. ) ;
#22546 = EDGE_LOOP ( 'NONE', ( #11306, #18687, #10264, #50099 ) ) ;
#22547 = CARTESIAN_POINT ( 'NONE',  ( -142.8550000000000182, 4.716976649647094177, 6.492361379858945902 ) ) ;
#22548 = ORIENTED_EDGE ( 'NONE', *, *, #4253, .F. ) ;
#22549 = ORIENTED_EDGE ( 'NONE', *, *, #52281, .F. ) ;
#22550 = LINE ( 'NONE', #39113, #7717 ) ;
#22551 = DIRECTION ( 'NONE',  ( 0.000000000000000000, 0.000000000000000000, 1.000000000000000000 ) ) ;
#22552 = EDGE_LOOP ( 'NONE', ( #41016, #8815, #36994, #66327 ) ) ;
#22553 = EDGE_CURVE ( 'NONE', #582, #46401, #26088, .T. ) ;
#22554 = DIRECTION ( 'NONE',  ( 0.000000000000000000, 1.000000000000000000, 0.000000000000000000 ) ) ;
#22555 = FILL_AREA_STYLE_COLOUR ( '', #53428 ) ;
#22556 = CARTESIAN_POINT ( 'NONE',  ( -10.01517768586949231, 134.1949999999999932, -6.132527647946036459E-16 ) ) ;
#22557 = CARTESIAN_POINT ( 'NONE',  ( 71.62068965517239860, 36.41396814395972115, -9.500000000000000000 ) ) ;
#22558 = AXIS2_PLACEMENT_3D ( 'NONE', #43854, #37901, #11096 ) ;
#22559 = EDGE_CURVE ( 'NONE', #49424, #2072, #48285, .T. ) ;
#22560 = AXIS2_PLACEMENT_3D ( 'NONE', #59630, #37900, #5812 ) ;
#22561 = EDGE_LOOP ( 'NONE', ( #49076, #33705 ) ) ;
#22562 = CARTESIAN_POINT ( 'NONE',  ( -5.598654528085806881, 125.8549999999999898, -7.705886871421374629 ) ) ;
#22563 = CARTESIAN_POINT ( 'NONE',  ( -50.45499999999996987, 7.632228543268599452, -2.479861379858951942 ) ) ;
#22564 = CARTESIAN_POINT ( 'NONE',  ( -120.2949999999999733, -2.607480562269069768, 8.024999999999991473 ) ) ;
#22565 = CARTESIAN_POINT ( 'NONE',  ( -0.9728900412908211282, 153.0000000000000000, -7.965808808122195828 ) ) ;
#22566 = ORIENTED_EDGE ( 'NONE', *, *, #22717, .T. ) ;
#22567 = CARTESIAN_POINT ( 'NONE',  ( -10.01517768586949231, 153.3050000000000068, -6.132527647946036459E-16 ) ) ;
#22568 = DIRECTION ( 'NONE',  ( 0.000000000000000000, 0.000000000000000000, -1.000000000000000000 ) ) ;
#22569 = COLOUR_RGB ( '', 0.72549020, 0.75294118, 0.79215686) ;
#22570 = EDGE_CURVE ( 'NONE', #47273, #61027, #21876, .T. ) ;
#22571 = DIRECTION ( 'NONE',  ( 0.000000000000000000, -1.000000000000000000, 0.000000000000000000 ) ) ;
#22572 = LINE ( 'NONE', #21888, #66509 ) ;
#22573 = EDGE_CURVE ( 'NONE', #26861, #53011, #44262, .T. ) ;
#22574 = EDGE_CURVE ( 'NONE', #26003, #7688, #35073, .T. ) ;
#22575 = ORIENTED_EDGE ( 'NONE', *, *, #43880, .T. ) ;
#22576 = CARTESIAN_POINT ( 'NONE',  ( -15.98999599679679839, 50.00000000000000000, 7.000000000000000000 ) ) ;
#22577 = CARTESIAN_POINT ( 'NONE',  ( -171.6550000000000011, -7.632228543268600340, -2.479861379858950166 ) ) ;
#22579 = VERTEX_POINT ( 'NONE', #59134 ) ;
#22578 = EDGE_CURVE ( 'NONE', #51757, #37913, #32882, .T. ) ;
#22580 = LINE ( 'NONE', #16974, #35105 ) ;
#22581 =( BOUNDED_CURVE ( )  B_SPLINE_CURVE ( 2, ( #54712, #59286, #6886, #22375, #17135, #27963, #38252, #37915, #1559, #50169, #7246 ),
 .UNSPECIFIED., .F., .F. ) 
 B_SPLINE_CURVE_WITH_KNOTS ( ( 3, 2, 2, 2, 2, 3 ),
 ( 0.4782608695652061370, 0.4804347826086843298, 0.4826086956521625226, 0.4847826086956407710, 0.4869565217391190193, 0.4891304347825972121 ),
 .UNSPECIFIED. ) 
 CURVE ( )  GEOMETRIC_REPRESENTATION_ITEM ( )  RATIONAL_B_SPLINE_CURVE ( ( 1.000000000000253797, 0.9510565162948998452, 1.000000000000000000, 0.9510565162951535312, 1.000000000000000000, 0.9510565162951535312, 1.000000000000000000, 0.9510565162951535312, 1.000000000000000000, 0.9510565162954122131, 0.9999999999997413180 ) ) 
 REPRESENTATION_ITEM ( '' )  );
#22582 =( NAMED_UNIT ( * ) PLANE_ANGLE_UNIT ( ) SI_UNIT ( $, .RADIAN. ) );
#22583 = AXIS2_PLACEMENT_3D ( 'NONE', #55681, #2132, #19428 ) ;
#22584 = EDGE_CURVE ( 'NONE', #30995, #53241, #5317, .T. ) ;
#22585 = PRESENTATION_LAYER_ASSIGNMENT (  '', '', ( #36048 ) ) ;
#22586 = LINE ( 'NONE', #7453, #53220 ) ;
#22587 =( NAMED_UNIT ( * ) PLANE_ANGLE_UNIT ( ) SI_UNIT ( $, .RADIAN. ) );
#22588 = CARTESIAN_POINT ( 'NONE',  ( -78.44292637653380496, -1.166476076187852838E-15, -9.524999999999991473 ) ) ;
#22589 = ORIENTED_EDGE ( 'NONE', *, *, #63854, .T. ) ;
#22590 = CARTESIAN_POINT ( 'NONE',  ( 13.75000000000000533, 30.74999999999999289, -3.750000000000000000 ) ) ;
#22591 = COLOUR_RGB ( '', 0.72549020, 0.75294118, 0.79215686) ;
#22592 = DIRECTION ( 'NONE',  ( 0.000000000000000000, 0.000000000000000000, -1.000000000000000000 ) ) ;
#22593 = CARTESIAN_POINT ( 'NONE',  ( -82.40500000000000114, -2.607480562269069768, 8.024999999999991473 ) ) ;
#22594 = VERTEX_POINT ( 'NONE', #42339 ) ;
#22595 = FACE_OUTER_BOUND ( 'NONE', #22656, .T. ) ;
#22596 = MECHANICAL_DESIGN_GEOMETRIC_PRESENTATION_REPRESENTATION (  '', ( #4600 ), #36115 ) ;
#22597 = SURFACE_STYLE_USAGE ( .BOTH. , #27147 ) ;
#22598 =( LENGTH_UNIT ( ) NAMED_UNIT ( * ) SI_UNIT ( .MILLI., .METRE. ) );
#22599 = CARTESIAN_POINT ( 'NONE',  ( -55.85707362346617799, -5.598654528085803328, -7.705886871421366635 ) ) ;
#22600 = SURFACE_SIDE_STYLE ('',( #60548 ) ) ;
#22601 = EDGE_LOOP ( 'NONE', ( #45480, #58109, #66847, #10555 ) ) ;
#22602 = CARTESIAN_POINT ( 'NONE',  ( 2.418535808707042101, 7.000000000000006217, 0.3989014552058406382 ) ) ;
#22603 = B_SPLINE_CURVE_WITH_KNOTS ( 'NONE', 3,
 ( #39489, #12710, #34186, #55639, #45123, #49014 ),
 .UNSPECIFIED., .F., .F.,
 ( 4, 2, 4 ),
 ( 0.000000000000000000, 0.0003058591473678601161, 0.0006117182947357202322 ),
 .UNSPECIFIED. ) ;
#22604 = VECTOR ( 'NONE', #4974, 1000.000000000000000 ) ;
#22605 = CARTESIAN_POINT ( 'NONE',  ( 39.74999999999999289, 18.74999999999997868, -3.750000000000000000 ) ) ;
#22606 = CARTESIAN_POINT ( 'NONE',  ( -104.6050000000000040, 6.826472737025113702, -4.959722759717902107 ) ) ;
#22607 = CARTESIAN_POINT ( 'NONE',  ( 9.058813317711337021, 126.5449999999999875, 2.943386871421375783 ) ) ;
#22608 = CARTESIAN_POINT ( 'NONE',  ( -116.6949999999999790, -8.437984349512085203, 5.166775262442717831E-16 ) ) ;
#22609 = CIRCLE ( 'NONE', #6879, 3.600000000000005862 ) ;
#22611 = CARTESIAN_POINT ( 'NONE',  ( -18.05403742664741529, 11.32513715180358993, -3.972212260121688931 ) ) ;
#22610 = DIRECTION ( 'NONE',  ( -1.000000000000000000, 1.189524669241239115E-16, 0.000000000000000000 ) ) ;
#22612 = CARTESIAN_POINT ( 'NONE',  ( -156.8929263765338362, -8.102448949553172852, -5.886773742842741797 ) ) ;
#22613 = CARTESIAN_POINT ( 'NONE',  ( -180.7449999999999761, 4.716976649647094177, 6.492361379858945902 ) ) ;
#22614 = VECTOR ( 'NONE', #61568, 1000.000000000000000 ) ;
#22615 = DIRECTION ( 'NONE',  ( 0.000000000000000000, 1.000000000000000000, -0.000000000000000000 ) ) ;
#22616 = FACE_OUTER_BOUND ( 'NONE', #67209, .T. ) ;
#22617 = ORIENTED_EDGE ( 'NONE', *, *, #8349, .T. ) ;
#22618 = DIRECTION ( 'NONE',  ( 0.000000000000000000, 0.000000000000000000, 1.000000000000000000 ) ) ;
#22619 = CARTESIAN_POINT ( 'NONE',  ( 10.39230484541326582, -1.107695154586738839, 1.440973567693753677E-18 ) ) ;
#22620 = ORIENTED_EDGE ( 'NONE', *, *, #34620, .T. ) ;
#22621 = CARTESIAN_POINT ( 'NONE',  ( -67.64292637653379359, -5.598654528085801552, 7.705886871421367523 ) ) ;
#22622 = B_SPLINE_CURVE_WITH_KNOTS ( 'NONE', 3,
 ( #50910, #47054, #25537, #51259, #52322, #62137, #61777, #24163, #18870, #9042, #30462, #62826, #35770, #3719 ),
 .UNSPECIFIED., .F., .F.,
 ( 4, 2, 2, 2, 2, 2, 4 ),
 ( 5.830426119014177358E-15, 0.002172676916780083827, 0.003259015375167209454, 0.004345353833554335514, 0.005431692291941461574, 0.006518030750328586767, 0.008690707667102838888 ),
 .UNSPECIFIED. ) ;
#22623 = LINE ( 'NONE', #65173, #52076 ) ;
#22624 =( LENGTH_UNIT ( ) NAMED_UNIT ( * ) SI_UNIT ( .MILLI., .METRE. ) );
#22625 = AXIS2_PLACEMENT_3D ( 'NONE', #8298, #25488, #25151 ) ;
#22626 = COLOUR_RGB ( '', 0.40784314, 0.44705882, 0.49803922) ;
#22627 = LINE ( 'NONE', #65176, #42830 ) ;
#22628 = SURFACE_SIDE_STYLE ('',( #12394 ) ) ;
#22629 = CARTESIAN_POINT ( 'NONE',  ( 44.28021770739999852, 9.999999999999980460, -3.500000000000000000 ) ) ;
#22631 = VECTOR ( 'NONE', #11340, 1000.000000000000000 ) ;
#22630 = SURFACE_STYLE_FILL_AREA ( #1091 ) ;
#22632 = ORIENTED_EDGE ( 'NONE', *, *, #13245, .T. ) ;
#22633 = CARTESIAN_POINT ( 'NONE',  ( -169.5549999999999784, 0.000000000000000000, 8.024999999999991473 ) ) ;
#22634 = ORIENTED_EDGE ( 'NONE', *, *, #55032, .F. ) ;
#22635 = CARTESIAN_POINT ( 'NONE',  ( -55.00000000000000000, -2.024042244987997205E-14, 11.50000000000003020 ) ) ;
#22636 = COLOUR_RGB ( '', 0.40784314, 0.44705882, 0.49803922) ;
#22637 =( NAMED_UNIT ( * ) PLANE_ANGLE_UNIT ( ) SI_UNIT ( $, .RADIAN. ) );
#22638 = ADVANCED_FACE ( 'NONE', ( #52858, #36710 ), #9936, .T. ) ;
#22639 = CIRCLE ( 'NONE', #52975, 0.5000000000000004441 ) ;
#22640 = CARTESIAN_POINT ( 'NONE',  ( -34.75000000000000711, 0.000000000000000000, -7.000000000000000000 ) ) ;
#22641 = CARTESIAN_POINT ( 'NONE',  ( -4.716976649647098618, 152.2570736234661695, 6.492361379858953008 ) ) ;
#22642 = EDGE_CURVE ( 'NONE', #36746, #25647, #48637, .T. ) ;
#22643 = VERTEX_POINT ( 'NONE', #28498 ) ;
#22644 = CARTESIAN_POINT ( 'NONE',  ( -80.90499999999998693, 2.607480562269069324, -8.024999999999993250 ) ) ;
#22645 = AXIS2_PLACEMENT_3D ( 'NONE', #6173, #11448, #44555 ) ;
#22646 = CARTESIAN_POINT ( 'NONE',  ( 7.632228543268608334, 132.4570736234661581, -2.479861379858951942 ) ) ;
#22647 = LINE ( 'NONE', #17401, #67613 ) ;
#22648 = CARTESIAN_POINT ( 'NONE',  ( 60.00000000000000000, 1.797044900979284448E-15, -11.50000000000000000 ) ) ;
#22649 = CARTESIAN_POINT ( 'NONE',  ( 71.50000000000000000, 35.92875272052971525, 7.000000000000000000 ) ) ;
#22650 = CIRCLE ( 'NONE', #61955, 1.000000000000000000 ) ;
#22651 = EDGE_CURVE ( 'NONE', #33880, #39293, #50853, .T. ) ;
#22652 =( LENGTH_UNIT ( ) NAMED_UNIT ( * ) SI_UNIT ( .MILLI., .METRE. ) );
#22653 = EDGE_LOOP ( 'NONE', ( #25154, #17605, #65305, #26165 ) ) ;
#22654 = DIRECTION ( 'NONE',  ( 0.000000000000000000, 0.000000000000000000, 1.000000000000000000 ) ) ;
#22655 = CARTESIAN_POINT ( 'NONE',  ( -63.14499999999998181, -4.716976649647092401, 6.492361379858946790 ) ) ;
#22656 = EDGE_LOOP ( 'NONE', ( #42300, #30368, #59577, #2884 ) ) ;
#22657 =( NAMED_UNIT ( * ) PLANE_ANGLE_UNIT ( ) SI_UNIT ( $, .RADIAN. ) );
#22658 = PRESENTATION_LAYER_ASSIGNMENT (  '', '', ( #37316 ) ) ;
#22659 = SURFACE_STYLE_USAGE ( .BOTH. , #64862 ) ;
#22660 = CARTESIAN_POINT ( 'NONE',  ( -45.00000000000000000, 8.443649368548083345, -5.542175914092441147 ) ) ;
#22661 = ADVANCED_FACE ( 'NONE', ( #680 ), #49645, .T. ) ;
#22662 = ORIENTED_EDGE ( 'NONE', *, *, #63219, .T. ) ;
#22663 = DIRECTION ( 'NONE',  ( 0.000000000000000000, 1.000000000000000000, 0.000000000000000000 ) ) ;
#22664 = ORIENTED_EDGE ( 'NONE', *, *, #51566, .F. ) ;
#22665 = CIRCLE ( 'NONE', #47467, 0.5000000000000006661 ) ;
#22666 = LINE ( 'NONE', #32876, #21301 ) ;
#22667 = CARTESIAN_POINT ( 'NONE',  ( -75.00000000000000000, 9.517485987480760912, 6.449082597785469773 ) ) ;
#22668 = CARTESIAN_POINT ( 'NONE',  ( -112.4050000000000011, -2.607480562269069768, 8.024999999999991473 ) ) ;
#22669 = ORIENTED_EDGE ( 'NONE', *, *, #52775, .T. ) ;
#22670 = PRESENTATION_STYLE_ASSIGNMENT (( #31203 ) ) ;
#22671 = SURFACE_STYLE_USAGE ( .BOTH. , #65924 ) ;
#22672 =( NAMED_UNIT ( * ) PLANE_ANGLE_UNIT ( ) SI_UNIT ( $, .RADIAN. ) );
#22673 = FILL_AREA_STYLE_COLOUR ( '', #35341 ) ;
#22674 = DIRECTION ( 'NONE',  ( 0.000000000000000000, 1.000000000000000000, 0.000000000000000000 ) ) ;
#22675 = CARTESIAN_POINT ( 'NONE',  ( -146.3070736234662093, -10.01517768586948698, 6.132527647946031529E-16 ) ) ;
#22676 = CARTESIAN_POINT ( 'NONE',  ( 8.102448949553179958, 132.3949999999999534, 5.886773742842750679 ) ) ;
#22677 = CARTESIAN_POINT ( 'NONE',  ( -98.75707362346616947, -5.598654528085801552, 7.705886871421367523 ) ) ;
#22678 = CIRCLE ( 'NONE', #4688, 4.999999999999997335 ) ;
#22679 = CIRCLE ( 'NONE', #61974, 0.2500000000000002220 ) ;
#22680 = CARTESIAN_POINT ( 'NONE',  ( -54.89978656749008223, -9.015750088250108263, -2.278575939223535851 ) ) ;
#22681 = ORIENTED_EDGE ( 'NONE', *, *, #22408, .F. ) ;
#22682 = DIRECTION ( 'NONE',  ( 0.000000000000000000, 0.000000000000000000, -1.000000000000000000 ) ) ;
#22685 = PRESENTATION_LAYER_ASSIGNMENT (  '', '', ( #9076 ) ) ;
#22684 = DIRECTION ( 'NONE',  ( 0.000000000000000000, 0.000000000000000000, 1.000000000000000000 ) ) ;
#22683 =( NAMED_UNIT ( * ) SI_UNIT ( $, .STERADIAN. ) SOLID_ANGLE_UNIT ( ) );
#22686 = DIRECTION ( 'NONE',  ( -1.000000000000000000, 0.000000000000000000, 0.000000000000000000 ) ) ;
#22687 = CARTESIAN_POINT ( 'NONE',  ( -126.9549999999999841, -7.632228543268599452, 2.479861379858951054 ) ) ;
#22688 = CYLINDRICAL_SURFACE ( 'NONE', #57815, 1.000000000000000000 ) ;
#22689 = CARTESIAN_POINT ( 'NONE',  ( -146.6929263765337623, 10.01517768586948698, -1.839758294383808966E-15 ) ) ;
#22690 = DIRECTION ( 'NONE',  ( -0.000000000000000000, -1.000000000000000000, -0.000000000000000000 ) ) ;
#22691 = CARTESIAN_POINT ( 'NONE',  ( -148.7950000000000159, 2.607480562269068880, -8.024999999999993250 ) ) ;
#22692 = CARTESIAN_POINT ( 'NONE',  ( -124.4949999999999761, 6.826472737025113702, -4.959722759717902107 ) ) ;
#22693 = VERTEX_POINT ( 'NONE', #22557 ) ;
#22694 = CARTESIAN_POINT ( 'NONE',  ( -44.50000000000000000, 99.99999999999992895, -3.500000000000000000 ) ) ;
#22695 = EDGE_CURVE ( 'NONE', #62632, #61113, #55243, .T. ) ;
#22696 = DIRECTION ( 'NONE',  ( -0.7071067811865425767, -0.000000000000000000, -0.7071067811865525687 ) ) ;
#22697 = CARTESIAN_POINT ( 'NONE',  ( -195.0000000000000000, 0.000000000000000000, 9.524999999999991473 ) ) ;
#22698 = UNCERTAINTY_MEASURE_WITH_UNIT (LENGTH_MEASURE( 1.000000000000000082E-05 ), #16278, 'distance_accuracy_value', 'NONE');
#22699 = CARTESIAN_POINT ( 'NONE',  ( -183.8929263765337794, -8.102448949553172852, -5.886773742842741797 ) ) ;
#22700 = SURFACE_STYLE_USAGE ( .BOTH. , #49445 ) ;
#22701 = CARTESIAN_POINT ( 'NONE',  ( -57.74499999999999034, 4.716976649647094177, 6.492361379858945902 ) ) ;
#22702 = AXIS2_PLACEMENT_3D ( 'NONE', #31915, #52701, #4838 ) ;
#22703 = SURFACE_SIDE_STYLE ('',( #39252 ) ) ;
#22704 = CARTESIAN_POINT ( 'NONE',  ( -15.98999599679679839, 50.00000000000000000, 7.500000000000000000 ) ) ;
#22705 = CARTESIAN_POINT ( 'NONE',  ( -195.0000000000000000, 1.166476076187852838E-15, -9.524999999999991473 ) ) ;
#22706 = MECHANICAL_DESIGN_GEOMETRIC_PRESENTATION_REPRESENTATION (  '', ( #54175 ), #67642 ) ;
#22707 = CARTESIAN_POINT ( 'NONE',  ( -45.00000000000000000, 9.708372675170618749, -3.611004237778681514 ) ) ;
#22708 = CARTESIAN_POINT ( 'NONE',  ( -95.24292637653381632, 5.598654528085804216, 7.705886871421366635 ) ) ;
#22709 = APPLICATION_PROTOCOL_DEFINITION ( 'draft international standard', 'automotive_design', 1998, #14129 ) ;
#22710 = DIRECTION ( 'NONE',  ( 1.000000000000000000, 0.000000000000000000, -1.300977106640442040E-16 ) ) ;
#22711 = CIRCLE ( 'NONE', #44103, 0.5000000000000004441 ) ;
#22712 = FACE_OUTER_BOUND ( 'NONE', #7395, .T. ) ;
#22713 = DIRECTION ( 'NONE',  ( -0.000000000000000000, -0.000000000000000000, 1.000000000000000000 ) ) ;
#22714 = CARTESIAN_POINT ( 'NONE',  ( -99.35707362346617799, 5.598654528085804216, 7.705886871421366635 ) ) ;
#22715 = AXIS2_PLACEMENT_3D ( 'NONE', #65485, #5006, #43726 ) ;
#22716 = EDGE_CURVE ( 'NONE', #22912, #56203, #10398, .T. ) ;
#22717 = EDGE_CURVE ( 'NONE', #43113, #50288, #44749, .T. ) ;
#22718 = ORIENTED_EDGE ( 'NONE', *, *, #4682, .T. ) ;
#22719 = DIRECTION ( 'NONE',  ( -2.168404344971009361E-16, 1.000000000000000000, 0.000000000000000000 ) ) ;
#22720 = ORIENTED_EDGE ( 'NONE', *, *, #15928, .F. ) ;
#22721 = DIRECTION ( 'NONE',  ( 1.000000000000000000, 0.000000000000000000, -0.000000000000000000 ) ) ;
#22722 = PRESENTATION_LAYER_ASSIGNMENT (  '', '', ( #59771 ) ) ;
#22723 = CARTESIAN_POINT ( 'NONE',  ( -8.437984349512095861, 127.8070736234661666, -5.166775262442723748E-16 ) ) ;
#22724 = STYLED_ITEM ( 'NONE', ( #1403 ), #46191 ) ;
#22725 = ADVANCED_FACE ( 'NONE', ( #43707 ), #44060, .F. ) ;
#22726 = DIRECTION ( 'NONE',  ( 0.000000000000000000, 0.000000000000000000, -1.000000000000000000 ) ) ;
#22727 = DIRECTION ( 'NONE',  ( -8.673617379884027583E-15, 1.295453483465570108E-14, 1.000000000000000000 ) ) ;
#22728 = VECTOR ( 'NONE', #33624, 1000.000000000000000 ) ;
#22729 = SURFACE_STYLE_FILL_AREA ( #1197 ) ;
#22730 = ORIENTED_EDGE ( 'NONE', *, *, #568, .T. ) ;
#22731 =( LENGTH_UNIT ( ) NAMED_UNIT ( * ) SI_UNIT ( .MILLI., .METRE. ) );
#22732 = ORIENTED_EDGE ( 'NONE', *, *, #64963, .F. ) ;
#22733 = DIRECTION ( 'NONE',  ( -1.000000000000000000, 0.000000000000000000, 0.000000000000000000 ) ) ;
#22734 = CARTESIAN_POINT ( 'NONE',  ( 57.00000000000000000, 16.00000000000000000, -60.00402776293825724 ) ) ;
#22735 =( GEOMETRIC_REPRESENTATION_CONTEXT ( 3 ) GLOBAL_UNCERTAINTY_ASSIGNED_CONTEXT ( ( #20205 ) ) GLOBAL_UNIT_ASSIGNED_CONTEXT ( ( #22211, #34490, #60864 ) ) REPRESENTATION_CONTEXT ( 'NONE', 'WORKASPACE' ) );
#22736 = EDGE_CURVE ( 'NONE', #22202, #32850, #30596, .T. ) ;
#22737 = AXIS2_PLACEMENT_3D ( 'NONE', #54651, #49390, #12078 ) ;
#22738 = DIRECTION ( 'NONE',  ( 0.000000000000000000, 0.000000000000000000, -1.000000000000000000 ) ) ;
#22739 = CARTESIAN_POINT ( 'NONE',  ( -87.89499999999998181, 6.826472737025116366, 4.959722759717898555 ) ) ;
#22740 = ORIENTED_EDGE ( 'NONE', *, *, #50219, .T. ) ;
#22741 = COLOUR_RGB ( '', 0.09019608, 0.27058824, 0.51372549) ;
#22742 =( NAMED_UNIT ( * ) PLANE_ANGLE_UNIT ( ) SI_UNIT ( $, .RADIAN. ) );
#22743 =( NAMED_UNIT ( * ) PLANE_ANGLE_UNIT ( ) SI_UNIT ( $, .RADIAN. ) );
#22744 = CYLINDRICAL_SURFACE ( 'NONE', #55381, 0.2500000000000002220 ) ;
#22745 = ADVANCED_FACE ( 'NONE', ( #8114 ), #14089, .F. ) ;
#22746 = ORIENTED_EDGE ( 'NONE', *, *, #58223, .F. ) ;
#22747 = FACE_OUTER_BOUND ( 'NONE', #50544, .T. ) ;
#22748 = FILL_AREA_STYLE ('',( #27641 ) ) ;
#22749 = CARTESIAN_POINT ( 'NONE',  ( -67.94292637653380496, 0.000000000000000000, 9.524999999999991473 ) ) ;
#22750 = VERTEX_POINT ( 'NONE', #61544 ) ;
#22751 = CIRCLE ( 'NONE', #59856, 0.5000000000000004441 ) ;
#22752 = DIRECTION ( 'NONE',  ( -1.000000000000000000, 0.000000000000000000, 0.000000000000000000 ) ) ;
#22753 = ORIENTED_EDGE ( 'NONE', *, *, #2368, .T. ) ;
#22754 = CARTESIAN_POINT ( 'NONE',  ( 1.000000000000000000, 0.9999999999999991118, 80.00402776293826435 ) ) ;
#22755 = DIRECTION ( 'NONE',  ( 0.000000000000000000, 0.000000000000000000, 1.000000000000000000 ) ) ;
#22756 = CARTESIAN_POINT ( 'NONE',  ( -4.683753779217433078, -2.005109422339666825, 5.887500484252660371 ) ) ;
#22757 = CARTESIAN_POINT ( 'NONE',  ( -182.1570736234661751, -9.058813317711329915, -2.943386871421370898 ) ) ;
#22758 = CARTESIAN_POINT ( 'NONE',  ( 60.00000000000000000, 1.797044900979284448E-15, 11.50000000000003730 ) ) ;
#22759 = CARTESIAN_POINT ( 'NONE',  ( 10.00000000000000711, 50.00000000000000000, -60.00000000000000000 ) ) ;
#22760 = COLOUR_RGB ( '', 0.40784314, 0.44705882, 0.49803922) ;
#22761 = CARTESIAN_POINT ( 'NONE',  ( -68.09292637653378222, 3.094860106618433360, 9.524999999999991473 ) ) ;
#22762 = CARTESIAN_POINT ( 'NONE',  ( -5.871527698221338909, 153.2522028323956533, -5.859198738425243747 ) ) ;
#22763 = ORIENTED_EDGE ( 'NONE', *, *, #4922, .F. ) ;
#22764 = STYLED_ITEM ( 'NONE', ( #6730 ), #24852 ) ;
#22765 = DIRECTION ( 'NONE',  ( 0.000000000000000000, 0.000000000000000000, 1.000000000000000000 ) ) ;
#22766 = DIRECTION ( 'NONE',  ( 0.000000000000000000, 0.000000000000000000, -1.000000000000000000 ) ) ;
#22767 = DIRECTION ( 'NONE',  ( 0.000000000000000000, 1.000000000000000000, -0.000000000000000000 ) ) ;
#22768 = FACE_OUTER_BOUND ( 'NONE', #24995, .T. ) ;
#22769 = EDGE_LOOP ( 'NONE', ( #34497, #55309, #54630, #46034 ) ) ;
#22770 = CARTESIAN_POINT ( 'NONE',  ( -161.6050000000000182, 6.826472737025113702, -4.959722759717902107 ) ) ;
#22771 = SPHERICAL_SURFACE ( 'NONE', #12803, 0.2500000000000000000 ) ;
#22772 = DIRECTION ( 'NONE',  ( 0.000000000000000000, 0.000000000000000000, 1.000000000000000000 ) ) ;
#22773 = CARTESIAN_POINT ( 'NONE',  ( -176.2449999999999761, -4.716976649647093289, -6.492361379858945902 ) ) ;
#22774 = VECTOR ( 'NONE', #62874, 1000.000000000000000 ) ;
#22775 = AXIS2_PLACEMENT_3D ( 'NONE', #65624, #17468, #38936 ) ;
#22776 = CARTESIAN_POINT ( 'NONE',  ( -160.0449999999999875, 7.632228543268600340, 2.479861379858949277 ) ) ;
#22777 = ORIENTED_EDGE ( 'NONE', *, *, #3952, .T. ) ;
#22778 = ADVANCED_FACE ( 'NONE', ( #67543 ), #19342, .T. ) ;
#22779 = SURFACE_STYLE_USAGE ( .BOTH. , #49520 ) ;
#22780 = CARTESIAN_POINT ( 'NONE',  ( 45.65811388296465623, 10.21937129432154556, 3.824795692829482174 ) ) ;
#22781 = CARTESIAN_POINT ( 'NONE',  ( 39.49999999999999289, 18.99999999999997868, 4.000000000000000000 ) ) ;
#22782 = CARTESIAN_POINT ( 'NONE',  ( -77.00499999999999545, 6.826472737025116366, 4.959722759717898555 ) ) ;
#22783 = DIRECTION ( 'NONE',  ( 1.000000000000000000, 0.000000000000000000, 0.000000000000000000 ) ) ;
#22784 = PRESENTATION_LAYER_ASSIGNMENT (  '', '', ( #46416 ) ) ;
#22785 = DIRECTION ( 'NONE',  ( 1.000000000000000000, 0.000000000000000000, 0.000000000000000000 ) ) ;
#22786 = CARTESIAN_POINT ( 'NONE',  ( -67.49499999999999034, 6.826472737025113702, -4.959722759717902107 ) ) ;
#22787 = CARTESIAN_POINT ( 'NONE',  ( -10.01517768586949231, 141.3050000000000068, -6.132527647946036459E-16 ) ) ;
#22788 = AXIS2_PLACEMENT_3D ( 'NONE', #28402, #49560, #1290 ) ;
#22789 = CARTESIAN_POINT ( 'NONE',  ( 6.239160159721276244, -3.193457606803200566, 4.616329562535936848E-16 ) ) ;
#22790 = CARTESIAN_POINT ( 'NONE',  ( 52.75000000000000000, 25.24999999999998579, -4.000000000000000000 ) ) ;
#22791 = UNCERTAINTY_MEASURE_WITH_UNIT (LENGTH_MEASURE( 1.000000000000000082E-05 ), #6639, 'distance_accuracy_value', 'NONE');
#22792 = AXIS2_PLACEMENT_3D ( 'NONE', #10637, #47635, #20852 ) ;
#22793 = EDGE_LOOP ( 'NONE', ( #21414, #57067, #12310, #50713 ) ) ;
#22794 = EDGE_CURVE ( 'NONE', #42291, #2399, #62261, .T. ) ;
#22795 = DIRECTION ( 'NONE',  ( -1.000000000000000000, 0.000000000000000000, 0.000000000000000000 ) ) ;
#22796 = DIRECTION ( 'NONE',  ( -0.000000000000000000, -0.000000000000000000, -1.000000000000000000 ) ) ;
#22797 = CONICAL_SURFACE ( 'NONE', #12688, 9.000000000000000000, 0.7853981633974500554 ) ;
#22798 = EDGE_CURVE ( 'NONE', #58151, #62845, #34831, .T. ) ;
#22799 = FACE_OUTER_BOUND ( 'NONE', #18789, .T. ) ;
#22800 = ADVANCED_FACE ( 'NONE', ( #2789 ), #3471, .F. ) ;
#22801 = PRESENTATION_LAYER_ASSIGNMENT (  '', '', ( #28378 ) ) ;
#22802 = CARTESIAN_POINT ( 'NONE',  ( 72.49999999999998579, 119.9999999999997868, -10.00000000000000000 ) ) ;
#22803 = SURFACE_STYLE_FILL_AREA ( #2675 ) ;
#22804 = VERTEX_POINT ( 'NONE', #36958 ) ;
#22805 = ORIENTED_EDGE ( 'NONE', *, *, #1447, .F. ) ;
#22806 = DIRECTION ( 'NONE',  ( -0.000000000000000000, -0.000000000000000000, 1.000000000000000000 ) ) ;
#22807 = VECTOR ( 'NONE', #5969, 1000.000000000000000 ) ;
#22808 = ADVANCED_FACE ( 'NONE', ( #5574 ), #43297, .F. ) ;
#22809 = PRESENTATION_STYLE_ASSIGNMENT (( #1275 ) ) ;
#22810 = DIRECTION ( 'NONE',  ( 0.000000000000000000, 0.000000000000000000, -1.000000000000000000 ) ) ;
#22811 = FACE_OUTER_BOUND ( 'NONE', #36582, .T. ) ;
#22812 = CARTESIAN_POINT ( 'NONE',  ( 6.000000000000017764, 14.00000000000000533, -35.50000000000000000 ) ) ;
#22813 = EDGE_CURVE ( 'NONE', #19551, #5309, #21666, .T. ) ;
#22814 = ORIENTED_EDGE ( 'NONE', *, *, #32910, .T. ) ;
#22815 = CARTESIAN_POINT ( 'NONE',  ( -111.9549999999999841, -7.632228543268599452, 2.479861379858951054 ) ) ;
#22816 = ORIENTED_EDGE ( 'NONE', *, *, #55015, .T. ) ;
#22817 = DIRECTION ( 'NONE',  ( 0.000000000000000000, 0.000000000000000000, 1.000000000000000000 ) ) ;
#22818 = DIRECTION ( 'NONE',  ( -1.000000000000000000, 0.000000000000000000, 0.000000000000000000 ) ) ;
#22819 = EDGE_LOOP ( 'NONE', ( #58029, #6132, #31803, #44096 ) ) ;
#22820 = FACE_BOUND ( 'NONE', #64205, .T. ) ;
#22821 = CARTESIAN_POINT ( 'NONE',  ( 62.24999999999998579, 33.74999999999999289, -3.750000000000000000 ) ) ;
#22822 = ORIENTED_EDGE ( 'NONE', *, *, #8077, .T. ) ;
#22823 = AXIS2_PLACEMENT_3D ( 'NONE', #40476, #34133, #29545 ) ;
#22824 = DIRECTION ( 'NONE',  ( 1.000000000000000000, -0.000000000000000000, 0.000000000000000000 ) ) ;
#22825 = CARTESIAN_POINT ( 'NONE',  ( -3.094860106618432471, 157.5949999999999989, -9.525000000000000355 ) ) ;
#22826 = CARTESIAN_POINT ( 'NONE',  ( 57.00000000000000000, 0.000000000000000000, 60.00402776293827145 ) ) ;
#22827 = VERTEX_POINT ( 'NONE', #251 ) ;
#22828 = VERTEX_POINT ( 'NONE', #15157 ) ;
#22829 = PRESENTATION_STYLE_ASSIGNMENT (( #34059 ) ) ;
#22830 = SURFACE_STYLE_FILL_AREA ( #33036 ) ;
#22831 = EDGE_LOOP ( 'NONE', ( #47429, #777 ) ) ;
#22832 = CARTESIAN_POINT ( 'NONE',  ( -2.607480562269073765, 138.0929263765337964, -8.025000000000000355 ) ) ;
#22833 = CARTESIAN_POINT ( 'NONE',  ( 21.25000000000001066, 24.74999999999998224, -3.750000000000000000 ) ) ;
#22834 = FILL_AREA_STYLE_COLOUR ( '', #63578 ) ;
#22835 = CARTESIAN_POINT ( 'NONE',  ( 4.793647677013328057, -9.000000000000007105, 1.191052472566601628 ) ) ;
#22836 = CARTESIAN_POINT ( 'NONE',  ( -7.632228543268607446, 114.5429263765338277, -2.479861379858953718 ) ) ;
#22837 = ADVANCED_FACE ( 'NONE', ( #31632 ), #20389, .F. ) ;
#22838 = EDGE_LOOP ( 'NONE', ( #26509, #37252, #28682, #24308 ) ) ;
#22839 = CIRCLE ( 'NONE', #60875, 0.2500000000000002220 ) ;
#22840 = DIRECTION ( 'NONE',  ( 0.000000000000000000, 1.000000000000000000, 0.000000000000000000 ) ) ;
#22841 = EDGE_LOOP ( 'NONE', ( #30952, #16735, #57309, #50520 ) ) ;
#22842 = CARTESIAN_POINT ( 'NONE',  ( -50.39292637653380780, 8.102448949553176405, 5.886773742842740909 ) ) ;
#22843 = SURFACE_STYLE_USAGE ( .BOTH. , #38367 ) ;
#22844 = DIRECTION ( 'NONE',  ( 0.000000000000000000, 0.000000000000000000, 1.000000000000000000 ) ) ;
#22845 = CYLINDRICAL_SURFACE ( 'NONE', #69165, 9.524999999999991473 ) ;
#22846 = CARTESIAN_POINT ( 'NONE',  ( -132.5049999999999670, -6.826472737025115478, -4.959722759717899443 ) ) ;
#22847 = EDGE_CURVE ( 'NONE', #51729, #37003, #63309, .T. ) ;
#22848 = UNCERTAINTY_MEASURE_WITH_UNIT (LENGTH_MEASURE( 1.000000000000000082E-05 ), #12733, 'distance_accuracy_value', 'NONE');
#22849 = VERTEX_POINT ( 'NONE', #42581 ) ;
#22850 = STYLED_ITEM ( 'NONE', ( #5945 ), #55422 ) ;
#22851 = CYLINDRICAL_SURFACE ( 'NONE', #50888, 0.2500000000000002220 ) ;
#22853 = CARTESIAN_POINT ( 'NONE',  ( -107.7570736234661695, -5.598654528085801552, 7.705886871421367523 ) ) ;
#22852 = MECHANICAL_DESIGN_GEOMETRIC_PRESENTATION_REPRESENTATION (  '', ( #56516 ), #41967 ) ;
#22854 = CARTESIAN_POINT ( 'NONE',  ( -9.827790563157511022E-16, 118.4429263765338192, 8.025000000000000355 ) ) ;
#22855 = ORIENTED_EDGE ( 'NONE', *, *, #28812, .T. ) ;
#22856 = ORIENTED_EDGE ( 'NONE', *, *, #19610, .F. ) ;
#22857 = CARTESIAN_POINT ( 'NONE',  ( -45.20196116979489176, 8.361269815420033780, 3.290768940563960854 ) ) ;
#22858 = CIRCLE ( 'NONE', #27270, 0.2500000000000002220 ) ;
#22859 = FILL_AREA_STYLE ('',( #65757 ) ) ;
#22860 = CARTESIAN_POINT ( 'NONE',  ( -56.00499999999996703, 6.826472737025116366, 4.959722759717898555 ) ) ;
#22861 = ORIENTED_EDGE ( 'NONE', *, *, #15928, .T. ) ;
#22862 = SURFACE_STYLE_FILL_AREA ( #28438 ) ;
#22863 = SURFACE_SIDE_STYLE ('',( #40431 ) ) ;
#22864 = DIRECTION ( 'NONE',  ( -1.000000000000000000, 0.000000000000000000, 0.000000000000000000 ) ) ;
#22865 = DIRECTION ( 'NONE',  ( 0.000000000000000000, 0.000000000000000000, 1.000000000000000000 ) ) ;
#22866 = CARTESIAN_POINT ( 'NONE',  ( -4.041451884327381450, 7.000000000000006217, 7.500000000000000000 ) ) ;
#22867 = ORIENTED_EDGE ( 'NONE', *, *, #42993, .T. ) ;
#22868 = CIRCLE ( 'NONE', #49826, 1.999999999999998224 ) ;
#22869 = VECTOR ( 'NONE', #10439, 1000.000000000000000 ) ;
#22870 = LINE ( 'NONE', #50292, #12466 ) ;
#22871 = FILL_AREA_STYLE_COLOUR ( '', #61158 ) ;
#22872 = DIRECTION ( 'NONE',  ( -1.000000000000000000, 0.000000000000000000, 0.000000000000000000 ) ) ;
#22873 = CARTESIAN_POINT ( 'NONE',  ( -109.0449999999999875, 7.632228543268600340, 2.479861379858949277 ) ) ;
#22874 = CARTESIAN_POINT ( 'NONE',  ( 3.094860106618435136, 157.2949999999999591, -9.525000000000000355 ) ) ;
#22875 = CARTESIAN_POINT ( 'NONE',  ( -80.54499999999998749, -7.632228543268600340, -2.479861379858950166 ) ) ;
#22876 = EDGE_CURVE ( 'NONE', #52155, #39296, #63986, .T. ) ;
#22877 = DIRECTION ( 'NONE',  ( -1.000000000000000000, 3.011817513800517074E-33, 1.300977106640435384E-16 ) ) ;
#22879 = CARTESIAN_POINT ( 'NONE',  ( -7.000000000000002665, 0.000000000000000000, 0.000000000000000000 ) ) ;
#22878 = COLOUR_RGB ( '', 0.08235294, 0.09019608, 0.10196078) ;
#22880 = COLOUR_RGB ( '', 0.72549020, 0.75294118, 0.79215686) ;
#22881 = FILL_AREA_STYLE_COLOUR ( '', #67408 ) ;
#22882 = CARTESIAN_POINT ( 'NONE',  ( 23.71231517720798010, 113.4999999999999858, -10.00000000000000000 ) ) ;
#22883 = UNCERTAINTY_MEASURE_WITH_UNIT (LENGTH_MEASURE( 1.000000000000000082E-05 ), #50936, 'distance_accuracy_value', 'NONE');
#22884 = SURFACE_SIDE_STYLE ('',( #17286 ) ) ;
#22885 = LINE ( 'NONE', #53708, #22928 ) ;
#22886 = ORIENTED_EDGE ( 'NONE', *, *, #11612, .T. ) ;
#22887 = AXIS2_PLACEMENT_3D ( 'NONE', #39532, #13454, #24692 ) ;
#22888 = EDGE_CURVE ( 'NONE', #19090, #34565, #36329, .T. ) ;
#22889 = CARTESIAN_POINT ( 'NONE',  ( -123.8929263765337794, -8.102448949553172852, -5.886773742842741797 ) ) ;
#22890 = SHAPE_REPRESENTATION_RELATIONSHIP ( 'NONE' , 'NONE' ,  #60355, #25286 ) ;
#22891 = CARTESIAN_POINT ( 'NONE',  ( -134.2450000000000045, -4.716976649647093289, -6.492361379858945902 ) ) ;
#22892 = CARTESIAN_POINT ( 'NONE',  ( -75.00000000000000000, 9.708372675170620525, 6.000000000000000888 ) ) ;
#22893 = ADVANCED_FACE ( 'NONE', ( #31980 ), #5944, .T. ) ;
#22894 = CIRCLE ( 'NONE', #35236, 29.50000000000000000 ) ;
#22895 = CARTESIAN_POINT ( 'NONE',  ( -48.29499999999997328, -2.607480562269069768, 8.024999999999991473 ) ) ;
#22896 = DIRECTION ( 'NONE',  ( -1.000000000000000000, -0.000000000000000000, -0.000000000000000000 ) ) ;
#22897 = VERTEX_POINT ( 'NONE', #26001 ) ;
#22898 = ORIENTED_EDGE ( 'NONE', *, *, #51804, .T. ) ;
#22899 = AXIS2_PLACEMENT_3D ( 'NONE', #18911, #12961, #29484 ) ;
#22900 =( BOUNDED_CURVE ( )  B_SPLINE_CURVE ( 2, ( #48797, #26579, #11102, #48448, #64594, #27616, #69179, #16766, #20981, #31517, #42478 ),
 .UNSPECIFIED., .F., .F. ) 
 B_SPLINE_CURVE_WITH_KNOTS ( ( 3, 2, 2, 2, 2, 3 ),
 ( 0.5294117647058825815, 0.5352941176470590312, 0.5411764705882354809, 0.5470588235294120416, 0.5529411764705884913, 0.5588235294117649410 ),
 .UNSPECIFIED. ) 
 CURVE ( )  GEOMETRIC_REPRESENTATION_ITEM ( )  RATIONAL_B_SPLINE_CURVE ( ( 0.9999999999999981126, 0.9510565162951554186, 1.000000000000000000, 0.9510565162951535312, 1.000000000000000000, 0.9510565162951535312, 1.000000000000000000, 0.9510565162951535312, 1.000000000000000000, 0.9510565162951516438, 1.000000000000001776 ) ) 
 REPRESENTATION_ITEM ( '' )  );
#22901 = CARTESIAN_POINT ( 'NONE',  ( 24.21231517720798010, 112.9999999999999858, 7.500000000000000000 ) ) ;
#22902 =( NAMED_UNIT ( * ) PLANE_ANGLE_UNIT ( ) SI_UNIT ( $, .RADIAN. ) );
#22903 =( GEOMETRIC_REPRESENTATION_CONTEXT ( 3 ) GLOBAL_UNCERTAINTY_ASSIGNED_CONTEXT ( ( #22182 ) ) GLOBAL_UNIT_ASSIGNED_CONTEXT ( ( #62178, #19956, #19258 ) ) REPRESENTATION_CONTEXT ( 'NONE', 'WORKASPACE' ) );
#22904 = CARTESIAN_POINT ( 'NONE',  ( 3.499999999999998668, 36.74999999999999289, -3.750000000000000000 ) ) ;
#22905 = DIRECTION ( 'NONE',  ( 0.000000000000000000, -0.000000000000000000, -1.000000000000000000 ) ) ;
#22906 = AXIS2_PLACEMENT_3D ( 'NONE', #14416, #68253, #36634 ) ;
#22907 = ADVANCED_FACE ( 'NONE', ( #20752 ), #37314, .T. ) ;
#22908 = EDGE_LOOP ( 'NONE', ( #19004, #4826, #54228, #60748, #22718, #6957, #25398, #45036 ) ) ;
#22909 = CARTESIAN_POINT ( 'NONE',  ( -143.7549999999999955, 4.716976649647091513, -6.492361379858946790 ) ) ;
#22910 = ORIENTED_EDGE ( 'NONE', *, *, #8592, .F. ) ;
#22911 = VECTOR ( 'NONE', #48183, 1000.000000000000000 ) ;
#22912 = VERTEX_POINT ( 'NONE', #48903 ) ;
#22913 = CARTESIAN_POINT ( 'NONE',  ( -12.72792206135785698, 115.4999999999999574, -10.50000000000000000 ) ) ;
#22914 = ORIENTED_EDGE ( 'NONE', *, *, #1776, .T. ) ;
#22915 = CARTESIAN_POINT ( 'NONE',  ( -54.89978656747977936, -9.015750088255273909, -2.278575939230922831 ) ) ;
#22916 = CARTESIAN_POINT ( 'NONE',  ( 3.094860106618431583, 126.0949999999999847, 9.525000000000000355 ) ) ;
#22917 = DIRECTION ( 'NONE',  ( 0.000000000000000000, -0.000000000000000000, -1.000000000000000000 ) ) ;
#22918 = EDGE_LOOP ( 'NONE', ( #33202, #12855, #19831, #27145 ) ) ;
#22919 = STYLED_ITEM ( 'NONE', ( #53793 ), #7618 ) ;
#22920 = DIRECTION ( 'NONE',  ( 0.000000000000000000, -1.000000000000000000, -0.000000000000000000 ) ) ;
#22921 = CARTESIAN_POINT ( 'NONE',  ( 8.102448949553179958, 127.5049999999999812, 5.886773742842750679 ) ) ;
#22922 = CARTESIAN_POINT ( 'NONE',  ( -58.40499999999997982, -2.607480562269069768, 8.024999999999991473 ) ) ;
#22923 = PRESENTATION_STYLE_ASSIGNMENT (( #23591 ) ) ;
#22924 = ORIENTED_EDGE ( 'NONE', *, *, #177, .T. ) ;
#22925 = CARTESIAN_POINT ( 'NONE',  ( 3.094860106618431583, 157.2050000000000125, 9.525000000000000355 ) ) ;
#22926 = CARTESIAN_POINT ( 'NONE',  ( 10.99999999999999645, 11.99999999999999289, 3.500000000000004885 ) ) ;
#22927 = UNCERTAINTY_MEASURE_WITH_UNIT (LENGTH_MEASURE( 1.000000000000000082E-05 ), #39450, 'distance_accuracy_value', 'NONE');
#22928 = VECTOR ( 'NONE', #21351, 1000.000000000000000 ) ;
#22929 = SURFACE_STYLE_USAGE ( .BOTH. , #60878 ) ;
#22930 = ORIENTED_EDGE ( 'NONE', *, *, #9603, .F. ) ;
#22931 = SURFACE_SIDE_STYLE ('',( #65118 ) ) ;
#22932 = ORIENTED_EDGE ( 'NONE', *, *, #12151, .F. ) ;
#22933 = AXIS2_PLACEMENT_3D ( 'NONE', #50233, #55839, #46370 ) ;
#22934 = COLOUR_RGB ( '', 0.66274510, 0.83137255, 0.94901961) ;
#22935 = CARTESIAN_POINT ( 'NONE',  ( -67.49999999999998579, -1.932193735051945844E-14, 11.50000000000000000 ) ) ;
#22936 = CARTESIAN_POINT ( 'NONE',  ( -176.6049999999999898, 6.826472737025113702, -4.959722759717902107 ) ) ;
#22937 = ORIENTED_EDGE ( 'NONE', *, *, #51175, .F. ) ;
#22938 = CARTESIAN_POINT ( 'NONE',  ( 22.00000000000002132, 50.00000000000000000, 60.00000000000000000 ) ) ;
#22939 = UNCERTAINTY_MEASURE_WITH_UNIT (LENGTH_MEASURE( 1.000000000000000082E-05 ), #36645, 'distance_accuracy_value', 'NONE');
#22940 = CARTESIAN_POINT ( 'NONE',  ( 1.000000000000000000, 43.00000000000000000, -35.50000000000000000 ) ) ;
#22941 = DIRECTION ( 'NONE',  ( -0.000000000000000000, -0.000000000000000000, -1.000000000000000000 ) ) ;
#22942 = FACE_OUTER_BOUND ( 'NONE', #59672, .T. ) ;
#22943 = EDGE_LOOP ( 'NONE', ( #62109, #52704, #42093 ) ) ;
#22944 = ORIENTED_EDGE ( 'NONE', *, *, #39429, .T. ) ;
#22945 = CARTESIAN_POINT ( 'NONE',  ( -83.60499999999998977, 6.826472737025113702, -4.959722759717902107 ) ) ;
#22946 = ORIENTED_EDGE ( 'NONE', *, *, #37138, .T. ) ;
#22947 = DIRECTION ( 'NONE',  ( 0.000000000000000000, 0.000000000000000000, 1.000000000000000000 ) ) ;
#22948 = VECTOR ( 'NONE', #42107, 1000.000000000000000 ) ;
#22949 = PRESENTATION_LAYER_ASSIGNMENT (  '', '', ( #6064 ) ) ;
#22950 = DIRECTION ( 'NONE',  ( -0.000000000000000000, -1.000000000000000000, -0.000000000000000000 ) ) ;
#22951 = AXIS2_PLACEMENT_3D ( 'NONE', #30631, #10591, #63698 ) ;
#22952 = EDGE_LOOP ( 'NONE', ( #11157, #45045, #32069, #55675 ) ) ;
#22953 = CARTESIAN_POINT ( 'NONE',  ( 5.000000000000000000, 6.123233995736766282E-16, 0.2499999999999941436 ) ) ;
#22955 = CARTESIAN_POINT ( 'NONE',  ( 44.25000000000000000, 0.000000000000000000, 4.000000000000000000 ) ) ;
#22954 = SURFACE_STYLE_FILL_AREA ( #48332 ) ;
#22956 = AXIS2_PLACEMENT_3D ( 'NONE', #69356, #46908, #58795 ) ;
#22957 = CARTESIAN_POINT ( 'NONE',  ( -10.01517768586949231, 128.1950000000000216, -6.132527647946036459E-16 ) ) ;
#22958 = CARTESIAN_POINT ( 'NONE',  ( -102.5949999999999704, 2.607480562269073321, 8.024999999999991473 ) ) ;
#22959 = EDGE_CURVE ( 'NONE', #61482, #44763, #43076, .T. ) ;
#22960 = VECTOR ( 'NONE', #31360, 1000.000000000000000 ) ;
#22961 = CIRCLE ( 'NONE', #56648, 0.2500000000000002220 ) ;
#22962 = SURFACE_STYLE_USAGE ( .BOTH. , #2109 ) ;
#22963 = PRESENTATION_LAYER_ASSIGNMENT (  '', '', ( #8404 ) ) ;
#22964 = CARTESIAN_POINT ( 'NONE',  ( -150.4429263765338192, -1.166476076187852838E-15, -9.524999999999991473 ) ) ;
#22965 =( NAMED_UNIT ( * ) PLANE_ANGLE_UNIT ( ) SI_UNIT ( $, .RADIAN. ) );
#22966 = CARTESIAN_POINT ( 'NONE',  ( -169.4949999999999761, 6.826472737025113702, -4.959722759717902107 ) ) ;
#22967 = VECTOR ( 'NONE', #22244, 1000.000000000000000 ) ;
#22968 = EDGE_CURVE ( 'NONE', #45132, #43730, #54253, .T. ) ;
#22969 = LINE ( 'NONE', #18389, #48994 ) ;
#22970 = ADVANCED_FACE ( 'NONE', ( #6979 ), #32663, .T. ) ;
#22971 = CIRCLE ( 'NONE', #31947, 8.524999999999977263 ) ;
#22972 = ORIENTED_EDGE ( 'NONE', *, *, #31106, .F. ) ;
#22973 = DIRECTION ( 'NONE',  ( 0.000000000000000000, 1.000000000000000000, 0.000000000000000000 ) ) ;
#22974 = EDGE_LOOP ( 'NONE', ( #22139, #45791, #63371, #9153 ) ) ;
#22975 = EDGE_CURVE ( 'NONE', #44696, #48050, #65381, .T. ) ;
#22976 = CARTESIAN_POINT ( 'NONE',  ( -66.14292637653379359, 5.598654528085800663, -7.705886871421367523 ) ) ;
#22977 = CARTESIAN_POINT ( 'NONE',  ( -45.91158085204516226, 9.415459729490459395, 6.077763577362913949 ) ) ;
#22978 = FILL_AREA_STYLE ('',( #1448 ) ) ;
#22979 = EDGE_CURVE ( 'NONE', #59464, #44845, #11573, .T. ) ;
#22980 = FACE_OUTER_BOUND ( 'NONE', #64641, .T. ) ;
#22981 = CARTESIAN_POINT ( 'NONE',  ( 0.7152604538204458962, 42.96841842781390852, 74.40727953928171701 ) ) ;
#22982 = CARTESIAN_POINT ( 'NONE',  ( 30.75000000000001066, 15.99999999999997691, -3.750000000000000000 ) ) ;
#22983 = CARTESIAN_POINT ( 'NONE',  ( 3.081487911019577365E-31, -7.500000000000000888, 24.00000000000000000 ) ) ;
#22984 = EDGE_CURVE ( 'NONE', #35304, #34116, #50900, .T. ) ;
#22985 = ORIENTED_EDGE ( 'NONE', *, *, #6344, .T. ) ;
#22987 = B_SPLINE_CURVE_WITH_KNOTS ( 'NONE', 3,
 ( #51110, #68324, #35624, #13446, #24681, #41608, #29642, #7827, #8195, #34560 ),
 .UNSPECIFIED., .F., .F.,
 ( 4, 2, 2, 2, 4 ),
 ( 0.000000000000000000, 0.0004222318702814410588, 0.0008444637405628821177, 0.001266695610844323231, 0.001688927481125764235 ),
 .UNSPECIFIED. ) ;
#22986 = CARTESIAN_POINT ( 'NONE',  ( -173.9049999999999443, 2.607480562269069324, -8.024999999999993250 ) ) ;
#22988 = MECHANICAL_DESIGN_GEOMETRIC_PRESENTATION_REPRESENTATION (  '', ( #42119 ), #35338 ) ;
#22989 = EDGE_LOOP ( 'NONE', ( #22549, #35054, #61533, #67211 ) ) ;
#22990 =( LENGTH_UNIT ( ) NAMED_UNIT ( * ) SI_UNIT ( .MILLI., .METRE. ) );
#22991 = PRESENTATION_STYLE_ASSIGNMENT (( #17387 ) ) ;
#22992 = CARTESIAN_POINT ( 'NONE',  ( -11.74999999999999645, -0.9999999999999995559, 7.000000000000001776 ) ) ;
#22993 = CIRCLE ( 'NONE', #62303, 6.999999999999997335 ) ;
#22994 =( NAMED_UNIT ( * ) PLANE_ANGLE_UNIT ( ) SI_UNIT ( $, .RADIAN. ) );
#22995 = CARTESIAN_POINT ( 'NONE',  ( -8.437984349512095861, 151.8070736234661524, -5.166775262442723748E-16 ) ) ;
#22996 =( GEOMETRIC_REPRESENTATION_CONTEXT ( 3 ) GLOBAL_UNCERTAINTY_ASSIGNED_CONTEXT ( ( #14382 ) ) GLOBAL_UNIT_ASSIGNED_CONTEXT ( ( #20916, #63803, #48370 ) ) REPRESENTATION_CONTEXT ( 'NONE', 'WORKASPACE' ) );
#22997 =( BOUNDED_CURVE ( )  B_SPLINE_CURVE ( 2, ( #49091, #32883, #32503, #64547, #59232, #26860, #54319, #16726, #17072, #1135, #11761 ),
 .UNSPECIFIED., .F., .F. ) 
 B_SPLINE_CURVE_WITH_KNOTS ( ( 3, 2, 2, 2, 2, 3 ),
 ( 0.8043478260869565410, 0.8065217391304347894, 0.8086956521739130377, 0.8108695652173912860, 0.8130434782608695343, 0.8152173913043477826 ),
 .UNSPECIFIED. ) 
 CURVE ( )  GEOMETRIC_REPRESENTATION_ITEM ( )  RATIONAL_B_SPLINE_CURVE ( ( 1.000000000000000000, 0.9510565162951535312, 1.000000000000000000, 0.9510565162951535312, 1.000000000000000000, 0.9510565162951535312, 1.000000000000000000, 0.9510565162951535312, 1.000000000000000000, 0.9510565162951535312, 1.000000000000000000 ) ) 
 REPRESENTATION_ITEM ( '' )  );
#22998 = EDGE_LOOP ( 'NONE', ( #3725, #10488, #24868, #26042 ) ) ;
#22999 = CARTESIAN_POINT ( 'NONE',  ( -87.35499999999998977, -4.716976649647093289, -6.492361379858945902 ) ) ;
#23000 = CARTESIAN_POINT ( 'NONE',  ( 9.058813317711338797, 127.9549999999999841, -2.943386871421372675 ) ) ;
#23001 = UNCERTAINTY_MEASURE_WITH_UNIT (LENGTH_MEASURE( 1.000000000000000082E-05 ), #60531, 'distance_accuracy_value', 'NONE');
#23002 = DIRECTION ( 'NONE',  ( -1.000000000000000000, 0.000000000000000000, -4.625929269271505635E-16 ) ) ;
#23003 = CARTESIAN_POINT ( 'NONE',  ( -92.60707362346617799, -8.102448949553174629, 5.886773742842742685 ) ) ;
#23004 = FACE_OUTER_BOUND ( 'NONE', #43747, .T. ) ;
#23005 =( NAMED_UNIT ( * ) SI_UNIT ( $, .STERADIAN. ) SOLID_ANGLE_UNIT ( ) );
#23006 = ORIENTED_EDGE ( 'NONE', *, *, #46837, .T. ) ;
#23007 = DIRECTION ( 'NONE',  ( 0.000000000000000000, 0.000000000000000000, 1.000000000000000000 ) ) ;
#23008 = FILL_AREA_STYLE_COLOUR ( '', #25037 ) ;
#23009 = CARTESIAN_POINT ( 'NONE',  ( -66.59499999999999886, 2.607480562269073321, 8.024999999999991473 ) ) ;
#23010 = ORIENTED_EDGE ( 'NONE', *, *, #63780, .F. ) ;
#23011 = STYLED_ITEM ( 'NONE', ( #15452 ), #27490 ) ;
#23012 = CARTESIAN_POINT ( 'NONE',  ( -49.49292637653378790, -8.102448949553174629, 5.886773742842742685 ) ) ;
#23013 = CARTESIAN_POINT ( 'NONE',  ( -45.66531550846541876, 8.455116999143502454, -6.464599779185706829 ) ) ;
#23014 = ORIENTED_EDGE ( 'NONE', *, *, #47577, .T. ) ;
#23015 = PRESENTATION_STYLE_ASSIGNMENT (( #26855 ) ) ;
#23016 = CARTESIAN_POINT ( 'NONE',  ( -52.04499999999998039, 7.632228543268600340, 2.479861379858949277 ) ) ;
#23017 = CARTESIAN_POINT ( 'NONE',  ( 22.99999999999995381, 5.000000000000000000, 32.00402776293825724 ) ) ;
#23018 = ORIENTED_EDGE ( 'NONE', *, *, #64732, .T. ) ;
#23019 = AXIS2_PLACEMENT_3D ( 'NONE', #64028, #43337, #53813 ) ;
#23020 = LINE ( 'NONE', #55360, #40440 ) ;
#23021 = CARTESIAN_POINT ( 'NONE',  ( -116.1550000000000011, 7.632228543268600340, 2.479861379858949277 ) ) ;
#23022 = ORIENTED_EDGE ( 'NONE', *, *, #8212, .T. ) ;
#23023 = CARTESIAN_POINT ( 'NONE',  ( 7.511572993685799101E-16, 2.500000000000000000, -6.999999999999997335 ) ) ;
#23024 = PRESENTATION_STYLE_ASSIGNMENT (( #49415 ) ) ;
#23025 = DIRECTION ( 'NONE',  ( 1.000000000000000000, -1.156482317317873451E-16, 0.000000000000000000 ) ) ;
#23026 = CIRCLE ( 'NONE', #62325, 1.000000000000000888 ) ;
#23027 = CARTESIAN_POINT ( 'NONE',  ( -146.1570736234662036, -9.058813317711329915, -2.943386871421370898 ) ) ;
#23028 = STYLED_ITEM ( 'NONE', ( #40059 ), #5800 ) ;
#23029 =( NAMED_UNIT ( * ) SI_UNIT ( $, .STERADIAN. ) SOLID_ANGLE_UNIT ( ) );
#23030 = CARTESIAN_POINT ( 'NONE',  ( -10.01517768586949408, 134.1949999999999932, -6.132527647946036459E-16 ) ) ;
#23031 = CARTESIAN_POINT ( 'NONE',  ( -86.60707362346619220, -8.102448949553172852, 5.886773742842742685 ) ) ;
#23032 = CARTESIAN_POINT ( 'NONE',  ( -53.18756747357344494, -10.02680648607920588, -3.499999999999314326 ) ) ;
#23033 = ORIENTED_EDGE ( 'NONE', *, *, #55827, .T. ) ;
#23034 = CIRCLE ( 'NONE', #17433, 0.9999999999999991118 ) ;
#23036 = SURFACE_STYLE_USAGE ( .BOTH. , #44865 ) ;
#23035 = SURFACE_STYLE_FILL_AREA ( #53981 ) ;
#23037 = FILL_AREA_STYLE_COLOUR ( '', #20899 ) ;
#23038 = AXIS2_PLACEMENT_3D ( 'NONE', #32305, #5555, #22451 ) ;
#23039 = CARTESIAN_POINT ( 'NONE',  ( -127.2550000000000097, -4.716976649647092401, 6.492361379858946790 ) ) ;
#23040 = FILL_AREA_STYLE_COLOUR ( '', #39266 ) ;
#23041 = CARTESIAN_POINT ( 'NONE',  ( -20.71231517720798010, 146.9999999999999716, 7.000000000000000000 ) ) ;
#23042 = CARTESIAN_POINT ( 'NONE',  ( -133.7949999999999875, 2.607480562269068880, -8.024999999999993250 ) ) ;
#23043 = MECHANICAL_DESIGN_GEOMETRIC_PRESENTATION_REPRESENTATION (  '', ( #47952 ), #1629 ) ;
#23044 = ADVANCED_FACE ( 'NONE', ( #17566 ), #39030, .F. ) ;
#23045 = CARTESIAN_POINT ( 'NONE',  ( -130.6449999999999818, 4.716976649647091513, -6.492361379858946790 ) ) ;
#23046 = ORIENTED_EDGE ( 'NONE', *, *, #41098, .T. ) ;
#23047 = EDGE_CURVE ( 'NONE', #39296, #13649, #10438, .T. ) ;
#23048 = CARTESIAN_POINT ( 'NONE',  ( -146.3070736234662093, -10.01517768586948698, 6.132527647946031529E-16 ) ) ;
#23049 = SURFACE_STYLE_USAGE ( .BOTH. , #5799 ) ;
#23050 =( NAMED_UNIT ( * ) SI_UNIT ( $, .STERADIAN. ) SOLID_ANGLE_UNIT ( ) );
#23051 = AXIS2_PLACEMENT_3D ( 'NONE', #29793, #56158, #55480 ) ;
#23052 = CARTESIAN_POINT ( 'NONE',  ( -178.6429263765338078, -5.598654528085801552, 7.705886871421367523 ) ) ;
#23053 = CARTESIAN_POINT ( 'NONE',  ( -58.79499999999998749, 2.607480562269068880, -8.024999999999993250 ) ) ;
#23054 = EDGE_CURVE ( 'NONE', #50331, #6652, #19410, .T. ) ;
#23055 = CARTESIAN_POINT ( 'NONE',  ( 55.89999999999999147, 11.99999999999999822, 3.499999999999992895 ) ) ;
#23056 = DIRECTION ( 'NONE',  ( 0.000000000000000000, 0.000000000000000000, 1.000000000000000000 ) ) ;
#23057 = ADVANCED_FACE ( 'NONE', ( #30489 ), #40392, .T. ) ;
#23058 = LINE ( 'NONE', #66293, #24485 ) ;
#23059 = SURFACE_STYLE_USAGE ( .BOTH. , #44888 ) ;
#23060 = CARTESIAN_POINT ( 'NONE',  ( -95.54292637653379927, 9.058813317711329915, 2.943386871421369566 ) ) ;
#23061 = APPLICATION_PROTOCOL_DEFINITION ( 'draft international standard', 'automotive_design', 1998, #32097 ) ;
#23062 = FILL_AREA_STYLE ('',( #28290 ) ) ;
#23063 = AXIS2_PLACEMENT_3D ( 'NONE', #20134, #25767, #42014 ) ;
#23064 = DIRECTION ( 'NONE',  ( -0.000000000000000000, -0.000000000000000000, 1.000000000000000000 ) ) ;
#23065 = VECTOR ( 'NONE', #36761, 1000.000000000000000 ) ;
#23066 = ADVANCED_FACE ( 'NONE', ( #56542 ), #67108, .F. ) ;
#23067 = CARTESIAN_POINT ( 'NONE',  ( 7.999999999999992895, 5.000000000000000000, 24.00402776293826079 ) ) ;
#23068 = CARTESIAN_POINT ( 'NONE',  ( -40.78947368421051323, 108.1536491499103505, 3.000000000000000444 ) ) ;
#23069 = EDGE_LOOP ( 'NONE', ( #52423, #27036, #55456, #28119 ) ) ;
#23070 = SURFACE_STYLE_FILL_AREA ( #65623 ) ;
#23071 = DIRECTION ( 'NONE',  ( -0.000000000000000000, 0.000000000000000000, -1.000000000000000000 ) ) ;
#23073 = ORIENTED_EDGE ( 'NONE', *, *, #11167, .F. ) ;
#23072 = VECTOR ( 'NONE', #51273, 1000.000000000000000 ) ;
#23074 =( LENGTH_UNIT ( ) NAMED_UNIT ( * ) SI_UNIT ( .MILLI., .METRE. ) );
#23075 = MECHANICAL_DESIGN_GEOMETRIC_PRESENTATION_REPRESENTATION (  '', ( #60119 ), #65743 ) ;
#23076 = CARTESIAN_POINT ( 'NONE',  ( 4.716976649647099507, 123.7570736234661695, -6.492361379858953008 ) ) ;
#23077 = CARTESIAN_POINT ( 'NONE',  ( 20.88905466131707200, 149.9999999999999432, 9.626351540309148191 ) ) ;
#23078 = CARTESIAN_POINT ( 'NONE',  ( -45.50000000000000000, 9.708372675170618749, 3.611004237778671744 ) ) ;
#23079 = CYLINDRICAL_SURFACE ( 'NONE', #56666, 0.2500000000000002220 ) ;
#23080 = ORIENTED_EDGE ( 'NONE', *, *, #47236, .T. ) ;
#23081 = DIRECTION ( 'NONE',  ( -1.000000000000000000, -0.000000000000000000, -0.000000000000000000 ) ) ;
#23082 = VECTOR ( 'NONE', #25397, 1000.000000000000000 ) ;
#23083 = SURFACE_STYLE_FILL_AREA ( #65974 ) ;
#23084 = ORIENTED_EDGE ( 'NONE', *, *, #60494, .F. ) ;
#23085 = CARTESIAN_POINT ( 'NONE',  ( -40.99999999999997868, 10.49999999999998224, 3.000000000000000000 ) ) ;
#23086 = DIRECTION ( 'NONE',  ( 0.000000000000000000, 0.000000000000000000, -1.000000000000000000 ) ) ;
#23087 =( GEOMETRIC_REPRESENTATION_CONTEXT ( 3 ) GLOBAL_UNCERTAINTY_ASSIGNED_CONTEXT ( ( #12290 ) ) GLOBAL_UNIT_ASSIGNED_CONTEXT ( ( #56295, #60203, #6721 ) ) REPRESENTATION_CONTEXT ( 'NONE', 'WORKASPACE' ) );
#23088 = CARTESIAN_POINT ( 'NONE',  ( 6.000000000000017764, -60.04052944165106709, -35.50000000000000000 ) ) ;
#23089 = CARTESIAN_POINT ( 'NONE',  ( -95.99499999999996191, -6.826472737025115478, 4.959722759717900331 ) ) ;
#23090 = ORIENTED_EDGE ( 'NONE', *, *, #5163, .F. ) ;
#23091 = VECTOR ( 'NONE', #56985, 1000.000000000000000 ) ;
#23092 = EDGE_CURVE ( 'NONE', #55156, #1652, #34403, .T. ) ;
#23093 = CARTESIAN_POINT ( 'NONE',  ( -74.99999999999998579, 50.00000000000000000, 10.00000000000000000 ) ) ;
#23094 = FILL_AREA_STYLE_COLOUR ( '', #22105 ) ;
#23095 = DIRECTION ( 'NONE',  ( 0.000000000000000000, 0.000000000000000000, -1.000000000000000000 ) ) ;
#23096 = CIRCLE ( 'NONE', #11829, 0.2500000000000002220 ) ;
#23097 = EDGE_LOOP ( 'NONE', ( #36243, #68586, #65373, #257 ) ) ;
#23098 = DIRECTION ( 'NONE',  ( 0.000000000000000000, 0.000000000000000000, -1.000000000000000000 ) ) ;
#23099 = CARTESIAN_POINT ( 'NONE',  ( -24.21231517720798010, 117.4999999999999716, -7.500000000000000000 ) ) ;
#23100 = SURFACE_SIDE_STYLE ('',( #12512 ) ) ;
#23101 = ORIENTED_EDGE ( 'NONE', *, *, #38244, .F. ) ;
#23102 = CARTESIAN_POINT ( 'NONE',  ( -8.082903768654761123, 1.417096231345241097, -1.759977097422839922E-15 ) ) ;
#23103 = ORIENTED_EDGE ( 'NONE', *, *, #1612, .T. ) ;
#23104 = CARTESIAN_POINT ( 'NONE',  ( -195.0000000000000000, 0.000000000000000000, 0.000000000000000000 ) ) ;
#23105 = CARTESIAN_POINT ( 'NONE',  ( 71.18918918918917882, 14.09971791521133255, -7.000000000000000000 ) ) ;
#23106 = SURFACE_STYLE_USAGE ( .BOTH. , #67386 ) ;
#23107 = SURFACE_SIDE_STYLE ('',( #11142 ) ) ;
#23108 = CARTESIAN_POINT ( 'NONE',  ( -177.2070736234661581, 3.094860106618433360, 9.524999999999991473 ) ) ;
#23109 = FILL_AREA_STYLE ('',( #44602 ) ) ;
#23110 = LINE ( 'NONE', #33990, #10573 ) ;
#23111 = CARTESIAN_POINT ( 'NONE',  ( -110.9070736234661609, -3.094860106618429807, 9.524999999999991473 ) ) ;
#23112 = AXIS2_PLACEMENT_3D ( 'NONE', #64280, #37256, #27660 ) ;
#23113 = CARTESIAN_POINT ( 'NONE',  ( -0.4573008633723372740, 9.000000000000007105, 0.008766315107681324145 ) ) ;
#23114 = LINE ( 'NONE', #44608, #54893 ) ;
#23115 = ORIENTED_EDGE ( 'NONE', *, *, #54007, .T. ) ;
#23116 = CARTESIAN_POINT ( 'NONE',  ( 7.632228543268608334, 122.3429263765338249, -2.479861379858951942 ) ) ;
#23117 = DIRECTION ( 'NONE',  ( -1.000000000000000000, 0.000000000000000000, 0.000000000000000000 ) ) ;
#23118 = SURFACE_STYLE_USAGE ( .BOTH. , #543 ) ;
#23119 = ADVANCED_FACE ( 'NONE', ( #55856 ), #7657, .F. ) ;
#23121 = SURFACE_STYLE_FILL_AREA ( #29411 ) ;
#23120 = VECTOR ( 'NONE', #41587, 1000.000000000000000 ) ;
#23122 = EDGE_LOOP ( 'NONE', ( #63547, #31960, #62009, #26553 ) ) ;
#23123 = CARTESIAN_POINT ( 'NONE',  ( -159.9549999999999841, -7.632228543268599452, 2.479861379858951054 ) ) ;
#23124 = EDGE_CURVE ( 'NONE', #23699, #34665, #17085, .T. ) ;
#23125 = DIRECTION ( 'NONE',  ( 0.000000000000000000, 0.000000000000000000, 1.000000000000000000 ) ) ;
#23126 = CARTESIAN_POINT ( 'NONE',  ( -184.0000000000000000, -8.446573402700972011, 1.153699593821606140 ) ) ;
#23127 = CARTESIAN_POINT ( 'NONE',  ( -175.6449999999999818, 4.716976649647091513, -6.492361379858946790 ) ) ;
#23128 = AXIS2_PLACEMENT_3D ( 'NONE', #32565, #60682, #1892 ) ;
#23129 = VECTOR ( 'NONE', #32654, 1000.000000000000000 ) ;
#23130 = CARTESIAN_POINT ( 'NONE',  ( -161.6949999999999932, -8.437984349512086979, 5.166775262442717831E-16 ) ) ;
#23131 = ORIENTED_EDGE ( 'NONE', *, *, #21590, .F. ) ;
#23132 = EDGE_CURVE ( 'NONE', #61898, #24543, #57237, .T. ) ;
#23133 = DIRECTION ( 'NONE',  ( 1.000000000000000000, 0.000000000000000000, 0.000000000000000000 ) ) ;
#23134 =( NAMED_UNIT ( * ) PLANE_ANGLE_UNIT ( ) SI_UNIT ( $, .RADIAN. ) );
#23135 = CARTESIAN_POINT ( 'NONE',  ( -75.05499999999997840, -9.827790563157499189E-16, -8.024999999999991473 ) ) ;
#23136 = CARTESIAN_POINT ( 'NONE',  ( -36.34584199317021103, -11.88577921580104579, 1.495499336507959853 ) ) ;
#23137 = AXIS2_PLACEMENT_3D ( 'NONE', #42661, #32753, #58455 ) ;
#23138 = CARTESIAN_POINT ( 'NONE',  ( -72.89499999999998181, 6.826472737025115478, 4.959722759717899443 ) ) ;
#23139 = CARTESIAN_POINT ( 'NONE',  ( 0.000000000000000000, 149.5550000000000068, -9.525000000000000355 ) ) ;
#23140 = CARTESIAN_POINT ( 'NONE',  ( -1.233556390963994831, 2.406758536253309710, -7.000000000000002665 ) ) ;
#23141 = STYLED_ITEM ( 'NONE', ( #5585 ), #58288 ) ;
#23142 = EDGE_CURVE ( 'NONE', #16451, #56993, #44214, .T. ) ;
#23143 = AXIS2_PLACEMENT_3D ( 'NONE', #67221, #3142, #35219 ) ;
#23144 = CARTESIAN_POINT ( 'NONE',  ( -176.0929263765339385, 3.094860106620248352, 9.524999999998673417 ) ) ;
#23145 = CIRCLE ( 'NONE', #5137, 3.100000000000000533 ) ;
#23146 = PRESENTATION_LAYER_ASSIGNMENT (  '', '', ( #5140 ) ) ;
#23147 = EDGE_CURVE ( 'NONE', #34665, #36214, #8015, .T. ) ;
#23148 = CARTESIAN_POINT ( 'NONE',  ( -60.00000000000000000, -2.024042244987997205E-14, 10.00000000000000000 ) ) ;
#23149 = CARTESIAN_POINT ( 'NONE',  ( -75.00000000000000000, 35.50862325381056905, -6.500000000000000888 ) ) ;
#23150 = DIRECTION ( 'NONE',  ( 0.000000000000000000, 1.000000000000000000, 0.000000000000000000 ) ) ;
#23151 = LINE ( 'NONE', #55836, #24968 ) ;
#23152 = VERTEX_POINT ( 'NONE', #30140 ) ;
#23153 = ORIENTED_EDGE ( 'NONE', *, *, #50141, .F. ) ;
#23154 =( NAMED_UNIT ( * ) PLANE_ANGLE_UNIT ( ) SI_UNIT ( $, .RADIAN. ) );
#23155 = LINE ( 'NONE', #53847, #66 ) ;
#23156 = AXIS2_PLACEMENT_3D ( 'NONE', #53983, #64196, #65236 ) ;
#23157 = CARTESIAN_POINT ( 'NONE',  ( 75.00000000000000000, -2.215169945516535778E-14, -7.000000000000000888 ) ) ;
#23158 = SURFACE_STYLE_FILL_AREA ( #17874 ) ;
#23159 = ORIENTED_EDGE ( 'NONE', *, *, #18068, .T. ) ;
#23160 = CARTESIAN_POINT ( 'NONE',  ( -111.0549999999999926, -9.827790563157499189E-16, -8.024999999999991473 ) ) ;
#23161 = VERTEX_POINT ( 'NONE', #61457 ) ;
#23162 = AXIS2_PLACEMENT_3D ( 'NONE', #29832, #9437, #26281 ) ;
#23163 = DIRECTION ( 'NONE',  ( 0.000000000000000000, -1.000000000000000000, 0.000000000000000000 ) ) ;
#23164 = CARTESIAN_POINT ( 'NONE',  ( 26.25000000000001066, 18.74999999999997868, -4.000000000000000000 ) ) ;
#23165 = ORIENTED_EDGE ( 'NONE', *, *, #59959, .F. ) ;
#23166 = CARTESIAN_POINT ( 'NONE',  ( -67.85707362346617799, -5.598654528085803328, -7.705886871421366635 ) ) ;
#23167 = ORIENTED_EDGE ( 'NONE', *, *, #58931, .T. ) ;
#23168 = PRESENTATION_LAYER_ASSIGNMENT (  '', '', ( #5166 ) ) ;
#23169 = AXIS2_PLACEMENT_3D ( 'NONE', #39722, #38358, #43629 ) ;
#23170 = DIRECTION ( 'NONE',  ( 0.000000000000000000, 0.000000000000000000, -1.000000000000000000 ) ) ;
#23171 = CARTESIAN_POINT ( 'NONE',  ( -48.50000000000000000, 14.49137674618942562, 10.00000000000000000 ) ) ;
#23172 = ORIENTED_EDGE ( 'NONE', *, *, #46096, .F. ) ;
#23173 = ADVANCED_FACE ( 'NONE', ( #34729 ), #35092, .T. ) ;
#23174 = EDGE_LOOP ( 'NONE', ( #6925, #62428, #34310, #42346 ) ) ;
#23175 = DIRECTION ( 'NONE',  ( -0.000000000000000000, -0.000000000000000000, 1.000000000000000000 ) ) ;
#23176 = CARTESIAN_POINT ( 'NONE',  ( -152.3070736234661524, -10.01517768586948698, 6.132527647946031529E-16 ) ) ;
#23177 =( LENGTH_UNIT ( ) NAMED_UNIT ( * ) SI_UNIT ( .MILLI., .METRE. ) );
#23178 = VERTEX_POINT ( 'NONE', #66767 ) ;
#23179 = CARTESIAN_POINT ( 'NONE',  ( -6.826472737025120807, 138.3929263765337794, -4.959722759717907437 ) ) ;
#23180 = LINE ( 'NONE', #6291, #1905 ) ;
#23181 = SURFACE_STYLE_FILL_AREA ( #27383 ) ;
#23182 = FACE_OUTER_BOUND ( 'NONE', #13138, .T. ) ;
#23183 = AXIS2_PLACEMENT_3D ( 'NONE', #36953, #58718, #10875 ) ;
#23184 = CARTESIAN_POINT ( 'NONE',  ( -8.437984349512095861, 114.6929263765338050, -5.166775262442723748E-16 ) ) ;
#23185 = VERTEX_POINT ( 'NONE', #40749 ) ;
#23186 =( NAMED_UNIT ( * ) SI_UNIT ( $, .STERADIAN. ) SOLID_ANGLE_UNIT ( ) );
#23187 = VERTEX_POINT ( 'NONE', #51625 ) ;
#23188 = CARTESIAN_POINT ( 'NONE',  ( -14.95322863490701870, 69.00000000000000000, -6.349999999999994316 ) ) ;
#23189 =( NAMED_UNIT ( * ) PLANE_ANGLE_UNIT ( ) SI_UNIT ( $, .RADIAN. ) );
#23190 = CARTESIAN_POINT ( 'NONE',  ( -129.6550000000000011, -7.632228543268600340, -2.479861379858950166 ) ) ;
#23191 = LINE ( 'NONE', #34423, #7240 ) ;
#23192 = VERTEX_POINT ( 'NONE', #24874 ) ;
#23193 = PRODUCT_RELATED_PRODUCT_CATEGORY ( 'part', '', ( #47375 ) ) ;
#23194 = EDGE_CURVE ( 'NONE', #23416, #54956, #13846, .T. ) ;
#23195 = CARTESIAN_POINT ( 'NONE',  ( -41.30760631258792870, -13.80057017807656550, 0.8185668606472049635 ) ) ;
#23196 = EDGE_CURVE ( 'NONE', #9969, #41177, #30538, .T. ) ;
#23197 = ORIENTED_EDGE ( 'NONE', *, *, #69263, .F. ) ;
#23198 = VERTEX_POINT ( 'NONE', #68860 ) ;
#23199 = CYLINDRICAL_SURFACE ( 'NONE', #11492, 9.524999999999991473 ) ;
#23200 = B_SPLINE_CURVE_WITH_KNOTS ( 'NONE', 3,
 ( #12039, #23636, #66559, #60556, #61596, #28896, #33838, #55300, #50055, #60916, #13081, #18383, #1788, #34890, #50384, #34535, #55993, #29251, #6413, #28189, #50734, #2478, #23988, #45502, #27845, #49347, #1433, #1069, #22611, #44115, #33501, #65514, #17364, #38830, #60244, #49697, #54932, #6760 ),
 .UNSPECIFIED., .F., .F.,
 ( 4, 2, 2, 2, 2, 2, 2, 2, 2, 2, 2, 2, 2, 2, 2, 2, 2, 2, 4 ),
 ( 3.576224061345498009E-18, 0.0009883658144282647922, 0.001976731628856526115, 0.002965097443284787221, 0.003953463257713048760, 0.004941829072141310300, 0.005930194886569570972, 0.006424377793783702176, 0.006918560700997832512, 0.007906926515426092317, 0.008895292329854354724, 0.009883658144282615396, 0.01087202395871087780, 0.01186038977313913674, 0.01284875558756739915, 0.01334293849478152862, 0.01383712140199565982, 0.01482548721642392743, 0.01581385303085219851 ),
 .UNSPECIFIED. ) ;
#23201 = CARTESIAN_POINT ( 'NONE',  ( -75.46551724137930250, 63.49197145334878201, 10.00000000000000000 ) ) ;
#23202 = EDGE_CURVE ( 'NONE', #36655, #8380, #36540, .T. ) ;
#23203 = PLANE ( 'NONE',  #20807 ) ;
#23204 = VERTEX_POINT ( 'NONE', #20662 ) ;
#23205 = SURFACE_STYLE_FILL_AREA ( #11948 ) ;
#23206 = EDGE_CURVE ( 'NONE', #10939, #56481, #42968, .T. ) ;
#23207 = DIRECTION ( 'NONE',  ( 0.000000000000000000, -0.3420201433256629953, -0.9396926207859104263 ) ) ;
#23208 = CARTESIAN_POINT ( 'NONE',  ( 55.89999999999999147, 11.99999999999999822, 3.499999999999992895 ) ) ;
#23209 = DIRECTION ( 'NONE',  ( 0.000000000000000000, 0.000000000000000000, -1.000000000000000000 ) ) ;
#23210 =( LENGTH_UNIT ( ) NAMED_UNIT ( * ) SI_UNIT ( .MILLI., .METRE. ) );
#23211 = ORIENTED_EDGE ( 'NONE', *, *, #22984, .T. ) ;
#23212 = EDGE_CURVE ( 'NONE', #41176, #67128, #4095, .T. ) ;
#23213 = CARTESIAN_POINT ( 'NONE',  ( -9.827790563157511022E-16, 116.5570736234661666, 8.025000000000000355 ) ) ;
#23214 = CARTESIAN_POINT ( 'NONE',  ( 5.374308355190992259, 154.5000000000000853, -7.876141323669411776 ) ) ;
#23215 = LINE ( 'NONE', #44708, #38220 ) ;
#23216 = PLANE ( 'NONE',  #58458 ) ;
#23217 = EDGE_CURVE ( 'NONE', #56838, #41529, #26601, .T. ) ;
#23218 = CARTESIAN_POINT ( 'NONE',  ( -95.69499999999997897, -8.437984349512086979, 5.166775262442717831E-16 ) ) ;
#23219 = CARTESIAN_POINT ( 'NONE',  ( 0.000000000000000000, 116.5549999999999926, -9.525000000000000355 ) ) ;
#23220 = STYLED_ITEM ( 'NONE', ( #10463 ), #3235 ) ;
#23221 = CARTESIAN_POINT ( 'NONE',  ( -77.99499999999997613, -6.826472737025115478, 4.959722759717900331 ) ) ;
#23222 = AXIS2_PLACEMENT_3D ( 'NONE', #52526, #57074, #68338 ) ;
#23223 = CARTESIAN_POINT ( 'NONE',  ( -147.4429263765338192, -1.166476076187852838E-15, -9.524999999999991473 ) ) ;
#23224 = DIRECTION ( 'NONE',  ( 1.000000000000000000, 0.000000000000000000, 0.000000000000000000 ) ) ;
#23225 = LINE ( 'NONE', #39777, #20463 ) ;
#23226 = SURFACE_STYLE_USAGE ( .BOTH. , #33761 ) ;
#23227 = DIRECTION ( 'NONE',  ( -0.000000000000000000, -0.000000000000000000, -1.000000000000000000 ) ) ;
#23228 = EDGE_LOOP ( 'NONE', ( #6456, #44079, #17295, #49637 ) ) ;
#23229 = CARTESIAN_POINT ( 'NONE',  ( -124.1929263765338192, -10.01517768586948698, 6.132527647946031529E-16 ) ) ;
#23230 = CARTESIAN_POINT ( 'NONE',  ( -140.3950000000000102, -6.826472737025115478, -4.959722759717899443 ) ) ;
#23231 = COLOUR_RGB ( '', 0.08235294, 0.09019608, 0.10196078) ;
#23232 = CARTESIAN_POINT ( 'NONE',  ( 1.999798566743339334, 49.09558629977726696, -2.000000000000000000 ) ) ;
#23233 = CARTESIAN_POINT ( 'NONE',  ( 5.000000000000000000, 6.123233995736766282E-16, 42.50000000000000000 ) ) ;
#23234 = ORIENTED_EDGE ( 'NONE', *, *, #4942, .T. ) ;
#23235 = VERTEX_POINT ( 'NONE', #52677 ) ;
#23236 = ADVANCED_FACE ( 'NONE', ( #47438 ), #42853, .F. ) ;
#23237 = DIRECTION ( 'NONE',  ( 5.782411586589351722E-16, -1.000000000000000000, 0.000000000000000000 ) ) ;
#23238 = CARTESIAN_POINT ( 'NONE',  ( -18.25000000000000711, 33.74999999999999289, -4.000000000000000000 ) ) ;
#23239 = MECHANICAL_DESIGN_GEOMETRIC_PRESENTATION_REPRESENTATION (  '', ( #5238 ), #60285 ) ;
#23240 = FACE_OUTER_BOUND ( 'NONE', #24280, .T. ) ;
#23241 = DIRECTION ( 'NONE',  ( -0.000000000000000000, 0.000000000000000000, -1.000000000000000000 ) ) ;
#23242 = SURFACE_STYLE_FILL_AREA ( #55231 ) ;
#23243 = ORIENTED_EDGE ( 'NONE', *, *, #24338, .F. ) ;
#23244 = CARTESIAN_POINT ( 'NONE',  ( -144.0549999999999784, -9.827790563157499189E-16, -8.024999999999991473 ) ) ;
#23245 = ORIENTED_EDGE ( 'NONE', *, *, #18557, .F. ) ;
#23246 = EDGE_LOOP ( 'NONE', ( #30056, #56312, #66769, #48932 ) ) ;
#23247 = DIRECTION ( 'NONE',  ( -1.000000000000000000, 0.000000000000000000, 0.000000000000000000 ) ) ;
#23248 = SURFACE_STYLE_FILL_AREA ( #55598 ) ;
#23249 = EDGE_LOOP ( 'NONE', ( #58729, #50686, #35837, #49628 ) ) ;
#23250 = CARTESIAN_POINT ( 'NONE',  ( 57.24999999999999289, 27.74999999999998934, 3.750000000000000000 ) ) ;
#23251 = CARTESIAN_POINT ( 'NONE',  ( 3.094860106618431583, 129.0949999999999704, 9.525000000000000355 ) ) ;
#23252 = CARTESIAN_POINT ( 'NONE',  ( 0.000000000000000000, -1.999999999999995337, 0.000000000000000000 ) ) ;
#23253 = ORIENTED_EDGE ( 'NONE', *, *, #52149, .T. ) ;
#23254 = DIRECTION ( 'NONE',  ( -1.000000000000000000, 0.000000000000000000, 0.000000000000000000 ) ) ;
#23255 = CARTESIAN_POINT ( 'NONE',  ( -9.058813317711338797, 141.4549999999999841, 2.943386871421373563 ) ) ;
#23256 = CARTESIAN_POINT ( 'NONE',  ( -53.30499999999998550, 8.437984349512086979, -1.550032578732815448E-15 ) ) ;
#23257 = PRODUCT_DEFINITION_SHAPE ( 'NONE', 'NONE',  #69696 ) ;
#23258 = ORIENTED_EDGE ( 'NONE', *, *, #52854, .T. ) ;
#23259 = CARTESIAN_POINT ( 'NONE',  ( -2.607480562269073765, 111.0929263765337964, -8.025000000000000355 ) ) ;
#23260 = CARTESIAN_POINT ( 'NONE',  ( 1.804495846578303864, 51.08602766979955589, 7.112547338523483198 ) ) ;
#23261 = AXIS2_PLACEMENT_3D ( 'NONE', #16566, #37696, #52804 ) ;
#23262 = FACE_OUTER_BOUND ( 'NONE', #61292, .T. ) ;
#23263 = CARTESIAN_POINT ( 'NONE',  ( -4.500000000000002665, 24.74999999999998579, 3.750000000000000000 ) ) ;
#23264 = COLOUR_RGB ( '', 0.40784314, 0.44705882, 0.49803922) ;
#23265 = EDGE_LOOP ( 'NONE', ( #67903, #66011, #57089, #1006 ) ) ;
#23266 = AXIS2_PLACEMENT_3D ( 'NONE', #61724, #25161, #13203 ) ;
#23267 = ORIENTED_EDGE ( 'NONE', *, *, #1609, .T. ) ;
#23268 = SURFACE_SIDE_STYLE ('',( #61243 ) ) ;
#23269 = FILL_AREA_STYLE_COLOUR ( '', #60348 ) ;
#23270 = DIRECTION ( 'NONE',  ( 1.000000000000000000, 9.376883653928660246E-17, 0.000000000000000000 ) ) ;
#23271 = CARTESIAN_POINT ( 'NONE',  ( -159.0550000000000068, -9.827790563157499189E-16, -8.024999999999991473 ) ) ;
#23272 = ORIENTED_EDGE ( 'NONE', *, *, #44790, .T. ) ;
#23273 = SURFACE_STYLE_USAGE ( .BOTH. , #51052 ) ;
#23274 = ADVANCED_FACE ( 'NONE', ( #57958 ), #30849, .T. ) ;
#23275 = LINE ( 'NONE', #26024, #49592 ) ;
#23276 = CARTESIAN_POINT ( 'NONE',  ( -74.99999999999998579, 50.00000000000000000, -9.500000000000000000 ) ) ;
#23277 =( BOUNDED_CURVE ( )  B_SPLINE_CURVE ( 3, ( #4731, #68418, #41714, #4356 ),
 .UNSPECIFIED., .F., .F. ) 
 B_SPLINE_CURVE_WITH_KNOTS ( ( 4, 4 ),
 ( 1.649859741910239874, 3.741551587622924835 ),
 .UNSPECIFIED. ) 
 CURVE ( )  GEOMETRIC_REPRESENTATION_ITEM ( )  RATIONAL_B_SPLINE_CURVE ( ( 1.000000000000000000, 0.6674467249320013007, 0.6674467249320013007, 1.000000000000000000 ) ) 
 REPRESENTATION_ITEM ( '' )  );
#23278 = ORIENTED_EDGE ( 'NONE', *, *, #58442, .F. ) ;
#23279 = VERTEX_POINT ( 'NONE', #15410 ) ;
#23280 = CARTESIAN_POINT ( 'NONE',  ( -11.00000000000000000, 8.000000000000000000, 3.500000000000003997 ) ) ;
#23281 = AXIS2_PLACEMENT_3D ( 'NONE', #57149, #47005, #14973 ) ;
#23282 = EDGE_CURVE ( 'NONE', #61605, #62693, #22839, .T. ) ;
#23283 = CARTESIAN_POINT ( 'NONE',  ( -75.80499999999997840, -8.437984349512085203, 5.166775262442717831E-16 ) ) ;
#23284 = VERTEX_POINT ( 'NONE', #25564 ) ;
#23285 = FACE_OUTER_BOUND ( 'NONE', #59651, .T. ) ;
#23286 = SURFACE_STYLE_FILL_AREA ( #55286 ) ;
#23287 = CARTESIAN_POINT ( 'NONE',  ( -54.50000000000002132, -1.956686671034893189E-14, -12.00000000000000000 ) ) ;
#23288 = CARTESIAN_POINT ( 'NONE',  ( 8.750000000000001776, 25.24999999999998934, -4.000000000000000000 ) ) ;
#23289 = ORIENTED_EDGE ( 'NONE', *, *, #55750, .F. ) ;
#23290 = CARTESIAN_POINT ( 'NONE',  ( 22.99999999999996447, 0.000000000000000000, 29.00402776293825369 ) ) ;
#23292 = CARTESIAN_POINT ( 'NONE',  ( 4.041451884327375232, -1.417096231345241097, -7.000000000000002665 ) ) ;
#23291 = CARTESIAN_POINT ( 'NONE',  ( -52.85707362346617089, -5.598654528085803328, -7.705886871421366635 ) ) ;
#23293 = EDGE_CURVE ( 'NONE', #52976, #1567, #62131, .T. ) ;
#23294 = CARTESIAN_POINT ( 'NONE',  ( 8.102448949553181734, 129.3949999999999818, 5.886773742842750679 ) ) ;
#23295 = CARTESIAN_POINT ( 'NONE',  ( -104.5449999999999875, -7.632228543268600340, -2.479861379858950166 ) ) ;
#23296 = CARTESIAN_POINT ( 'NONE',  ( -15.00000000000000000, 8.000000000000000000, 3.500000000000003997 ) ) ;
#23298 = LINE ( 'NONE', #34205, #37068 ) ;
#23297 = FACE_OUTER_BOUND ( 'NONE', #65079, .T. ) ;
#23299 = CARTESIAN_POINT ( 'NONE',  ( -151.0429263765337851, -9.058813317711329915, -2.943386871421370898 ) ) ;
#23300 = SHAPE_REPRESENTATION_RELATIONSHIP ( 'NONE' , 'NONE' ,  #14558, #41398 ) ;
#23301 = CARTESIAN_POINT ( 'NONE',  ( -167.3949999999999534, -6.826472737025115478, -4.959722759717899443 ) ) ;
#23302 = CIRCLE ( 'NONE', #62606, 16.50000000000000000 ) ;
#23303 = B_SPLINE_CURVE_WITH_KNOTS ( 'NONE', 3,
 ( #63663, #37679, #59077, #10894, #32335, #27035 ),
 .UNSPECIFIED., .F., .F.,
 ( 4, 2, 4 ),
 ( 0.004189585287972439308, 0.006269578072783813308, 0.008349570857595188175 ),
 .UNSPECIFIED. ) ;
#23304 = EDGE_CURVE ( 'NONE', #49636, #64569, #59721, .T. ) ;
#23305 = DIRECTION ( 'NONE',  ( -1.000000000000000000, 0.000000000000000000, 0.000000000000000000 ) ) ;
#23306 = VERTEX_POINT ( 'NONE', #69201 ) ;
#23307 = CARTESIAN_POINT ( 'NONE',  ( -9.908575283019910450E-16, -6.500000000000000888, 0.000000000000000000 ) ) ;
#23308 = ORIENTED_EDGE ( 'NONE', *, *, #13481, .T. ) ;
#23309 = CARTESIAN_POINT ( 'NONE',  ( -63.59292637653378932, -3.094860106618431139, -9.524999999999991473 ) ) ;
#23310 = EDGE_CURVE ( 'NONE', #21071, #38290, #37343, .T. ) ;
#23311 = SURFACE_SIDE_STYLE ('',( #50070 ) ) ;
#23312 = CARTESIAN_POINT ( 'NONE',  ( 0.08961491207241870094, 42.48853761352472702, 74.70442652852922549 ) ) ;
#23313 = CARTESIAN_POINT ( 'NONE',  ( 27.00000000000001776, 43.00000000000000000, 36.50000000000000000 ) ) ;
#23314 = AXIS2_PLACEMENT_3D ( 'NONE', #3613, #41323, #3259 ) ;
#23315 = CARTESIAN_POINT ( 'NONE',  ( -4.041451884327380562, 1.417096231345237545, -7.000000000000003553 ) ) ;
#23316 = AXIS2_PLACEMENT_3D ( 'NONE', #46851, #67202, #66875 ) ;
#23317 = VERTEX_POINT ( 'NONE', #53370 ) ;
#23318 = CARTESIAN_POINT ( 'NONE',  ( -170.7549999999999955, 4.716976649647091513, -6.492361379858946790 ) ) ;
#23319 = ORIENTED_EDGE ( 'NONE', *, *, #16562, .F. ) ;
#23320 = CARTESIAN_POINT ( 'NONE',  ( 48.00000000000000000, 14.49137674618942562, -7.500000000000000000 ) ) ;
#23321 = CARTESIAN_POINT ( 'NONE',  ( -15.98999599679679839, 146.4999999999999716, 9.500000000000000000 ) ) ;
#23322 = B_SPLINE_CURVE_WITH_KNOTS ( 'NONE', 3,
 ( #15678, #41383, #57534, #31474, #25510, #57895, #63504, #51921, #52960, #4749 ),
 .UNSPECIFIED., .F., .F.,
 ( 4, 2, 2, 2, 4 ),
 ( 0.000000000000000000, 0.0004706383985570308597, 0.0009412767971140617194, 0.001411915195671093392, 0.001882553594228125174 ),
 .UNSPECIFIED. ) ;
#23323 = DIRECTION ( 'NONE',  ( 0.000000000000000000, 0.000000000000000000, 1.000000000000000000 ) ) ;
#23324 = CARTESIAN_POINT ( 'NONE',  ( 7.632228543268607446, 156.1570736234661467, 2.479861379858954606 ) ) ;
#23325 = ORIENTED_EDGE ( 'NONE', *, *, #11988, .T. ) ;
#23326 =( NAMED_UNIT ( * ) SI_UNIT ( $, .STERADIAN. ) SOLID_ANGLE_UNIT ( ) );
#23327 = CARTESIAN_POINT ( 'NONE',  ( 0.000000000000000000, -2.500000000000000000, -5.500000000000005329 ) ) ;
#23328 = CARTESIAN_POINT ( 'NONE',  ( -85.25499999999998124, -4.716976649647092401, 6.492361379858946790 ) ) ;
#23329 = DIRECTION ( 'NONE',  ( 0.000000000000000000, -1.000000000000000000, 0.000000000000000000 ) ) ;
#23330 = CARTESIAN_POINT ( 'NONE',  ( -5.598654528085806881, 125.8549999999999898, -7.705886871421374629 ) ) ;
#23331 = CARTESIAN_POINT ( 'NONE',  ( -127.1929263765338192, -10.01517768586948698, 6.132527647946031529E-16 ) ) ;
#23332 = CARTESIAN_POINT ( 'NONE',  ( 41.49999999999998579, 106.9282032302754999, -3.500000000000000000 ) ) ;
#23333 = EDGE_CURVE ( 'NONE', #46369, #16845, #29387, .T. ) ;
#23334 = CARTESIAN_POINT ( 'NONE',  ( -74.99999999999998579, 113.4999999999999858, 7.000000000000000000 ) ) ;
#23335 = ORIENTED_EDGE ( 'NONE', *, *, #15292, .F. ) ;
#23336 =( LENGTH_UNIT ( ) NAMED_UNIT ( * ) SI_UNIT ( .MILLI., .METRE. ) );
#23337 = CARTESIAN_POINT ( 'NONE',  ( -52.49499999999999034, 6.826472737025113702, -4.959722759717902107 ) ) ;
#23338 = EDGE_LOOP ( 'NONE', ( #10173, #20886, #22937, #9961 ) ) ;
#23339 = CARTESIAN_POINT ( 'NONE',  ( -75.00000000000000000, -2.215169945516535778E-14, -9.500000000000000000 ) ) ;
#23340 = CARTESIAN_POINT ( 'NONE',  ( -45.91547276418385337, 9.430195785006416642, -6.025268399887218074 ) ) ;
#23341 = AXIS2_PLACEMENT_3D ( 'NONE', #41944, #15536, #57737 ) ;
#23342 = DIRECTION ( 'NONE',  ( 8.881784197001252323E-16, 0.000000000000000000, 1.000000000000000000 ) ) ;
#23343 = ORIENTED_EDGE ( 'NONE', *, *, #67271, .T. ) ;
#23344 = CARTESIAN_POINT ( 'NONE',  ( -57.44499999999999318, 0.000000000000000000, 8.024999999999991473 ) ) ;
#23345 = EDGE_LOOP ( 'NONE', ( #13340, #52077, #24353, #40554 ) ) ;
#23346 = VECTOR ( 'NONE', #65561, 1000.000000000000000 ) ;
#23347 = AXIS2_PLACEMENT_3D ( 'NONE', #50542, #61076, #25184 ) ;
#23349 = ADVANCED_FACE ( 'NONE', ( #17808 ), #43208, .T. ) ;
#23348 = CARTESIAN_POINT ( 'NONE',  ( -75.00000000000000000, 9.708372641349372500, 6.050536800209464161 ) ) ;
#23350 = CARTESIAN_POINT ( 'NONE',  ( -113.1549999999999869, 7.632228543268600340, 2.479861379858949277 ) ) ;
#23351 = ORIENTED_EDGE ( 'NONE', *, *, #54620, .T. ) ;
#23352 = CARTESIAN_POINT ( 'NONE',  ( -4.716976649647098618, 119.2570736234661553, 6.492361379858953008 ) ) ;
#23353 = CARTESIAN_POINT ( 'NONE',  ( 17.00000000000000711, 25.24999999999998224, 3.750000000000000000 ) ) ;
#23354 = VECTOR ( 'NONE', #28287, 1000.000000000000000 ) ;
#23355 = CARTESIAN_POINT ( 'NONE',  ( -152.6070736234661354, -8.102448949553172852, 5.886773742842742685 ) ) ;
#23356 = EDGE_CURVE ( 'NONE', #26455, #3143, #17483, .T. ) ;
#23357 = DIRECTION ( 'NONE',  ( -0.000000000000000000, -1.000000000000000000, -0.000000000000000000 ) ) ;
#23358 = CARTESIAN_POINT ( 'NONE',  ( 8.102448949553179958, 144.3949999999999818, 5.886773742842750679 ) ) ;
#23359 = CARTESIAN_POINT ( 'NONE',  ( -85.55707362346618083, -1.166476076187852838E-15, -9.524999999999991473 ) ) ;
#23360 = EDGE_CURVE ( 'NONE', #43611, #11506, #40676, .T. ) ;
#23361 = EDGE_LOOP ( 'NONE', ( #14904, #4025, #35360 ) ) ;
#23362 = AXIS2_PLACEMENT_3D ( 'NONE', #34204, #18018, #12732 ) ;
#23364 = CARTESIAN_POINT ( 'NONE',  ( -44.99999999999998579, 119.9999999999999716, -9.500000000000000000 ) ) ;
#23363 = DIRECTION ( 'NONE',  ( -0.000000000000000000, -0.000000000000000000, 1.000000000000000000 ) ) ;
#23365 = DIRECTION ( 'NONE',  ( 1.000000000000000000, -0.000000000000000000, -1.300977106640434891E-16 ) ) ;
#23367 = ADVANCED_FACE ( 'NONE', ( #60688 ), #37922, .T. ) ;
#23366 = PRESENTATION_LAYER_ASSIGNMENT (  '', '', ( #3076 ) ) ;
#23368 = CARTESIAN_POINT ( 'NONE',  ( -126.3549999999999898, -4.716976649647093289, -6.492361379858945902 ) ) ;
#23369 = CARTESIAN_POINT ( 'NONE',  ( 61.99999999999998579, 30.74999999999999289, -3.750000000000000000 ) ) ;
#23370 =( NAMED_UNIT ( * ) SI_UNIT ( $, .STERADIAN. ) SOLID_ANGLE_UNIT ( ) );
#23371 = CARTESIAN_POINT ( 'NONE',  ( -137.2450000000000045, -4.716976649647093289, -6.492361379858945902 ) ) ;
#23372 = CARTESIAN_POINT ( 'NONE',  ( -126.2949999999999875, -2.607480562269069768, 8.024999999999991473 ) ) ;
#23373 = DIRECTION ( 'NONE',  ( 0.000000000000000000, 1.000000000000000000, 0.000000000000000000 ) ) ;
#23374 = ORIENTED_EDGE ( 'NONE', *, *, #35683, .T. ) ;
#23375 = CARTESIAN_POINT ( 'NONE',  ( -145.7070736234666413, -3.094860106626094787, -9.524999999994424371 ) ) ;
#23376 = FILL_AREA_STYLE_COLOUR ( '', #26653 ) ;
#23377 = CARTESIAN_POINT ( 'NONE',  ( -74.99999999999998579, 64.49137674618943095, 10.00000000000000000 ) ) ;
#23378 = CARTESIAN_POINT ( 'NONE',  ( -182.0929263765337964, 3.094860106618433360, 9.524999999999991473 ) ) ;
#23379 = CARTESIAN_POINT ( 'NONE',  ( -46.94499999999998607, -9.827790563157499189E-16, -8.024999999999991473 ) ) ;
#23380 =( NAMED_UNIT ( * ) PLANE_ANGLE_UNIT ( ) SI_UNIT ( $, .RADIAN. ) );
#23381 = CARTESIAN_POINT ( 'NONE',  ( -60.00000000000000000, -2.024042244987997205E-14, -10.00000000000000000 ) ) ;
#23382 = AXIS2_PLACEMENT_3D ( 'NONE', #10951, #4627, #25732 ) ;
#23383 = CARTESIAN_POINT ( 'NONE',  ( 10.00000000000001954, 43.00000000000000000, 45.61250543006183733 ) ) ;
#23384 = PLANE ( 'NONE',  #57450 ) ;
#23385 = CARTESIAN_POINT ( 'NONE',  ( -98.99292637653378790, 8.102448949553171076, -5.886773742842744461 ) ) ;
#23386 = PRODUCT_CONTEXT ( 'NONE', #37069, 'mechanical' ) ;
#23387 = CARTESIAN_POINT ( 'NONE',  ( 0.000000000000000000, 0.000000000000000000, 4.000000000000000000 ) ) ;
#23388 =( BOUNDED_CURVE ( )  B_SPLINE_CURVE ( 2, ( #5311, #43380, #58803, #59129, #26757, #63386, #26430, #47962, #67545, #53855, #27103 ),
 .UNSPECIFIED., .F., .F. ) 
 B_SPLINE_CURVE_WITH_KNOTS ( ( 3, 2, 2, 2, 2, 3 ),
 ( 0.2934782608695583606, 0.2956521739130365534, 0.2978260869565147462, 0.2999999999999929945, 0.3021739130434711873, 0.3043478260869494356 ),
 .UNSPECIFIED. ) 
 CURVE ( )  GEOMETRIC_REPRESENTATION_ITEM ( )  RATIONAL_B_SPLINE_CURVE ( ( 1.000000000000154987, 0.9510565162949985440, 1.000000000000000000, 0.9510565162951535312, 1.000000000000000000, 0.9510565162951535312, 1.000000000000000000, 0.9510565162951535312, 1.000000000000000000, 0.9510565162953135143, 0.9999999999998400169 ) ) 
 REPRESENTATION_ITEM ( '' )  );
#23389 = CARTESIAN_POINT ( 'NONE',  ( -162.3570736234661922, 5.598654528085804216, 7.705886871421366635 ) ) ;
#23390 = DIRECTION ( 'NONE',  ( -0.000000000000000000, -0.000000000000000000, -1.000000000000000000 ) ) ;
#23391 = SURFACE_STYLE_USAGE ( .BOTH. , #34304 ) ;
#23392 = ORIENTED_EDGE ( 'NONE', *, *, #17807, .T. ) ;
#23393 = CARTESIAN_POINT ( 'NONE',  ( -57.09597854763558900, -7.829934782661390535, -1.044957726401560594 ) ) ;
#23394 = ORIENTED_EDGE ( 'NONE', *, *, #61417, .T. ) ;
#23395 = DIRECTION ( 'NONE',  ( 1.000000000000000000, 0.000000000000000000, -0.000000000000000000 ) ) ;
#23396 = AXIS2_PLACEMENT_3D ( 'NONE', #61014, #12830, #7558 ) ;
#23397 = CARTESIAN_POINT ( 'NONE',  ( -6.826472737025120807, 119.1070736234661496, 4.959722759717906548 ) ) ;
#23398 =( GEOMETRIC_REPRESENTATION_CONTEXT ( 3 ) GLOBAL_UNCERTAINTY_ASSIGNED_CONTEXT ( ( #45273 ) ) GLOBAL_UNIT_ASSIGNED_CONTEXT ( ( #26609, #42863, #53380 ) ) REPRESENTATION_CONTEXT ( 'NONE', 'WORKASPACE' ) );
#23399 = DIRECTION ( 'NONE',  ( 0.000000000000000000, 0.000000000000000000, -1.000000000000000000 ) ) ;
#23400 =( NAMED_UNIT ( * ) PLANE_ANGLE_UNIT ( ) SI_UNIT ( $, .RADIAN. ) );
#23401 = PRESENTATION_LAYER_ASSIGNMENT (  '', '', ( #30121 ) ) ;
#23402 =( NAMED_UNIT ( * ) SI_UNIT ( $, .STERADIAN. ) SOLID_ANGLE_UNIT ( ) );
#23403 = ORIENTED_EDGE ( 'NONE', *, *, #35040, .T. ) ;
#23404 = DIRECTION ( 'NONE',  ( -1.239088197126290817E-16, 0.000000000000000000, -1.000000000000000000 ) ) ;
#23405 = CARTESIAN_POINT ( 'NONE',  ( 0.000000000000000000, 152.9999999999999716, 0.000000000000000000 ) ) ;
#23406 = EDGE_CURVE ( 'NONE', #67825, #7755, #8887, .T. ) ;
#23407 = CARTESIAN_POINT ( 'NONE',  ( 13.75000000000000533, 30.74999999999999289, 3.750000000000000000 ) ) ;
#23408 = CARTESIAN_POINT ( 'NONE',  ( -90.59499999999999886, 2.607480562269073321, 8.024999999999991473 ) ) ;
#23409 = EDGE_LOOP ( 'NONE', ( #632, #46994 ) ) ;
#23410 = EDGE_CURVE ( 'NONE', #48589, #39136, #67617, .T. ) ;
#23411 = DIRECTION ( 'NONE',  ( 0.000000000000000000, 0.000000000000000000, 1.000000000000000000 ) ) ;
#23412 = EDGE_CURVE ( 'NONE', #58654, #62684, #24926, .T. ) ;
#23413 = DIRECTION ( 'NONE',  ( 0.000000000000000000, 0.000000000000000000, 1.000000000000000000 ) ) ;
#23414 = CARTESIAN_POINT ( 'NONE',  ( -44.50000000000000000, 99.99999999999998579, 4.000000000000000000 ) ) ;
#23415 = AXIS2_PLACEMENT_3D ( 'NONE', #21123, #4587, #68989 ) ;
#23416 = VERTEX_POINT ( 'NONE', #44580 ) ;
#23417 =( LENGTH_UNIT ( ) NAMED_UNIT ( * ) SI_UNIT ( .MILLI., .METRE. ) );
#23418 = EDGE_CURVE ( 'NONE', #12977, #41202, #159, .T. ) ;
#23419 = CARTESIAN_POINT ( 'NONE',  ( 3.000000000000002665, 43.00000000000000000, -90.00000000000000000 ) ) ;
#23420 = EDGE_CURVE ( 'NONE', #26152, #52352, #37391, .T. ) ;
#23421 = VERTEX_POINT ( 'NONE', #49823 ) ;
#23422 = DIRECTION ( 'NONE',  ( 0.000000000000000000, 0.000000000000000000, 1.000000000000000000 ) ) ;
#23423 = EDGE_CURVE ( 'NONE', #13722, #34864, #60921, .T. ) ;
#23424 = ORIENTED_EDGE ( 'NONE', *, *, #50588, .T. ) ;
#23425 = CARTESIAN_POINT ( 'NONE',  ( -15.00000000000000000, -12.00000000000000000, 0.000000000000000000 ) ) ;
#23426 = STYLED_ITEM ( 'NONE', ( #48549 ), #10344 ) ;
#23427 = CARTESIAN_POINT ( 'NONE',  ( -176.6070736234661354, -8.102448949553172852, 5.886773742842742685 ) ) ;
#23428 = EDGE_CURVE ( 'NONE', #46008, #42263, #840, .T. ) ;
#23429 = CYLINDRICAL_SURFACE ( 'NONE', #15189, 0.5000000000000004441 ) ;
#23430 = DIRECTION ( 'NONE',  ( -0.5000000000000003331, -0.8660254037844384856, 0.000000000000000000 ) ) ;
#23431 = CIRCLE ( 'NONE', #57127, 18.00000000000000355 ) ;
#23432 = CARTESIAN_POINT ( 'NONE',  ( -116.7570736234661695, -5.598654528085801552, 7.705886871421367523 ) ) ;
#23433 = DIRECTION ( 'NONE',  ( 0.000000000000000000, 0.000000000000000000, 1.000000000000000000 ) ) ;
#23434 = EDGE_CURVE ( 'NONE', #69376, #582, #36277, .T. ) ;
#23435 = CARTESIAN_POINT ( 'NONE',  ( -23.21231517720797655, 118.4999999999999716, 7.000000000000000000 ) ) ;
#23436 = ORIENTED_EDGE ( 'NONE', *, *, #61615, .F. ) ;
#23437 = CARTESIAN_POINT ( 'NONE',  ( -74.99999999999998579, 50.00000000000000000, -6.499999999999999112 ) ) ;
#23438 = AXIS2_PLACEMENT_3D ( 'NONE', #50045, #2829, #40184 ) ;
#23439 = SURFACE_STYLE_FILL_AREA ( #55094 ) ;
#23440 = DIRECTION ( 'NONE',  ( 1.000000000000000000, 0.000000000000000000, 0.000000000000000000 ) ) ;
#23441 = SURFACE_SIDE_STYLE ('',( #23121 ) ) ;
#23442 = ORIENTED_EDGE ( 'NONE', *, *, #49174, .F. ) ;
#23443 = CARTESIAN_POINT ( 'NONE',  ( -163.8549999999999898, 4.716976649647094177, 6.492361379858945902 ) ) ;
#23444 = DIRECTION ( 'NONE',  ( 1.000000000000000000, -4.336808689941999001E-16, 0.000000000000000000 ) ) ;
#23445 = CARTESIAN_POINT ( 'NONE',  ( -160.1950000000000216, 8.437984349512085203, -1.550032578732815448E-15 ) ) ;
#23446 = AXIS2_PLACEMENT_3D ( 'NONE', #51573, #15365, #56857 ) ;
#23447 = CARTESIAN_POINT ( 'NONE',  ( -153.7450000000000045, 4.716976649647094177, 6.492361379858945902 ) ) ;
#23448 = ORIENTED_EDGE ( 'NONE', *, *, #24389, .T. ) ;
#23449 = CARTESIAN_POINT ( 'NONE',  ( -9.984889265949535186, 0.7056644834263136046, 0.9848892659495233071 ) ) ;
#23450 = FILL_AREA_STYLE_COLOUR ( '', #64909 ) ;
#23451 = CARTESIAN_POINT ( 'NONE',  ( 9.984889265949528081, -1.515110734050476582, -0.7056644834263100519 ) ) ;
#23452 = CARTESIAN_POINT ( 'NONE',  ( -72.95499999999999829, -7.632228543268599452, 2.479861379858951054 ) ) ;
#23453 = CARTESIAN_POINT ( 'NONE',  ( -24.21231517720798010, 113.4999999999999858, -10.00000000000000000 ) ) ;
#23455 =( NAMED_UNIT ( * ) SI_UNIT ( $, .STERADIAN. ) SOLID_ANGLE_UNIT ( ) );
#23454 = CIRCLE ( 'NONE', #30169, 0.5000000000000004441 ) ;
#23456 = CARTESIAN_POINT ( 'NONE',  ( -69.44499999999999318, 0.000000000000000000, 8.024999999999991473 ) ) ;
#23457 = CARTESIAN_POINT ( 'NONE',  ( 0.000000000000000000, 143.5549999999999784, -9.525000000000000355 ) ) ;
#23458 = DIRECTION ( 'NONE',  ( -1.000000000000000000, 0.000000000000000000, 0.000000000000000000 ) ) ;
#23459 = CARTESIAN_POINT ( 'NONE',  ( 3.906371588341139400, 154.3107745167562825, 8.486918976161017980 ) ) ;
#23460 = UNCERTAINTY_MEASURE_WITH_UNIT (LENGTH_MEASURE( 1.000000000000000082E-05 ), #45731, 'distance_accuracy_value', 'NONE');
#23461 = EDGE_CURVE ( 'NONE', #42583, #12229, #61878, .T. ) ;
#23462 = DIRECTION ( 'NONE',  ( 0.000000000000000000, 1.000000000000000000, 0.000000000000000000 ) ) ;
#23463 = VECTOR ( 'NONE', #21733, 1000.000000000000000 ) ;
#23464 =( NAMED_UNIT ( * ) PLANE_ANGLE_UNIT ( ) SI_UNIT ( $, .RADIAN. ) );
#23465 = CARTESIAN_POINT ( 'NONE',  ( 60.00000000000000000, -2.024042244987997205E-14, 9.500000000000000000 ) ) ;
#23466 = AXIS2_PLACEMENT_3D ( 'NONE', #28258, #17760, #34270 ) ;
#23467 = CARTESIAN_POINT ( 'NONE',  ( 25.75000000000001066, 21.74999999999998224, 4.000000000000000000 ) ) ;
#23468 = AXIS2_PLACEMENT_3D ( 'NONE', #12987, #34444, #24560 ) ;
#23469 = DIRECTION ( 'NONE',  ( -1.000000000000000000, 0.000000000000000000, 0.000000000000000000 ) ) ;
#23470 = ORIENTED_EDGE ( 'NONE', *, *, #46764, .F. ) ;
#23471 = AXIS2_PLACEMENT_3D ( 'NONE', #38340, #1284, #5921 ) ;
#23472 = ORIENTED_EDGE ( 'NONE', *, *, #27364, .F. ) ;
#23473 = FACE_OUTER_BOUND ( 'NONE', #62378, .T. ) ;
#23475 = VECTOR ( 'NONE', #11411, 1000.000000000000000 ) ;
#23474 = CARTESIAN_POINT ( 'NONE',  ( -132.0570736234661808, 0.000000000000000000, 9.524999999999991473 ) ) ;
#23476 = FACE_OUTER_BOUND ( 'NONE', #5909, .T. ) ;
#23477 = SURFACE_SIDE_STYLE ('',( #6963 ) ) ;
#23478 = MECHANICAL_DESIGN_GEOMETRIC_PRESENTATION_REPRESENTATION (  '', ( #57181 ), #30203 ) ;
#23479 = CARTESIAN_POINT ( 'NONE',  ( 4.041451884327379673, -7.000000000000002665, 1.082903768654758903 ) ) ;
#23480 = FACE_OUTER_BOUND ( 'NONE', #62058, .T. ) ;
#23481 = ORIENTED_EDGE ( 'NONE', *, *, #43890, .F. ) ;
#23482 = CARTESIAN_POINT ( 'NONE',  ( -98.75499999999999545, 4.716976649647091513, -6.492361379858946790 ) ) ;
#23483 = ORIENTED_EDGE ( 'NONE', *, *, #43529, .F. ) ;
#23484 = LINE ( 'NONE', #33362, #28665 ) ;
#23485 = EDGE_CURVE ( 'NONE', #7596, #69443, #18358, .T. ) ;
#23486 = VERTEX_POINT ( 'NONE', #12863 ) ;
#23487 = ORIENTED_EDGE ( 'NONE', *, *, #6431, .F. ) ;
#23488 = COLOUR_RGB ( '', 0.72549020, 0.75294118, 0.79215686) ;
#23489 = ORIENTED_EDGE ( 'NONE', *, *, #44446, .F. ) ;
#23490 = AXIS2_PLACEMENT_3D ( 'NONE', #9287, #30705, #68368 ) ;
#23491 = ADVANCED_FACE ( 'NONE', ( #51208 ), #34652, .T. ) ;
#23492 = ORIENTED_EDGE ( 'NONE', *, *, #65183, .F. ) ;
#23493 = CARTESIAN_POINT ( 'NONE',  ( 61.74999999999998579, 30.99999999999999289, -3.750000000000000000 ) ) ;
#23494 = CARTESIAN_POINT ( 'NONE',  ( 24.50753990722797226, 26.84611427229081215, -27.39925439962615883 ) ) ;
#23495 = DIRECTION ( 'NONE',  ( 1.000000000000000000, 0.000000000000000000, 0.000000000000000000 ) ) ;
#23496 = EDGE_LOOP ( 'NONE', ( #573, #56570, #68987, #66615 ) ) ;
#23497 = CARTESIAN_POINT ( 'NONE',  ( -8.437984349512095861, 132.6929263765338192, -5.166775262442723748E-16 ) ) ;
#23498 = CARTESIAN_POINT ( 'NONE',  ( -69.74999999999998579, -4.000000000000000000, 20.00000000000000000 ) ) ;
#23499 = AXIS2_PLACEMENT_3D ( 'NONE', #69154, #31489, #64891 ) ;
#23500 = DIRECTION ( 'NONE',  ( -0.000000000000000000, -0.000000000000000000, -1.000000000000000000 ) ) ;
#23501 = CARTESIAN_POINT ( 'NONE',  ( -12.74999999999999822, -0.9999999999999995559, 5.000000000000001776 ) ) ;
#23502 = ORIENTED_EDGE ( 'NONE', *, *, #15835, .F. ) ;
#23503 = CARTESIAN_POINT ( 'NONE',  ( -45.00000000000000000, 99.99999999999992895, -4.000000000000000000 ) ) ;
#23504 = ADVANCED_FACE ( 'NONE', ( #62443 ), #56411, .F. ) ;
#23505 = EDGE_LOOP ( 'NONE', ( #4614, #51380, #67187, #63725 ) ) ;
#23506 = DIRECTION ( 'NONE',  ( -7.703719777548941223E-32, 1.000000000000000000, 0.000000000000000000 ) ) ;
#23507 = DIRECTION ( 'NONE',  ( 0.000000000000000000, 0.000000000000000000, 1.000000000000000000 ) ) ;
#23508 = DIRECTION ( 'NONE',  ( 0.000000000000000000, 0.000000000000000000, 1.000000000000000000 ) ) ;
#23509 = CARTESIAN_POINT ( 'NONE',  ( -133.4049999999999443, -2.607480562269069768, 8.024999999999991473 ) ) ;
#23510 = VECTOR ( 'NONE', #68102, 1000.000000000000000 ) ;
#23511 = SURFACE_STYLE_USAGE ( .BOTH. , #1991 ) ;
#23512 = ORIENTED_EDGE ( 'NONE', *, *, #34461, .T. ) ;
#23513 = AXIS2_PLACEMENT_3D ( 'NONE', #51082, #18381, #55298 ) ;
#23514 = FACE_OUTER_BOUND ( 'NONE', #36933, .T. ) ;
#23515 = EDGE_CURVE ( 'NONE', #58700, #10966, #13739, .T. ) ;
#23516 = CARTESIAN_POINT ( 'NONE',  ( 43.75000000000000000, 18.99999999999998224, 3.750000000000000000 ) ) ;
#23517 = FACE_OUTER_BOUND ( 'NONE', #50578, .T. ) ;
#23518 = EDGE_LOOP ( 'NONE', ( #10723, #32492, #15827, #16483, #36281, #20576, #52260, #3373, #61523, #4562, #11596, #7458, #63321, #19678 ) ) ;
#23519 = ORIENTED_EDGE ( 'NONE', *, *, #13511, .F. ) ;
#23520 = DIRECTION ( 'NONE',  ( 1.000000000000000000, 0.000000000000000000, 0.000000000000000000 ) ) ;
#23521 = AXIS2_PLACEMENT_3D ( 'NONE', #14206, #40971, #3597 ) ;
#23522 = DIRECTION ( 'NONE',  ( 0.000000000000000000, 0.000000000000000000, -1.000000000000000000 ) ) ;
#23523 = CARTESIAN_POINT ( 'NONE',  ( -52.40707362346616804, 3.094860106618428031, -9.524999999999993250 ) ) ;
#23524 = CARTESIAN_POINT ( 'NONE',  ( -10.11618306975752368, 54.14354156754873060, 6.790106699912857202 ) ) ;
#23525 = ORIENTED_EDGE ( 'NONE', *, *, #62985, .T. ) ;
#23526 = CARTESIAN_POINT ( 'NONE',  ( 57.00000000000000000, 16.00000000000000000, 60.00402776293825724 ) ) ;
#23527 = CARTESIAN_POINT ( 'NONE',  ( -17.75000000000000711, 30.74999999999999289, 3.750000000000000000 ) ) ;
#23528 = AXIS2_PLACEMENT_3D ( 'NONE', #12122, #42818, #27593 ) ;
#23529 = AXIS2_PLACEMENT_3D ( 'NONE', #45628, #62450, #46313 ) ;
#23530 = CARTESIAN_POINT ( 'NONE',  ( -181.9449999999999932, -9.827790563157499189E-16, -8.024999999999991473 ) ) ;
#23531 = CIRCLE ( 'NONE', #62837, 5.000000000000004441 ) ;
#23532 = MECHANICAL_DESIGN_GEOMETRIC_PRESENTATION_REPRESENTATION (  '', ( #58338 ), #68489 ) ;
#23533 = ORIENTED_EDGE ( 'NONE', *, *, #5425, .F. ) ;
#23534 = CARTESIAN_POINT ( 'NONE',  ( -74.94185258274741557, 35.62135875951527453, -9.737060520187748480 ) ) ;
#23535 = CARTESIAN_POINT ( 'NONE',  ( -144.3570736234661638, 5.598654528085804216, 7.705886871421366635 ) ) ;
#23536 = VECTOR ( 'NONE', #53308, 1000.000000000000000 ) ;
#23537 = CARTESIAN_POINT ( 'NONE',  ( 53.00000000000000000, 25.24999999999998579, -3.750000000000000000 ) ) ;
#23538 = CARTESIAN_POINT ( 'NONE',  ( -28.03849660526295295, -8.499999999999996447, 0.9189689158111923328 ) ) ;
#23539 = DIRECTION ( 'NONE',  ( 0.000000000000000000, 0.000000000000000000, 1.000000000000000000 ) ) ;
#23540 = COLOUR_RGB ( '', 0.66274510, 0.83137255, 0.94901961) ;
#23541 = FACE_OUTER_BOUND ( 'NONE', #67174, .T. ) ;
#23542 = CARTESIAN_POINT ( 'NONE',  ( -98.84499999999998465, -7.632228543268599452, 2.479861379858951054 ) ) ;
#23543 = CARTESIAN_POINT ( 'NONE',  ( 5.598654528085809545, 113.2549999999999812, -7.705886871421373741 ) ) ;
#23544 = CARTESIAN_POINT ( 'NONE',  ( -76.04499999999998749, 7.632228543268600340, 2.479861379858949277 ) ) ;
#23545 = STYLED_ITEM ( 'NONE', ( #36314 ), #15209 ) ;
#23546 = CARTESIAN_POINT ( 'NONE',  ( -60.00000000000000000, -2.024042244987997205E-14, -11.50000000000000000 ) ) ;
#23547 = CARTESIAN_POINT ( 'NONE',  ( 1.224646799147353256E-15, 2.299999999999999822, 10.00000000000000000 ) ) ;
#23548 = DIRECTION ( 'NONE',  ( 0.000000000000000000, 0.000000000000000000, 1.000000000000000000 ) ) ;
#23549 = UNCERTAINTY_MEASURE_WITH_UNIT (LENGTH_MEASURE( 1.000000000000000082E-05 ), #10636, 'distance_accuracy_value', 'NONE');
#23550 = AXIS2_PLACEMENT_3D ( 'NONE', #5041, #65159, #38494 ) ;
#23551 = EDGE_CURVE ( 'NONE', #48746, #61898, #26077, .T. ) ;
#23552 = ORIENTED_EDGE ( 'NONE', *, *, #19129, .T. ) ;
#23553 = CARTESIAN_POINT ( 'NONE',  ( -111.8929263765338078, -8.102448949553172852, -5.886773742842741797 ) ) ;
#23554 = CARTESIAN_POINT ( 'NONE',  ( -142.0449999999999875, 7.632228543268600340, 2.479861379858949277 ) ) ;
#23555 = EDGE_CURVE ( 'NONE', #33880, #47282, #67371, .T. ) ;
#23556 =( LENGTH_UNIT ( ) NAMED_UNIT ( * ) SI_UNIT ( .MILLI., .METRE. ) );
#23557 = MECHANICAL_DESIGN_GEOMETRIC_PRESENTATION_REPRESENTATION (  '', ( #53888 ), #30315 ) ;
#23558 = SURFACE_STYLE_USAGE ( .BOTH. , #2033 ) ;
#23559 = CARTESIAN_POINT ( 'NONE',  ( -60.00000000000000000, -2.024042244987997205E-14, 10.00000000000000000 ) ) ;
#23560 = CARTESIAN_POINT ( 'NONE',  ( 0.000000000000000000, 110.4999999999999858, 0.000000000000000000 ) ) ;
#23561 = VERTEX_POINT ( 'NONE', #18502 ) ;
#23562 = ORIENTED_EDGE ( 'NONE', *, *, #5219, .T. ) ;
#23563 = COLOUR_RGB ( '', 0.09019608, 0.27058824, 0.51372549) ;
#23564 = STYLED_ITEM ( 'NONE', ( #21107 ), #59214 ) ;
#23565 = CARTESIAN_POINT ( 'NONE',  ( -12.74999999999999822, -3.000000000000000000, 7.000000000000001776 ) ) ;
#23566 = SURFACE_STYLE_USAGE ( .BOTH. , #2040 ) ;
#23567 =( GEOMETRIC_REPRESENTATION_CONTEXT ( 3 ) GLOBAL_UNCERTAINTY_ASSIGNED_CONTEXT ( ( #49442 ) ) GLOBAL_UNIT_ASSIGNED_CONTEXT ( ( #20447, #41950, #3165 ) ) REPRESENTATION_CONTEXT ( 'NONE', 'WORKASPACE' ) );
#23568 = DIRECTION ( 'NONE',  ( -0.000000000000000000, 0.000000000000000000, -1.000000000000000000 ) ) ;
#23569 = CARTESIAN_POINT ( 'NONE',  ( 98.00000000000000000, 16.00000000000000000, -12.50000000000000178 ) ) ;
#23570 = LINE ( 'NONE', #45084, #11668 ) ;
#23571 = EDGE_LOOP ( 'NONE', ( #13051, #9931, #20141, #18317 ) ) ;
#23572 = CARTESIAN_POINT ( 'NONE',  ( -130.5549999999999784, 0.000000000000000000, 8.024999999999991473 ) ) ;
#23574 = EDGE_CURVE ( 'NONE', #65204, #23886, #44918, .T. ) ;
#23573 = ORIENTED_EDGE ( 'NONE', *, *, #1201, .F. ) ;
#23575 = EDGE_CURVE ( 'NONE', #41309, #52342, #19352, .T. ) ;
#23576 = ORIENTED_EDGE ( 'NONE', *, *, #15387, .T. ) ;
#23577 = DIRECTION ( 'NONE',  ( 0.000000000000000000, 1.000000000000000000, 0.000000000000000000 ) ) ;
#23578 = ORIENTED_EDGE ( 'NONE', *, *, #67628, .F. ) ;
#23579 = AXIS2_PLACEMENT_3D ( 'NONE', #37855, #28238, #53626 ) ;
#23580 = FACE_OUTER_BOUND ( 'NONE', #1929, .T. ) ;
#23581 = DIRECTION ( 'NONE',  ( 0.000000000000000000, 0.000000000000000000, 1.000000000000000000 ) ) ;
#23582 = AXIS2_PLACEMENT_3D ( 'NONE', #35962, #67260, #29973 ) ;
#23583 = CARTESIAN_POINT ( 'NONE',  ( -8.102448949553181734, 140.4949999999999761, 5.886773742842747126 ) ) ;
#23584 = SURFACE_STYLE_USAGE ( .BOTH. , #34147 ) ;
#23585 = ORIENTED_EDGE ( 'NONE', *, *, #35279, .F. ) ;
#23586 = CARTESIAN_POINT ( 'NONE',  ( 3.749999999999999556, 33.99999999999998579, 3.750000000000000000 ) ) ;
#23588 = EDGE_CURVE ( 'NONE', #48074, #37145, #50855, .T. ) ;
#23587 = CARTESIAN_POINT ( 'NONE',  ( 0.000000000000000000, 143.5549999999999784, -9.525000000000000355 ) ) ;
#23589 = CARTESIAN_POINT ( 'NONE',  ( -57.95499999999997698, -7.632228543268599452, 2.479861379858951054 ) ) ;
#23590 = MECHANICAL_DESIGN_GEOMETRIC_PRESENTATION_REPRESENTATION (  '', ( #37148 ), #11241 ) ;
#23591 = SURFACE_STYLE_USAGE ( .BOTH. , #8121 ) ;
#23592 = ORIENTED_EDGE ( 'NONE', *, *, #44539, .T. ) ;
#23593 = CARTESIAN_POINT ( 'NONE',  ( 3.094860106618435136, 161.4050000000000296, -9.525000000000000355 ) ) ;
#23594 = DIRECTION ( 'NONE',  ( 0.000000000000000000, -0.000000000000000000, -1.000000000000000000 ) ) ;
#23595 = UNCERTAINTY_MEASURE_WITH_UNIT (LENGTH_MEASURE( 1.000000000000000082E-05 ), #58794, 'distance_accuracy_value', 'NONE');
#23596 = AXIS2_PLACEMENT_3D ( 'NONE', #57211, #46363, #30119 ) ;
#23597 = CARTESIAN_POINT ( 'NONE',  ( 57.00000000000000000, 0.000000000000000000, -55.00402776293825724 ) ) ;
#23598 = EDGE_CURVE ( 'NONE', #24181, #11645, #30069, .T. ) ;
#23599 = CARTESIAN_POINT ( 'NONE',  ( 8.082903768654762899, -1.105959442090949618E-15, 7.500000000000000000 ) ) ;
#23600 = ORIENTED_EDGE ( 'NONE', *, *, #65439, .F. ) ;
#23601 = CIRCLE ( 'NONE', #56166, 0.5000000000000004441 ) ;
#23602 = FACE_OUTER_BOUND ( 'NONE', #22952, .T. ) ;
#23603 = EDGE_CURVE ( 'NONE', #27627, #31846, #65412, .T. ) ;
#23604 = VERTEX_POINT ( 'NONE', #20214 ) ;
#23605 = DIRECTION ( 'NONE',  ( 1.000000000000000000, -0.000000000000000000, -0.000000000000000000 ) ) ;
#23606 = AXIS2_PLACEMENT_3D ( 'NONE', #67866, #57289, #46803 ) ;
#23607 = CARTESIAN_POINT ( 'NONE',  ( -122.0070736234661553, -8.102448949553174629, -5.886773742842741797 ) ) ;
#23608 = CARTESIAN_POINT ( 'NONE',  ( 0.000000000000000000, -2.500000000000000000, -3.499999999999997780 ) ) ;
#23609 = CARTESIAN_POINT ( 'NONE',  ( -161.4549999999999841, 7.632228543268599452, -2.479861379858951942 ) ) ;
#23610 = EDGE_LOOP ( 'NONE', ( #34183, #54545, #17877, #14696 ) ) ;
#23611 = UNCERTAINTY_MEASURE_WITH_UNIT (LENGTH_MEASURE( 1.000000000000000082E-05 ), #42378, 'distance_accuracy_value', 'NONE');
#23612 = FILL_AREA_STYLE_COLOUR ( '', #8324 ) ;
#23613 = EDGE_CURVE ( 'NONE', #27683, #14403, #50804, .T. ) ;
#23614 = FACE_OUTER_BOUND ( 'NONE', #18143, .T. ) ;
#23615 = VERTEX_POINT ( 'NONE', #42775 ) ;
#23616 = VERTEX_POINT ( 'NONE', #19869 ) ;
#23617 = SURFACE_STYLE_USAGE ( .BOTH. , #61934 ) ;
#23618 = DIRECTION ( 'NONE',  ( -1.000000000000000000, 0.000000000000000000, 0.000000000000000000 ) ) ;
#23619 = CARTESIAN_POINT ( 'NONE',  ( -79.85499999999997556, 4.716976649647094177, 6.492361379858945902 ) ) ;
#23620 = ORIENTED_EDGE ( 'NONE', *, *, #8212, .F. ) ;
#23621 = COLOUR_RGB ( '', 0.31764706, 0.68627451, 0.89019608) ;
#23622 = CARTESIAN_POINT ( 'NONE',  ( 6.330869393641157750, 43.00000000000000000, -28.38386403503541899 ) ) ;
#23623 = DIRECTION ( 'NONE',  ( -0.000000000000000000, -0.000000000000000000, 1.000000000000000000 ) ) ;
#23624 = AXIS2_PLACEMENT_3D ( 'NONE', #50303, #34110, #23224 ) ;
#23625 = ORIENTED_EDGE ( 'NONE', *, *, #47750, .F. ) ;
#23626 = DIRECTION ( 'NONE',  ( 1.000000000000000000, 0.000000000000000000, 0.000000000000000000 ) ) ;
#23627 =( LENGTH_UNIT ( ) NAMED_UNIT ( * ) SI_UNIT ( .MILLI., .METRE. ) );
#23628 = CARTESIAN_POINT ( 'NONE',  ( 0.000000000000000000, 142.4449999999999932, -9.525000000000000355 ) ) ;
#23629 = CARTESIAN_POINT ( 'NONE',  ( -107.3949999999999960, -6.826472737025115478, -4.959722759717899443 ) ) ;
#23630 = AXIS2_PLACEMENT_3D ( 'NONE', #2587, #6869, #28294 ) ;
#23631 = PRESENTATION_LAYER_ASSIGNMENT (  '', '', ( #34826 ) ) ;
#23632 = LINE ( 'NONE', #28894, #46056 ) ;
#23633 = AXIS2_PLACEMENT_3D ( 'NONE', #8785, #67178, #9504 ) ;
#23634 = ADVANCED_FACE ( 'NONE', ( #21244 ), #58672, .T. ) ;
#23636 = CARTESIAN_POINT ( 'NONE',  ( -15.33454427322983626, 10.90871211463571555, 5.000000000000000888 ) ) ;
#23635 = CARTESIAN_POINT ( 'NONE',  ( -6.062177826491069510, 2.500000000000000000, 3.499999999999999556 ) ) ;
#23637 = COLOUR_RGB ( '', 0.66274510, 0.83137255, 0.94901961) ;
#23638 = CARTESIAN_POINT ( 'NONE',  ( -150.2929263765338135, 3.094860106618428031, -9.524999999999993250 ) ) ;
#23639 = CARTESIAN_POINT ( 'NONE',  ( -170.3950000000000102, -6.826472737025115478, -4.959722759717899443 ) ) ;
#23640 = STYLED_ITEM ( 'NONE', ( #53468 ), #17773 ) ;
#23641 = VECTOR ( 'NONE', #49871, 1000.000000000000000 ) ;
#23642 = CARTESIAN_POINT ( 'NONE',  ( 24.21231517720798010, 113.4999999999999858, 7.500000000000000000 ) ) ;
#23643 = ORIENTED_EDGE ( 'NONE', *, *, #66218, .T. ) ;
#23644 = CARTESIAN_POINT ( 'NONE',  ( 24.00000000000000000, 0.000000000000000000, -4.000000000000000000 ) ) ;
#23645 = VERTEX_POINT ( 'NONE', #68090 ) ;
#23646 = AXIS2_PLACEMENT_3D ( 'NONE', #51690, #2758, #24247 ) ;
#23647 = FILL_AREA_STYLE_COLOUR ( '', #27316 ) ;
#23648 = AXIS2_PLACEMENT_3D ( 'NONE', #35768, #61199, #9038 ) ;
#23649 = EDGE_CURVE ( 'NONE', #67128, #23842, #30591, .T. ) ;
#23650 = CARTESIAN_POINT ( 'NONE',  ( 26.00000000000001776, 15.00000000000000000, -29.68999999999999417 ) ) ;
#23651 = CARTESIAN_POINT ( 'NONE',  ( 0.4644257559287117698, 42.85561152959480324, 74.47757672716494426 ) ) ;
#23652 = DIRECTION ( 'NONE',  ( -0.000000000000000000, -1.000000000000000000, -0.000000000000000000 ) ) ;
#23653 = PRESENTATION_LAYER_ASSIGNMENT (  '', '', ( #32635 ) ) ;
#23654 = EDGE_CURVE ( 'NONE', #57008, #55641, #19789, .T. ) ;
#23655 =( NAMED_UNIT ( * ) PLANE_ANGLE_UNIT ( ) SI_UNIT ( $, .RADIAN. ) );
#23656 = VERTEX_POINT ( 'NONE', #52609 ) ;
#23657 = CARTESIAN_POINT ( 'NONE',  ( -166.7049999999999557, 2.607480562269072433, 8.024999999999991473 ) ) ;
#23658 = EDGE_CURVE ( 'NONE', #36574, #2399, #23277, .T. ) ;
#23659 = EDGE_CURVE ( 'NONE', #5753, #69477, #40728, .T. ) ;
#23660 = ORIENTED_EDGE ( 'NONE', *, *, #24969, .F. ) ;
#23661 = SURFACE_STYLE_USAGE ( .BOTH. , #49720 ) ;
#23662 = VECTOR ( 'NONE', #5049, 1000.000000000000000 ) ;
#23663 = DIRECTION ( 'NONE',  ( 0.000000000000000000, 1.000000000000000000, 0.000000000000000000 ) ) ;
#23664 = CARTESIAN_POINT ( 'NONE',  ( 8.437984349512095861, 153.3070736234660956, 1.550032578732817026E-15 ) ) ;
#23665 = ORIENTED_EDGE ( 'NONE', *, *, #68140, .F. ) ;
#23666 = AXIS2_PLACEMENT_3D ( 'NONE', #59131, #11301, #32755 ) ;
#23667 = PRESENTATION_STYLE_ASSIGNMENT (( #13112 ) ) ;
#23669 = EDGE_CURVE ( 'NONE', #12588, #59936, #29438, .T. ) ;
#23668 = DIRECTION ( 'NONE',  ( 0.000000000000000000, 0.000000000000000000, 1.000000000000000000 ) ) ;
#23670 = CARTESIAN_POINT ( 'NONE',  ( -83.60499999999998977, 6.826472737025113702, -4.959722759717902107 ) ) ;
#23671 =( BOUNDED_CURVE ( )  B_SPLINE_CURVE ( 2, ( #24643, #20068, #10235, #9560, #20435, #47212, #57024, #15530, #40885, #3881, #25358 ),
 .UNSPECIFIED., .F., .F. ) 
 B_SPLINE_CURVE_WITH_KNOTS ( ( 3, 2, 2, 2, 2, 3 ),
 ( 0.4347826086956418368, 0.4369565217391200296, 0.4391304347825982779, 0.4413043478260764707, 0.4434782608695546635, 0.4456521739130328563 ),
 .UNSPECIFIED. ) 
 CURVE ( )  GEOMETRIC_REPRESENTATION_ITEM ( )  RATIONAL_B_SPLINE_CURVE ( ( 1.000000000000232481, 0.9510565162949210505, 1.000000000000000000, 0.9510565162951535312, 1.000000000000000000, 0.9510565162951535312, 1.000000000000000000, 0.9510565162951535312, 1.000000000000000000, 0.9510565162953922291, 0.9999999999997613020 ) ) 
 REPRESENTATION_ITEM ( '' )  );
#23672 = CARTESIAN_POINT ( 'NONE',  ( -5.598654528085808657, 132.7549999999999955, 7.705886871421373741 ) ) ;
#23673 = UNCERTAINTY_MEASURE_WITH_UNIT (LENGTH_MEASURE( 1.000000000000000082E-05 ), #33078, 'distance_accuracy_value', 'NONE');
#23674 = FACE_OUTER_BOUND ( 'NONE', #56284, .T. ) ;
#23675 = LINE ( 'NONE', #45857, #35527 ) ;
#23676 = EDGE_CURVE ( 'NONE', #14403, #27683, #53070, .T. ) ;
#23677 = DIRECTION ( 'NONE',  ( 0.000000000000000000, 0.000000000000000000, -1.000000000000000000 ) ) ;
#23678 = DIRECTION ( 'NONE',  ( -0.000000000000000000, -0.000000000000000000, -1.000000000000000000 ) ) ;
#23679 = CIRCLE ( 'NONE', #46172, 1.000000000000000888 ) ;
#23680 = DIRECTION ( 'NONE',  ( 1.000000000000000000, 0.000000000000000000, 0.000000000000000000 ) ) ;
#23681 = VERTEX_POINT ( 'NONE', #36795 ) ;
#23682 = DIRECTION ( 'NONE',  ( -1.000000000000000000, -0.000000000000000000, -0.000000000000000000 ) ) ;
#23683 = DIRECTION ( 'NONE',  ( -1.000000000000000000, -1.156482317317866302E-16, 0.000000000000000000 ) ) ;
#23684 = CARTESIAN_POINT ( 'NONE',  ( -55.34499999999997755, 7.632228543268599452, -2.479861379858951942 ) ) ;
#23686 = ORIENTED_EDGE ( 'NONE', *, *, #52057, .F. ) ;
#23685 = VECTOR ( 'NONE', #50575, 1000.000000000000000 ) ;
#23687 = LINE ( 'NONE', #34579, #51948 ) ;
#23688 = AXIS2_PLACEMENT_3D ( 'NONE', #60746, #11888, #44300 ) ;
#23689 = DIRECTION ( 'NONE',  ( -0.000000000000000000, -1.000000000000000000, -0.000000000000000000 ) ) ;
#23690 = CARTESIAN_POINT ( 'NONE',  ( 65.50000000000000000, 2.470600640510328946E-15, 6.500000000000000000 ) ) ;
#23691 = FILL_AREA_STYLE ('',( #28606 ) ) ;
#23692 = ORIENTED_EDGE ( 'NONE', *, *, #60335, .T. ) ;
#23693 = CARTESIAN_POINT ( 'NONE',  ( -49.29458994068759381, -11.22445319598486435, 3.543713891411715000 ) ) ;
#23694 = CARTESIAN_POINT ( 'NONE',  ( -52.19499999999999318, 8.437984349512086979, -1.550032578732815448E-15 ) ) ;
#23695 = PRESENTATION_LAYER_ASSIGNMENT (  '', '', ( #55159 ) ) ;
#23696 = VERTEX_POINT ( 'NONE', #58209 ) ;
#23697 = CARTESIAN_POINT ( 'NONE',  ( -75.00000000000000000, 9.115532208874117970, 6.738970650128760731 ) ) ;
#23698 = CARTESIAN_POINT ( 'NONE',  ( -101.4549999999999841, 7.632228543268599452, -2.479861379858951942 ) ) ;
#23699 = VERTEX_POINT ( 'NONE', #31455 ) ;
#23700 = EDGE_CURVE ( 'NONE', #27009, #28073, #42427, .T. ) ;
#23701 = DIRECTION ( 'NONE',  ( 0.07898106964430649801, 0.9968761159932768567, -1.346643164337371088E-16 ) ) ;
#23702 = MECHANICAL_DESIGN_GEOMETRIC_PRESENTATION_REPRESENTATION (  '', ( #23640 ), #29257 ) ;
#23703 = DIRECTION ( 'NONE',  ( 0.000000000000000000, 0.000000000000000000, 1.000000000000000000 ) ) ;
#23704 = CARTESIAN_POINT ( 'NONE',  ( -148.7070736234662149, -3.094860106618431139, -9.524999999999991473 ) ) ;
#23705 = ADVANCED_FACE ( 'NONE', ( #15661 ), #58551, .T. ) ;
#23706 = DIRECTION ( 'NONE',  ( 0.000000000000000000, 0.000000000000000000, 1.000000000000000000 ) ) ;
#23707 = CIRCLE ( 'NONE', #50679, 14.49999999999999822 ) ;
#23708 = CARTESIAN_POINT ( 'NONE',  ( -5.598654528085806881, 139.7449999999999761, -7.705886871421374629 ) ) ;
#23709 = CARTESIAN_POINT ( 'NONE',  ( -87.65707362346617515, 9.058813317711329915, 2.943386871421369566 ) ) ;
#23710 = DIRECTION ( 'NONE',  ( 0.000000000000000000, 0.000000000000000000, -1.000000000000000000 ) ) ;
#23711 = CARTESIAN_POINT ( 'NONE',  ( 20.71231517720798010, 149.9999999999999716, 10.00000000000000000 ) ) ;
#23712 = EDGE_LOOP ( 'NONE', ( #54724, #41032, #7047, #24531 ) ) ;
#23713 =( GEOMETRIC_REPRESENTATION_CONTEXT ( 3 ) GLOBAL_UNCERTAINTY_ASSIGNED_CONTEXT ( ( #2998 ) ) GLOBAL_UNIT_ASSIGNED_CONTEXT ( ( #60919, #1071, #6763 ) ) REPRESENTATION_CONTEXT ( 'NONE', 'WORKASPACE' ) );
#23715 = FACE_OUTER_BOUND ( 'NONE', #57047, .T. ) ;
#23714 =( LENGTH_UNIT ( ) NAMED_UNIT ( * ) SI_UNIT ( .MILLI., .METRE. ) );
#23716 = CARTESIAN_POINT ( 'NONE',  ( -118.5549999999999926, 0.000000000000000000, 8.024999999999991473 ) ) ;
#23717 = CARTESIAN_POINT ( 'NONE',  ( -164.8429263765337964, 9.058813317711329915, -2.943386871421373119 ) ) ;
#23718 = CARTESIAN_POINT ( 'NONE',  ( 3.094860106618431583, 114.0949999999999704, 9.525000000000000355 ) ) ;
#23719 = CARTESIAN_POINT ( 'NONE',  ( -131.9949999999999477, -6.826472737025115478, 4.959722759717900331 ) ) ;
#23720 = CARTESIAN_POINT ( 'NONE',  ( -131.5449999999999875, -7.632228543268600340, -2.479861379858950166 ) ) ;
#23721 = STYLED_ITEM ( 'NONE', ( #61602 ), #60130 ) ;
#23722 = LINE ( 'NONE', #62037, #17859 ) ;
#23723 = ORIENTED_EDGE ( 'NONE', *, *, #19136, .T. ) ;
#23724 = CARTESIAN_POINT ( 'NONE',  ( 0.000000000000000000, 2.299999999999999822, -3.000000000000000444 ) ) ;
#23725 = CIRCLE ( 'NONE', #27064, 0.5000000000000004441 ) ;
#23726 = VECTOR ( 'NONE', #63521, 1000.000000000000000 ) ;
#23727 = CARTESIAN_POINT ( 'NONE',  ( -183.7429263765338021, -5.598654528085803328, -7.705886871421366635 ) ) ;
#23728 = PLANE ( 'NONE',  #25257 ) ;
#23729 = AXIS2_PLACEMENT_3D ( 'NONE', #26986, #64665, #52402 ) ;
#23730 = CARTESIAN_POINT ( 'NONE',  ( 30.75000000000001066, 16.24999999999997513, 4.000000000000000000 ) ) ;
#23731 = EDGE_CURVE ( 'NONE', #50952, #53532, #12617, .T. ) ;
#23732 =( NAMED_UNIT ( * ) SI_UNIT ( $, .STERADIAN. ) SOLID_ANGLE_UNIT ( ) );
#23733 = DIRECTION ( 'NONE',  ( 6.938893903907222067E-15, 0.000000000000000000, 1.000000000000000000 ) ) ;
#23734 = CARTESIAN_POINT ( 'NONE',  ( -93.59292637653378222, -3.094860106618431139, -9.524999999999991473 ) ) ;
#23735 = SHAPE_DEFINITION_REPRESENTATION ( #68112, #12274 ) ;
#23736 = CARTESIAN_POINT ( 'NONE',  ( -50.46281877639898283, -12.29960362420287012, 1.307293633603369809 ) ) ;
#23737 = DIRECTION ( 'NONE',  ( 0.000000000000000000, 0.000000000000000000, 1.000000000000000000 ) ) ;
#23738 =( GEOMETRIC_REPRESENTATION_CONTEXT ( 3 ) GLOBAL_UNCERTAINTY_ASSIGNED_CONTEXT ( ( #29956 ) ) GLOBAL_UNIT_ASSIGNED_CONTEXT ( ( #44897, #23744, #33271 ) ) REPRESENTATION_CONTEXT ( 'NONE', 'WORKASPACE' ) );
#23739 = ADVANCED_FACE ( 'NONE', ( #11394 ), #12079, .F. ) ;
#23740 = LINE ( 'NONE', #44561, #28078 ) ;
#23741 = CYLINDRICAL_SURFACE ( 'NONE', #33713, 26.99999999999999645 ) ;
#23742 = CARTESIAN_POINT ( 'NONE',  ( -41.36364127011528069, 107.7184400395438644, 3.928466540244182958 ) ) ;
#23743 = MECHANICAL_DESIGN_GEOMETRIC_PRESENTATION_REPRESENTATION (  '', ( #9206 ), #13643 ) ;
#23744 =( NAMED_UNIT ( * ) PLANE_ANGLE_UNIT ( ) SI_UNIT ( $, .RADIAN. ) );
#23745 = ADVANCED_FACE ( 'NONE', ( #65557 ), #65454, .T. ) ;
#23746 = ORIENTED_EDGE ( 'NONE', *, *, #46439, .F. ) ;
#23747 = COLOUR_RGB ( '', 0.31764706, 0.68627451, 0.89019608) ;
#23748 = PRESENTATION_STYLE_ASSIGNMENT (( #50491 ) ) ;
#23749 = CARTESIAN_POINT ( 'NONE',  ( 26.00000000000001066, 19.24999999999997868, -3.750000000000000000 ) ) ;
#23750 = VERTEX_POINT ( 'NONE', #64531 ) ;
#23751 = CARTESIAN_POINT ( 'NONE',  ( -43.75000000000000000, 0.000000000000000000, 0.000000000000000000 ) ) ;
#23752 = AXIS2_PLACEMENT_3D ( 'NONE', #32833, #39177, #12052 ) ;
#23753 = CARTESIAN_POINT ( 'NONE',  ( 2.607480562269076430, 120.9070736234661609, -8.025000000000000355 ) ) ;
#23754 = MECHANICAL_DESIGN_GEOMETRIC_PRESENTATION_REPRESENTATION (  '', ( #62055 ), #64323 ) ;
#23755 = CARTESIAN_POINT ( 'NONE',  ( -8.750000000000001776, 24.74999999999998579, -4.000000000000000000 ) ) ;
#23756 = FACE_OUTER_BOUND ( 'NONE', #21853, .T. ) ;
#23757 = VECTOR ( 'NONE', #54144, 1000.000000000000000 ) ;
#23758 = FACE_OUTER_BOUND ( 'NONE', #38433, .T. ) ;
#23759 = ORIENTED_EDGE ( 'NONE', *, *, #4171, .F. ) ;
#23760 = ADVANCED_FACE ( 'NONE', ( #17406 ), #32864, .F. ) ;
#23761 = CARTESIAN_POINT ( 'NONE',  ( 0.000000000000000000, 0.000000000000000000, 1.000000000000000000 ) ) ;
#23762 = CARTESIAN_POINT ( 'NONE',  ( 4.716976649647099507, 150.7570736234661695, -6.492361379858953008 ) ) ;
#23763 = CARTESIAN_POINT ( 'NONE',  ( -83.24499999999999034, -4.716976649647093289, -6.492361379858945902 ) ) ;
#23764 = VERTEX_POINT ( 'NONE', #66606 ) ;
#23765 = CIRCLE ( 'NONE', #45153, 0.5000000000000004441 ) ;
#23766 = SURFACE_STYLE_FILL_AREA ( #29018 ) ;
#23767 = CIRCLE ( 'NONE', #38446, 0.5000000000000004441 ) ;
#23768 = PRESENTATION_STYLE_ASSIGNMENT (( #12508 ) ) ;
#23769 = ORIENTED_EDGE ( 'NONE', *, *, #44790, .F. ) ;
#23770 = SURFACE_STYLE_FILL_AREA ( #30076 ) ;
#23771 = CARTESIAN_POINT ( 'NONE',  ( -75.44292637653379074, -1.166476076187852838E-15, -9.524999999999991473 ) ) ;
#23772 = COLOUR_RGB ( '', 0.40784314, 0.44705882, 0.49803922) ;
#23773 = CARTESIAN_POINT ( 'NONE',  ( 8.000000000000035527, 5.000000000000000000, 77.00402776293825013 ) ) ;
#23774 = ORIENTED_EDGE ( 'NONE', *, *, #38570, .F. ) ;
#23775 = AXIS2_PLACEMENT_3D ( 'NONE', #65708, #27005, #66041 ) ;
#23776 =( NAMED_UNIT ( * ) SI_UNIT ( $, .STERADIAN. ) SOLID_ANGLE_UNIT ( ) );
#23777 = ORIENTED_EDGE ( 'NONE', *, *, #33823, .T. ) ;
#23778 =( NAMED_UNIT ( * ) PLANE_ANGLE_UNIT ( ) SI_UNIT ( $, .RADIAN. ) );
#23779 = PRESENTATION_STYLE_ASSIGNMENT (( #19178 ) ) ;
#23780 = CARTESIAN_POINT ( 'NONE',  ( 1.224646799147353256E-15, 2.299999999999999822, 10.00000000000000000 ) ) ;
#23781 = CARTESIAN_POINT ( 'NONE',  ( -175.1070736234661922, 8.102448949553171076, -5.886773742842744461 ) ) ;
#23782 = PRESENTATION_LAYER_ASSIGNMENT (  '', '', ( #4703 ) ) ;
#23783 = CARTESIAN_POINT ( 'NONE',  ( -10.11618306975752368, 54.14354156754873060, -6.790106699912857202 ) ) ;
#23784 = CARTESIAN_POINT ( 'NONE',  ( -8.102448949553179958, 112.8949999999999818, -5.886773742842749790 ) ) ;
#23785 = CARTESIAN_POINT ( 'NONE',  ( -116.9070736234661894, -3.094860106618429807, 9.524999999999991473 ) ) ;
#23786 = CIRCLE ( 'NONE', #29402, 9.000000000000007105 ) ;
#23787 = FACE_OUTER_BOUND ( 'NONE', #7746, .T. ) ;
#23788 = FACE_OUTER_BOUND ( 'NONE', #26016, .T. ) ;
#23789 = ORIENTED_EDGE ( 'NONE', *, *, #9558, .F. ) ;
#23790 = STYLED_ITEM ( 'NONE', ( #63456 ), #53305 ) ;
#23791 = CARTESIAN_POINT ( 'NONE',  ( 10.00000000000000533, 43.00000000000000000, -74.38749456993816978 ) ) ;
#23792 = FACE_OUTER_BOUND ( 'NONE', #47628, .T. ) ;
#23793 = CARTESIAN_POINT ( 'NONE',  ( 62.24999999999998579, 31.24999999999999289, 3.750000000000000000 ) ) ;
#23794 = CARTESIAN_POINT ( 'NONE',  ( 44.50000000000000000, 99.99999999999992895, -3.500000000000000000 ) ) ;
#23795 = ORIENTED_EDGE ( 'NONE', *, *, #8917, .F. ) ;
#23796 = CIRCLE ( 'NONE', #11441, 13.99999999999999822 ) ;
#23797 = CARTESIAN_POINT ( 'NONE',  ( -160.8549999999999898, 4.716976649647094177, 6.492361379858945902 ) ) ;
#23798 = DIRECTION ( 'NONE',  ( 1.000000000000000000, 0.000000000000000000, -0.000000000000000000 ) ) ;
#23799 = CIRCLE ( 'NONE', #36184, 0.2500000000000002220 ) ;
#23800 = B_SPLINE_CURVE_WITH_KNOTS ( 'NONE', 3,
 ( #33326, #29776, #19196, #46706, #57189, #9376, #24824, #25524, #57548, #2983, #2646, #7969, #45651, #35411, #41054, #40343, #67070, #9019, #51238, #41397, #19560, #52302, #47036, #68451, #62805, #13581, #30436, #51938, #3693 ),
 .UNSPECIFIED., .F., .F.,
 ( 4, 2, 2, 2, 2, 2, 2, 1, 2, 2, 2, 2, 2, 2, 4 ),
 ( 5.102712030719938591E-17, 0.002418039429563660549, 0.003627059144345467188, 0.004836078859127274261, 0.006045098573909080467, 0.007254118288690887539, 0.008463138003472692877, 0.009672157718254499950, 0.01088117743303630876, 0.01209019714781811757, 0.01329921686259992637, 0.01450823657738173518, 0.01692627600694535453, 0.01813529572172715987, 0.01934431543650896868 ),
 .UNSPECIFIED. ) ;
#23801 = CARTESIAN_POINT ( 'NONE',  ( -164.0949999999999989, -2.607480562269071545, -8.024999999999991473 ) ) ;
#23802 = CARTESIAN_POINT ( 'NONE',  ( -160.6449999999999818, 4.716976649647091513, -6.492361379858946790 ) ) ;
#23803 = ORIENTED_EDGE ( 'NONE', *, *, #36207, .F. ) ;
#23804 =( BOUNDED_CURVE ( )  B_SPLINE_CURVE ( 2, ( #50675, #2417, #61906, #5148, #42494, #63559, #16453, #37216, #31178, #64929, #26594 ),
 .UNSPECIFIED., .F., .F. ) 
 B_SPLINE_CURVE_WITH_KNOTS ( ( 3, 2, 2, 2, 2, 3 ),
 ( 0.5978260869565075186, 0.5999999999999856559, 0.6021739130434639042, 0.6043478260869420415, 0.6065217391304204009, 0.6086956521738985382 ),
 .UNSPECIFIED. ) 
 CURVE ( )  GEOMETRIC_REPRESENTATION_ITEM ( )  RATIONAL_B_SPLINE_CURVE ( ( 1.000000000000319966, 0.9510565162948335649, 1.000000000000000000, 0.9510565162951535312, 1.000000000000000000, 0.9510565162951535312, 1.000000000000000000, 0.9510565162951535312, 1.000000000000000000, 0.9510565162954809360, 0.9999999999996725952 ) ) 
 REPRESENTATION_ITEM ( '' )  );
#23805 = DIRECTION ( 'NONE',  ( 1.224646799147353207E-16, 1.000000000000000000, -0.000000000000000000 ) ) ;
#23806 = VECTOR ( 'NONE', #40087, 1000.000000000000114 ) ;
#23807 = CARTESIAN_POINT ( 'NONE',  ( -72.20499999999998408, -2.607480562269071545, -8.024999999999991473 ) ) ;
#23808 = CARTESIAN_POINT ( 'NONE',  ( 24.75000000000000355, 37.00000000000000000, 3.000000000000000000 ) ) ;
#23809 = COLOUR_RGB ( '', 0.09019608, 0.27058824, 0.51372549) ;
#23810 = DIRECTION ( 'NONE',  ( 0.000000000000000000, 0.000000000000000000, -1.000000000000000000 ) ) ;
#23811 = CARTESIAN_POINT ( 'NONE',  ( -72.44499999999997897, 0.000000000000000000, 8.024999999999991473 ) ) ;
#23812 = CARTESIAN_POINT ( 'NONE',  ( -8.102448949553181734, 147.6049999999999329, 5.886773742842747126 ) ) ;
#23813 = CARTESIAN_POINT ( 'NONE',  ( -0.1770589935874656851, 2.499999999999994227, -7.000000000000004441 ) ) ;
#23814 = ADVANCED_FACE ( 'NONE', ( #24705 ), #7171, .T. ) ;
#23815 = CIRCLE ( 'NONE', #68735, 0.4999999999999994449 ) ;
#23816 = FACE_OUTER_BOUND ( 'NONE', #34483, .T. ) ;
#23817 = DIRECTION ( 'NONE',  ( -0.000000000000000000, -0.000000000000000000, -1.000000000000000000 ) ) ;
#23818 = CARTESIAN_POINT ( 'NONE',  ( -19.89974874213239886, 115.4999999999999574, -10.00000000000000000 ) ) ;
#23819 = AXIS2_PLACEMENT_3D ( 'NONE', #49615, #976, #49971 ) ;
#23820 = MECHANICAL_DESIGN_GEOMETRIC_PRESENTATION_REPRESENTATION (  '', ( #1323 ), #62027 ) ;
#23821 = ADVANCED_FACE ( 'NONE', ( #34575 ), #56383, .F. ) ;
#23822 = CARTESIAN_POINT ( 'NONE',  ( 60.00000000000000000, 1.797044900979284448E-15, 12.00000000000000000 ) ) ;
#23823 = EDGE_CURVE ( 'NONE', #68013, #2160, #35126, .T. ) ;
#23824 = AXIS2_PLACEMENT_3D ( 'NONE', #61117, #62146, #66753 ) ;
#23825 = ADVANCED_FACE ( 'NONE', ( #56753 ), #31752, .F. ) ;
#23826 = CARTESIAN_POINT ( 'NONE',  ( -12.74999999999999822, -4.000000000000000000, 18.00000000000000000 ) ) ;
#23827 = EDGE_LOOP ( 'NONE', ( #45542, #46677, #11232, #28273, #15656 ) ) ;
#23828 = ORIENTED_EDGE ( 'NONE', *, *, #25712, .T. ) ;
#23829 =( LENGTH_UNIT ( ) NAMED_UNIT ( * ) SI_UNIT ( .MILLI., .METRE. ) );
#23830 = EDGE_CURVE ( 'NONE', #53774, #54731, #20126, .T. ) ;
#23831 = SURFACE_STYLE_USAGE ( .BOTH. , #12924 ) ;
#23832 = EDGE_CURVE ( 'NONE', #43960, #54714, #31039, .T. ) ;
#23833 = PLANE ( 'NONE',  #45164 ) ;
#23834 =( NAMED_UNIT ( * ) PLANE_ANGLE_UNIT ( ) SI_UNIT ( $, .RADIAN. ) );
#23835 = VERTEX_POINT ( 'NONE', #3574 ) ;
#23836 = VERTEX_POINT ( 'NONE', #19799 ) ;
#23837 = CARTESIAN_POINT ( 'NONE',  ( -74.99999999999998579, 50.00000000000000000, 12.00000000000000000 ) ) ;
#23838 =( LENGTH_UNIT ( ) NAMED_UNIT ( * ) SI_UNIT ( .MILLI., .METRE. ) );
#23839 = ORIENTED_EDGE ( 'NONE', *, *, #9897, .T. ) ;
#23840 = DIRECTION ( 'NONE',  ( 1.000000000000000000, 0.000000000000000000, -0.000000000000000000 ) ) ;
#23841 = DIRECTION ( 'NONE',  ( -1.000000000000000000, -0.000000000000000000, 4.625929269271505635E-16 ) ) ;
#23842 = VERTEX_POINT ( 'NONE', #9266 ) ;
#23843 = DIRECTION ( 'NONE',  ( 0.000000000000000000, 0.000000000000000000, 1.000000000000000000 ) ) ;
#23844 = CARTESIAN_POINT ( 'NONE',  ( -195.0000000000000000, 0.000000000000000000, 0.000000000000000000 ) ) ;
#23845 = CARTESIAN_POINT ( 'NONE',  ( -113.8449999999999847, -7.632228543268599452, 2.479861379858951054 ) ) ;
#23846 = VERTEX_POINT ( 'NONE', #46588 ) ;
#23847 = ORIENTED_EDGE ( 'NONE', *, *, #42275, .T. ) ;
#23848 = CARTESIAN_POINT ( 'NONE',  ( 30.99999999999999289, 5.000000000000000000, 24.00402776293822171 ) ) ;
#23849 = CARTESIAN_POINT ( 'NONE',  ( -9.999969304761462396, -12.00001278968254148, -0.1637141617949805783 ) ) ;
#23850 = FACE_OUTER_BOUND ( 'NONE', #12786, .T. ) ;
#23851 = ORIENTED_EDGE ( 'NONE', *, *, #69500, .T. ) ;
#23852 = CARTESIAN_POINT ( 'NONE',  ( 8.437984349512095861, 149.1929263765337623, 1.550032578732817026E-15 ) ) ;
#23853 = DIRECTION ( 'NONE',  ( 0.000000000000000000, 0.000000000000000000, 1.000000000000000000 ) ) ;
#23854 = CARTESIAN_POINT ( 'NONE',  ( 17.75000000000000711, 31.24999999999999289, 4.000000000000000000 ) ) ;
#23855 = AXIS2_PLACEMENT_3D ( 'NONE', #7513, #39910, #50779 ) ;
#23856 =( NAMED_UNIT ( * ) SI_UNIT ( $, .STERADIAN. ) SOLID_ANGLE_UNIT ( ) );
#23857 = CARTESIAN_POINT ( 'NONE',  ( 0.000000000000000000, 113.9429263765338192, -8.025000000000000355 ) ) ;
#23858 = ORIENTED_EDGE ( 'NONE', *, *, #26374, .T. ) ;
#23859 = DIRECTION ( 'NONE',  ( -0.000000000000000000, -0.000000000000000000, 1.000000000000000000 ) ) ;
#23860 = ORIENTED_EDGE ( 'NONE', *, *, #10823, .T. ) ;
#23861 =( NAMED_UNIT ( * ) SI_UNIT ( $, .STERADIAN. ) SOLID_ANGLE_UNIT ( ) );
#23862 = FACE_OUTER_BOUND ( 'NONE', #3868, .T. ) ;
#23863 = CARTESIAN_POINT ( 'NONE',  ( -7.794228634059950700, -4.500000000000003553, 0.000000000000000000 ) ) ;
#23865 = CARTESIAN_POINT ( 'NONE',  ( -130.5549999999999784, 0.000000000000000000, 8.024999999999991473 ) ) ;
#23864 = COLOUR_RGB ( '', 0.72549020, 0.75294118, 0.79215686) ;
#23866 = CARTESIAN_POINT ( 'NONE',  ( 0.000000000000000000, 149.9429263765338476, -8.025000000000000355 ) ) ;
#23867 = ORIENTED_EDGE ( 'NONE', *, *, #34317, .F. ) ;
#23868 = DIRECTION ( 'NONE',  ( 0.000000000000000000, 1.000000000000000000, 0.000000000000000000 ) ) ;
#23869 = COLOUR_RGB ( '', 0.08235294, 0.09019608, 0.10196078) ;
#23870 = FACE_OUTER_BOUND ( 'NONE', #44591, .T. ) ;
#23871 = CARTESIAN_POINT ( 'NONE',  ( -106.5570736234661666, -1.166476076187852838E-15, -9.524999999999991473 ) ) ;
#23872 = CARTESIAN_POINT ( 'NONE',  ( -45.00000000000000711, 7.967268226264182296, -7.000000000000000000 ) ) ;
#23873 = ORIENTED_EDGE ( 'NONE', *, *, #62228, .F. ) ;
#23874 = VERTEX_POINT ( 'NONE', #63741 ) ;
#23875 = CARTESIAN_POINT ( 'NONE',  ( 4.357963766315029019, -1.733608113333017897, -6.451785339198144342 ) ) ;
#23876 = LINE ( 'NONE', #18261, #17461 ) ;
#23877 = ORIENTED_EDGE ( 'NONE', *, *, #57660, .F. ) ;
#23878 = CARTESIAN_POINT ( 'NONE',  ( 34.99999999999992895, 112.9999999999999858, -7.500000000000000000 ) ) ;
#23879 = DIRECTION ( 'NONE',  ( 0.000000000000000000, 0.000000000000000000, 1.000000000000000000 ) ) ;
#23880 = CARTESIAN_POINT ( 'NONE',  ( 0.000000000000000000, 115.4999999999999574, 0.000000000000000000 ) ) ;
#23881 =( GEOMETRIC_REPRESENTATION_CONTEXT ( 3 ) GLOBAL_UNCERTAINTY_ASSIGNED_CONTEXT ( ( #69446 ) ) GLOBAL_UNIT_ASSIGNED_CONTEXT ( ( #45447, #51028, #66867 ) ) REPRESENTATION_CONTEXT ( 'NONE', 'WORKASPACE' ) );
#23882 = DIRECTION ( 'NONE',  ( -1.000000000000000000, -0.000000000000000000, -0.000000000000000000 ) ) ;
#23883 = CARTESIAN_POINT ( 'NONE',  ( -59.90707362346616094, -3.094860106618429807, 9.524999999999991473 ) ) ;
#23884 = AXIS2_PLACEMENT_3D ( 'NONE', #35643, #30324, #8900 ) ;
#23885 = CARTESIAN_POINT ( 'NONE',  ( -177.9570736234661865, 9.058813317711329915, -2.943386871421373119 ) ) ;
#23886 = VERTEX_POINT ( 'NONE', #47638 ) ;
#23887 = MECHANICAL_DESIGN_GEOMETRIC_PRESENTATION_REPRESENTATION (  '', ( #44182 ), #45270 ) ;
#23888 = CARTESIAN_POINT ( 'NONE',  ( -161.9070736234664594, -3.094860106613992912, 9.525000000003217338 ) ) ;
#23889 = CARTESIAN_POINT ( 'NONE',  ( -94.94292637653380496, 0.000000000000000000, 9.524999999999991473 ) ) ;
#23890 = PRESENTATION_STYLE_ASSIGNMENT (( #46075 ) ) ;
#23891 = CARTESIAN_POINT ( 'NONE',  ( -98.30499999999997840, 8.437984349512085203, -1.550032578732815448E-15 ) ) ;
#23892 = CARTESIAN_POINT ( 'NONE',  ( -29.43102036153494439, -7.714630622815294103, -0.5236166406898870029 ) ) ;
#23893 = DIRECTION ( 'NONE',  ( -2.312964634635740689E-15, 1.000000000000000000, 0.000000000000000000 ) ) ;
#23894 = AXIS2_PLACEMENT_3D ( 'NONE', #49954, #50627, #12982 ) ;
#23895 = CARTESIAN_POINT ( 'NONE',  ( -100.7950000000000017, 2.607480562269069324, -8.024999999999993250 ) ) ;
#23896 = CARTESIAN_POINT ( 'NONE',  ( -1.166476076187854022E-15, 115.0549999999999926, 9.525000000000000355 ) ) ;
#23897 = CARTESIAN_POINT ( 'NONE',  ( -77.09499999999997044, -2.607480562269071545, -8.024999999999991473 ) ) ;
#23898 = CIRCLE ( 'NONE', #30619, 13.99999999999999822 ) ;
#23899 = SURFACE_SIDE_STYLE ('',( #56246 ) ) ;
#23900 = ADVANCED_FACE ( 'NONE', ( #57440 ), #26104, .F. ) ;
#23901 = DIRECTION ( 'NONE',  ( 0.000000000000000000, 0.000000000000000000, -1.000000000000000000 ) ) ;
#23902 = CARTESIAN_POINT ( 'NONE',  ( -71.62068965517239860, 36.41396814395972115, -7.500000000000000000 ) ) ;
#23903 = EDGE_CURVE ( 'NONE', #7911, #4242, #28099, .T. ) ;
#23904 = CONICAL_SURFACE ( 'NONE', #37430, 9.000000000000000000, 0.7853981633974500554 ) ;
#23905 = CARTESIAN_POINT ( 'NONE',  ( 7.500000000000000000, 9.184850993605147944E-16, 0.2499999999999924227 ) ) ;
#23906 = CARTESIAN_POINT ( 'NONE',  ( 41.38256758237926647, 107.6997254016901451, -3.907089461173330225 ) ) ;
#23907 = EDGE_LOOP ( 'NONE', ( #39047, #14173, #26106, #17557 ) ) ;
#23908 = CARTESIAN_POINT ( 'NONE',  ( -116.6929263765337907, 10.01517768586948698, -1.839758294383808571E-15 ) ) ;
#23909 = CARTESIAN_POINT ( 'NONE',  ( 2.000000000000022204, 14.00000000000001599, 34.99999999999999289 ) ) ;
#23910 = CARTESIAN_POINT ( 'NONE',  ( -139.3449999999999989, 7.632228543268599452, -2.479861379858951942 ) ) ;
#23911 = DIRECTION ( 'NONE',  ( -0.000000000000000000, -1.000000000000000000, 0.000000000000000000 ) ) ;
#23912 = EDGE_CURVE ( 'NONE', #6337, #40506, #31373, .T. ) ;
#23913 = CARTESIAN_POINT ( 'NONE',  ( 48.00000000000000000, 13.41640786499872284, 7.000000000000000000 ) ) ;
#23914 = ORIENTED_EDGE ( 'NONE', *, *, #9466, .T. ) ;
#23916 = ORIENTED_EDGE ( 'NONE', *, *, #20569, .F. ) ;
#23915 = AXIS2_PLACEMENT_3D ( 'NONE', #28791, #50272, #66436 ) ;
#23917 = CIRCLE ( 'NONE', #22775, 0.5000000000000004441 ) ;
#23918 = PRESENTATION_STYLE_ASSIGNMENT (( #7734 ) ) ;
#23919 = STYLED_ITEM ( 'NONE', ( #66614 ), #46858 ) ;
#23920 = EDGE_CURVE ( 'NONE', #3684, #27751, #20854, .T. ) ;
#23921 = CARTESIAN_POINT ( 'NONE',  ( -17.75000000000000711, 30.74999999999999289, -4.000000000000000000 ) ) ;
#23922 = ORIENTED_EDGE ( 'NONE', *, *, #1211, .T. ) ;
#23923 = CARTESIAN_POINT ( 'NONE',  ( -135.0549999999999784, -9.827790563157499189E-16, -8.024999999999991473 ) ) ;
#23924 = VERTEX_POINT ( 'NONE', #9621 ) ;
#23925 = EDGE_LOOP ( 'NONE', ( #913, #19670, #48056, #58578 ) ) ;
#23926 = LINE ( 'NONE', #67188, #45961 ) ;
#23927 = CARTESIAN_POINT ( 'NONE',  ( -83.69292637653379074, 10.01517768586948698, -1.839758294383808966E-15 ) ) ;
#23928 = COLOUR_RGB ( '', 0.40784314, 0.44705882, 0.49803922) ;
#23929 = ORIENTED_EDGE ( 'NONE', *, *, #16469, .F. ) ;
#23930 = DIRECTION ( 'NONE',  ( -1.000000000000000000, 0.000000000000000000, 0.000000000000000000 ) ) ;
#23931 = AXIS2_PLACEMENT_3D ( 'NONE', #9541, #69629, #68267 ) ;
#23932 = CARTESIAN_POINT ( 'NONE',  ( 5.598654528085809545, 136.1449999999999818, -7.705886871421373741 ) ) ;
#23933 = CARTESIAN_POINT ( 'NONE',  ( -10.11618306975752368, 54.14354156754873060, 2.000000000000000000 ) ) ;
#23934 = AXIS2_PLACEMENT_3D ( 'NONE', #36641, #42952, #42595 ) ;
#23935 = EDGE_LOOP ( 'NONE', ( #3854, #16596, #37993, #11735 ) ) ;
#23936 = CARTESIAN_POINT ( 'NONE',  ( -1.166476076187854022E-15, 139.0549999999999784, 9.525000000000000355 ) ) ;
#23937 = CARTESIAN_POINT ( 'NONE',  ( -47.90499999999997272, 2.607480562269069324, -8.024999999999993250 ) ) ;
#23938 = CARTESIAN_POINT ( 'NONE',  ( 71.62068965517238439, 63.58603185604027885, -7.000000000000000000 ) ) ;
#23939 = VECTOR ( 'NONE', #9151, 999.9999999999998863 ) ;
#23940 = VERTEX_POINT ( 'NONE', #41634 ) ;
#23941 = CARTESIAN_POINT ( 'NONE',  ( -9.827790563157511022E-16, 115.4429263765338192, 8.025000000000000355 ) ) ;
#23942 = CARTESIAN_POINT ( 'NONE',  ( 5.000000000000000000, 6.123233995736766282E-16, 1.000000000000000000 ) ) ;
#23943 =( LENGTH_UNIT ( ) NAMED_UNIT ( * ) SI_UNIT ( .MILLI., .METRE. ) );
#23944 = VECTOR ( 'NONE', #64079, 1000.000000000000000 ) ;
#23945 = STYLED_ITEM ( 'NONE', ( #33738 ), #29309 ) ;
#23946 = SURFACE_STYLE_USAGE ( .BOTH. , #51737 ) ;
#23947 = CARTESIAN_POINT ( 'NONE',  ( -74.99999999999998579, 50.00000000000000000, -10.49999999999999822 ) ) ;
#23948 = ORIENTED_EDGE ( 'NONE', *, *, #39165, .F. ) ;
#23949 = CARTESIAN_POINT ( 'NONE',  ( 1.000000000000000000, 43.00000000000000000, 79.00402776293826435 ) ) ;
#23950 = EDGE_LOOP ( 'NONE', ( #67355, #21685, #58341, #20846 ) ) ;
#23951 = LINE ( 'NONE', #50350, #37098 ) ;
#23952 = CARTESIAN_POINT ( 'NONE',  ( 20.57648123223228964, 114.5812418126072174, 10.27659574468084891 ) ) ;
#23953 = CARTESIAN_POINT ( 'NONE',  ( 10.00000000000001954, 42.00000000000000000, 29.68999999999999417 ) ) ;
#23954 = CARTESIAN_POINT ( 'NONE',  ( -164.3049999999999784, 8.437984349512085203, -1.550032578732815448E-15 ) ) ;
#23955 = EDGE_LOOP ( 'NONE', ( #46877, #54028, #36459, #59614 ) ) ;
#23956 = DIRECTION ( 'NONE',  ( 0.000000000000000000, 0.000000000000000000, -1.000000000000000000 ) ) ;
#23957 = ADVANCED_FACE ( 'NONE', ( #36377 ), #52533, .T. ) ;
#23958 = PRESENTATION_LAYER_ASSIGNMENT (  '', '', ( #16106 ) ) ;
#23959 = CARTESIAN_POINT ( 'NONE',  ( 15.98999599679679839, 118.4999999999999716, -7.000000000000000000 ) ) ;
#23960 = CARTESIAN_POINT ( 'NONE',  ( 3.046771365092978190, 72.00000000000001421, 12.50000000000000000 ) ) ;
#23961 = CARTESIAN_POINT ( 'NONE',  ( 45.58253334211749319, 9.942242644401853013, -6.446113437190194695 ) ) ;
#23962 = ORIENTED_EDGE ( 'NONE', *, *, #11768, .F. ) ;
#23963 = EDGE_LOOP ( 'NONE', ( #33678, #19453, #6509, #42426 ) ) ;
#23964 = CARTESIAN_POINT ( 'NONE',  ( 21.75000000000001066, 22.24999999999998224, 4.000000000000000000 ) ) ;
#23965 = DIRECTION ( 'NONE',  ( -5.782411586589351722E-16, 1.000000000000000000, 0.000000000000000000 ) ) ;
#23966 = CARTESIAN_POINT ( 'NONE',  ( -73.40500000000000114, -2.607480562269069768, 8.024999999999991473 ) ) ;
#23967 = ORIENTED_EDGE ( 'NONE', *, *, #52660, .F. ) ;
#23968 = AXIS2_PLACEMENT_3D ( 'NONE', #12886, #66710, #29037 ) ;
#23970 = CIRCLE ( 'NONE', #8266, 0.5000000000000004441 ) ;
#23969 = CIRCLE ( 'NONE', #22823, 0.2500000000000002220 ) ;
#23971 = CARTESIAN_POINT ( 'NONE',  ( -151.2570736234661979, 5.598654528085800663, -7.705886871421367523 ) ) ;
#23972 =( REPRESENTATION_RELATIONSHIP ('NONE','NONE', #5102, #15001 ) REPRESENTATION_RELATIONSHIP_WITH_TRANSFORMATION ( #9312 )SHAPE_REPRESENTATION_RELATIONSHIP( ) );
#23973 = CARTESIAN_POINT ( 'NONE',  ( -74.45867456775532389, 7.945093266341785920, -6.500000000000000888 ) ) ;
#23974 = VERTEX_POINT ( 'NONE', #14896 ) ;
#23975 =( LENGTH_UNIT ( ) NAMED_UNIT ( * ) SI_UNIT ( .MILLI., .METRE. ) );
#23977 = SURFACE_STYLE_FILL_AREA ( #30985 ) ;
#23976 = FACE_OUTER_BOUND ( 'NONE', #8115, .T. ) ;
#23978 = EDGE_CURVE ( 'NONE', #44039, #32321, #57794, .T. ) ;
#23979 = COLOUR_RGB ( '', 0.40784314, 0.44705882, 0.49803922) ;
#23980 = EDGE_CURVE ( 'NONE', #6580, #3957, #14187, .T. ) ;
#23981 = CARTESIAN_POINT ( 'NONE',  ( -8.102448949553181734, 143.4949999999999477, 5.886773742842747126 ) ) ;
#23982 = CARTESIAN_POINT ( 'NONE',  ( -104.3949999999999960, -6.826472737025115478, -4.959722759717899443 ) ) ;
#23983 = FACE_OUTER_BOUND ( 'NONE', #12936, .T. ) ;
#23984 = AXIS2_PLACEMENT_3D ( 'NONE', #61820, #67465, #29831 ) ;
#23985 = FACE_OUTER_BOUND ( 'NONE', #11130, .T. ) ;
#23986 = COLOUR_RGB ( '', 0.31764706, 0.68627451, 0.89019608) ;
#23988 = CARTESIAN_POINT ( 'NONE',  ( -19.74070358558185490, 11.89371749334803141, -1.623204134912098917 ) ) ;
#23987 = PRESENTATION_STYLE_ASSIGNMENT (( #2477 ) ) ;
#23989 = EDGE_CURVE ( 'NONE', #55259, #63576, #8901, .T. ) ;
#23990 = CARTESIAN_POINT ( 'NONE',  ( -138.8929263765338078, -8.102448949553172852, -5.886773742842741797 ) ) ;
#23991 =( LENGTH_UNIT ( ) NAMED_UNIT ( * ) SI_UNIT ( .MILLI., .METRE. ) );
#23992 = CARTESIAN_POINT ( 'NONE',  ( -171.2949999999999875, -2.607480562269069768, 8.024999999999991473 ) ) ;
#23993 = AXIS2_PLACEMENT_3D ( 'NONE', #47179, #68599, #13734 ) ;
#23994 = CIRCLE ( 'NONE', #35249, 22.50000000000000000 ) ;
#23995 = DIRECTION ( 'NONE',  ( -0.000000000000000000, -0.000000000000000000, 1.000000000000000000 ) ) ;
#23996 = ADVANCED_FACE ( 'NONE', ( #36725 ), #30325, .T. ) ;
#23997 = CYLINDRICAL_SURFACE ( 'NONE', #20353, 19.99999999999998934 ) ;
#23998 = EDGE_LOOP ( 'NONE', ( #17415, #8569, #30133, #27386 ) ) ;
#23999 = LINE ( 'NONE', #39878, #67637 ) ;
#24001 = VERTEX_POINT ( 'NONE', #6333 ) ;
#24000 = VECTOR ( 'NONE', #36268, 1000.000000000000000 ) ;
#24002 = FACE_OUTER_BOUND ( 'NONE', #27828, .T. ) ;
#24003 =( BOUNDED_CURVE ( )  B_SPLINE_CURVE ( 2, ( #59325, #28349, #33320, #64964, #49855, #54743, #59686, #6551, #1236, #55095, #17511 ),
 .UNSPECIFIED., .F., .F. ) 
 B_SPLINE_CURVE_WITH_KNOTS ( ( 3, 2, 2, 2, 2, 3 ),
 ( 0.2391304347826030685, 0.2413043478260812613, 0.2434782608695594819, 0.2456521739130377024, 0.2478260869565159230, 0.2499999999999941158 ),
 .UNSPECIFIED. ) 
 CURVE ( )  GEOMETRIC_REPRESENTATION_ITEM ( )  RATIONAL_B_SPLINE_CURVE ( ( 1.000000000000127010, 0.9510565162950267437, 1.000000000000000000, 0.9510565162951535312, 1.000000000000000000, 0.9510565162951535312, 1.000000000000000000, 0.9510565162951535312, 1.000000000000000000, 0.9510565162952859808, 0.9999999999998675504 ) ) 
 REPRESENTATION_ITEM ( '' )  );
#24004 = AXIS2_PLACEMENT_3D ( 'NONE', #21364, #15443, #16492 ) ;
#24005 = EDGE_CURVE ( 'NONE', #50943, #65527, #12287, .T. ) ;
#24006 =( NAMED_UNIT ( * ) SI_UNIT ( $, .STERADIAN. ) SOLID_ANGLE_UNIT ( ) );
#24007 = CARTESIAN_POINT ( 'NONE',  ( 0.000000000000000000, 50.00000000000000000, -60.00000000000000000 ) ) ;
#24008 = LINE ( 'NONE', #66936, #44920 ) ;
#24009 = LINE ( 'NONE', #3547, #51018 ) ;
#24010 = ORIENTED_EDGE ( 'NONE', *, *, #64385, .F. ) ;
#24011 = CARTESIAN_POINT ( 'NONE',  ( -159.6550000000000011, -7.632228543268600340, -2.479861379858950166 ) ) ;
#24012 = AXIS2_PLACEMENT_3D ( 'NONE', #22759, #6914, #17504 ) ;
#24013 = ORIENTED_EDGE ( 'NONE', *, *, #62717, .F. ) ;
#24014 = FILL_AREA_STYLE_COLOUR ( '', #15586 ) ;
#24015 = DIRECTION ( 'NONE',  ( 1.000000000000000000, 0.000000000000000000, 0.000000000000000000 ) ) ;
#24016 = ORIENTED_EDGE ( 'NONE', *, *, #2904, .T. ) ;
#24017 = FACE_OUTER_BOUND ( 'NONE', #69387, .T. ) ;
#24018 = FACE_OUTER_BOUND ( 'NONE', #35787, .T. ) ;
#24019 = CARTESIAN_POINT ( 'NONE',  ( 5.598654528085805993, 111.2449999999999761, 7.705886871421374629 ) ) ;
#24020 = VECTOR ( 'NONE', #47912, 1000.000000000000227 ) ;
#24021 = ORIENTED_EDGE ( 'NONE', *, *, #5273, .F. ) ;
#24022 = SURFACE_STYLE_FILL_AREA ( #40574 ) ;
#24023 = CARTESIAN_POINT ( 'NONE',  ( -3.094860106618432471, 110.7049999999999983, -9.525000000000000355 ) ) ;
#24024 = CARTESIAN_POINT ( 'NONE',  ( -74.45499999999999829, 7.632228543268599452, -2.479861379858951942 ) ) ;
#24025 = FILL_AREA_STYLE_COLOUR ( '', #34266 ) ;
#24026 = CARTESIAN_POINT ( 'NONE',  ( 10.01517768586949231, 127.8050000000000068, 1.839758294383810543E-15 ) ) ;
#24027 = CARTESIAN_POINT ( 'NONE',  ( 20.58910881788679603, 114.8399099445016276, 10.00000000000000355 ) ) ;
#24028 = STYLED_ITEM ( 'NONE', ( #25389 ), #38079 ) ;
#24029 = CARTESIAN_POINT ( 'NONE',  ( -85.94292637653380496, 0.000000000000000000, 9.524999999999991473 ) ) ;
#24030 =( NAMED_UNIT ( * ) SI_UNIT ( $, .STERADIAN. ) SOLID_ANGLE_UNIT ( ) );
#24031 = VERTEX_POINT ( 'NONE', #22179 ) ;
#24033 = PRESENTATION_STYLE_ASSIGNMENT (( #56030 ) ) ;
#24032 = TOROIDAL_SURFACE ( 'NONE', #63355, 1.000000000000000000, 0.5000000000000000000 ) ;
#24034 = CARTESIAN_POINT ( 'NONE',  ( -56.09499999999997044, -2.607480562269071545, -8.024999999999991473 ) ) ;
#24035 = ORIENTED_EDGE ( 'NONE', *, *, #25255, .F. ) ;
#24036 = CARTESIAN_POINT ( 'NONE',  ( -71.75000000000000000, 4.336808689942018722E-16, 19.00000000000000000 ) ) ;
#24037 = COLOUR_RGB ( '', 0.66274510, 0.83137255, 0.94901961) ;
#24038 = EDGE_CURVE ( 'NONE', #34838, #33800, #61963, .T. ) ;
#24039 = CARTESIAN_POINT ( 'NONE',  ( 15.00000000000000000, 8.000000000000000000, -4.000000000000000000 ) ) ;
#24040 = CARTESIAN_POINT ( 'NONE',  ( -67.49999999999998579, -1.932193735051945844E-14, -11.50000000000000000 ) ) ;
#24041 = AXIS2_PLACEMENT_3D ( 'NONE', #35942, #57742, #9572 ) ;
#24042 = CARTESIAN_POINT ( 'NONE',  ( 25.75000000000001066, 21.74999999999998224, -3.750000000000000000 ) ) ;
#24043 = ORIENTED_EDGE ( 'NONE', *, *, #39429, .F. ) ;
#24044 = FACE_OUTER_BOUND ( 'NONE', #35562, .T. ) ;
#24045 = CARTESIAN_POINT ( 'NONE',  ( -52.49499999999999034, 6.826472737025113702, -4.959722759717902107 ) ) ;
#24046 =( NAMED_UNIT ( * ) PLANE_ANGLE_UNIT ( ) SI_UNIT ( $, .RADIAN. ) );
#24047 = ORIENTED_EDGE ( 'NONE', *, *, #2940, .F. ) ;
#24048 = CARTESIAN_POINT ( 'NONE',  ( -75.00000000000000000, 8.547452476118923670, 5.556748833514874697 ) ) ;
#24049 = CARTESIAN_POINT ( 'NONE',  ( -103.5549999999999926, 0.000000000000000000, 8.024999999999991473 ) ) ;
#24050 = ORIENTED_EDGE ( 'NONE', *, *, #11129, .T. ) ;
#24051 = DIRECTION ( 'NONE',  ( 1.000000000000000000, 0.000000000000000000, 0.000000000000000000 ) ) ;
#24052 = CARTESIAN_POINT ( 'NONE',  ( -195.0000000000000000, 0.000000000000000000, 0.000000000000000000 ) ) ;
#24053 = CARTESIAN_POINT ( 'NONE',  ( -143.7570736234661695, -5.598654528085801552, 7.705886871421367523 ) ) ;
#24054 = STYLED_ITEM ( 'NONE', ( #64435 ), #2613 ) ;
#24055 = CARTESIAN_POINT ( 'NONE',  ( 0.000000000000000000, 154.4999999999999432, -23.00000000000000000 ) ) ;
#24056 = CARTESIAN_POINT ( 'NONE',  ( -3.094860106618434248, 137.7949999999999875, 9.525000000000000355 ) ) ;
#24057 = CARTESIAN_POINT ( 'NONE',  ( -81.50707362346615525, 8.102448949553176405, 5.886773742842740909 ) ) ;
#24058 =( GEOMETRIC_REPRESENTATION_CONTEXT ( 3 ) GLOBAL_UNCERTAINTY_ASSIGNED_CONTEXT ( ( #20050 ) ) GLOBAL_UNIT_ASSIGNED_CONTEXT ( ( #46675, #25496, #62084 ) ) REPRESENTATION_CONTEXT ( 'NONE', 'WORKASPACE' ) );
#24059 = EDGE_CURVE ( 'NONE', #35967, #12421, #33537, .T. ) ;
#24060 = DIRECTION ( 'NONE',  ( 0.000000000000000000, 0.000000000000000000, 1.000000000000000000 ) ) ;
#24061 =( NAMED_UNIT ( * ) SI_UNIT ( $, .STERADIAN. ) SOLID_ANGLE_UNIT ( ) );
#24062 = SURFACE_STYLE_FILL_AREA ( #50453 ) ;
#24063 = CARTESIAN_POINT ( 'NONE',  ( 6.826472737025119919, 120.0070736234661410, 4.959722759717908325 ) ) ;
#24064 = EDGE_CURVE ( 'NONE', #15837, #64993, #50302, .T. ) ;
#24065 = AXIS2_PLACEMENT_3D ( 'NONE', #4218, #58088, #20436 ) ;
#24066 = CARTESIAN_POINT ( 'NONE',  ( -117.9549999999999841, -7.632228543268599452, 2.479861379858951054 ) ) ;
#24067 = EDGE_CURVE ( 'NONE', #42007, #25839, #45056, .T. ) ;
#24068 = CARTESIAN_POINT ( 'NONE',  ( 3.249999999999999556, 34.24999999999998579, 3.750000000000000000 ) ) ;
#24069 = CARTESIAN_POINT ( 'NONE',  ( -136.9449999999999932, -9.827790563157499189E-16, -8.024999999999991473 ) ) ;
#24070 = CIRCLE ( 'NONE', #56665, 3.499999999999999556 ) ;
#24071 = AXIS2_PLACEMENT_3D ( 'NONE', #43197, #11111, #22034 ) ;
#24072 = CARTESIAN_POINT ( 'NONE',  ( -120.8949999999999818, 6.826472737025115478, 4.959722759717899443 ) ) ;
#24073 = LINE ( 'NONE', #8255, #49348 ) ;
#24074 = EDGE_LOOP ( 'NONE', ( #59925, #17922, #11560, #22276 ) ) ;
#24075 = CARTESIAN_POINT ( 'NONE',  ( -195.0000000000000000, 1.469576158976823553E-15, -11.99999999999999645 ) ) ;
#24076 = DIRECTION ( 'NONE',  ( 0.000000000000000000, 1.000000000000000000, 0.000000000000000000 ) ) ;
#24077 = EDGE_CURVE ( 'NONE', #2411, #16463, #8097, .T. ) ;
#24078 = CARTESIAN_POINT ( 'NONE',  ( -121.6429263765338078, -5.598654528085801552, 7.705886871421367523 ) ) ;
#24079 = CARTESIAN_POINT ( 'NONE',  ( -171.2929263765338135, 3.094860106618428031, -9.524999999999993250 ) ) ;
#24080 = CARTESIAN_POINT ( 'NONE',  ( -52.04499999999998039, 7.632228543268600340, 2.479861379858949277 ) ) ;
#24081 = EDGE_CURVE ( 'NONE', #7106, #35167, #29425, .T. ) ;
#24082 = VECTOR ( 'NONE', #45428, 1000.000000000000000 ) ;
#24083 = DIRECTION ( 'NONE',  ( -0.000000000000000000, -0.000000000000000000, -1.000000000000000000 ) ) ;
#24084 = VECTOR ( 'NONE', #60298, 1000.000000000000000 ) ;
#24085 =( LENGTH_UNIT ( ) NAMED_UNIT ( * ) SI_UNIT ( .MILLI., .METRE. ) );
#24086 = CARTESIAN_POINT ( 'NONE',  ( -1.953228634907021810, 72.00000000000001421, 6.349999999999997868 ) ) ;
#24087 = VERTEX_POINT ( 'NONE', #44378 ) ;
#24088 = CARTESIAN_POINT ( 'NONE',  ( -93.29292637653379927, 3.094860106618428031, -9.524999999999993250 ) ) ;
#24089 = SURFACE_STYLE_FILL_AREA ( #8617 ) ;
#24090 = AXIS2_PLACEMENT_3D ( 'NONE', #62223, #24244, #66466 ) ;
#24091 = CARTESIAN_POINT ( 'NONE',  ( 6.735557395310443995E-16, 2.500000000000000000, -5.500000000000001776 ) ) ;
#24092 = CARTESIAN_POINT ( 'NONE',  ( 44.99999999999977973, 149.9999999999999716, 10.00000000000000000 ) ) ;
#24093 = CIRCLE ( 'NONE', #17400, 2.500000000000002220 ) ;
#24094 = CARTESIAN_POINT ( 'NONE',  ( -156.9570736234661581, 9.058813317711329915, -2.943386871421373119 ) ) ;
#24095 = ORIENTED_EDGE ( 'NONE', *, *, #3774, .F. ) ;
#24096 = LINE ( 'NONE', #51518, #6654 ) ;
#24097 =( LENGTH_UNIT ( ) NAMED_UNIT ( * ) SI_UNIT ( .MILLI., .METRE. ) );
#24098 = CARTESIAN_POINT ( 'NONE',  ( -55.75572903516371071, -8.276929449822308271, -1.923638504044224318 ) ) ;
#24099 = ORIENTED_EDGE ( 'NONE', *, *, #65617, .F. ) ;
#24100 = CARTESIAN_POINT ( 'NONE',  ( -64.64292637653379359, -5.598654528085801552, 7.705886871421367523 ) ) ;
#24101 = EDGE_CURVE ( 'NONE', #10939, #28531, #44045, .T. ) ;
#24102 = CARTESIAN_POINT ( 'NONE',  ( 0.000000000000000000, 136.0570736234661808, -8.025000000000000355 ) ) ;
#24103 = AXIS2_PLACEMENT_3D ( 'NONE', #37361, #48243, #21830 ) ;
#24104 = AXIS2_PLACEMENT_3D ( 'NONE', #53707, #59676, #15764 ) ;
#24105 = CARTESIAN_POINT ( 'NONE',  ( 44.25000000000000000, 21.74999999999998579, -3.750000000000000000 ) ) ;
#24106 = FACE_OUTER_BOUND ( 'NONE', #33707, .T. ) ;
#24107 = CARTESIAN_POINT ( 'NONE',  ( -24.00000000000000000, 1.000000000000000000, 3.000000000000000000 ) ) ;
#24108 = VERTEX_POINT ( 'NONE', #23223 ) ;
#24109 = LINE ( 'NONE', #45613, #37733 ) ;
#24110 = VECTOR ( 'NONE', #14366, 1000.000000000000000 ) ;
#24111 = CARTESIAN_POINT ( 'NONE',  ( -104.0070736234661553, -8.102448949553174629, -5.886773742842741797 ) ) ;
#24112 = DIRECTION ( 'NONE',  ( 0.000000000000000000, 0.000000000000000000, 1.000000000000000000 ) ) ;
#24113 = TOROIDAL_SURFACE ( 'NONE', #30830, 16.50000000000000000, 0.5000000000000000000 ) ;
#24114 = STYLED_ITEM ( 'NONE', ( #16363 ), #62317 ) ;
#24115 = CARTESIAN_POINT ( 'NONE',  ( -84.89499999999996760, 6.826472737025116366, 4.959722759717898555 ) ) ;
#24116 = VERTEX_POINT ( 'NONE', #11618 ) ;
#24117 = FILL_AREA_STYLE_COLOUR ( '', #31033 ) ;
#24118 = CYLINDRICAL_SURFACE ( 'NONE', #34150, 3.499999999999999556 ) ;
#24119 = UNCERTAINTY_MEASURE_WITH_UNIT (LENGTH_MEASURE( 1.000000000000000082E-05 ), #20669, 'distance_accuracy_value', 'NONE');
#24120 = VERTEX_POINT ( 'NONE', #22879 ) ;
#24121 = PRESENTATION_STYLE_ASSIGNMENT (( #61393 ) ) ;
#24122 = MECHANICAL_DESIGN_GEOMETRIC_PRESENTATION_REPRESENTATION (  '', ( #44426 ), #60071 ) ;
#24123 = FACE_OUTER_BOUND ( 'NONE', #14107, .T. ) ;
#24124 = VECTOR ( 'NONE', #35358, 1000.000000000000000 ) ;
#24125 = ORIENTED_EDGE ( 'NONE', *, *, #31260, .F. ) ;
#24126 = EDGE_CURVE ( 'NONE', #42981, #46203, #14236, .T. ) ;
#24127 = CYLINDRICAL_SURFACE ( 'NONE', #21840, 0.5000000000000004441 ) ;
#24128 = ORIENTED_EDGE ( 'NONE', *, *, #33659, .F. ) ;
#24129 = CARTESIAN_POINT ( 'NONE',  ( -167.7570736234661695, -5.598654528085801552, 7.705886871421367523 ) ) ;
#24130 = CARTESIAN_POINT ( 'NONE',  ( -13.23915246117191025, 52.65078610323165265, -6.947530358905292580 ) ) ;
#24131 = CARTESIAN_POINT ( 'NONE',  ( 3.094860106618431583, 117.0949999999999847, 9.525000000000000355 ) ) ;
#24132 = VECTOR ( 'NONE', #42665, 1000.000000000000000 ) ;
#24133 = CARTESIAN_POINT ( 'NONE',  ( -116.1570736234661751, -9.058813317711329915, -2.943386871421370898 ) ) ;
#24134 = EDGE_CURVE ( 'NONE', #36214, #62297, #52995, .T. ) ;
#24135 = CARTESIAN_POINT ( 'NONE',  ( -183.2329476844139720, 2.873132234127047102, -8.866736753779713709 ) ) ;
#24136 = CIRCLE ( 'NONE', #30856, 5.500000000000005329 ) ;
#24137 = CARTESIAN_POINT ( 'NONE',  ( 3.000000000000029754, 42.58578643762690774, 80.00402776293826435 ) ) ;
#24138 = ORIENTED_EDGE ( 'NONE', *, *, #60025, .T. ) ;
#24139 = CARTESIAN_POINT ( 'NONE',  ( 0.000000000000000000, 42.00000000000000711, 44.99999999999999289 ) ) ;
#24140 = PRESENTATION_STYLE_ASSIGNMENT (( #7282 ) ) ;
#24141 = CARTESIAN_POINT ( 'NONE',  ( 25.00000000000001421, 43.00000000000000000, 0.000000000000000000 ) ) ;
#24142 = EDGE_CURVE ( 'NONE', #25552, #30753, #13664, .T. ) ;
#24143 = CARTESIAN_POINT ( 'NONE',  ( -149.1549999999999727, 7.632228543268600340, 2.479861379858949277 ) ) ;
#24144 = CARTESIAN_POINT ( 'NONE',  ( -165.7450000000000045, 4.716976649647094177, 6.492361379858945902 ) ) ;
#24145 = CARTESIAN_POINT ( 'NONE',  ( -147.4449999999999932, 0.000000000000000000, 8.024999999999991473 ) ) ;
#24146 = ORIENTED_EDGE ( 'NONE', *, *, #45391, .T. ) ;
#24147 = AXIS2_PLACEMENT_3D ( 'NONE', #10839, #48164, #48511 ) ;
#24148 = CARTESIAN_POINT ( 'NONE',  ( -67.04292637653381348, -9.058813317711329915, -2.943386871421370898 ) ) ;
#24149 =( NAMED_UNIT ( * ) PLANE_ANGLE_UNIT ( ) SI_UNIT ( $, .RADIAN. ) );
#24150 = DIRECTION ( 'NONE',  ( -1.000000000000000000, -7.709882115452468306E-16, 0.000000000000000000 ) ) ;
#24151 = CARTESIAN_POINT ( 'NONE',  ( -72.05499999999997840, -9.827790563157499189E-16, -8.024999999999991473 ) ) ;
#24152 = CARTESIAN_POINT ( 'NONE',  ( 0.000000000000000000, 42.00000000000000000, 36.50000000000000000 ) ) ;
#24153 = DIRECTION ( 'NONE',  ( 0.000000000000000000, 0.000000000000000000, 1.000000000000000000 ) ) ;
#24154 = EDGE_CURVE ( 'NONE', #10212, #49424, #63142, .T. ) ;
#24155 = AXIS2_PLACEMENT_3D ( 'NONE', #32906, #6845, #28268 ) ;
#24156 = CARTESIAN_POINT ( 'NONE',  ( -72.29499999999998749, -2.607480562269069768, 8.024999999999991473 ) ) ;
#24157 = CARTESIAN_POINT ( 'NONE',  ( 10.01517768586949231, 148.8050000000000068, 1.839758294383810543E-15 ) ) ;
#24158 = CARTESIAN_POINT ( 'NONE',  ( -195.0000000000000000, 0.000000000000000000, 0.000000000000000000 ) ) ;
#24159 = STYLED_ITEM ( 'NONE', ( #49207 ), #49121 ) ;
#24160 = CARTESIAN_POINT ( 'NONE',  ( 0.000000000000000000, 154.5000000000000000, -9.524999999999998579 ) ) ;
#24161 = UNCERTAINTY_MEASURE_WITH_UNIT (LENGTH_MEASURE( 1.000000000000000082E-05 ), #18113, 'distance_accuracy_value', 'NONE');
#24162 = CARTESIAN_POINT ( 'NONE',  ( -20.07516809221520404, 115.0406803144924766, -9.999999999999998224 ) ) ;
#24163 = CARTESIAN_POINT ( 'NONE',  ( -3.906371588338814149, 110.6892254832438311, 8.486918976161996753 ) ) ;
#24164 = CARTESIAN_POINT ( 'NONE',  ( 0.000000000000000000, 30.74999999999999289, 4.000000000000000000 ) ) ;
#24165 = AXIS2_PLACEMENT_3D ( 'NONE', #44816, #55325, #65890 ) ;
#24166 = CARTESIAN_POINT ( 'NONE',  ( 60.00000000000000000, 1.797044900979284448E-15, 11.50000000000003730 ) ) ;
#24167 = VECTOR ( 'NONE', #34502, 1000.000000000000000 ) ;
#24168 = CARTESIAN_POINT ( 'NONE',  ( -195.0000000000000000, 0.000000000000000000, 0.000000000000000000 ) ) ;
#24169 = SURFACE_STYLE_USAGE ( .BOTH. , #40371 ) ;
#24170 = ORIENTED_EDGE ( 'NONE', *, *, #37794, .F. ) ;
#24171 = ORIENTED_EDGE ( 'NONE', *, *, #68633, .T. ) ;
#24172 =( NAMED_UNIT ( * ) SI_UNIT ( $, .STERADIAN. ) SOLID_ANGLE_UNIT ( ) );
#24173 = ADVANCED_FACE ( 'NONE', ( #14611 ), #20577, .F. ) ;
#24175 = LINE ( 'NONE', #21859, #23 ) ;
#24174 = VECTOR ( 'NONE', #62940, 1000.000000000000000 ) ;
#24176 = COLOUR_RGB ( '', 0.08235294, 0.09019608, 0.10196078) ;
#24177 = SURFACE_STYLE_FILL_AREA ( #24502 ) ;
#24178 = ORIENTED_EDGE ( 'NONE', *, *, #21690, .F. ) ;
#24179 = EDGE_LOOP ( 'NONE', ( #61646, #6000, #67328, #6835 ) ) ;
#24180 = DIRECTION ( 'NONE',  ( 5.782411586589351722E-16, -1.000000000000000000, 0.000000000000000000 ) ) ;
#24181 = VERTEX_POINT ( 'NONE', #42094 ) ;
#24182 = CARTESIAN_POINT ( 'NONE',  ( -4.041451884327381450, 7.000000000000006217, 1.082903768654761345 ) ) ;
#24183 = ORIENTED_EDGE ( 'NONE', *, *, #29777, .F. ) ;
#24184 = CARTESIAN_POINT ( 'NONE',  ( -16.75000000000000000, -4.000000000000000000, 20.00000000000000000 ) ) ;
#24185 = DIRECTION ( 'NONE',  ( -1.000000000000000000, 0.000000000000000000, 0.000000000000000000 ) ) ;
#24186 = CARTESIAN_POINT ( 'NONE',  ( -114.2950000000000017, -2.607480562269069768, 8.024999999999991473 ) ) ;
#24187 = ORIENTED_EDGE ( 'NONE', *, *, #38101, .T. ) ;
#24188 = AXIS2_PLACEMENT_3D ( 'NONE', #40956, #62694, #63420 ) ;
#24189 = CIRCLE ( 'NONE', #25305, 8.500000000000000000 ) ;
#24190 = CARTESIAN_POINT ( 'NONE',  ( -6.724421053716080898, 110.4999999999999574, -6.760127308664230839 ) ) ;
#24191 = CARTESIAN_POINT ( 'NONE',  ( -54.14292637653381490, 5.598654528085800663, -7.705886871421367523 ) ) ;
#24192 = CARTESIAN_POINT ( 'NONE',  ( -11.23428045036074252, -11.53834988893305713, 3.305092309263673034 ) ) ;
#24193 = CARTESIAN_POINT ( 'NONE',  ( -179.9070736234662604, -3.094860106617838280, 9.525000000000423128 ) ) ;
#24194 = ORIENTED_EDGE ( 'NONE', *, *, #42809, .F. ) ;
#24195 = CARTESIAN_POINT ( 'NONE',  ( -6.826472737025120807, 147.9929263765338305, 4.959722759717906548 ) ) ;
#24196 = CYLINDRICAL_SURFACE ( 'NONE', #61450, 3.100000000000003642 ) ;
#24197 = VECTOR ( 'NONE', #47598, 1000.000000000000000 ) ;
#24198 = PRESENTATION_STYLE_ASSIGNMENT (( #2707 ) ) ;
#24199 = VERTEX_POINT ( 'NONE', #53294 ) ;
#24200 = EDGE_CURVE ( 'NONE', #19239, #4086, #22665, .T. ) ;
#24201 = DIRECTION ( 'NONE',  ( 0.7071067811865549002, 0.000000000000000000, 0.7071067811865401342 ) ) ;
#24202 = ORIENTED_EDGE ( 'NONE', *, *, #24313, .T. ) ;
#24203 =( NAMED_UNIT ( * ) PLANE_ANGLE_UNIT ( ) SI_UNIT ( $, .RADIAN. ) );
#24204 = LINE ( 'NONE', #45022, #8286 ) ;
#24205 = DIRECTION ( 'NONE',  ( 0.000000000000000000, -0.000000000000000000, 1.000000000000000000 ) ) ;
#24206 = AXIS2_PLACEMENT_3D ( 'NONE', #57987, #63924, #9803 ) ;
#24207 = CARTESIAN_POINT ( 'NONE',  ( -134.7549999999999955, 4.716976649647091513, -6.492361379858946790 ) ) ;
#24208 = DIRECTION ( 'NONE',  ( 0.000000000000000000, 0.000000000000000000, 1.000000000000000000 ) ) ;
#24209 = CARTESIAN_POINT ( 'NONE',  ( -10.39230484541327293, 3.469446951953614189E-15, 7.500000000000000000 ) ) ;
#24210 = ORIENTED_EDGE ( 'NONE', *, *, #60737, .T. ) ;
#24211 = LINE ( 'NONE', #66799, #13782 ) ;
#24212 = FILL_AREA_STYLE ('',( #50961 ) ) ;
#24213 = FILL_AREA_STYLE ('',( #39059 ) ) ;
#24214 = VERTEX_POINT ( 'NONE', #15664 ) ;
#24215 = EDGE_LOOP ( 'NONE', ( #31893, #27200, #68750 ) ) ;
#24216 = FILL_AREA_STYLE ('',( #19272 ) ) ;
#24217 = CARTESIAN_POINT ( 'NONE',  ( -21.02379604162863558, 114.6405644170961153, 10.00000000000000000 ) ) ;
#24218 = DIRECTION ( 'NONE',  ( 0.000000000000000000, 0.000000000000000000, -1.000000000000000000 ) ) ;
#24219 = CARTESIAN_POINT ( 'NONE',  ( -49.25499999999999545, -4.716976649647092401, 6.492361379858946790 ) ) ;
#24221 = EDGE_LOOP ( 'NONE', ( #2081, #7598, #43054, #44031 ) ) ;
#24220 = STYLED_ITEM ( 'NONE', ( #58123 ), #39202 ) ;
#24222 = FILL_AREA_STYLE ('',( #35131 ) ) ;
#24223 = EDGE_CURVE ( 'NONE', #6919, #51912, #38485, .T. ) ;
#24224 = CARTESIAN_POINT ( 'NONE',  ( -182.1549999999999727, 7.632228543268600340, 2.479861379858949277 ) ) ;
#24225 = SURFACE_SIDE_STYLE ('',( #33734 ) ) ;
#24226 = AXIS2_PLACEMENT_3D ( 'NONE', #39380, #45014, #66068 ) ;
#24227 = CARTESIAN_POINT ( 'NONE',  ( -58.25707362346617657, 5.598654528085800663, -7.705886871421367523 ) ) ;
#24228 = EDGE_CURVE ( 'NONE', #34547, #47241, #58606, .T. ) ;
#24229 =( NAMED_UNIT ( * ) SI_UNIT ( $, .STERADIAN. ) SOLID_ANGLE_UNIT ( ) );
#24230 = CIRCLE ( 'NONE', #13038, 3.499999999999999556 ) ;
#24231 = ORIENTED_EDGE ( 'NONE', *, *, #5247, .T. ) ;
#24232 = DIRECTION ( 'NONE',  ( 1.000000000000000000, 0.000000000000000000, -1.300977106640434891E-16 ) ) ;
#24233 = EDGE_CURVE ( 'NONE', #5366, #54390, #25845, .T. ) ;
#24234 = CARTESIAN_POINT ( 'NONE',  ( -3.000000000000000444, 0.000000000000000000, 52.50000000000000000 ) ) ;
#24235 = AXIS2_PLACEMENT_3D ( 'NONE', #37109, #58515, #10345 ) ;
#24236 = CARTESIAN_POINT ( 'NONE',  ( 2.607480562269128388, 117.9070736234661609, -8.024999999999963052 ) ) ;
#24237 = CARTESIAN_POINT ( 'NONE',  ( -101.6049999999999898, 6.826472737025113702, -4.959722759717902107 ) ) ;
#24238 = CARTESIAN_POINT ( 'NONE',  ( -30.01048380477565658, -8.499999999999998224, -0.6003161102123087955 ) ) ;
#24239 = SURFACE_STYLE_USAGE ( .BOTH. , #14043 ) ;
#24240 = ADVANCED_FACE ( 'NONE', ( #15343 ), #63129, .F. ) ;
#24241 = CARTESIAN_POINT ( 'NONE',  ( -104.6949999999999790, -8.437984349512086979, 5.166775262442717831E-16 ) ) ;
#24242 = CARTESIAN_POINT ( 'NONE',  ( -9.058813317711337021, 120.1549999999999869, -2.943386871421374895 ) ) ;
#24243 = CARTESIAN_POINT ( 'NONE',  ( -69.14499999999998181, -4.716976649647092401, 6.492361379858946790 ) ) ;
#24244 = DIRECTION ( 'NONE',  ( 0.000000000000000000, 0.000000000000000000, -1.000000000000000000 ) ) ;
#24245 = DIRECTION ( 'NONE',  ( 0.000000000000000000, 0.000000000000000000, 1.000000000000000000 ) ) ;
#24246 = UNCERTAINTY_MEASURE_WITH_UNIT (LENGTH_MEASURE( 1.000000000000000082E-05 ), #17404, 'distance_accuracy_value', 'NONE');
#24247 = DIRECTION ( 'NONE',  ( -1.000000000000000000, 0.000000000000000000, -0.000000000000000000 ) ) ;
#24248 = AXIS2_PLACEMENT_3D ( 'NONE', #21276, #53326, #32520 ) ;
#24249 = DIRECTION ( 'NONE',  ( -0.000000000000000000, -1.000000000000000000, 0.000000000000000000 ) ) ;
#24250 = VERTEX_POINT ( 'NONE', #69127 ) ;
#24251 = CARTESIAN_POINT ( 'NONE',  ( -112.6429263765338078, -5.598654528085801552, 7.705886871421367523 ) ) ;
#24252 = CARTESIAN_POINT ( 'NONE',  ( -135.1449999999999818, -4.716976649647092401, 6.492361379858946790 ) ) ;
#24253 = VECTOR ( 'NONE', #31693, 1000.000000000000000 ) ;
#24254 = CYLINDRICAL_SURFACE ( 'NONE', #20164, 9.524999999999991473 ) ;
#24255 = CARTESIAN_POINT ( 'NONE',  ( -45.00000000000000000, 1.166476076187854022E-15, -9.525000000000000355 ) ) ;
#24257 = CIRCLE ( 'NONE', #57972, 0.9999999999999995559 ) ;
#24256 = CARTESIAN_POINT ( 'NONE',  ( 19.89974874213240597, 115.4999999999999574, -10.50000000000000000 ) ) ;
#24258 = EDGE_LOOP ( 'NONE', ( #26357, #52465, #49956, #50667 ) ) ;
#24259 = VERTEX_POINT ( 'NONE', #52612 ) ;
#24260 = AXIS2_PLACEMENT_3D ( 'NONE', #44611, #13576, #35045 ) ;
#24261 = CARTESIAN_POINT ( 'NONE',  ( 28.00000000000002842, 43.00000000000000000, 90.00000000000000000 ) ) ;
#24262 = FILL_AREA_STYLE_COLOUR ( '', #34933 ) ;
#24263 = CARTESIAN_POINT ( 'NONE',  ( 23.21231517720797655, 117.9999999999999716, -7.000000000000000000 ) ) ;
#24264 = DIRECTION ( 'NONE',  ( -0.000000000000000000, -1.000000000000000000, -0.000000000000000000 ) ) ;
#24265 = CARTESIAN_POINT ( 'NONE',  ( -22.75000000000000711, 36.75000000000000000, 3.750000000000000000 ) ) ;
#24266 = ORIENTED_EDGE ( 'NONE', *, *, #22312, .T. ) ;
#24267 = CARTESIAN_POINT ( 'NONE',  ( -128.1550000000000011, 7.632228543268600340, 2.479861379858949277 ) ) ;
#24268 = EDGE_LOOP ( 'NONE', ( #8910, #24128, #29360, #26295 ) ) ;
#24269 = CARTESIAN_POINT ( 'NONE',  ( 98.00000000000000000, 16.00000000000000000, 0.000000000000000000 ) ) ;
#24270 = CIRCLE ( 'NONE', #1782, 0.5000000000000004441 ) ;
#24271 = CARTESIAN_POINT ( 'NONE',  ( -123.9570736234661723, 9.058813317711329915, -2.943386871421373119 ) ) ;
#24272 = ORIENTED_EDGE ( 'NONE', *, *, #23649, .F. ) ;
#24273 = CARTESIAN_POINT ( 'NONE',  ( 44.36184162591897717, 10.11502268137275351, -3.500000000000000000 ) ) ;
#24274 = ORIENTED_EDGE ( 'NONE', *, *, #10087, .T. ) ;
#24275 = PRESENTATION_LAYER_ASSIGNMENT (  '', '', ( #20930 ) ) ;
#24276 = CARTESIAN_POINT ( 'NONE',  ( 0.000000000000000000, 0.000000000000000000, 0.000000000000000000 ) ) ;
#24277 = CARTESIAN_POINT ( 'NONE',  ( 8.102448949553181734, 144.3950000000000102, 5.886773742842750679 ) ) ;
#24278 = FILL_AREA_STYLE ('',( #3837 ) ) ;
#24279 = TOROIDAL_SURFACE ( 'NONE', #2754, 18.53939201416945082, 5.000000000000000000 ) ;
#24280 = EDGE_LOOP ( 'NONE', ( #11567, #15585, #69043, #67442, #34726 ) ) ;
#24281 = CYLINDRICAL_SURFACE ( 'NONE', #27394, 1.000000000000000000 ) ;
#24282 = CARTESIAN_POINT ( 'NONE',  ( 3.094860106618431583, 139.2050000000000125, 9.525000000000000355 ) ) ;
#24283 = ORIENTED_EDGE ( 'NONE', *, *, #68539, .F. ) ;
#24284 = CARTESIAN_POINT ( 'NONE',  ( -4.716976649647098618, 118.1429263765338078, 6.492361379858953008 ) ) ;
#24285 = CARTESIAN_POINT ( 'NONE',  ( -74.99999999999998579, 50.00000000000000000, 7.000000000000000000 ) ) ;
#24286 = UNCERTAINTY_MEASURE_WITH_UNIT (LENGTH_MEASURE( 1.000000000000000082E-05 ), #62426, 'distance_accuracy_value', 'NONE');
#24287 = FACE_OUTER_BOUND ( 'NONE', #19707, .T. ) ;
#24288 = LINE ( 'NONE', #29919, #46361 ) ;
#24289 = CARTESIAN_POINT ( 'NONE',  ( -4.041451884327378785, 2.500000000000000000, 7.000000000000000000 ) ) ;
#24290 = ORIENTED_EDGE ( 'NONE', *, *, #59802, .F. ) ;
#24291 = ADVANCED_FACE ( 'NONE', ( #51907 ), #25159, .T. ) ;
#24292 = CARTESIAN_POINT ( 'NONE',  ( 71.99999999999998579, 64.07124727947029896, -7.000000000000000000 ) ) ;
#24293 = ORIENTED_EDGE ( 'NONE', *, *, #9491, .F. ) ;
#24294 = SPHERICAL_SURFACE ( 'NONE', #38190, 0.2500000000000000000 ) ;
#24295 = LINE ( 'NONE', #19001, #21051 ) ;
#24296 = LINE ( 'NONE', #23608, #54255 ) ;
#24297 = CARTESIAN_POINT ( 'NONE',  ( -161.6050000000000182, 6.826472737025113702, -4.959722759717902107 ) ) ;
#24298 = ORIENTED_EDGE ( 'NONE', *, *, #332, .T. ) ;
#24299 =( NAMED_UNIT ( * ) SI_UNIT ( $, .STERADIAN. ) SOLID_ANGLE_UNIT ( ) );
#24300 = UNCERTAINTY_MEASURE_WITH_UNIT (LENGTH_MEASURE( 1.000000000000000082E-05 ), #66822, 'distance_accuracy_value', 'NONE');
#24301 = EDGE_CURVE ( 'NONE', #60790, #6587, #5817, .T. ) ;
#24302 = ADVANCED_FACE ( 'NONE', ( #9703, #36798 ), #38875, .T. ) ;
#24303 = CARTESIAN_POINT ( 'NONE',  ( 71.50000000000000000, 14.49137674618942562, 7.000000000000000000 ) ) ;
#24304 = CARTESIAN_POINT ( 'NONE',  ( 45.65811388300841855, 10.21937129433612235, -5.999999999999999112 ) ) ;
#24305 =( NAMED_UNIT ( * ) SI_UNIT ( $, .STERADIAN. ) SOLID_ANGLE_UNIT ( ) );
#24306 = ORIENTED_EDGE ( 'NONE', *, *, #47317, .T. ) ;
#24307 = EDGE_CURVE ( 'NONE', #40140, #7265, #39568, .T. ) ;
#24308 = ORIENTED_EDGE ( 'NONE', *, *, #8684, .T. ) ;
#24309 = FILL_AREA_STYLE_COLOUR ( '', #59693 ) ;
#24310 = DIRECTION ( 'NONE',  ( 0.000000000000000000, 0.000000000000000000, -1.000000000000000000 ) ) ;
#24311 = CARTESIAN_POINT ( 'NONE',  ( -79.55499999999999261, 0.000000000000000000, 8.024999999999991473 ) ) ;
#24312 = ORIENTED_EDGE ( 'NONE', *, *, #43869, .T. ) ;
#24313 = EDGE_CURVE ( 'NONE', #67765, #38434, #58910, .T. ) ;
#24314 = CARTESIAN_POINT ( 'NONE',  ( -44.50000000000000000, 10.49999999999998579, 4.000000000000000000 ) ) ;
#24315 = ADVANCED_FACE ( 'NONE', ( #54982 ), #22302, .T. ) ;
#24316 =( GEOMETRIC_REPRESENTATION_CONTEXT ( 3 ) GLOBAL_UNCERTAINTY_ASSIGNED_CONTEXT ( ( #1523 ) ) GLOBAL_UNIT_ASSIGNED_CONTEXT ( ( #37418, #27474, #59142 ) ) REPRESENTATION_CONTEXT ( 'NONE', 'WORKASPACE' ) );
#24317 = CARTESIAN_POINT ( 'NONE',  ( 6.000000000000017764, 43.00000000000000000, -29.06445261836602256 ) ) ;
#24318 = EDGE_CURVE ( 'NONE', #60144, #49636, #53954, .T. ) ;
#24319 = CARTESIAN_POINT ( 'NONE',  ( -75.00000000000000000, 9.675769070491714530, -6.195678411461598145 ) ) ;
#24320 = ORIENTED_EDGE ( 'NONE', *, *, #44917, .F. ) ;
#24321 = CARTESIAN_POINT ( 'NONE',  ( 22.83552561521075575, 27.23845256177168039, -27.27469245111273111 ) ) ;
#24323 = FACE_OUTER_BOUND ( 'NONE', #21207, .T. ) ;
#24322 = LINE ( 'NONE', #28890, #43732 ) ;
#24324 = STYLED_ITEM ( 'NONE', ( #27632 ), #40275 ) ;
#24325 = CARTESIAN_POINT ( 'NONE',  ( -10.01517768586949231, 137.1949999999999363, -6.132527647946036459E-16 ) ) ;
#24326 = CARTESIAN_POINT ( 'NONE',  ( -109.6449999999999960, 4.716976649647091513, -6.492361379858946790 ) ) ;
#24327 = PLANE ( 'NONE',  #12305 ) ;
#24328 = UNCERTAINTY_MEASURE_WITH_UNIT (LENGTH_MEASURE( 1.000000000000000082E-05 ), #16512, 'distance_accuracy_value', 'NONE');
#24330 = CARTESIAN_POINT ( 'NONE',  ( -6.826472737025120807, 144.9929263765338021, 4.959722759717906548 ) ) ;
#24329 = DIRECTION ( 'NONE',  ( 1.000000000000000000, -0.000000000000000000, -0.000000000000000000 ) ) ;
#24331 = CARTESIAN_POINT ( 'NONE',  ( -145.7929263765337851, -3.094860106618429807, 9.524999999999991473 ) ) ;
#24332 = CARTESIAN_POINT ( 'NONE',  ( -169.0449999999999875, 7.632228543268600340, 2.479861379858949277 ) ) ;
#24333 = CARTESIAN_POINT ( 'NONE',  ( -20.42000000000000881, -1.426810058990923835E-13, 12.50000000000000000 ) ) ;
#24334 = DIRECTION ( 'NONE',  ( -1.000000000000000000, -0.000000000000000000, -0.000000000000000000 ) ) ;
#24335 = ORIENTED_EDGE ( 'NONE', *, *, #59802, .T. ) ;
#24336 = CARTESIAN_POINT ( 'NONE',  ( -11.99999999999999822, -6.499999999999999112, 3.000000000000000000 ) ) ;
#24337 = ORIENTED_EDGE ( 'NONE', *, *, #36806, .T. ) ;
#24338 = EDGE_CURVE ( 'NONE', #54731, #25443, #50832, .T. ) ;
#24339 = CARTESIAN_POINT ( 'NONE',  ( 2.607480562269128388, 119.7929263765338277, -8.024999999999963052 ) ) ;
#24340 = CARTESIAN_POINT ( 'NONE',  ( 44.86933527532148247, 9.999999999999984013, 3.235873323885559039 ) ) ;
#24341 = CARTESIAN_POINT ( 'NONE',  ( -1.908195823574483386E-14, 24.74999999999996803, 3.750000000000000000 ) ) ;
#24342 = AXIS2_PLACEMENT_3D ( 'NONE', #47023, #20233, #20593 ) ;
#24343 = ORIENTED_EDGE ( 'NONE', *, *, #68006, .T. ) ;
#24344 = CARTESIAN_POINT ( 'NONE',  ( -163.4050000000000011, -2.607480562269069768, 8.024999999999991473 ) ) ;
#24345 = CIRCLE ( 'NONE', #693, 26.99999999999999645 ) ;
#24346 = ORIENTED_EDGE ( 'NONE', *, *, #67754, .F. ) ;
#24347 = CARTESIAN_POINT ( 'NONE',  ( 48.50000000000000000, 14.49137674618942562, -7.500000000000000000 ) ) ;
#24348 = VERTEX_POINT ( 'NONE', #59581 ) ;
#24349 = AXIS2_PLACEMENT_3D ( 'NONE', #62273, #14100, #47184 ) ;
#24350 = DIRECTION ( 'NONE',  ( -1.000000000000000000, 0.000000000000000000, 0.000000000000000000 ) ) ;
#24351 = CYLINDRICAL_SURFACE ( 'NONE', #53373, 0.2500000000000002220 ) ;
#24352 = CARTESIAN_POINT ( 'NONE',  ( -5.598654528085806881, 115.7449999999999903, -7.705886871421374629 ) ) ;
#24353 = ORIENTED_EDGE ( 'NONE', *, *, #35845, .F. ) ;
#24354 = DIRECTION ( 'NONE',  ( 1.000000000000000000, 0.000000000000000000, 0.000000000000000000 ) ) ;
#24355 = CARTESIAN_POINT ( 'NONE',  ( 5.598654528085805993, 112.3549999999999898, 7.705886871421374629 ) ) ;
#24356 = CARTESIAN_POINT ( 'NONE',  ( -77.45499999999998408, 7.632228543268599452, -2.479861379858951942 ) ) ;
#24357 = DIRECTION ( 'NONE',  ( 1.000000000000000000, 0.000000000000000000, 0.000000000000000000 ) ) ;
#24358 = ORIENTED_EDGE ( 'NONE', *, *, #69191, .F. ) ;
#24359 = CARTESIAN_POINT ( 'NONE',  ( 8.102448949553181734, 142.5049999999999955, 5.886773742842750679 ) ) ;
#24360 = UNCERTAINTY_MEASURE_WITH_UNIT (LENGTH_MEASURE( 1.000000000000000082E-05 ), #62928, 'distance_accuracy_value', 'NONE');
#24361 = FACE_OUTER_BOUND ( 'NONE', #657, .T. ) ;
#24362 = DIRECTION ( 'NONE',  ( 0.000000000000000000, 1.000000000000000000, 0.000000000000000000 ) ) ;
#24363 = EDGE_CURVE ( 'NONE', #39136, #25552, #32867, .T. ) ;
#24364 =( LENGTH_UNIT ( ) NAMED_UNIT ( * ) SI_UNIT ( .MILLI., .METRE. ) );
#24365 = FACE_OUTER_BOUND ( 'NONE', #43002, .T. ) ;
#24366 = ORIENTED_EDGE ( 'NONE', *, *, #48261, .T. ) ;
#24367 = DIRECTION ( 'NONE',  ( -0.000000000000000000, 1.000000000000000000, -0.000000000000000000 ) ) ;
#24368 = DIRECTION ( 'NONE',  ( 0.000000000000000000, 1.000000000000000000, 0.000000000000000000 ) ) ;
#24369 = CARTESIAN_POINT ( 'NONE',  ( -49.34499999999997044, 7.632228543268599452, -2.479861379858951942 ) ) ;
#24370 = EDGE_LOOP ( 'NONE', ( #62156, #26954, #51802, #38765 ) ) ;
#24371 = DIRECTION ( 'NONE',  ( -1.000000000000000000, 1.387778780781444256E-14, 0.000000000000000000 ) ) ;
#24372 = ADVANCED_FACE ( 'NONE', ( #11747 ), #33216, .T. ) ;
#24373 = CARTESIAN_POINT ( 'NONE',  ( 6.062177826491068622, 2.500000000000000000, -3.500000000000001332 ) ) ;
#24374 = DIRECTION ( 'NONE',  ( 0.000000000000000000, 0.000000000000000000, 1.000000000000000000 ) ) ;
#24375 = FILL_AREA_STYLE ('',( #13130 ) ) ;
#24376 = VERTEX_POINT ( 'NONE', #39557 ) ;
#24377 = CARTESIAN_POINT ( 'NONE',  ( -58.34499999999997755, 7.632228543268599452, -2.479861379858951942 ) ) ;
#24378 = DIRECTION ( 'NONE',  ( 0.000000000000000000, 0.000000000000000000, -1.000000000000000000 ) ) ;
#24379 = ORIENTED_EDGE ( 'NONE', *, *, #39843, .F. ) ;
#24380 = CARTESIAN_POINT ( 'NONE',  ( -108.8049999999999784, -8.437984349512085203, 5.166775262442717831E-16 ) ) ;
#24381 = ORIENTED_EDGE ( 'NONE', *, *, #61606, .T. ) ;
#24382 = CARTESIAN_POINT ( 'NONE',  ( 45.00000000000000000, 99.99999999999992895, 10.00000000000000000 ) ) ;
#24383 = ADVANCED_FACE ( 'NONE', ( #44841 ), #45865, .T. ) ;
#24384 = CARTESIAN_POINT ( 'NONE',  ( -74.99999999999998579, 50.00000000000000000, 12.00000000000000000 ) ) ;
#24385 = CARTESIAN_POINT ( 'NONE',  ( -138.6570736234661751, 9.058813317711329915, 2.943386871421369566 ) ) ;
#24386 = FACE_BOUND ( 'NONE', #39316, .T. ) ;
#24387 = CARTESIAN_POINT ( 'NONE',  ( 10.01517768586949408, 141.6949999999999648, 1.839758294383810543E-15 ) ) ;
#24388 = CARTESIAN_POINT ( 'NONE',  ( -84.95707362346617231, 9.058813317711329915, -2.943386871421373119 ) ) ;
#24389 = EDGE_CURVE ( 'NONE', #21071, #52175, #23687, .T. ) ;
#24390 = SURFACE_STYLE_USAGE ( .BOTH. , #30021 ) ;
#24391 = PRODUCT_DEFINITION_SHAPE ( 'NONE', 'NONE',  #69698 ) ;
#24392 = CARTESIAN_POINT ( 'NONE',  ( 24.00000000000000355, 36.75000000000000000, 3.000000000000000000 ) ) ;
#24393 =( LENGTH_UNIT ( ) NAMED_UNIT ( * ) SI_UNIT ( .MILLI., .METRE. ) );
#24395 = DIRECTION ( 'NONE',  ( 0.000000000000000000, 1.000000000000000000, 0.000000000000000000 ) ) ;
#24394 =( NAMED_UNIT ( * ) PLANE_ANGLE_UNIT ( ) SI_UNIT ( $, .RADIAN. ) );
#24396 = MECHANICAL_DESIGN_GEOMETRIC_PRESENTATION_REPRESENTATION (  '', ( #69317 ), #8650 ) ;
#24397 = CARTESIAN_POINT ( 'NONE',  ( -119.9049999999999869, 2.607480562269068880, -8.024999999999993250 ) ) ;
#24398 = COLOUR_RGB ( '', 0.09019608, 0.27058824, 0.51372549) ;
#24399 = CARTESIAN_POINT ( 'NONE',  ( -157.9429263765338192, 0.000000000000000000, 9.524999999999991473 ) ) ;
#24400 = CARTESIAN_POINT ( 'NONE',  ( -9.058813317711338797, 113.3449999999999847, 2.943386871421373563 ) ) ;
#24401 = CARTESIAN_POINT ( 'NONE',  ( -136.3449999999999989, 7.632228543268599452, -2.479861379858951942 ) ) ;
#24402 = CARTESIAN_POINT ( 'NONE',  ( -118.4949999999999903, 6.826472737025113702, -4.959722759717902107 ) ) ;
#24403 = CARTESIAN_POINT ( 'NONE',  ( 69.99999999999998579, 36.75000000000000000, -3.000000000000000000 ) ) ;
#24404 = ORIENTED_EDGE ( 'NONE', *, *, #47948, .F. ) ;
#24405 = CARTESIAN_POINT ( 'NONE',  ( -19.00000000000000000, 8.000000000000000000, 3.500000000000003997 ) ) ;
#24406 = DIRECTION ( 'NONE',  ( -0.000000000000000000, -1.000000000000000000, -0.000000000000000000 ) ) ;
#24407 = CARTESIAN_POINT ( 'NONE',  ( -170.6929263765337623, 10.01517768586948698, -1.839758294383808571E-15 ) ) ;
#24408 = CARTESIAN_POINT ( 'NONE',  ( -47.69499999999999318, -8.437984349512085203, 5.166775262442717831E-16 ) ) ;
#24409 = CIRCLE ( 'NONE', #31171, 16.00000000000000000 ) ;
#24410 = PRESENTATION_LAYER_ASSIGNMENT (  '', '', ( #6437 ) ) ;
#24411 = CARTESIAN_POINT ( 'NONE',  ( -6.826472737025120807, 124.5070736234661553, -4.959722759717907437 ) ) ;
#24412 = DIRECTION ( 'NONE',  ( -0.000000000000000000, 1.000000000000000000, -0.000000000000000000 ) ) ;
#24413 = DIRECTION ( 'NONE',  ( 0.000000000000000000, 0.000000000000000000, 1.000000000000000000 ) ) ;
#24414 = EDGE_LOOP ( 'NONE', ( #21233, #16688, #35220, #42334 ) ) ;
#24415 = CARTESIAN_POINT ( 'NONE',  ( -88.04292637653379927, -9.058813317711329915, -2.943386871421370898 ) ) ;
#24416 = DIRECTION ( 'NONE',  ( 0.000000000000000000, 1.000000000000000000, 0.000000000000000000 ) ) ;
#24417 = CARTESIAN_POINT ( 'NONE',  ( 3.999798566743339556, 49.09558629977726696, 2.000000000000000000 ) ) ;
#24418 = EDGE_CURVE ( 'NONE', #16904, #22316, #40717, .T. ) ;
#24419 = DIRECTION ( 'NONE',  ( 0.000000000000000000, 0.000000000000000000, -1.000000000000000000 ) ) ;
#24420 = CARTESIAN_POINT ( 'NONE',  ( -23.21231517720797655, 117.4999999999999716, 9.500000000000000000 ) ) ;
#24421 = CARTESIAN_POINT ( 'NONE',  ( -41.00000000735875716, 108.0041655766031568, 3.104053578549263115 ) ) ;
#24422 = SURFACE_SIDE_STYLE ('',( #2590 ) ) ;
#24423 = VERTEX_POINT ( 'NONE', #29300 ) ;
#24424 = CARTESIAN_POINT ( 'NONE',  ( -18.00000000000000711, 33.74999999999999289, -3.750000000000000000 ) ) ;
#24425 = EDGE_LOOP ( 'NONE', ( #54467, #42370, #13719, #43401 ) ) ;
#24426 = CARTESIAN_POINT ( 'NONE',  ( 27.00000000000001776, 42.00000000000000000, -35.50000000000000000 ) ) ;
#24427 = CARTESIAN_POINT ( 'NONE',  ( 6.826472737025119919, 129.0070736234661695, 4.959722759717908325 ) ) ;
#24428 = VERTEX_POINT ( 'NONE', #33884 ) ;
#24429 = AXIS2_PLACEMENT_3D ( 'NONE', #31679, #26049, #53157 ) ;
#24430 = DIRECTION ( 'NONE',  ( 0.000000000000000000, 0.000000000000000000, -1.000000000000000000 ) ) ;
#24431 = CYLINDRICAL_SURFACE ( 'NONE', #66566, 13.99999999999999822 ) ;
#24432 = PRESENTATION_LAYER_ASSIGNMENT (  '', '', ( #51426 ) ) ;
#24433 = ORIENTED_EDGE ( 'NONE', *, *, #47966, .T. ) ;
#24434 =( NAMED_UNIT ( * ) PLANE_ANGLE_UNIT ( ) SI_UNIT ( $, .RADIAN. ) );
#24435 = EDGE_CURVE ( 'NONE', #58978, #9509, #13469, .T. ) ;
#24436 = FACE_OUTER_BOUND ( 'NONE', #28327, .T. ) ;
#24437 = EDGE_CURVE ( 'NONE', #21392, #30006, #66609, .T. ) ;
#24438 = DIRECTION ( 'NONE',  ( 0.000000000000000000, 0.000000000000000000, -1.000000000000000000 ) ) ;
#24439 = PRESENTATION_STYLE_ASSIGNMENT (( #40665 ) ) ;
#24440 = AXIS2_PLACEMENT_3D ( 'NONE', #35430, #8688, #3350 ) ;
#24441 = CARTESIAN_POINT ( 'NONE',  ( -82.04499999999998749, 7.632228543268600340, 2.479861379858949277 ) ) ;
#24442 = VERTEX_POINT ( 'NONE', #13127 ) ;
#24443 = FACE_OUTER_BOUND ( 'NONE', #48551, .T. ) ;
#24444 = SURFACE_SIDE_STYLE ('',( #2618 ) ) ;
#24445 = ADVANCED_FACE ( 'NONE', ( #67299, #56033 ), #50100, .F. ) ;
#24446 = ORIENTED_EDGE ( 'NONE', *, *, #57493, .T. ) ;
#24447 = DIRECTION ( 'NONE',  ( 0.000000000000000000, 0.000000000000000000, -1.000000000000000000 ) ) ;
#24448 = LINE ( 'NONE', #35386, #7800 ) ;
#24449 = CIRCLE ( 'NONE', #23314, 3.000000000000000444 ) ;
#24450 = EDGE_CURVE ( 'NONE', #46237, #46026, #18746, .T. ) ;
#24451 = COLOUR_RGB ( '', 0.08235294, 0.09019608, 0.10196078) ;
#24452 = DIRECTION ( 'NONE',  ( 0.000000000000000000, 1.000000000000000000, 0.000000000000000000 ) ) ;
#24453 = ORIENTED_EDGE ( 'NONE', *, *, #11903, .F. ) ;
#24454 = SURFACE_SIDE_STYLE ('',( #41038 ) ) ;
#24455 = ORIENTED_EDGE ( 'NONE', *, *, #3191, .F. ) ;
#24456 = EDGE_CURVE ( 'NONE', #13502, #35776, #37378, .T. ) ;
#24457 = DIRECTION ( 'NONE',  ( 1.000000000000000000, 0.000000000000000000, 0.000000000000000000 ) ) ;
#24458 = CARTESIAN_POINT ( 'NONE',  ( -170.4570736234661865, -9.058813317711329915, 2.943386871421371787 ) ) ;
#24459 = CARTESIAN_POINT ( 'NONE',  ( 0.000000000000000000, 21.74999999999998579, 4.000000000000000000 ) ) ;
#24460 = CARTESIAN_POINT ( 'NONE',  ( 3.094860106618435136, 115.2949999999999733, -9.525000000000000355 ) ) ;
#24461 = CARTESIAN_POINT ( 'NONE',  ( -113.9070736234661751, -3.094860106618429807, 9.524999999999991473 ) ) ;
#24462 = CARTESIAN_POINT ( 'NONE',  ( -0.1770589935948753968, 2.499999999999996891, 7.000000000000000000 ) ) ;
#24463 = EDGE_CURVE ( 'NONE', #1828, #1406, #2529, .T. ) ;
#24464 = CYLINDRICAL_SURFACE ( 'NONE', #11114, 0.2500000000000002220 ) ;
#24465 = ORIENTED_EDGE ( 'NONE', *, *, #35751, .T. ) ;
#24466 = CARTESIAN_POINT ( 'NONE',  ( 71.18918918918917882, 14.09971791521133433, -9.500000000000000000 ) ) ;
#24467 =( NAMED_UNIT ( * ) PLANE_ANGLE_UNIT ( ) SI_UNIT ( $, .RADIAN. ) );
#24469 = DIRECTION ( 'NONE',  ( 0.000000000000000000, 0.000000000000000000, -1.000000000000000000 ) ) ;
#24468 = DIRECTION ( 'NONE',  ( 0.000000000000000000, 0.000000000000000000, 1.000000000000000000 ) ) ;
#24470 = DIRECTION ( 'NONE',  ( 0.000000000000000000, 0.000000000000000000, -1.000000000000000000 ) ) ;
#24471 = CARTESIAN_POINT ( 'NONE',  ( -145.5549999999999784, 0.000000000000000000, 8.024999999999991473 ) ) ;
#24472 =( LENGTH_UNIT ( ) NAMED_UNIT ( * ) SI_UNIT ( .MILLI., .METRE. ) );
#24473 = CARTESIAN_POINT ( 'NONE',  ( 23.50000000000001776, 15.00000000000000000, 29.68999999999999417 ) ) ;
#24474 = CARTESIAN_POINT ( 'NONE',  ( -168.4449999999999932, 0.000000000000000000, 8.024999999999991473 ) ) ;
#24475 = CARTESIAN_POINT ( 'NONE',  ( -144.4449999999999932, 0.000000000000000000, 8.024999999999991473 ) ) ;
#24476 = VERTEX_POINT ( 'NONE', #18759 ) ;
#24477 = DIRECTION ( 'NONE',  ( 1.000000000000000000, 0.000000000000000000, 0.000000000000000000 ) ) ;
#24478 = CARTESIAN_POINT ( 'NONE',  ( -68.15499999999997272, 7.632228543268600340, 2.479861379858949277 ) ) ;
#24479 =( NAMED_UNIT ( * ) PLANE_ANGLE_UNIT ( ) SI_UNIT ( $, .RADIAN. ) );
#24480 =( GEOMETRIC_REPRESENTATION_CONTEXT ( 3 ) GLOBAL_UNCERTAINTY_ASSIGNED_CONTEXT ( ( #63700 ) ) GLOBAL_UNIT_ASSIGNED_CONTEXT ( ( #58831, #42697, #53555 ) ) REPRESENTATION_CONTEXT ( 'NONE', 'WORKASPACE' ) );
#24481 =( GEOMETRIC_REPRESENTATION_CONTEXT ( 3 ) GLOBAL_UNCERTAINTY_ASSIGNED_CONTEXT ( ( #39681 ) ) GLOBAL_UNIT_ASSIGNED_CONTEXT ( ( #28709, #27659, #6231 ) ) REPRESENTATION_CONTEXT ( 'NONE', 'WORKASPACE' ) );
#24482 = CARTESIAN_POINT ( 'NONE',  ( -63.14499999999998181, -4.716976649647092401, 6.492361379858946790 ) ) ;
#24483 = CARTESIAN_POINT ( 'NONE',  ( -3.094860106618434248, 150.9050000000000011, 9.525000000000000355 ) ) ;
#24484 = DIRECTION ( 'NONE',  ( 0.000000000000000000, -0.000000000000000000, 1.000000000000000000 ) ) ;
#24485 = VECTOR ( 'NONE', #7899, 1000.000000000000000 ) ;
#24486 = MECHANICAL_DESIGN_GEOMETRIC_PRESENTATION_REPRESENTATION (  '', ( #39164 ), #67124 ) ;
#24487 = CARTESIAN_POINT ( 'NONE',  ( 45.50000000000000000, -1.469576158976824618E-14, -6.500000000000000000 ) ) ;
#24488 = CARTESIAN_POINT ( 'NONE',  ( 0.000000000000000000, 0.000000000000000000, 0.000000000000000000 ) ) ;
#24489 = SURFACE_SIDE_STYLE ('',( #34708 ) ) ;
#24490 = CARTESIAN_POINT ( 'NONE',  ( 1.804495846578303864, 51.08602766979955589, 2.000000000000000000 ) ) ;
#24491 = VECTOR ( 'NONE', #45821, 1000.000000000000000 ) ;
#24492 = DIRECTION ( 'NONE',  ( 0.000000000000000000, 1.000000000000000000, 0.000000000000000000 ) ) ;
#24493 = SURFACE_STYLE_USAGE ( .BOTH. , #3007 ) ;
#24494 = FACE_OUTER_BOUND ( 'NONE', #59697, .T. ) ;
#24495 = ORIENTED_EDGE ( 'NONE', *, *, #3610, .T. ) ;
#24496 = EDGE_LOOP ( 'NONE', ( #39858, #56533, #28485, #42490 ) ) ;
#24497 = CARTESIAN_POINT ( 'NONE',  ( -61.10707362346615668, 8.102448949553172852, -5.886773742842744461 ) ) ;
#24498 = DIRECTION ( 'NONE',  ( 1.000000000000000000, -0.000000000000000000, 0.000000000000000000 ) ) ;
#24499 = EDGE_CURVE ( 'NONE', #43827, #3256, #40237, .T. ) ;
#24500 =( GEOMETRIC_REPRESENTATION_CONTEXT ( 3 ) GLOBAL_UNCERTAINTY_ASSIGNED_CONTEXT ( ( #5244 ) ) GLOBAL_UNIT_ASSIGNED_CONTEXT ( ( #56322, #29947, #30269 ) ) REPRESENTATION_CONTEXT ( 'NONE', 'WORKASPACE' ) );
#24501 = CARTESIAN_POINT ( 'NONE',  ( -45.00000000000000711, 9.298035018096991067, 6.651463925736444516 ) ) ;
#24503 = EDGE_CURVE ( 'NONE', #60196, #58400, #27191, .T. ) ;
#24502 = FILL_AREA_STYLE ('',( #1958 ) ) ;
#24504 = ORIENTED_EDGE ( 'NONE', *, *, #41265, .F. ) ;
#24506 = EDGE_LOOP ( 'NONE', ( #68188, #48471, #67255, #51906 ) ) ;
#24505 = AXIS2_PLACEMENT_3D ( 'NONE', #22238, #43734, #16982 ) ;
#24507 = SURFACE_STYLE_USAGE ( .BOTH. , #30131 ) ;
#24508 = SURFACE_SIDE_STYLE ('',( #19235 ) ) ;
#24509 = EDGE_CURVE ( 'NONE', #26721, #29573, #63186, .T. ) ;
#24510 = ORIENTED_EDGE ( 'NONE', *, *, #34379, .T. ) ;
#24511 = CARTESIAN_POINT ( 'NONE',  ( -8.102448949553181734, 111.6049999999999613, 5.886773742842747126 ) ) ;
#24512 = CARTESIAN_POINT ( 'NONE',  ( -145.3429263765338249, -9.058813317711329915, 2.943386871421371787 ) ) ;
#24513 = ORIENTED_EDGE ( 'NONE', *, *, #14530, .T. ) ;
#24514 = STYLED_ITEM ( 'NONE', ( #63719 ), #9738 ) ;
#24515 = FILL_AREA_STYLE ('',( #19240 ) ) ;
#24516 = CARTESIAN_POINT ( 'NONE',  ( -114.1449999999999960, -4.716976649647092401, 6.492361379858946790 ) ) ;
#24517 = ORIENTED_EDGE ( 'NONE', *, *, #45528, .T. ) ;
#24518 = AXIS2_PLACEMENT_3D ( 'NONE', #57973, #26280, #41123 ) ;
#24519 =( LENGTH_UNIT ( ) NAMED_UNIT ( * ) SI_UNIT ( .MILLI., .METRE. ) );
#24520 =( NAMED_UNIT ( * ) SI_UNIT ( $, .STERADIAN. ) SOLID_ANGLE_UNIT ( ) );
#24521 = CARTESIAN_POINT ( 'NONE',  ( -11.94707626989746529, -11.32487227758645432, -3.972914747560817972 ) ) ;
#24522 = ORIENTED_EDGE ( 'NONE', *, *, #50987, .F. ) ;
#24523 = CARTESIAN_POINT ( 'NONE',  ( 7.632228543268607446, 146.0429263765338135, 2.479861379858954606 ) ) ;
#24524 = CARTESIAN_POINT ( 'NONE',  ( -53.42555371347750537, -9.981032396169707610, -3.023059613375645327 ) ) ;
#24525 = AXIS2_PLACEMENT_3D ( 'NONE', #42467, #10427, #31856 ) ;
#24526 = EDGE_CURVE ( 'NONE', #68025, #6587, #68347, .T. ) ;
#24527 = DIRECTION ( 'NONE',  ( 1.000000000000000000, -0.000000000000000000, -1.300977106640434891E-16 ) ) ;
#24528 = SURFACE_STYLE_FILL_AREA ( #57609 ) ;
#24529 = ORIENTED_EDGE ( 'NONE', *, *, #13427, .T. ) ;
#24530 = DIRECTION ( 'NONE',  ( -0.000000000000000000, 1.000000000000000000, -0.000000000000000000 ) ) ;
#24531 = ORIENTED_EDGE ( 'NONE', *, *, #39346, .T. ) ;
#24532 = DIRECTION ( 'NONE',  ( 0.000000000000000000, 0.000000000000000000, 1.000000000000000000 ) ) ;
#24533 = FACE_OUTER_BOUND ( 'NONE', #51903, .T. ) ;
#24534 = FACE_OUTER_BOUND ( 'NONE', #58222, .T. ) ;
#24535 = CARTESIAN_POINT ( 'NONE',  ( -195.0000000000000000, 0.000000000000000000, 0.000000000000000000 ) ) ;
#24536 = CARTESIAN_POINT ( 'NONE',  ( -124.8549999999999898, 4.716976649647094177, 6.492361379858945902 ) ) ;
#24537 = CARTESIAN_POINT ( 'NONE',  ( -184.0000000000000000, -4.077197870136868296, 6.923068838537520975 ) ) ;
#24538 =( NAMED_UNIT ( * ) SI_UNIT ( $, .STERADIAN. ) SOLID_ANGLE_UNIT ( ) );
#24539 = ORIENTED_EDGE ( 'NONE', *, *, #32461, .F. ) ;
#24540 = DIRECTION ( 'NONE',  ( -5.782411586589351722E-16, 1.000000000000000000, 0.000000000000000000 ) ) ;
#24541 = DIRECTION ( 'NONE',  ( -1.000000000000000000, -0.000000000000000000, -0.000000000000000000 ) ) ;
#24542 = CARTESIAN_POINT ( 'NONE',  ( -7.342319042881619851, 5.282730372348555470, 1.478919525906007998E-15 ) ) ;
#24543 = VERTEX_POINT ( 'NONE', #4655 ) ;
#24544 = CIRCLE ( 'NONE', #39169, 11.99999999999999645 ) ;
#24545 = ORIENTED_EDGE ( 'NONE', *, *, #53832, .F. ) ;
#24546 = LINE ( 'NONE', #46061, #174 ) ;
#24547 = CARTESIAN_POINT ( 'NONE',  ( 45.59262096826685706, 9.979230606950402205, 6.500000000000000000 ) ) ;
#24548 = DIRECTION ( 'NONE',  ( 0.000000000000000000, 0.000000000000000000, -1.000000000000000000 ) ) ;
#24549 = CARTESIAN_POINT ( 'NONE',  ( -2.448909842207114274, 50.66868219381804295, 7.156559940361793437 ) ) ;
#24550 = ORIENTED_EDGE ( 'NONE', *, *, #16824, .T. ) ;
#24551 = CARTESIAN_POINT ( 'NONE',  ( -180.6550000000000011, -7.632228543268600340, -2.479861379858950166 ) ) ;
#24552 = CARTESIAN_POINT ( 'NONE',  ( -87.50000000000000000, -7.499999999999990230, 1.000000000000000000 ) ) ;
#24553 = EDGE_CURVE ( 'NONE', #408, #4398, #35647, .T. ) ;
#24554 = CARTESIAN_POINT ( 'NONE',  ( -45.48309787872866394, 9.683080749504643592, -6.499999999999997335 ) ) ;
#24555 = CARTESIAN_POINT ( 'NONE',  ( -51.50707362346617657, 8.102448949553176405, 5.886773742842740909 ) ) ;
#24556 = CARTESIAN_POINT ( 'NONE',  ( -172.9449999999999932, -9.827790563157499189E-16, -8.024999999999991473 ) ) ;
#24557 = EDGE_CURVE ( 'NONE', #19551, #49493, #46591, .T. ) ;
#24558 = DIRECTION ( 'NONE',  ( -1.000000000000000000, 0.000000000000000000, 0.000000000000000000 ) ) ;
#24559 = ORIENTED_EDGE ( 'NONE', *, *, #6662, .T. ) ;
#24560 = DIRECTION ( 'NONE',  ( -1.000000000000000000, 9.376883653928660246E-17, 0.000000000000000000 ) ) ;
#24562 = CARTESIAN_POINT ( 'NONE',  ( -24.21231517720798365, 50.00000000000000000, 7.000000000000000000 ) ) ;
#24561 =( GEOMETRIC_REPRESENTATION_CONTEXT ( 3 ) GLOBAL_UNCERTAINTY_ASSIGNED_CONTEXT ( ( #19907 ) ) GLOBAL_UNIT_ASSIGNED_CONTEXT ( ( #5522, #58325, #43246 ) ) REPRESENTATION_CONTEXT ( 'NONE', 'WORKASPACE' ) );
#24563 = DIRECTION ( 'NONE',  ( -0.000000000000000000, -1.000000000000000000, 0.000000000000000000 ) ) ;
#24564 = CARTESIAN_POINT ( 'NONE',  ( -94.10499999999997556, -6.826472737025115478, 4.959722759717900331 ) ) ;
#24565 = DIRECTION ( 'NONE',  ( 0.000000000000000000, 0.000000000000000000, 1.000000000000000000 ) ) ;
#24566 = SURFACE_STYLE_FILL_AREA ( #3075 ) ;
#24567 = AXIS2_PLACEMENT_3D ( 'NONE', #30791, #9012, #57179 ) ;
#24568 = CARTESIAN_POINT ( 'NONE',  ( -90.29499999999997328, -2.607480562269069768, 8.024999999999991473 ) ) ;
#24569 = CARTESIAN_POINT ( 'NONE',  ( 8.102448949553181734, 121.5049999999999670, 5.886773742842750679 ) ) ;
#24570 = CARTESIAN_POINT ( 'NONE',  ( -72.59499999999998465, 2.607480562269073321, 8.024999999999991473 ) ) ;
#24571 =( NAMED_UNIT ( * ) PLANE_ANGLE_UNIT ( ) SI_UNIT ( $, .RADIAN. ) );
#24572 = TOROIDAL_SURFACE ( 'NONE', #38095, 1.499999999999998668, 1.000000000000000000 ) ;
#24573 = CIRCLE ( 'NONE', #63891, 0.5000000000000004441 ) ;
#24574 = FACE_OUTER_BOUND ( 'NONE', #48944, .T. ) ;
#24575 = MECHANICAL_DESIGN_GEOMETRIC_PRESENTATION_REPRESENTATION (  '', ( #37002 ), #30196 ) ;
#24576 = CARTESIAN_POINT ( 'NONE',  ( -71.50000000000000000, 14.49137674618942206, -7.000000000000000000 ) ) ;
#24577 = ORIENTED_EDGE ( 'NONE', *, *, #2888, .T. ) ;
#24578 = CARTESIAN_POINT ( 'NONE',  ( -113.5429263765338135, 9.058813317711329915, 2.943386871421369566 ) ) ;
#24579 = CARTESIAN_POINT ( 'NONE',  ( -130.1950000000000216, 8.437984349512085203, -1.550032578732815448E-15 ) ) ;
#24580 = DIRECTION ( 'NONE',  ( -1.000000000000000000, 0.000000000000000000, 0.000000000000000000 ) ) ;
#24581 =( GEOMETRIC_REPRESENTATION_CONTEXT ( 3 ) GLOBAL_UNCERTAINTY_ASSIGNED_CONTEXT ( ( #51775 ) ) GLOBAL_UNIT_ASSIGNED_CONTEXT ( ( #65605, #23380, #39253 ) ) REPRESENTATION_CONTEXT ( 'NONE', 'WORKASPACE' ) );
#24582 = STYLED_ITEM ( 'NONE', ( #38820 ), #66751 ) ;
#24583 = CARTESIAN_POINT ( 'NONE',  ( 179.4361977533490347, 5.000000000000000000, -103.7004518695263044 ) ) ;
#24584 = EDGE_CURVE ( 'NONE', #55142, #38982, #43996, .T. ) ;
#24586 = LINE ( 'NONE', #63286, #55064 ) ;
#24585 = DIRECTION ( 'NONE',  ( 0.000000000000000000, 0.000000000000000000, -1.000000000000000000 ) ) ;
#24587 = VERTEX_POINT ( 'NONE', #30002 ) ;
#24588 = ORIENTED_EDGE ( 'NONE', *, *, #13167, .T. ) ;
#24589 = CARTESIAN_POINT ( 'NONE',  ( 0.000000000000000000, 2.500000000000000000, 0.000000000000000000 ) ) ;
#24590 =( GEOMETRIC_REPRESENTATION_CONTEXT ( 3 ) GLOBAL_UNCERTAINTY_ASSIGNED_CONTEXT ( ( #9362 ) ) GLOBAL_UNIT_ASSIGNED_CONTEXT ( ( #24393, #60987, #33573 ) ) REPRESENTATION_CONTEXT ( 'NONE', 'WORKASPACE' ) );
#24591 = DIRECTION ( 'NONE',  ( -1.000000000000000000, 0.000000000000000000, 0.000000000000000000 ) ) ;
#24592 = CARTESIAN_POINT ( 'NONE',  ( -20.71231517720798010, 149.9999999999999716, -10.00000000000000000 ) ) ;
#24593 = FACE_OUTER_BOUND ( 'NONE', #43366, .T. ) ;
#24594 = VERTEX_POINT ( 'NONE', #52875 ) ;
#24595 = CARTESIAN_POINT ( 'NONE',  ( -128.6049999999999898, 6.826472737025113702, -4.959722759717902107 ) ) ;
#24596 = ORIENTED_EDGE ( 'NONE', *, *, #64734, .T. ) ;
#24597 = FACE_OUTER_BOUND ( 'NONE', #47524, .T. ) ;
#24598 = CARTESIAN_POINT ( 'NONE',  ( -119.6070736234661638, -8.102448949553172852, 5.886773742842742685 ) ) ;
#24599 = EDGE_CURVE ( 'NONE', #5542, #35967, #27958, .T. ) ;
#24600 = ORIENTED_EDGE ( 'NONE', *, *, #56238, .F. ) ;
#24601 = CARTESIAN_POINT ( 'NONE',  ( -172.1929263765337907, -10.01517768586948698, 6.132527647946031529E-16 ) ) ;
#24602 = LINE ( 'NONE', #68244, #53462 ) ;
#24603 = ORIENTED_EDGE ( 'NONE', *, *, #4149, .F. ) ;
#24604 = CARTESIAN_POINT ( 'NONE',  ( 17.15973193263811680, -3.000000000000000000, 2.000000000000000000 ) ) ;
#24605 = CARTESIAN_POINT ( 'NONE',  ( -3.094860106618432471, 142.5950000000000273, -9.525000000000000355 ) ) ;
#24606 = ORIENTED_EDGE ( 'NONE', *, *, #43877, .T. ) ;
#24607 = CARTESIAN_POINT ( 'NONE',  ( -54.50707362346614104, 8.102448949553176405, 5.886773742842740909 ) ) ;
#24608 = CARTESIAN_POINT ( 'NONE',  ( -3.094860106618434248, 135.9050000000000011, 9.525000000000000355 ) ) ;
#24609 = CARTESIAN_POINT ( 'NONE',  ( 24.21231517720798010, 112.9999999999999858, -9.500000000000000000 ) ) ;
#24610 = COLOUR_RGB ( '', 0.08235294, 0.09019608, 0.10196078) ;
#24611 = SURFACE_STYLE_FILL_AREA ( #30944 ) ;
#24612 = ORIENTED_EDGE ( 'NONE', *, *, #60125, .F. ) ;
#24613 = CARTESIAN_POINT ( 'NONE',  ( 2.607480562269071989, 118.5929263765338106, 8.025000000000002132 ) ) ;
#24614 = DIRECTION ( 'NONE',  ( -0.000000000000000000, -0.000000000000000000, -1.000000000000000000 ) ) ;
#24615 = EDGE_CURVE ( 'NONE', #65906, #62684, #54229, .T. ) ;
#24616 = FACE_OUTER_BOUND ( 'NONE', #635, .T. ) ;
#24617 = SURFACE_SIDE_STYLE ('',( #15172 ) ) ;
#24618 = ORIENTED_EDGE ( 'NONE', *, *, #27307, .T. ) ;
#24619 = CIRCLE ( 'NONE', #46005, 1.000000000000000888 ) ;
#24620 = CARTESIAN_POINT ( 'NONE',  ( -22.75000000000000711, 37.00000000000000000, -3.750000000000000000 ) ) ;
#24621 = VERTEX_POINT ( 'NONE', #1035 ) ;
#24622 = DIRECTION ( 'NONE',  ( 1.000000000000000000, 0.000000000000000000, 0.000000000000000000 ) ) ;
#24623 = CIRCLE ( 'NONE', #35902, 6.999999999999997335 ) ;
#24624 = FACE_BOUND ( 'NONE', #11211, .T. ) ;
#24625 = FACE_OUTER_BOUND ( 'NONE', #496, .T. ) ;
#24626 = CARTESIAN_POINT ( 'NONE',  ( -163.1050000000000182, -6.826472737025115478, 4.959722759717900331 ) ) ;
#24627 = VERTEX_POINT ( 'NONE', #16302 ) ;
#24628 = VECTOR ( 'NONE', #40207, 1000.000000000000000 ) ;
#24629 = CARTESIAN_POINT ( 'NONE',  ( 71.50000000000000000, 35.92875272052971525, -7.500000000000000000 ) ) ;
#24630 = VECTOR ( 'NONE', #12065, 1000.000000000000227 ) ;
#24631 = CARTESIAN_POINT ( 'NONE',  ( 9.827790563157511022E-16, 111.9999999999999858, 8.025000000000000355 ) ) ;
#24632 = CARTESIAN_POINT ( 'NONE',  ( 74.65399860055322279, 19.87094859200032815, 6.130873952096200341 ) ) ;
#24633 = CARTESIAN_POINT ( 'NONE',  ( -71.75000000000000000, 4.336808689942018722E-16, 24.00000000000000000 ) ) ;
#24634 = EDGE_LOOP ( 'NONE', ( #40322, #16597, #53608, #36298, #35457, #26129, #1209 ) ) ;
#24635 = COLOUR_RGB ( '', 0.08235294, 0.09019608, 0.10196078) ;
#24636 = ORIENTED_EDGE ( 'NONE', *, *, #58361, .T. ) ;
#24637 = DIRECTION ( 'NONE',  ( 1.000000000000000000, -0.000000000000000000, 0.000000000000000000 ) ) ;
#24638 = DIRECTION ( 'NONE',  ( 0.000000000000000000, -1.000000000000000000, 0.000000000000000000 ) ) ;
#24639 = CARTESIAN_POINT ( 'NONE',  ( -76.55499999999997840, 0.000000000000000000, 8.024999999999991473 ) ) ;
#24640 = ORIENTED_EDGE ( 'NONE', *, *, #10096, .T. ) ;
#24641 = DIRECTION ( 'NONE',  ( -0.000000000000000000, -0.000000000000000000, 1.000000000000000000 ) ) ;
#24642 = AXIS2_PLACEMENT_3D ( 'NONE', #27837, #44456, #6407 ) ;
#24643 = CARTESIAN_POINT ( 'NONE',  ( -124.9429263765338192, 0.000000000000000000, 9.524999999999991473 ) ) ;
#24644 = DIRECTION ( 'NONE',  ( -0.000000000000000000, -0.000000000000000000, 1.000000000000000000 ) ) ;
#24645 = VECTOR ( 'NONE', #15979, 1000.000000000000000 ) ;
#24646 = CARTESIAN_POINT ( 'NONE',  ( -75.00000000000000000, 9.484039020261590736, -6.483595844450460888 ) ) ;
#24647 = CARTESIAN_POINT ( 'NONE',  ( 31.00000000000002132, 42.00000000000000000, 75.00000000000000000 ) ) ;
#24648 = ORIENTED_EDGE ( 'NONE', *, *, #58546, .F. ) ;
#24649 = CARTESIAN_POINT ( 'NONE',  ( 9.000000000000003553, 27.74999999999998934, -3.750000000000000000 ) ) ;
#24650 = COLOUR_RGB ( '', 0.08235294, 0.09019608, 0.10196078) ;
#24651 = DIRECTION ( 'NONE',  ( -0.000000000000000000, -0.000000000000000000, -1.000000000000000000 ) ) ;
#24652 = CARTESIAN_POINT ( 'NONE',  ( -9.058813317711338797, 140.3449999999999989, 2.943386871421373563 ) ) ;
#24653 = CARTESIAN_POINT ( 'NONE',  ( -94.79499999999997328, 2.607480562269068880, -8.024999999999993250 ) ) ;
#24654 = FILL_AREA_STYLE_COLOUR ( '', #19515 ) ;
#24655 = CIRCLE ( 'NONE', #26847, 0.5000000000000004441 ) ;
#24656 = PRESENTATION_LAYER_ASSIGNMENT (  '', '', ( #39323 ) ) ;
#24658 = DIRECTION ( 'NONE',  ( 1.000000000000000000, 0.000000000000000000, 0.000000000000000000 ) ) ;
#24657 = CARTESIAN_POINT ( 'NONE',  ( -96.50707362346616947, 8.102448949553176405, 5.886773742842740909 ) ) ;
#24659 = VECTOR ( 'NONE', #16921, 1000.000000000000114 ) ;
#24660 = CARTESIAN_POINT ( 'NONE',  ( -146.0929263765337964, 3.094860106618433360, 9.524999999999991473 ) ) ;
#24661 = SURFACE_STYLE_USAGE ( .BOTH. , #3171 ) ;
#24662 = CARTESIAN_POINT ( 'NONE',  ( -155.8449999999999704, -7.632228543268599452, 2.479861379858951054 ) ) ;
#24663 = PRESENTATION_LAYER_ASSIGNMENT (  '', '', ( #31401 ) ) ;
#24664 = DIRECTION ( 'NONE',  ( -0.000000000000000000, 1.000000000000000000, -0.000000000000000000 ) ) ;
#24665 = EDGE_CURVE ( 'NONE', #12387, #47261, #3938, .T. ) ;
#24666 = AXIS2_PLACEMENT_3D ( 'NONE', #24744, #9659, #31070 ) ;
#24667 = VECTOR ( 'NONE', #16598, 1000.000000000000000 ) ;
#24668 = EDGE_LOOP ( 'NONE', ( #10399, #69405, #44050, #15933 ) ) ;
#24669 = CARTESIAN_POINT ( 'NONE',  ( -9.827790563157511022E-16, 128.5570736234661524, 8.025000000000000355 ) ) ;
#24670 = EDGE_LOOP ( 'NONE', ( #42175, #30258 ) ) ;
#24671 = AXIS2_PLACEMENT_3D ( 'NONE', #7412, #54873, #6693 ) ;
#24672 = AXIS2_PLACEMENT_3D ( 'NONE', #35306, #51839, #61650 ) ;
#24673 = SURFACE_SIDE_STYLE ('',( #40205 ) ) ;
#24674 = CARTESIAN_POINT ( 'NONE',  ( -45.64493973069768629, 8.371839367610334648, 6.471715848474669741 ) ) ;
#24675 = CARTESIAN_POINT ( 'NONE',  ( 44.81375845693835203, 9.999999999999982236, 3.255894049711700600 ) ) ;
#24676 = CARTESIAN_POINT ( 'NONE',  ( -57.48951619522305378, -8.499999999999996447, -0.6003161102129058735 ) ) ;
#24677 = ORIENTED_EDGE ( 'NONE', *, *, #38883, .F. ) ;
#24678 = CARTESIAN_POINT ( 'NONE',  ( -161.1550000000000011, 7.632228543268600340, 2.479861379858949277 ) ) ;
#24679 = EDGE_CURVE ( 'NONE', #51004, #49493, #19328, .T. ) ;
#24680 = ORIENTED_EDGE ( 'NONE', *, *, #43201, .F. ) ;
#24681 = CARTESIAN_POINT ( 'NONE',  ( -20.77867704735745136, 115.1383905251040716, -10.00000000000000000 ) ) ;
#24682 = CARTESIAN_POINT ( 'NONE',  ( 53.00000000000000000, 25.24999999999998579, 3.750000000000000000 ) ) ;
#24684 = EDGE_CURVE ( 'NONE', #28127, #39701, #22580, .T. ) ;
#24683 = ORIENTED_EDGE ( 'NONE', *, *, #28489, .T. ) ;
#24685 = CARTESIAN_POINT ( 'NONE',  ( -43.75000000000000000, -13.49999999999999645, 8.000000000000000000 ) ) ;
#24686 = EDGE_CURVE ( 'NONE', #38153, #10996, #8162, .T. ) ;
#24687 = DIRECTION ( 'NONE',  ( 1.000000000000000000, 0.000000000000000000, 0.000000000000000000 ) ) ;
#24688 = CARTESIAN_POINT ( 'NONE',  ( -6.826472737025120807, 158.1070736234661922, 4.959722759717906548 ) ) ;
#24689 = VECTOR ( 'NONE', #16591, 1000.000000000000227 ) ;
#24690 =( GEOMETRIC_REPRESENTATION_CONTEXT ( 3 ) GLOBAL_UNCERTAINTY_ASSIGNED_CONTEXT ( ( #14304 ) ) GLOBAL_UNIT_ASSIGNED_CONTEXT ( ( #23991, #16253, #63006 ) ) REPRESENTATION_CONTEXT ( 'NONE', 'WORKASPACE' ) );
#24691 = ORIENTED_EDGE ( 'NONE', *, *, #23360, .F. ) ;
#24692 = DIRECTION ( 'NONE',  ( -0.07898106964430656740, -0.9968761159932768567, 0.000000000000000000 ) ) ;
#24694 = EDGE_CURVE ( 'NONE', #58540, #1721, #59863, .T. ) ;
#24693 = CARTESIAN_POINT ( 'NONE',  ( -8.102448949553179958, 111.6049999999999613, 5.886773742842747126 ) ) ;
#24695 = CARTESIAN_POINT ( 'NONE',  ( -76.70499999999999829, 2.607480562269072433, 8.024999999999991473 ) ) ;
#24696 = CARTESIAN_POINT ( 'NONE',  ( 82.09357085539566867, 5.000000000000000000, -32.00402776293823592 ) ) ;
#24697 = ORIENTED_EDGE ( 'NONE', *, *, #34232, .T. ) ;
#24698 = CARTESIAN_POINT ( 'NONE',  ( 9.058813317711338797, 139.9549999999999841, -2.943386871421372675 ) ) ;
#24699 = PRESENTATION_LAYER_ASSIGNMENT (  '', '', ( #28037 ) ) ;
#24700 = SURFACE_STYLE_FILL_AREA ( #45855 ) ;
#24701 = DIRECTION ( 'NONE',  ( 0.000000000000000000, 0.000000000000000000, -1.000000000000000000 ) ) ;
#24702 = SURFACE_STYLE_FILL_AREA ( #41286 ) ;
#24703 = FACE_OUTER_BOUND ( 'NONE', #11641, .T. ) ;
#24704 = ORIENTED_EDGE ( 'NONE', *, *, #3914, .F. ) ;
#24705 = FACE_OUTER_BOUND ( 'NONE', #16862, .T. ) ;
#24707 = CARTESIAN_POINT ( 'NONE',  ( -52.19499999999999318, 8.437984349512085203, -1.550032578732815448E-15 ) ) ;
#24706 = AXIS2_PLACEMENT_3D ( 'NONE', #29122, #1996, #61161 ) ;
#24708 = ORIENTED_EDGE ( 'NONE', *, *, #61758, .T. ) ;
#24709 =( BOUNDED_CURVE ( )  B_SPLINE_CURVE ( 2, ( #20114, #26095, #3565, #69034, #36365, #25408, #62678, #56744, #41991, #8556, #8886 ),
 .UNSPECIFIED., .F., .F. ) 
 B_SPLINE_CURVE_WITH_KNOTS ( ( 3, 2, 2, 2, 2, 3 ),
 ( 0.7391304347826086474, 0.7413043478260870067, 0.7434782608695652550, 0.7456521739130435034, 0.7478260869565217517, 0.7500000000000000000 ),
 .UNSPECIFIED. ) 
 CURVE ( )  GEOMETRIC_REPRESENTATION_ITEM ( )  RATIONAL_B_SPLINE_CURVE ( ( 1.000000000000000000, 0.9510565162951535312, 1.000000000000000000, 0.9510565162951535312, 1.000000000000000000, 0.9510565162951535312, 1.000000000000000000, 0.9510565162951535312, 1.000000000000000000, 0.9510565162951535312, 1.000000000000000000 ) ) 
 REPRESENTATION_ITEM ( '' )  );
#24710 = CARTESIAN_POINT ( 'NONE',  ( 7.863253753129176182, 111.2778445948750203, 3.841316429231172780 ) ) ;
#24711 = CARTESIAN_POINT ( 'NONE',  ( 0.000000000000000000, 115.0570736234661666, -8.025000000000000355 ) ) ;
#24712 = CARTESIAN_POINT ( 'NONE',  ( -45.54107139885136490, 7.944008872641631136, -6.500000000000004441 ) ) ;
#24713 = AXIS2_PLACEMENT_3D ( 'NONE', #46809, #51338, #68216 ) ;
#24714 = PRESENTATION_STYLE_ASSIGNMENT (( #68016 ) ) ;
#24715 = EDGE_LOOP ( 'NONE', ( #65494, #2466, #44105, #25604 ) ) ;
#24716 = DIRECTION ( 'NONE',  ( 1.000000000000000000, 7.709882115452469292E-16, 0.000000000000000000 ) ) ;
#24717 = ORIENTED_EDGE ( 'NONE', *, *, #44604, .T. ) ;
#24718 = FACE_OUTER_BOUND ( 'NONE', #66360, .T. ) ;
#24719 = CARTESIAN_POINT ( 'NONE',  ( -106.1049999999999756, -6.826472737025115478, 4.959722759717900331 ) ) ;
#24720 = VERTEX_POINT ( 'NONE', #48666 ) ;
#24721 = FACE_OUTER_BOUND ( 'NONE', #12140, .T. ) ;
#24722 = STYLED_ITEM ( 'NONE', ( #33944 ), #21122 ) ;
#24723 = PLANE ( 'NONE',  #26870 ) ;
#24724 = VECTOR ( 'NONE', #15869, 1000.000000000000000 ) ;
#24725 = CARTESIAN_POINT ( 'NONE',  ( -145.1070736234661638, 8.102448949553171076, -5.886773742842744461 ) ) ;
#24726 = DIRECTION ( 'NONE',  ( 0.000000000000000000, 0.000000000000000000, -1.000000000000000000 ) ) ;
#24727 = CARTESIAN_POINT ( 'NONE',  ( -9.058813317711338797, 140.3449999999999989, 2.943386871421373563 ) ) ;
#24728 = CARTESIAN_POINT ( 'NONE',  ( -70.70707362346615810, -3.094860106618431139, -9.524999999999991473 ) ) ;
#24729 = VECTOR ( 'NONE', #24664, 1000.000000000000000 ) ;
#24730 = CARTESIAN_POINT ( 'NONE',  ( 7.000000000000017764, 42.74314482547740113, -27.71473342867655987 ) ) ;
#24731 = SURFACE_SIDE_STYLE ('',( #4301 ) ) ;
#24732 = CIRCLE ( 'NONE', #39343, 17.00000000000000711 ) ;
#24733 = PRESENTATION_STYLE_ASSIGNMENT (( #66988 ) ) ;
#24735 =( LENGTH_UNIT ( ) NAMED_UNIT ( * ) SI_UNIT ( .MILLI., .METRE. ) );
#24734 = CARTESIAN_POINT ( 'NONE',  ( -169.5570736234661808, -1.166476076187852838E-15, -9.524999999999991473 ) ) ;
#24736 = CARTESIAN_POINT ( 'NONE',  ( -117.3549999999999898, -4.716976649647093289, -6.492361379858945902 ) ) ;
#24737 = CARTESIAN_POINT ( 'NONE',  ( -158.0929263765341375, 3.094860106624147011, 9.524999999995840128 ) ) ;
#24738 = CARTESIAN_POINT ( 'NONE',  ( 8.102448949553183510, 111.9949999999999761, -5.886773742842746238 ) ) ;
#24739 = CARTESIAN_POINT ( 'NONE',  ( -126.1450000000000102, -4.716976649647092401, 6.492361379858946790 ) ) ;
#24740 = AXIS2_PLACEMENT_3D ( 'NONE', #9495, #30916, #40820 ) ;
#24741 = CARTESIAN_POINT ( 'NONE',  ( -116.8449999999999847, -7.632228543268599452, 2.479861379858951054 ) ) ;
#24742 = ORIENTED_EDGE ( 'NONE', *, *, #5383, .T. ) ;
#24743 = AXIS2_PLACEMENT_3D ( 'NONE', #57300, #35158, #9128 ) ;
#24744 = CARTESIAN_POINT ( 'NONE',  ( 0.000000000000000000, 114.4999999999999574, 0.000000000000000000 ) ) ;
#24745 = PRODUCT_DEFINITION_FORMATION_WITH_SPECIFIED_SOURCE ( 'ANY', '', #21518, .NOT_KNOWN. ) ;
#24746 = CARTESIAN_POINT ( 'NONE',  ( 44.99999999999977973, 146.9999999999999716, 7.500000000000000000 ) ) ;
#24747 = CARTESIAN_POINT ( 'NONE',  ( -173.3929263765337510, 8.102448949553176405, 5.886773742842740909 ) ) ;
#24748 =( LENGTH_UNIT ( ) NAMED_UNIT ( * ) SI_UNIT ( .MILLI., .METRE. ) );
#24749 = CIRCLE ( 'NONE', #41625, 17.42000000000001236 ) ;
#24750 = CARTESIAN_POINT ( 'NONE',  ( -51.74499999999998323, 4.716976649647094177, 6.492361379858945902 ) ) ;
#24751 = EDGE_CURVE ( 'NONE', #66441, #53362, #69693, .T. ) ;
#24752 = DIRECTION ( 'NONE',  ( -0.000000000000000000, -0.000000000000000000, -1.000000000000000000 ) ) ;
#24753 = CARTESIAN_POINT ( 'NONE',  ( -21.02379604162863913, 110.4999999999999858, 10.50000000000000000 ) ) ;
#24754 = ORIENTED_EDGE ( 'NONE', *, *, #31000, .T. ) ;
#24755 = COLOUR_RGB ( '', 0.72549020, 0.75294118, 0.79215686) ;
#24756 = CARTESIAN_POINT ( 'NONE',  ( -83.84292637653379643, 9.058813317711329915, -2.943386871421373119 ) ) ;
#24758 = EDGE_CURVE ( 'NONE', #23750, #23681, #38798, .T. ) ;
#24757 = SURFACE_STYLE_USAGE ( .BOTH. , #8271 ) ;
#24759 = SURFACE_STYLE_USAGE ( .BOTH. , #29350 ) ;
#24760 = AXIS2_PLACEMENT_3D ( 'NONE', #36355, #31019, #57778 ) ;
#24761 = CIRCLE ( 'NONE', #38455, 12.50000000000000000 ) ;
#24762 =( LENGTH_UNIT ( ) NAMED_UNIT ( * ) SI_UNIT ( .MILLI., .METRE. ) );
#24763 = SURFACE_SIDE_STYLE ('',( #18806 ) ) ;
#24764 = CARTESIAN_POINT ( 'NONE',  ( -5.196152422706636465, 2.500000000000000000, 9.000000000000001776 ) ) ;
#24765 = CARTESIAN_POINT ( 'NONE',  ( -157.1070736234661922, 8.102448949553172852, -5.886773742842744461 ) ) ;
#24766 = EDGE_LOOP ( 'NONE', ( #58488, #46638, #4336, #33481 ) ) ;
#24767 = CARTESIAN_POINT ( 'NONE',  ( -45.00000000000000000, 99.99999999999992895, 4.000000000000000000 ) ) ;
#24768 = CYLINDRICAL_SURFACE ( 'NONE', #52232, 1.000000000000000000 ) ;
#24769 = VECTOR ( 'NONE', #25391, 1000.000000000000000 ) ;
#24770 = ADVANCED_FACE ( 'NONE', ( #6048 ), #28295, .F. ) ;
#24771 = LINE ( 'NONE', #51189, #14960 ) ;
#24772 = ORIENTED_EDGE ( 'NONE', *, *, #46692, .F. ) ;
#24773 = CARTESIAN_POINT ( 'NONE',  ( -6.826472737025120807, 134.1070736234661638, 4.959722759717906548 ) ) ;
#24774 = FILL_AREA_STYLE_COLOUR ( '', #27428 ) ;
#24775 = CARTESIAN_POINT ( 'NONE',  ( -6.826472737025120807, 130.5070736234661695, -4.959722759717907437 ) ) ;
#24776 = AXIS2_PLACEMENT_3D ( 'NONE', #23822, #39011, #7639 ) ;
#24777 = ORIENTED_EDGE ( 'NONE', *, *, #7241, .F. ) ;
#24779 = EDGE_CURVE ( 'NONE', #19343, #37744, #4777, .T. ) ;
#24778 = LINE ( 'NONE', #56104, #49614 ) ;
#24780 = CARTESIAN_POINT ( 'NONE',  ( -103.2549999999999812, -4.716976649647092401, 6.492361379858946790 ) ) ;
#24781 = DIRECTION ( 'NONE',  ( 0.000000000000000000, 0.000000000000000000, -1.000000000000000000 ) ) ;
#24782 = AXIS2_PLACEMENT_3D ( 'NONE', #742, #17025, #6432 ) ;
#24783 = CARTESIAN_POINT ( 'NONE',  ( 0.000000000000000000, -2.500000000000000000, 0.000000000000000000 ) ) ;
#24784 = ORIENTED_EDGE ( 'NONE', *, *, #54775, .F. ) ;
#24785 = CARTESIAN_POINT ( 'NONE',  ( 2.000000000000015543, 26.00000000000000355, 23.99999999999999645 ) ) ;
#24786 = CARTESIAN_POINT ( 'NONE',  ( -104.1570736234661751, -9.058813317711329915, -2.943386871421370898 ) ) ;
#24787 = LINE ( 'NONE', #2232, #40081 ) ;
#24788 = CARTESIAN_POINT ( 'NONE',  ( 71.49999999999998579, 64.07124727947029896, 9.500000000000000000 ) ) ;
#24789 = MECHANICAL_DESIGN_GEOMETRIC_PRESENTATION_REPRESENTATION (  '', ( #56229 ), #51784 ) ;
#24790 = CARTESIAN_POINT ( 'NONE',  ( 71.50000000000000000, 14.49137674618942562, 7.500000000000000000 ) ) ;
#24791 = CARTESIAN_POINT ( 'NONE',  ( -83.09499999999999886, -2.607480562269071545, -8.024999999999991473 ) ) ;
#24792 = ORIENTED_EDGE ( 'NONE', *, *, #61221, .F. ) ;
#24793 = VECTOR ( 'NONE', #28993, 1000.000000000000000 ) ;
#24794 = DIRECTION ( 'NONE',  ( 1.000000000000000000, -0.000000000000000000, 0.000000000000000000 ) ) ;
#24795 = UNCERTAINTY_MEASURE_WITH_UNIT (LENGTH_MEASURE( 1.000000000000000082E-05 ), #24519, 'distance_accuracy_value', 'NONE');
#24796 = EDGE_LOOP ( 'NONE', ( #66672, #44184, #29757, #7917 ) ) ;
#24797 = CARTESIAN_POINT ( 'NONE',  ( -76.94292637653380496, 0.000000000000000000, 9.524999999999991473 ) ) ;
#24798 = SURFACE_STYLE_FILL_AREA ( #7593 ) ;
#24799 = CARTESIAN_POINT ( 'NONE',  ( -1.011095968855053334E-15, -8.500000000000000000, 21.00000000000000000 ) ) ;
#24800 = EDGE_LOOP ( 'NONE', ( #52493, #27131, #25245, #66337 ) ) ;
#24801 =( LENGTH_UNIT ( ) NAMED_UNIT ( * ) SI_UNIT ( .MILLI., .METRE. ) );
#24802 = ORIENTED_EDGE ( 'NONE', *, *, #60732, .F. ) ;
#24803 = SURFACE_STYLE_FILL_AREA ( #9358 ) ;
#24804 = CARTESIAN_POINT ( 'NONE',  ( -150.1429263765338078, 5.598654528085800663, -7.705886871421367523 ) ) ;
#24805 = CARTESIAN_POINT ( 'NONE',  ( -167.9070736234661751, -3.094860106618429807, 9.524999999999991473 ) ) ;
#24806 = AXIS2_PLACEMENT_3D ( 'NONE', #7309, #28736, #66031 ) ;
#24807 = SURFACE_STYLE_FILL_AREA ( #13566 ) ;
#24808 = CARTESIAN_POINT ( 'NONE',  ( -1.166476076187854022E-15, 116.9449999999999932, 9.525000000000000355 ) ) ;
#24809 =( BOUNDED_CURVE ( )  B_SPLINE_CURVE ( 3, ( #10707, #37496, #63484, #19864 ),
 .UNSPECIFIED., .F., .F. ) 
 B_SPLINE_CURVE_WITH_KNOTS ( ( 4, 4 ),
 ( 1.570796326794893227, 3.141592653589793116 ),
 .UNSPECIFIED. ) 
 CURVE ( )  GEOMETRIC_REPRESENTATION_ITEM ( )  RATIONAL_B_SPLINE_CURVE ( ( 1.000000000000000000, 0.8047378541243641603, 0.8047378541243641603, 1.000000000000000000 ) ) 
 REPRESENTATION_ITEM ( '' )  );
#24810 = CARTESIAN_POINT ( 'NONE',  ( -108.0570736234661666, 0.000000000000000000, 9.524999999999991473 ) ) ;
#24811 = ADVANCED_FACE ( 'NONE', ( #69388 ), #5681, .T. ) ;
#24812 =( NAMED_UNIT ( * ) PLANE_ANGLE_UNIT ( ) SI_UNIT ( $, .RADIAN. ) );
#24813 = PRESENTATION_LAYER_ASSIGNMENT (  '', '', ( #52917 ) ) ;
#24814 = CARTESIAN_POINT ( 'NONE',  ( -65.30707362346618083, -10.01517768586948698, 6.132527647946031529E-16 ) ) ;
#24815 = ORIENTED_EDGE ( 'NONE', *, *, #61376, .T. ) ;
#24816 = DIRECTION ( 'NONE',  ( -0.000000000000000000, -1.000000000000000000, 0.000000000000000000 ) ) ;
#24817 = CARTESIAN_POINT ( 'NONE',  ( 23.21231517720797655, 113.4999999999999858, 9.500000000000000000 ) ) ;
#24820 = AXIS2_PLACEMENT_3D ( 'NONE', #53079, #32291, #58018 ) ;
#24819 =( LENGTH_UNIT ( ) NAMED_UNIT ( * ) SI_UNIT ( .MILLI., .METRE. ) );
#24818 = LINE ( 'NONE', #46335, #13242 ) ;
#24821 = FILL_AREA_STYLE ('',( #15367 ) ) ;
#24822 = CARTESIAN_POINT ( 'NONE',  ( -153.0550000000000068, -9.827790563157499189E-16, -8.024999999999991473 ) ) ;
#24823 = CARTESIAN_POINT ( 'NONE',  ( -75.00000000000000000, 9.708372675170620525, 6.100915009778867137 ) ) ;
#24824 = CARTESIAN_POINT ( 'NONE',  ( -8.337051230037234362, 111.6531430745036886, 0.8624690973152070450 ) ) ;
#24825 = CARTESIAN_POINT ( 'NONE',  ( -167.2450000000000045, -4.716976649647093289, -6.492361379858945902 ) ) ;
#24826 = CARTESIAN_POINT ( 'NONE',  ( -148.6450000000000102, 4.716976649647091513, -6.492361379858946790 ) ) ;
#24827 = AXIS2_PLACEMENT_3D ( 'NONE', #62759, #29732, #46659 ) ;
#24828 = ORIENTED_EDGE ( 'NONE', *, *, #28292, .F. ) ;
#24829 = AXIS2_PLACEMENT_3D ( 'NONE', #43185, #48103, #5131 ) ;
#24830 = CARTESIAN_POINT ( 'NONE',  ( -70.75000000000000000, -3.000000000000000000, 20.00000000000000000 ) ) ;
#24831 =( NAMED_UNIT ( * ) SI_UNIT ( $, .STERADIAN. ) SOLID_ANGLE_UNIT ( ) );
#24832 = UNCERTAINTY_MEASURE_WITH_UNIT (LENGTH_MEASURE( 1.000000000000000082E-05 ), #9868, 'distance_accuracy_value', 'NONE');
#24833 = CARTESIAN_POINT ( 'NONE',  ( -63.65499999999998693, -7.632228543268600340, -2.479861379858950166 ) ) ;
#24834 = PLANE ( 'NONE',  #42806 ) ;
#24835 = CIRCLE ( 'NONE', #64158, 0.5000000000000004441 ) ;
#24836 = DIRECTION ( 'NONE',  ( 0.000000000000000000, 1.000000000000000000, 0.000000000000000000 ) ) ;
#24837 = ADVANCED_FACE ( 'NONE', ( #42695 ), #37428, .T. ) ;
#24838 = CARTESIAN_POINT ( 'NONE',  ( -66.14499999999998181, -4.716976649647092401, 6.492361379858946790 ) ) ;
#24839 = EDGE_CURVE ( 'NONE', #26439, #33948, #57559, .T. ) ;
#24840 = CARTESIAN_POINT ( 'NONE',  ( 0.000000000000000000, 158.5550000000000068, -9.525000000000000355 ) ) ;
#24841 = FACE_OUTER_BOUND ( 'NONE', #58798, .T. ) ;
#24842 = PRESENTATION_LAYER_ASSIGNMENT (  '', '', ( #32677 ) ) ;
#24843 = CARTESIAN_POINT ( 'NONE',  ( -0.7423632831649431552, 154.4999999999999716, -9.503379274660218812 ) ) ;
#24844 = UNCERTAINTY_MEASURE_WITH_UNIT (LENGTH_MEASURE( 1.000000000000000082E-05 ), #65869, 'distance_accuracy_value', 'NONE');
#24845 = DIRECTION ( 'NONE',  ( 1.000000000000000000, 0.000000000000000000, 0.000000000000000000 ) ) ;
#24846 = ADVANCED_FACE ( 'NONE', ( #67217 ), #55964, .T. ) ;
#24847 = FACE_OUTER_BOUND ( 'NONE', #19057, .T. ) ;
#24848 = PRESENTATION_LAYER_ASSIGNMENT (  '', '', ( #20346 ) ) ;
#24849 = AXIS2_PLACEMENT_3D ( 'NONE', #23960, #22941, #44438 ) ;
#24850 = DIRECTION ( 'NONE',  ( 0.000000000000000000, 0.000000000000000000, 1.000000000000000000 ) ) ;
#24851 = DIRECTION ( 'NONE',  ( 0.000000000000000000, -1.000000000000000000, 0.000000000000000000 ) ) ;
#24852 = ADVANCED_FACE ( 'NONE', ( #50355 ), #17672, .F. ) ;
#24853 = DIRECTION ( 'NONE',  ( -0.000000000000000000, -0.000000000000000000, 1.000000000000000000 ) ) ;
#24854 = VERTEX_POINT ( 'NONE', #39141 ) ;
#24855 = VERTEX_POINT ( 'NONE', #33813 ) ;
#24856 = FILL_AREA_STYLE_COLOUR ( '', #29645 ) ;
#24857 = AXIS2_PLACEMENT_3D ( 'NONE', #53919, #5720, #27166 ) ;
#24858 = CARTESIAN_POINT ( 'NONE',  ( -2.607480562269073765, 109.2070736234661439, -8.025000000000000355 ) ) ;
#24859 = PRESENTATION_LAYER_ASSIGNMENT (  '', '', ( #28159 ) ) ;
#24861 = EDGE_CURVE ( 'NONE', #34471, #18929, #14790, .T. ) ;
#24860 = FILL_AREA_STYLE ('',( #7055 ) ) ;
#24862 = SURFACE_STYLE_USAGE ( .BOTH. , #56890 ) ;
#24863 = ORIENTED_EDGE ( 'NONE', *, *, #59801, .T. ) ;
#24864 = AXIS2_PLACEMENT_3D ( 'NONE', #59013, #56057, #37954 ) ;
#24865 = ORIENTED_EDGE ( 'NONE', *, *, #47304, .T. ) ;
#24866 = CARTESIAN_POINT ( 'NONE',  ( -71.49999999999998579, 64.07124727947029896, 7.000000000000000000 ) ) ;
#24867 =( NAMED_UNIT ( * ) PLANE_ANGLE_UNIT ( ) SI_UNIT ( $, .RADIAN. ) );
#24868 = ORIENTED_EDGE ( 'NONE', *, *, #40105, .F. ) ;
#24869 = CARTESIAN_POINT ( 'NONE',  ( 5.598654528085809545, 113.2549999999999812, -7.705886871421373741 ) ) ;
#24870 = CARTESIAN_POINT ( 'NONE',  ( 23.00000000000000000, 5.000000000000000000, -24.00402776293825013 ) ) ;
#24871 = ORIENTED_EDGE ( 'NONE', *, *, #67748, .F. ) ;
#24872 = STYLED_ITEM ( 'NONE', ( #63968 ), #22015 ) ;
#24873 = AXIS2_PLACEMENT_3D ( 'NONE', #32323, #48208, #65386 ) ;
#24874 = CARTESIAN_POINT ( 'NONE',  ( -11.74999999999999645, -3.000000000000000000, 19.00000000000000000 ) ) ;
#24875 = CARTESIAN_POINT ( 'NONE',  ( -114.4449999999999932, 0.000000000000000000, 8.024999999999991473 ) ) ;
#24876 = EDGE_LOOP ( 'NONE', ( #56038, #7743, #61989, #61702 ) ) ;
#24877 =( GEOMETRIC_REPRESENTATION_CONTEXT ( 3 ) GLOBAL_UNCERTAINTY_ASSIGNED_CONTEXT ( ( #19400 ) ) GLOBAL_UNIT_ASSIGNED_CONTEXT ( ( #68396, #45601, #8279 ) ) REPRESENTATION_CONTEXT ( 'NONE', 'WORKASPACE' ) );
#24878 = APPLICATION_CONTEXT ( 'automotive_design' ) ;
#24879 = FACE_OUTER_BOUND ( 'NONE', #36935, .T. ) ;
#24880 = CARTESIAN_POINT ( 'NONE',  ( -53.39292637653380780, 8.102448949553176405, 5.886773742842740909 ) ) ;
#24881 = DIRECTION ( 'NONE',  ( -0.7071067811865352493, 0.000000000000000000, -0.7071067811865597852 ) ) ;
#24882 = ORIENTED_EDGE ( 'NONE', *, *, #54170, .F. ) ;
#24883 = CARTESIAN_POINT ( 'NONE',  ( -8.437984349512095861, 147.6929263765338192, -5.166775262442723748E-16 ) ) ;
#24884 = CARTESIAN_POINT ( 'NONE',  ( -9.827790563157511022E-16, 146.5570736234661524, 8.025000000000000355 ) ) ;
#24885 = CIRCLE ( 'NONE', #56325, 0.2500000000000002220 ) ;
#24886 = DIRECTION ( 'NONE',  ( 1.074176415464006764E-16, -1.000000000000000000, 0.000000000000000000 ) ) ;
#24887 = VECTOR ( 'NONE', #61832, 1000.000000000000000 ) ;
#24888 = VERTEX_POINT ( 'NONE', #30605 ) ;
#24889 = DIRECTION ( 'NONE',  ( -0.9968761159932768567, 0.07898106964430649801, 0.000000000000000000 ) ) ;
#24890 = ORIENTED_EDGE ( 'NONE', *, *, #45943, .F. ) ;
#24891 = DIRECTION ( 'NONE',  ( -1.000000000000000000, 0.000000000000000000, 0.000000000000000000 ) ) ;
#24892 = DIRECTION ( 'NONE',  ( -1.000000000000000000, 0.000000000000000000, 0.000000000000000000 ) ) ;
#24893 = CARTESIAN_POINT ( 'NONE',  ( 41.03154609328242941, 107.7014457728230354, -3.191672614837956612 ) ) ;
#24894 = CARTESIAN_POINT ( 'NONE',  ( -122.7549999999999955, 4.716976649647091513, -6.492361379858946790 ) ) ;
#24895 = DIRECTION ( 'NONE',  ( 0.000000000000000000, 1.000000000000000000, 0.000000000000000000 ) ) ;
#24896 = FILL_AREA_STYLE_COLOUR ( '', #40019 ) ;
#24897 = EDGE_CURVE ( 'NONE', #1324, #1454, #36312, .T. ) ;
#24898 = CIRCLE ( 'NONE', #12545, 0.2500000000000002220 ) ;
#24899 =( LENGTH_UNIT ( ) NAMED_UNIT ( * ) SI_UNIT ( .MILLI., .METRE. ) );
#24900 = CARTESIAN_POINT ( 'NONE',  ( 30.25000000000000711, 18.74999999999997868, -3.750000000000000000 ) ) ;
#24901 = SURFACE_STYLE_USAGE ( .BOTH. , #57982 ) ;
#24902 = EDGE_LOOP ( 'NONE', ( #40072, #69116, #55152, #68019 ) ) ;
#24903 = PRESENTATION_LAYER_ASSIGNMENT (  '', '', ( #19270 ) ) ;
#24904 = ORIENTED_EDGE ( 'NONE', *, *, #56333, .T. ) ;
#24905 = DIRECTION ( 'NONE',  ( 0.000000000000000000, 0.000000000000000000, -1.000000000000000000 ) ) ;
#24906 = CARTESIAN_POINT ( 'NONE',  ( -103.9429263765338050, 0.000000000000000000, 9.524999999999991473 ) ) ;
#24907 = CARTESIAN_POINT ( 'NONE',  ( 7.632228543268607446, 114.1570736234661609, 2.479861379858954606 ) ) ;
#24908 = ORIENTED_EDGE ( 'NONE', *, *, #33043, .T. ) ;
#24909 = DIRECTION ( 'NONE',  ( -0.000000000000000000, 0.000000000000000000, 1.000000000000000000 ) ) ;
#24910 = CARTESIAN_POINT ( 'NONE',  ( -176.1550000000000011, 7.632228543268600340, 2.479861379858949277 ) ) ;
#24911 = CARTESIAN_POINT ( 'NONE',  ( 22.00000000000002132, 50.00000000000000000, 46.00000000000000000 ) ) ;
#24912 = CARTESIAN_POINT ( 'NONE',  ( -60.65707362346617515, 9.058813317711329915, 2.943386871421369566 ) ) ;
#24913 = COLOUR_RGB ( '', 0.09019608, 0.27058824, 0.51372549) ;
#24914 = CARTESIAN_POINT ( 'NONE',  ( -175.1949999999999932, 8.437984349512086979, -1.550032578732815448E-15 ) ) ;
#24915 = SURFACE_SIDE_STYLE ('',( #3421 ) ) ;
#24916 = VERTEX_POINT ( 'NONE', #8822 ) ;
#24917 = CARTESIAN_POINT ( 'NONE',  ( 9.000000000000003553, 24.99999999999998579, 3.750000000000000000 ) ) ;
#24918 = AXIS2_PLACEMENT_3D ( 'NONE', #32410, #38091, #60202 ) ;
#24919 = ADVANCED_FACE ( 'NONE', ( #68270 ), #20049, .F. ) ;
#24920 = VECTOR ( 'NONE', #38216, 1000.000000000000000 ) ;
#24921 =( NAMED_UNIT ( * ) SI_UNIT ( $, .STERADIAN. ) SOLID_ANGLE_UNIT ( ) );
#24922 = DIRECTION ( 'NONE',  ( 0.000000000000000000, 0.000000000000000000, -1.000000000000000000 ) ) ;
#24923 = CARTESIAN_POINT ( 'NONE',  ( -88.55499999999999261, 0.000000000000000000, 8.024999999999991473 ) ) ;
#24924 =( NAMED_UNIT ( * ) PLANE_ANGLE_UNIT ( ) SI_UNIT ( $, .RADIAN. ) );
#24925 = CARTESIAN_POINT ( 'NONE',  ( 2.000000000000008882, 26.00000000000000355, -24.00000000000000355 ) ) ;
#24926 = CIRCLE ( 'NONE', #64233, 0.5000000000000004441 ) ;
#24927 = LINE ( 'NONE', #68208, #29212 ) ;
#24928 = EDGE_CURVE ( 'NONE', #53321, #38434, #49732, .T. ) ;
#24929 = CARTESIAN_POINT ( 'NONE',  ( -88.19499999999996476, 8.437984349512086979, -1.550032578732815448E-15 ) ) ;
#24930 = ADVANCED_FACE ( 'NONE', ( #41217 ), #51749, .F. ) ;
#24931 = CARTESIAN_POINT ( 'NONE',  ( 8.102448949553183510, 128.1049999999999898, -5.886773742842746238 ) ) ;
#24932 = CARTESIAN_POINT ( 'NONE',  ( -66.59499999999999886, 2.607480562269073321, 8.024999999999991473 ) ) ;
#24933 = AXIS2_PLACEMENT_3D ( 'NONE', #17800, #24781, #46298 ) ;
#24934 = LINE ( 'NONE', #10159, #8388 ) ;
#24935 = VECTOR ( 'NONE', #1116, 1000.000000000000000 ) ;
#24936 =( LENGTH_UNIT ( ) NAMED_UNIT ( * ) SI_UNIT ( .MILLI., .METRE. ) );
#24937 = UNCERTAINTY_MEASURE_WITH_UNIT (LENGTH_MEASURE( 1.000000000000000082E-05 ), #46089, 'distance_accuracy_value', 'NONE');
#24938 = VECTOR ( 'NONE', #39905, 1000.000000000000000 ) ;
#24939 = DIRECTION ( 'NONE',  ( -1.000000000000000000, 0.000000000000000000, 0.000000000000000000 ) ) ;
#24940 = ORIENTED_EDGE ( 'NONE', *, *, #8132, .T. ) ;
#24941 = EDGE_CURVE ( 'NONE', #29891, #67533, #53098, .T. ) ;
#24942 = CARTESIAN_POINT ( 'NONE',  ( -115.1929263765338050, -10.01517768586948698, 6.132527647946031529E-16 ) ) ;
#24943 = CARTESIAN_POINT ( 'NONE',  ( -131.5449999999999875, -7.632228543268600340, -2.479861379858950166 ) ) ;
#24945 = PRESENTATION_STYLE_ASSIGNMENT (( #46819 ) ) ;
#24944 = AXIS2_PLACEMENT_3D ( 'NONE', #29968, #51431, #14151 ) ;
#24946 = EDGE_CURVE ( 'NONE', #56993, #19879, #1360, .T. ) ;
#24947 = AXIS2_PLACEMENT_3D ( 'NONE', #33905, #55372, #2175 ) ;
#24948 = DIRECTION ( 'NONE',  ( 0.000000000000000000, 0.000000000000000000, 1.000000000000000000 ) ) ;
#24949 = FACE_OUTER_BOUND ( 'NONE', #17546, .T. ) ;
#24950 = SURFACE_SIDE_STYLE ('',( #62578 ) ) ;
#24951 = VERTEX_POINT ( 'NONE', #46865 ) ;
#24952 = ORIENTED_EDGE ( 'NONE', *, *, #3124, .F. ) ;
#24953 = LINE ( 'NONE', #51353, #40991 ) ;
#24954 = CARTESIAN_POINT ( 'NONE',  ( -6.826472737025120807, 147.3929263765337794, -4.959722759717907437 ) ) ;
#24955 = SURFACE_SIDE_STYLE ('',( #56632 ) ) ;
#24956 = FILL_AREA_STYLE ('',( #51708 ) ) ;
#24957 = PLANE ( 'NONE',  #50989 ) ;
#24958 = ORIENTED_EDGE ( 'NONE', *, *, #68464, .F. ) ;
#24959 = CARTESIAN_POINT ( 'NONE',  ( -127.4049999999999869, -2.607480562269069768, 8.024999999999991473 ) ) ;
#24960 = EDGE_LOOP ( 'NONE', ( #61281, #25553, #4358, #36786 ) ) ;
#24961 = DIRECTION ( 'NONE',  ( 1.000000000000000000, 0.000000000000000000, 0.000000000000000000 ) ) ;
#24962 = CARTESIAN_POINT ( 'NONE',  ( -119.9070736234661609, -3.094860106618429807, 9.524999999999991473 ) ) ;
#24963 = EDGE_CURVE ( 'NONE', #30586, #17689, #43055, .T. ) ;
#24964 = ORIENTED_EDGE ( 'NONE', *, *, #16159, .T. ) ;
#24965 = FACE_OUTER_BOUND ( 'NONE', #39289, .T. ) ;
#24966 = DIRECTION ( 'NONE',  ( 1.000000000000000000, 0.000000000000000000, 0.000000000000000000 ) ) ;
#24967 = VERTEX_POINT ( 'NONE', #11581 ) ;
#24968 = VECTOR ( 'NONE', #56167, 1000.000000000000000 ) ;
#24969 = EDGE_CURVE ( 'NONE', #10638, #29261, #21104, .T. ) ;
#24970 = DIRECTION ( 'NONE',  ( 0.000000000000000000, 0.000000000000000000, 1.000000000000000000 ) ) ;
#24971 = CARTESIAN_POINT ( 'NONE',  ( -3.094860106618434248, 143.7949999999999875, 9.525000000000000355 ) ) ;
#24972 =( LENGTH_UNIT ( ) NAMED_UNIT ( * ) SI_UNIT ( .MILLI., .METRE. ) );
#24973 = ORIENTED_EDGE ( 'NONE', *, *, #6200, .T. ) ;
#24974 = DIRECTION ( 'NONE',  ( 0.000000000000000000, 1.000000000000000000, -0.000000000000000000 ) ) ;
#24975 = CARTESIAN_POINT ( 'NONE',  ( 8.102448949553181734, 149.1049999999999898, -5.886773742842746238 ) ) ;
#24976 = CARTESIAN_POINT ( 'NONE',  ( 34.99999999999999289, 99.99999999999998579, -7.000000000000000000 ) ) ;
#24977 = SURFACE_SIDE_STYLE ('',( #24611 ) ) ;
#24978 = ORIENTED_EDGE ( 'NONE', *, *, #68940, .F. ) ;
#24979 = CARTESIAN_POINT ( 'NONE',  ( -7.632228543268608334, 120.8429263765338249, 2.479861379858952830 ) ) ;
#24980 = CARTESIAN_POINT ( 'NONE',  ( -71.50000000000000000, 50.00000000000000000, 7.000000000000000000 ) ) ;
#24981 = UNCERTAINTY_MEASURE_WITH_UNIT (LENGTH_MEASURE( 1.000000000000000082E-05 ), #50719, 'distance_accuracy_value', 'NONE');
#24982 =( NAMED_UNIT ( * ) SI_UNIT ( $, .STERADIAN. ) SOLID_ANGLE_UNIT ( ) );
#24983 = VECTOR ( 'NONE', #5841, 1000.000000000000000 ) ;
#24984 = CARTESIAN_POINT ( 'NONE',  ( -98.24292637653380211, 5.598654528085804216, 7.705886871421366635 ) ) ;
#24985 = FACE_BOUND ( 'NONE', #4559, .T. ) ;
#24986 = DIRECTION ( 'NONE',  ( -1.000000000000000000, 0.000000000000000000, 0.000000000000000000 ) ) ;
#24987 = EDGE_LOOP ( 'NONE', ( #23442, #63750, #62211, #8622 ) ) ;
#24988 = CARTESIAN_POINT ( 'NONE',  ( 109.0067032876572455, 14.00000000000000000, -19.20378738324562207 ) ) ;
#24989 = ORIENTED_EDGE ( 'NONE', *, *, #40301, .T. ) ;
#24990 = CARTESIAN_POINT ( 'NONE',  ( -56.24292637653380211, 5.598654528085804216, 7.705886871421366635 ) ) ;
#24991 = LINE ( 'NONE', #46500, #14313 ) ;
#24992 = DIRECTION ( 'NONE',  ( 2.312964634635740689E-15, -1.000000000000000000, 0.000000000000000000 ) ) ;
#24993 = CARTESIAN_POINT ( 'NONE',  ( -155.7549999999999955, 4.716976649647091513, -6.492361379858946790 ) ) ;
#24995 = EDGE_LOOP ( 'NONE', ( #40000, #7234, #2869, #27350 ) ) ;
#24994 =( GEOMETRIC_REPRESENTATION_CONTEXT ( 3 ) GLOBAL_UNCERTAINTY_ASSIGNED_CONTEXT ( ( #53874 ) ) GLOBAL_UNIT_ASSIGNED_CONTEXT ( ( #15944, #36376, #42356 ) ) REPRESENTATION_CONTEXT ( 'NONE', 'WORKASPACE' ) );
#24996 = DIRECTION ( 'NONE',  ( 1.000000000000000000, -8.881784197001254296E-16, 0.000000000000000000 ) ) ;
#24997 = UNCERTAINTY_MEASURE_WITH_UNIT (LENGTH_MEASURE( 1.000000000000000082E-05 ), #64629, 'distance_accuracy_value', 'NONE');
#24998 = AXIS2_PLACEMENT_3D ( 'NONE', #51286, #35464, #4101 ) ;
#24999 = CARTESIAN_POINT ( 'NONE',  ( -55.47676709573605081, -8.704246530741306387, 6.357025138608363157 ) ) ;
#25000 = CARTESIAN_POINT ( 'NONE',  ( 75.00000000000000000, 20.36037960999351881, 6.130923279862163788 ) ) ;
#25001 = CARTESIAN_POINT ( 'NONE',  ( -74.99999999999998579, 50.00000000000000000, 11.50000000000000000 ) ) ;
#25002 = ORIENTED_EDGE ( 'NONE', *, *, #27682, .F. ) ;
#25003 = SURFACE_STYLE_FILL_AREA ( #3500 ) ;
#25004 = VERTEX_POINT ( 'NONE', #64716 ) ;
#25005 = CYLINDRICAL_SURFACE ( 'NONE', #21550, 0.2500000000000002220 ) ;
#25006 = PRESENTATION_STYLE_ASSIGNMENT (( #3504 ) ) ;
#25007 = AXIS2_PLACEMENT_3D ( 'NONE', #30017, #8240, #56771 ) ;
#25008 = CARTESIAN_POINT ( 'NONE',  ( -68.45499999999998408, 7.632228543268599452, -2.479861379858951942 ) ) ;
#25009 = ORIENTED_EDGE ( 'NONE', *, *, #40958, .T. ) ;
#25010 = DIRECTION ( 'NONE',  ( -1.000000000000000000, 0.000000000000000000, 0.000000000000000000 ) ) ;
#25011 = CIRCLE ( 'NONE', #53088, 1.000000000000000888 ) ;
#25012 = EDGE_CURVE ( 'NONE', #20601, #373, #60950, .T. ) ;
#25013 =( LENGTH_UNIT ( ) NAMED_UNIT ( * ) SI_UNIT ( .MILLI., .METRE. ) );
#25014 = DIRECTION ( 'NONE',  ( -0.000000000000000000, -1.000000000000000000, -0.000000000000000000 ) ) ;
#25015 = ORIENTED_EDGE ( 'NONE', *, *, #13825, .F. ) ;
#25016 = PRESENTATION_LAYER_ASSIGNMENT (  '', '', ( #9316 ) ) ;
#25017 = ADVANCED_FACE ( 'NONE', ( #54490 ), #58747, .F. ) ;
#25018 = PRESENTATION_LAYER_ASSIGNMENT (  '', '', ( #43050 ) ) ;
#25019 = CARTESIAN_POINT ( 'NONE',  ( -45.91547277936962246, 9.430195807687219656, -6.500000000000000000 ) ) ;
#25020 = DIRECTION ( 'NONE',  ( -0.000000000000000000, -0.000000000000000000, -1.000000000000000000 ) ) ;
#25022 =( NAMED_UNIT ( * ) SI_UNIT ( $, .STERADIAN. ) SOLID_ANGLE_UNIT ( ) );
#25021 = DIRECTION ( 'NONE',  ( -0.000000000000000000, -0.000000000000000000, -1.000000000000000000 ) ) ;
#25023 = EDGE_CURVE ( 'NONE', #59058, #36322, #63669, .T. ) ;
#25024 = CARTESIAN_POINT ( 'NONE',  ( 9.058813317711337021, 153.5449999999999875, 2.943386871421375783 ) ) ;
#25025 = CARTESIAN_POINT ( 'NONE',  ( -100.3449999999999847, 7.632228543268599452, -2.479861379858951942 ) ) ;
#25026 = FACE_OUTER_BOUND ( 'NONE', #13838, .T. ) ;
#25027 = AXIS2_PLACEMENT_3D ( 'NONE', #48487, #38633, #60036 ) ;
#25028 = DIRECTION ( 'NONE',  ( -1.156482317317870344E-15, -1.000000000000000000, 0.000000000000000000 ) ) ;
#25029 = UNCERTAINTY_MEASURE_WITH_UNIT (LENGTH_MEASURE( 1.000000000000000082E-05 ), #51102, 'distance_accuracy_value', 'NONE');
#25030 = CARTESIAN_POINT ( 'NONE',  ( -72.14292637653379359, 5.598654528085800663, -7.705886871421367523 ) ) ;
#25031 =( GEOMETRIC_REPRESENTATION_CONTEXT ( 3 ) GLOBAL_UNCERTAINTY_ASSIGNED_CONTEXT ( ( #21292 ) ) GLOBAL_UNIT_ASSIGNED_CONTEXT ( ( #67821, #47088, #20308 ) ) REPRESENTATION_CONTEXT ( 'NONE', 'WORKASPACE' ) );
#25032 = ORIENTED_EDGE ( 'NONE', *, *, #37471, .T. ) ;
#25033 = CARTESIAN_POINT ( 'NONE',  ( -139.3429263765337964, -9.058813317711329915, 2.943386871421371787 ) ) ;
#25034 =( NAMED_UNIT ( * ) PLANE_ANGLE_UNIT ( ) SI_UNIT ( $, .RADIAN. ) );
#25035 = CARTESIAN_POINT ( 'NONE',  ( 9.827790563157511022E-16, 87.30187232391182306, -8.025000000000000355 ) ) ;
#25036 = CARTESIAN_POINT ( 'NONE',  ( -156.1450000000000102, -4.716976649647092401, 6.492361379858946790 ) ) ;
#25037 = COLOUR_RGB ( '', 0.40784314, 0.44705882, 0.49803922) ;
#25038 = EDGE_CURVE ( 'NONE', #54990, #39699, #19266, .T. ) ;
#25039 = CLOSED_SHELL ( 'NONE', ( #60689, #60835, #16156, #25973, #24291, #9984, #58022, #10200, #37057, #55802, #52944, #44702, #46696, #9881, #15527, #42393, #39605, #55918, #6653, #66000, #63293, #9879, #58451, #53450, #17652 ) ) ;
#25040 = SURFACE_STYLE_FILL_AREA ( #25715 ) ;
#25041 = CARTESIAN_POINT ( 'NONE',  ( -133.0429263765338135, -9.058813317711329915, -2.943386871421370898 ) ) ;
#25042 = VERTEX_POINT ( 'NONE', #626 ) ;
#25043 = FACE_OUTER_BOUND ( 'NONE', #31987, .T. ) ;
#25044 = EDGE_LOOP ( 'NONE', ( #23562, #41448, #16459 ) ) ;
#25045 = STYLED_ITEM ( 'NONE', ( #39907 ), #35828 ) ;
#25046 = CARTESIAN_POINT ( 'NONE',  ( 21.00000000000001776, 42.00000000000000000, -29.68999999999999417 ) ) ;
#25047 = UNCERTAINTY_MEASURE_WITH_UNIT (LENGTH_MEASURE( 1.000000000000000082E-05 ), #12026, 'distance_accuracy_value', 'NONE');
#25048 = LINE ( 'NONE', #46559, #31503 ) ;
#25049 = DIRECTION ( 'NONE',  ( 0.000000000000000000, 1.000000000000000000, 0.000000000000000000 ) ) ;
#25050 = COLOUR_RGB ( '', 0.31764706, 0.68627451, 0.89019608) ;
#25051 = ORIENTED_EDGE ( 'NONE', *, *, #49039, .T. ) ;
#25052 = CARTESIAN_POINT ( 'NONE',  ( -161.9050000000000011, 2.607480562269069324, -8.024999999999993250 ) ) ;
#25053 = AXIS2_PLACEMENT_3D ( 'NONE', #9898, #4583, #46523 ) ;
#25054 = ORIENTED_EDGE ( 'NONE', *, *, #24779, .F. ) ;
#25055 =( GEOMETRIC_REPRESENTATION_CONTEXT ( 3 ) GLOBAL_UNCERTAINTY_ASSIGNED_CONTEXT ( ( #41084 ) ) GLOBAL_UNIT_ASSIGNED_CONTEXT ( ( #786, #22331, #49769 ) ) REPRESENTATION_CONTEXT ( 'NONE', 'WORKASPACE' ) );
#25056 = CARTESIAN_POINT ( 'NONE',  ( -47.51430879217793546, 5.598654528085803328, -7.705886871421366635 ) ) ;
#25057 = DIRECTION ( 'NONE',  ( 0.000000000000000000, -6.938893903907222067E-15, 1.000000000000000000 ) ) ;
#25058 = ORIENTED_EDGE ( 'NONE', *, *, #38497, .T. ) ;
#25059 = LINE ( 'NONE', #14169, #3340 ) ;
#25060 = EDGE_CURVE ( 'NONE', #42967, #5418, #7039, .T. ) ;
#25061 = CARTESIAN_POINT ( 'NONE',  ( -9.058813317711337021, 113.0449999999999875, -2.943386871421374895 ) ) ;
#25062 = STYLED_ITEM ( 'NONE', ( #60803 ), #26314 ) ;
#25063 = EDGE_LOOP ( 'NONE', ( #62771, #61576, #57761, #40779 ) ) ;
#25064 = DIRECTION ( 'NONE',  ( 0.000000000000000000, -0.000000000000000000, -1.000000000000000000 ) ) ;
#25065 = CARTESIAN_POINT ( 'NONE',  ( -71.50000000000000000, 35.92875272052971525, 10.00000000000000000 ) ) ;
#25066 = CARTESIAN_POINT ( 'NONE',  ( -78.35499999999997556, -4.716976649647093289, -6.492361379858945902 ) ) ;
#25067 = DIRECTION ( 'NONE',  ( 0.000000000000000000, 1.000000000000000000, 0.000000000000000000 ) ) ;
#25068 = EDGE_LOOP ( 'NONE', ( #68506, #32317, #53923, #65981 ) ) ;
#25069 = CARTESIAN_POINT ( 'NONE',  ( -5.598654528085806881, 140.8549999999999898, -7.705886871421374629 ) ) ;
#25070 = UNCERTAINTY_MEASURE_WITH_UNIT (LENGTH_MEASURE( 1.000000000000000082E-05 ), #10529, 'distance_accuracy_value', 'NONE');
#25071 = DIRECTION ( 'NONE',  ( -0.000000000000000000, 1.000000000000000000, 0.000000000000000000 ) ) ;
#25072 = FACE_OUTER_BOUND ( 'NONE', #12668, .T. ) ;
#25073 = CARTESIAN_POINT ( 'NONE',  ( 19.98523465219084017, 114.9999999999999574, 10.47102667436386625 ) ) ;
#25074 = DIRECTION ( 'NONE',  ( 1.000000000000000000, 0.000000000000000000, 0.000000000000000000 ) ) ;
#25075 = SURFACE_STYLE_USAGE ( .BOTH. , #29660 ) ;
#25076 = ORIENTED_EDGE ( 'NONE', *, *, #51542, .T. ) ;
#25077 = CIRCLE ( 'NONE', #16119, 0.2500000000000002220 ) ;
#25078 = VECTOR ( 'NONE', #48036, 1000.000000000000000 ) ;
#25079 = FILL_AREA_STYLE ('',( #40944 ) ) ;
#25080 = DIRECTION ( 'NONE',  ( -1.000000000000000000, -0.000000000000000000, -0.000000000000000000 ) ) ;
#25081 = CARTESIAN_POINT ( 'NONE',  ( -178.5549999999999784, 0.000000000000000000, 8.024999999999991473 ) ) ;
#25082 = ORIENTED_EDGE ( 'NONE', *, *, #11006, .F. ) ;
#25083 = CARTESIAN_POINT ( 'NONE',  ( 8.440061761865212731, 111.3586140163384215, 2.039925464057781745 ) ) ;
#25084 = PRESENTATION_LAYER_ASSIGNMENT (  '', '', ( #11563 ) ) ;
#25085 = CARTESIAN_POINT ( 'NONE',  ( 6.239160159721271803, 2.500000000000000000, -3.193457606803198789 ) ) ;
#25086 = DIRECTION ( 'NONE',  ( 0.000000000000000000, 0.000000000000000000, -1.000000000000000000 ) ) ;
#25087 = ORIENTED_EDGE ( 'NONE', *, *, #6111, .T. ) ;
#25088 = DIRECTION ( 'NONE',  ( 0.000000000000000000, 1.000000000000000000, 0.000000000000000000 ) ) ;
#25089 = ORIENTED_EDGE ( 'NONE', *, *, #2230, .F. ) ;
#25090 = SURFACE_STYLE_USAGE ( .BOTH. , #18769 ) ;
#25091 = CARTESIAN_POINT ( 'NONE',  ( -105.8050000000000068, -8.437984349512085203, 5.166775262442717831E-16 ) ) ;
#25093 = VERTEX_POINT ( 'NONE', #274 ) ;
#25092 = CIRCLE ( 'NONE', #65604, 0.4999999999999991118 ) ;
#25094 = PLANE ( 'NONE',  #16010 ) ;
#25095 = EDGE_CURVE ( 'NONE', #17136, #64475, #21444, .T. ) ;
#25096 = CARTESIAN_POINT ( 'NONE',  ( 0.000000000000000000, 0.000000000000000000, 0.000000000000000000 ) ) ;
#25097 = CARTESIAN_POINT ( 'NONE',  ( -143.9070736234661751, -3.094860106618429807, 9.524999999999991473 ) ) ;
#25098 = VECTOR ( 'NONE', #24992, 1000.000000000000000 ) ;
#25099 = CARTESIAN_POINT ( 'NONE',  ( 27.00000000000001776, 15.00000000000000000, -35.50000000000000000 ) ) ;
#25100 = CARTESIAN_POINT ( 'NONE',  ( -74.45707362346617231, -9.058813317711329915, 2.943386871421371787 ) ) ;
#25101 = DIRECTION ( 'NONE',  ( 0.000000000000000000, 1.000000000000000000, 0.000000000000000000 ) ) ;
#25102 = EDGE_LOOP ( 'NONE', ( #59275, #58933, #42241 ) ) ;
#25103 = CARTESIAN_POINT ( 'NONE',  ( 0.000000000000000000, 0.000000000000000000, 1.000000000000000000 ) ) ;
#25104 = LINE ( 'NONE', #62714, #66183 ) ;
#25105 = PRESENTATION_LAYER_ASSIGNMENT (  '', '', ( #23945 ) ) ;
#25106 = CARTESIAN_POINT ( 'NONE',  ( -125.9049999999999869, 2.607480562269068880, -8.024999999999993250 ) ) ;
#25107 = ADVANCED_FACE ( 'NONE', ( #36980 ), #12612, .T. ) ;
#25108 = CARTESIAN_POINT ( 'NONE',  ( 10.01517768586949231, 111.6949999999999932, 1.839758294383810543E-15 ) ) ;
#25109 = CARTESIAN_POINT ( 'NONE',  ( -130.3449999999999989, 7.632228543268599452, -2.479861379858951942 ) ) ;
#25110 = EDGE_CURVE ( 'NONE', #18094, #62990, #28235, .T. ) ;
#25111 = ORIENTED_EDGE ( 'NONE', *, *, #2415, .F. ) ;
#25112 = AXIS2_PLACEMENT_3D ( 'NONE', #59691, #16136, #37260 ) ;
#25113 = DIRECTION ( 'NONE',  ( -0.000000000000000000, -0.000000000000000000, -1.000000000000000000 ) ) ;
#25114 = STYLED_ITEM ( 'NONE', ( #6875 ), #9057 ) ;
#25115 = EDGE_CURVE ( 'NONE', #62949, #4733, #39737, .T. ) ;
#25116 = CARTESIAN_POINT ( 'NONE',  ( 8.000000000000035527, 5.000000000000000000, -77.00402776293825013 ) ) ;
#25117 = CARTESIAN_POINT ( 'NONE',  ( -172.0429263765338135, -9.058813317711329915, -2.943386871421370898 ) ) ;
#25118 = ADVANCED_FACE ( 'NONE', ( #28788 ), #8039, .F. ) ;
#25119 = AXIS2_PLACEMENT_3D ( 'NONE', #30675, #3207, #8559 ) ;
#25120 = CARTESIAN_POINT ( 'NONE',  ( -45.00000000000463984, 9.678589032125119118, -3.510839860134217005 ) ) ;
#25121 = MECHANICAL_DESIGN_GEOMETRIC_PRESENTATION_REPRESENTATION (  '', ( #16167 ), #38733 ) ;
#25122 = AXIS2_PLACEMENT_3D ( 'NONE', #46108, #55589, #28839 ) ;
#25123 = CARTESIAN_POINT ( 'NONE',  ( -26.79538245034556354, -7.499999999999999112, 0.000000000000000000 ) ) ;
#25124 = CARTESIAN_POINT ( 'NONE',  ( 7.766391886667110889, 0.5482146608018589884, 0.7663918866669823249 ) ) ;
#25125 = ORIENTED_EDGE ( 'NONE', *, *, #25242, .F. ) ;
#25126 = CARTESIAN_POINT ( 'NONE',  ( -83.69292637653379074, 10.01517768586948698, -1.839758294383808571E-15 ) ) ;
#25127 = ITEM_DEFINED_TRANSFORMATION ( 'NONE', 'NONE', #16955,  #42840 ) ;
#25128 = CARTESIAN_POINT ( 'NONE',  ( 22.75000000000000711, 36.75000000000000000, 3.750000000000000000 ) ) ;
#25129 = CARTESIAN_POINT ( 'NONE',  ( -58.75000000000000000, -4.000000000000000000, 11.89999999999999680 ) ) ;
#25130 = CIRCLE ( 'NONE', #2585, 0.5000000000000004441 ) ;
#25131 = DIRECTION ( 'NONE',  ( 0.000000000000000000, 0.000000000000000000, 1.000000000000000000 ) ) ;
#25132 = CARTESIAN_POINT ( 'NONE',  ( 4.716976649647096842, 122.8570736234661638, 6.492361379858953896 ) ) ;
#25133 = CARTESIAN_POINT ( 'NONE',  ( -162.8929263765338078, -8.102448949553174629, -5.886773742842741797 ) ) ;
#25134 = PRESENTATION_STYLE_ASSIGNMENT (( #57131 ) ) ;
#25135 = AXIS2_PLACEMENT_3D ( 'NONE', #323, #47606, #41965 ) ;
#25136 = ORIENTED_EDGE ( 'NONE', *, *, #39007, .T. ) ;
#25137 =( NAMED_UNIT ( * ) PLANE_ANGLE_UNIT ( ) SI_UNIT ( $, .RADIAN. ) );
#25138 = EDGE_LOOP ( 'NONE', ( #50063, #13191, #15225, #14767 ) ) ;
#25139 = DIRECTION ( 'NONE',  ( 0.000000000000000000, 0.000000000000000000, -1.000000000000000000 ) ) ;
#25140 = STYLED_ITEM ( 'NONE', ( #42511 ), #36609 ) ;
#25141 =( BOUNDED_CURVE ( )  B_SPLINE_CURVE ( 2, ( #43088, #16341, #37814, #32453, #25185, #15008, #40700, #62800, #3688, #46702, #67757 ),
 .UNSPECIFIED., .F., .F. ) 
 B_SPLINE_CURVE_WITH_KNOTS ( ( 3, 2, 2, 2, 2, 3 ),
 ( 0.8913043478260869179, 0.8934782608695651662, 0.8956521739130435256, 0.8978260869565217739, 0.9000000000000000222, 0.9021739130434782705 ),
 .UNSPECIFIED. ) 
 CURVE ( )  GEOMETRIC_REPRESENTATION_ITEM ( )  RATIONAL_B_SPLINE_CURVE ( ( 1.000000000000000000, 0.9510565162951535312, 1.000000000000000000, 0.9510565162951535312, 1.000000000000000000, 0.9510565162951535312, 1.000000000000000000, 0.9510565162951535312, 1.000000000000000000, 0.9510565162951535312, 1.000000000000000000 ) ) 
 REPRESENTATION_ITEM ( '' )  );
#25142 = SURFACE_STYLE_FILL_AREA ( #51524 ) ;
#25143 = CARTESIAN_POINT ( 'NONE',  ( 6.826472737025119919, 132.0070736234661695, 4.959722759717908325 ) ) ;
#25144 = PRESENTATION_STYLE_ASSIGNMENT (( #30752 ) ) ;
#25145 = ORIENTED_EDGE ( 'NONE', *, *, #17291, .F. ) ;
#25146 = CARTESIAN_POINT ( 'NONE',  ( -106.1049999999999756, -6.826472737025113702, 4.959722759717902107 ) ) ;
#25147 =( GEOMETRIC_REPRESENTATION_CONTEXT ( 3 ) GLOBAL_UNCERTAINTY_ASSIGNED_CONTEXT ( ( #29992 ) ) GLOBAL_UNIT_ASSIGNED_CONTEXT ( ( #37368, #15884, #41579 ) ) REPRESENTATION_CONTEXT ( 'NONE', 'WORKASPACE' ) );
#25148 =( NAMED_UNIT ( * ) SI_UNIT ( $, .STERADIAN. ) SOLID_ANGLE_UNIT ( ) );
#25149 = ORIENTED_EDGE ( 'NONE', *, *, #33983, .F. ) ;
#25150 = CARTESIAN_POINT ( 'NONE',  ( -37.17007440505049942, -12.37226643102196633, 1.277129481866865035 ) ) ;
#25151 = DIRECTION ( 'NONE',  ( 1.000000000000000000, 0.000000000000000000, 0.000000000000000000 ) ) ;
#25152 =( NAMED_UNIT ( * ) PLANE_ANGLE_UNIT ( ) SI_UNIT ( $, .RADIAN. ) );
#25153 = SURFACE_STYLE_USAGE ( .BOTH. , #30398 ) ;
#25154 = ORIENTED_EDGE ( 'NONE', *, *, #35524, .F. ) ;
#25155 =( GEOMETRIC_REPRESENTATION_CONTEXT ( 3 ) GLOBAL_UNCERTAINTY_ASSIGNED_CONTEXT ( ( #43406 ) ) GLOBAL_UNIT_ASSIGNED_CONTEXT ( ( #55608, #12323, #9857 ) ) REPRESENTATION_CONTEXT ( 'NONE', 'WORKASPACE' ) );
#25156 =( NAMED_UNIT ( * ) PLANE_ANGLE_UNIT ( ) SI_UNIT ( $, .RADIAN. ) );
#25157 = CARTESIAN_POINT ( 'NONE',  ( -81.74499999999999034, 4.716976649647094177, 6.492361379858945902 ) ) ;
#25158 = EDGE_LOOP ( 'NONE', ( #33782, #7077, #58719, #47331, #34480, #26796, #40521, #34781, #37795, #66085 ) ) ;
#25159 = CYLINDRICAL_SURFACE ( 'NONE', #67604, 3.000000000000000444 ) ;
#25160 = VECTOR ( 'NONE', #52613, 1000.000000000000000 ) ;
#25161 = DIRECTION ( 'NONE',  ( 0.000000000000000000, -0.3420201433256630508, 0.9396926207859105373 ) ) ;
#25162 = ORIENTED_EDGE ( 'NONE', *, *, #22584, .T. ) ;
#25163 = LINE ( 'NONE', #15347, #11123 ) ;
#25164 = SURFACE_STYLE_FILL_AREA ( #56839 ) ;
#25166 = CARTESIAN_POINT ( 'NONE',  ( -6.413663052920317575, -2.891209729714697030, 1.212104147520903391E-15 ) ) ;
#25165 = AXIS2_PLACEMENT_3D ( 'NONE', #16477, #37941, #59315 ) ;
#25167 = ORIENTED_EDGE ( 'NONE', *, *, #40354, .F. ) ;
#25168 = CARTESIAN_POINT ( 'NONE',  ( -154.9429263765338192, 0.000000000000000000, 9.524999999999991473 ) ) ;
#25170 = ORIENTED_EDGE ( 'NONE', *, *, #54583, .F. ) ;
#25169 = EDGE_CURVE ( 'NONE', #68919, #61482, #24898, .T. ) ;
#25171 = DIRECTION ( 'NONE',  ( 1.000000000000000000, 0.000000000000000000, 0.000000000000000000 ) ) ;
#25172 = DIRECTION ( 'NONE',  ( 0.000000000000000000, 0.000000000000000000, 1.000000000000000000 ) ) ;
#25173 = FACE_OUTER_BOUND ( 'NONE', #19797, .T. ) ;
#25174 = CIRCLE ( 'NONE', #65638, 18.53939201416945082 ) ;
#25175 = CARTESIAN_POINT ( 'NONE',  ( -168.2070736234661297, 3.094860106618433360, 9.524999999999991473 ) ) ;
#25176 = CARTESIAN_POINT ( 'NONE',  ( -1.166476076187854022E-15, 110.9449999999999932, 9.525000000000000355 ) ) ;
#25177 = EDGE_CURVE ( 'NONE', #28083, #58801, #43989, .T. ) ;
#25178 = CARTESIAN_POINT ( 'NONE',  ( -103.8570736234661780, -5.598654528085803328, -7.705886871421366635 ) ) ;
#25179 = LINE ( 'NONE', #9010, #36373 ) ;
#25180 = VERTEX_POINT ( 'NONE', #18250 ) ;
#25181 = FACE_OUTER_BOUND ( 'NONE', #23069, .T. ) ;
#25182 = EDGE_CURVE ( 'NONE', #1374, #3091, #8042, .T. ) ;
#25183 = CARTESIAN_POINT ( 'NONE',  ( -106.4070736234671131, 3.094860106602697503, -9.525000000011422330 ) ) ;
#25185 = CARTESIAN_POINT ( 'NONE',  ( -61.34292637653379643, -9.058813317711329915, 2.943386871421371787 ) ) ;
#25184 = DIRECTION ( 'NONE',  ( 1.000000000000000000, 0.000000000000000000, 0.000000000000000000 ) ) ;
#25186 =( GEOMETRIC_REPRESENTATION_CONTEXT ( 3 ) GLOBAL_UNCERTAINTY_ASSIGNED_CONTEXT ( ( #29201 ) ) GLOBAL_UNIT_ASSIGNED_CONTEXT ( ( #10176, #47871, #20732 ) ) REPRESENTATION_CONTEXT ( 'NONE', 'WORKASPACE' ) );
#25187 = CARTESIAN_POINT ( 'NONE',  ( -147.2050000000000125, -2.607480562269071545, -8.024999999999991473 ) ) ;
#25188 = CARTESIAN_POINT ( 'NONE',  ( -147.7429263765338021, -5.598654528085803328, -7.705886871421366635 ) ) ;
#25189 = CARTESIAN_POINT ( 'NONE',  ( -155.0949999999999989, -2.607480562269071545, -8.024999999999991473 ) ) ;
#25190 = ADVANCED_FACE ( 'NONE', ( #65404 ), #28072, .T. ) ;
#25191 = CARTESIAN_POINT ( 'NONE',  ( -151.7949999999999591, 2.607480562269069324, -8.024999999999993250 ) ) ;
#25192 = ORIENTED_EDGE ( 'NONE', *, *, #64981, .T. ) ;
#25193 = TOROIDAL_SURFACE ( 'NONE', #61088, 0.5000000000000000000, 0.2500000000000000000 ) ;
#25194 = CARTESIAN_POINT ( 'NONE',  ( 30.25000000000000711, 18.74999999999997868, -3.750000000000000000 ) ) ;
#25195 = STYLED_ITEM ( 'NONE', ( #5077 ), #413 ) ;
#25196 = FILL_AREA_STYLE_COLOUR ( '', #32325 ) ;
#25197 = EDGE_CURVE ( 'NONE', #40324, #61550, #34425, .T. ) ;
#25198 = DIRECTION ( 'NONE',  ( 0.000000000000000000, 0.000000000000000000, 1.000000000000000000 ) ) ;
#25199 = COLOUR_RGB ( '', 0.08235294, 0.09019608, 0.10196078) ;
#25200 = CARTESIAN_POINT ( 'NONE',  ( -60.20499999999998408, -2.607480562269071545, -8.024999999999991473 ) ) ;
#25201 = CIRCLE ( 'NONE', #15099, 1.000000000000000888 ) ;
#25202 = CARTESIAN_POINT ( 'NONE',  ( -62.24499999999998323, -4.716976649647093289, -6.492361379858945902 ) ) ;
#25203 = CARTESIAN_POINT ( 'NONE',  ( -5.598654528085806881, 158.8549999999999898, -7.705886871421374629 ) ) ;
#25204 = CARTESIAN_POINT ( 'NONE',  ( 3.000000000000002665, 5.569094604152796002, 2.026984667724101463 ) ) ;
#25205 =( LENGTH_UNIT ( ) NAMED_UNIT ( * ) SI_UNIT ( .MILLI., .METRE. ) );
#25206 = DIRECTION ( 'NONE',  ( -1.091587353480403297E-16, 1.000000000000000000, -1.942918990250874836E-16 ) ) ;
#25207 = MECHANICAL_DESIGN_GEOMETRIC_PRESENTATION_REPRESENTATION (  '', ( #37619 ), #12849 ) ;
#25208 = DIRECTION ( 'NONE',  ( 0.000000000000000000, 1.000000000000000000, 0.000000000000000000 ) ) ;
#25209 = CARTESIAN_POINT ( 'NONE',  ( -32.62570226935650197, -8.499999999999996447, 8.000000000000000000 ) ) ;
#25210 = AXIS2_PLACEMENT_3D ( 'NONE', #26793, #65499, #28175 ) ;
#25211 = CARTESIAN_POINT ( 'NONE',  ( 45.00000000000000000, -1.469576158976824618E-14, 10.00000000000000000 ) ) ;
#25212 = FILL_AREA_STYLE ('',( #68838 ) ) ;
#25213 = LINE ( 'NONE', #46733, #61145 ) ;
#25214 = LINE ( 'NONE', #35775, #54188 ) ;
#25215 = VERTEX_POINT ( 'NONE', #44345 ) ;
#25216 = EDGE_LOOP ( 'NONE', ( #27960, #17513, #57610, #34914 ) ) ;
#25217 = VECTOR ( 'NONE', #49072, 1000.000000000000000 ) ;
#25218 = FACE_OUTER_BOUND ( 'NONE', #68017, .T. ) ;
#25219 = LINE ( 'NONE', #31167, #65265 ) ;
#25220 = ADVANCED_FACE ( 'NONE', ( #65746 ), #39054, .T. ) ;
#25221 = CIRCLE ( 'NONE', #1625, 5.000000000000004441 ) ;
#25222 = FILL_AREA_STYLE ('',( #3730 ) ) ;
#25223 = ORIENTED_EDGE ( 'NONE', *, *, #65758, .T. ) ;
#25224 = EDGE_LOOP ( 'NONE', ( #59994, #64341, #17951 ) ) ;
#25225 = CARTESIAN_POINT ( 'NONE',  ( -21.02379604162863913, 154.9999999999999716, 10.50000000000000000 ) ) ;
#25226 = LINE ( 'NONE', #41097, #14034 ) ;
#25227 = ORIENTED_EDGE ( 'NONE', *, *, #57101, .F. ) ;
#25228 = CARTESIAN_POINT ( 'NONE',  ( 5.598654528085805993, 115.3549999999999898, 7.705886871421374629 ) ) ;
#25229 = DIRECTION ( 'NONE',  ( 1.000000000000000000, 0.000000000000000000, -1.300977106640434891E-16 ) ) ;
#25230 = DIRECTION ( 'NONE',  ( 0.000000000000000000, -1.000000000000000000, 0.000000000000000000 ) ) ;
#25231 = VECTOR ( 'NONE', #50443, 1000.000000000000000 ) ;
#25232 =( NAMED_UNIT ( * ) SI_UNIT ( $, .STERADIAN. ) SOLID_ANGLE_UNIT ( ) );
#25233 = CARTESIAN_POINT ( 'NONE',  ( -113.5449999999999875, -7.632228543268600340, -2.479861379858950166 ) ) ;
#25234 = ORIENTED_EDGE ( 'NONE', *, *, #55670, .T. ) ;
#25235 =( BOUNDED_SURFACE ( )  B_SPLINE_SURFACE ( 3, 2, ( 
 ( #21934, #65524, #37813 ),
 ( #53588, #12384, #64496 ),
 ( #39171, #32825, #6424 ),
 ( #54265, #48702, #43445 ),
 ( #54942, #44121, #5372 ),
 ( #6087, #17373, #27519 ),
 ( #49045, #736, #60249 ),
 ( #12045, #65167, #21574 ),
 ( #17012, #16340, #40 ),
 ( #59895, #11713, #59185 ) ),
 .UNSPECIFIED., .F., .F., .F. ) 
 B_SPLINE_SURFACE_WITH_KNOTS ( ( 4, 2, 2, 2, 4 ),
 ( 3, 3 ),
 ( 0.01935955400260480630, 0.02095281869284682311, 0.02254608338308883991, 0.02413934807333086019, 0.02573261276357287700 ),
 ( 0.000000000000000000, 1.000000000000000000 ),
 .UNSPECIFIED. ) 
 GEOMETRIC_REPRESENTATION_ITEM ( )  RATIONAL_B_SPLINE_SURFACE ( (
 ( 1.000000000000000000, 0.8093049424017613180, 1.000000000000000000),
 ( 1.000000000000000000, 0.8049424280649992713, 1.000000000000000000),
 ( 1.000000000000000000, 0.8014042547541196937, 1.000000000000000000),
 ( 1.000000000000000000, 0.7967637600457907476, 1.000000000000000000),
 ( 1.000000000000000000, 0.7956476677631215688, 1.000000000000000000),
 ( 1.000000000000000000, 0.7960422929644409562, 1.000000000000000000),
 ( 1.000000000000000000, 0.7975419603936064750, 1.000000000000000000),
 ( 1.000000000000000000, 0.8027988638271628119, 1.000000000000000000),
 ( 1.000000000000000000, 0.8065519299663326258, 1.000000000000000000),
 ( 1.000000000000000000, 0.8111477107414843957, 1.000000000000000000) ) ) 
 REPRESENTATION_ITEM ( '' )  SURFACE ( )  );
#25236 = CARTESIAN_POINT ( 'NONE',  ( 6.000000000000017764, 43.00000000000000000, -35.50000000000000000 ) ) ;
#25237 = DIRECTION ( 'NONE',  ( 0.000000000000000000, 0.000000000000000000, 1.000000000000000000 ) ) ;
#25238 = FILL_AREA_STYLE ('',( #8387 ) ) ;
#25239 =( GEOMETRIC_REPRESENTATION_CONTEXT ( 3 ) GLOBAL_UNCERTAINTY_ASSIGNED_CONTEXT ( ( #20117 ) ) GLOBAL_UNIT_ASSIGNED_CONTEXT ( ( #9395, #58253, #19211 ) ) REPRESENTATION_CONTEXT ( 'NONE', 'WORKASPACE' ) );
#25240 = ORIENTED_EDGE ( 'NONE', *, *, #21203, .T. ) ;
#25241 = CARTESIAN_POINT ( 'NONE',  ( -2.607480562269075097, 145.2929263765338135, 8.025000000000000355 ) ) ;
#25242 = EDGE_CURVE ( 'NONE', #58823, #27375, #14014, .T. ) ;
#25243 = CARTESIAN_POINT ( 'NONE',  ( 6.887213563469345878, 2.329718218673042962, 6.070996185493596542 ) ) ;
#25244 = EDGE_CURVE ( 'NONE', #60543, #44642, #3525, .T. ) ;
#25245 = ORIENTED_EDGE ( 'NONE', *, *, #8981, .T. ) ;
#25246 = FILL_AREA_STYLE_COLOUR ( '', #23986 ) ;
#25247 = EDGE_LOOP ( 'NONE', ( #59833, #15959, #50614 ) ) ;
#25248 = CARTESIAN_POINT ( 'NONE',  ( 29.00000000000002842, 42.00000000000000000, 80.00402776293826435 ) ) ;
#25249 = LINE ( 'NONE', #57614, #40284 ) ;
#25250 = PLANE ( 'NONE',  #64467 ) ;
#25251 = CARTESIAN_POINT ( 'NONE',  ( 4.500000000000002665, 24.74999999999998579, 4.000000000000000000 ) ) ;
#25252 = CARTESIAN_POINT ( 'NONE',  ( -126.0550000000000068, -9.827790563157499189E-16, -8.024999999999991473 ) ) ;
#25253 = DIRECTION ( 'NONE',  ( -1.000000000000000000, 1.189524669241239115E-16, 0.000000000000000000 ) ) ;
#25254 = FILL_AREA_STYLE ('',( #35120 ) ) ;
#25255 = EDGE_CURVE ( 'NONE', #28559, #10363, #47099, .T. ) ;
#25256 = TOROIDAL_SURFACE ( 'NONE', #15213, 0.5000000000000000000, 0.2500000000000000000 ) ;
#25257 = AXIS2_PLACEMENT_3D ( 'NONE', #13162, #29704, #2570 ) ;
#25258 = CARTESIAN_POINT ( 'NONE',  ( -125.8429263765337964, 9.058813317711329915, -2.943386871421373119 ) ) ;
#25259 = DIRECTION ( 'NONE',  ( 1.000000000000000000, -0.000000000000000000, 0.000000000000000000 ) ) ;
#25260 = CARTESIAN_POINT ( 'NONE',  ( -60.00000000000000000, -2.024042244987997205E-14, -7.000000000000000000 ) ) ;
#25261 = ORIENTED_EDGE ( 'NONE', *, *, #58396, .T. ) ;
#25262 = ORIENTED_EDGE ( 'NONE', *, *, #60865, .F. ) ;
#25263 = CYLINDRICAL_SURFACE ( 'NONE', #5081, 0.5000000000000004441 ) ;
#25264 = CARTESIAN_POINT ( 'NONE',  ( -54.50000000000002132, -2.024042244987997205E-14, 12.00000000000000000 ) ) ;
#25265 = PRESENTATION_LAYER_ASSIGNMENT (  '', '', ( #17416 ) ) ;
#25266 = ORIENTED_EDGE ( 'NONE', *, *, #64319, .F. ) ;
#25267 = CARTESIAN_POINT ( 'NONE',  ( -181.2549999999999955, -4.716976649647092401, 6.492361379858946790 ) ) ;
#25268 = CARTESIAN_POINT ( 'NONE',  ( 44.00000000000000000, 19.24999999999998224, 3.750000000000000000 ) ) ;
#25269 = SURFACE_STYLE_FILL_AREA ( #57636 ) ;
#25270 = CARTESIAN_POINT ( 'NONE',  ( -179.3950000000000102, -6.826472737025115478, -4.959722759717899443 ) ) ;
#25271 = EDGE_CURVE ( 'NONE', #4737, #19853, #35118, .T. ) ;
#25272 = CIRCLE ( 'NONE', #41070, 0.5000000000000004441 ) ;
#25273 =( GEOMETRIC_REPRESENTATION_CONTEXT ( 3 ) GLOBAL_UNCERTAINTY_ASSIGNED_CONTEXT ( ( #1036 ) ) GLOBAL_UNIT_ASSIGNED_CONTEXT ( ( #23838, #24867, #66759 ) ) REPRESENTATION_CONTEXT ( 'NONE', 'WORKASPACE' ) );
#25274 = CARTESIAN_POINT ( 'NONE',  ( -176.5450000000000159, -7.632228543268600340, -2.479861379858950166 ) ) ;
#25275 = CARTESIAN_POINT ( 'NONE',  ( 40.96599324808799025, 108.0258340745533161, 3.573232801688252636 ) ) ;
#25276 = ORIENTED_EDGE ( 'NONE', *, *, #29472, .T. ) ;
#25277 = CARTESIAN_POINT ( 'NONE',  ( 9.250000000000003553, 25.24999999999998934, 3.750000000000000000 ) ) ;
#25278 = EDGE_CURVE ( 'NONE', #34471, #55705, #13656, .T. ) ;
#25279 =( NAMED_UNIT ( * ) PLANE_ANGLE_UNIT ( ) SI_UNIT ( $, .RADIAN. ) );
#25280 = CARTESIAN_POINT ( 'NONE',  ( -91.55499999999997840, 0.000000000000000000, 8.024999999999991473 ) ) ;
#25281 = CARTESIAN_POINT ( 'NONE',  ( 9.527321842919894479, 154.4999999999999716, 0.3821556790526681180 ) ) ;
#25282 = CARTESIAN_POINT ( 'NONE',  ( -60.00000000000000000, -2.024042244987997205E-14, 6.999999999999999112 ) ) ;
#25283 = CARTESIAN_POINT ( 'NONE',  ( -88.79499999999998749, 2.607480562269069324, -8.024999999999993250 ) ) ;
#25284 = CARTESIAN_POINT ( 'NONE',  ( -10.01517768586949231, 126.3049999999999784, -6.132527647946036459E-16 ) ) ;
#25285 = CARTESIAN_POINT ( 'NONE',  ( -72.29499999999998749, -2.607480562269069768, 8.024999999999991473 ) ) ;
#25286 = ADVANCED_BREP_SHAPE_REPRESENTATION ( '', ( #50051, #42840 ), #1086 ) ;
#25287 = DIRECTION ( 'NONE',  ( 0.000000000000000000, 0.000000000000000000, 1.000000000000000000 ) ) ;
#25288 = CARTESIAN_POINT ( 'NONE',  ( -70.75000000000000000, -4.000000000000000000, 19.00000000000000000 ) ) ;
#25289 = COLOUR_RGB ( '', 0.40784314, 0.44705882, 0.49803922) ;
#25290 = CARTESIAN_POINT ( 'NONE',  ( -40.99999999999998579, 107.7459666924148394, 3.000000000000000000 ) ) ;
#25291 = FILL_AREA_STYLE_COLOUR ( '', #39427 ) ;
#25292 = ORIENTED_EDGE ( 'NONE', *, *, #27840, .T. ) ;
#25293 = CARTESIAN_POINT ( 'NONE',  ( -104.0929263765338106, 3.094860106618433360, 9.524999999999991473 ) ) ;
#25294 = VECTOR ( 'NONE', #46273, 1000.000000000000000 ) ;
#25295 = CARTESIAN_POINT ( 'NONE',  ( -130.9449999999999648, -9.827790563157499189E-16, -8.024999999999991473 ) ) ;
#25296 = CARTESIAN_POINT ( 'NONE',  ( -4.041451884327378785, 1.417096231345241542, 7.000000000000000000 ) ) ;
#25297 = SURFACE_STYLE_FILL_AREA ( #3813 ) ;
#25298 = DIRECTION ( 'NONE',  ( 0.000000000000000000, 0.000000000000000000, 1.000000000000000000 ) ) ;
#25299 = DIRECTION ( 'NONE',  ( -0.6216216216216174928, 0.7833176619561892373, 0.000000000000000000 ) ) ;
#25300 = ORIENTED_EDGE ( 'NONE', *, *, #54561, .F. ) ;
#25301 = ORIENTED_EDGE ( 'NONE', *, *, #63216, .T. ) ;
#25302 = CARTESIAN_POINT ( 'NONE',  ( -174.8070736234661524, 10.01517768586948698, -1.839758294383808966E-15 ) ) ;
#25303 = ADVANCED_FACE ( 'NONE', ( #3763 ), #57621, .T. ) ;
#25304 = APPLICATION_CONTEXT ( 'automotive_design' ) ;
#25305 = AXIS2_PLACEMENT_3D ( 'NONE', #60043, #21720, #21360 ) ;
#25306 = DIRECTION ( 'NONE',  ( 1.000000000000000000, 0.000000000000000000, -0.000000000000000000 ) ) ;
#25307 = DIRECTION ( 'NONE',  ( 0.000000000000000000, 0.000000000000000000, 1.000000000000000000 ) ) ;
#25308 =( LENGTH_UNIT ( ) NAMED_UNIT ( * ) SI_UNIT ( .MILLI., .METRE. ) );
#25309 = CARTESIAN_POINT ( 'NONE',  ( -76.75000000000000000, 4.336808689942018722E-16, 7.000000000000001776 ) ) ;
#25310 = ORIENTED_EDGE ( 'NONE', *, *, #68859, .F. ) ;
#25311 = CARTESIAN_POINT ( 'NONE',  ( -119.0049999999999812, 6.826472737025115478, 4.959722759717899443 ) ) ;
#25312 = EDGE_LOOP ( 'NONE', ( #1322, #15486, #23967 ) ) ;
#25313 = CARTESIAN_POINT ( 'NONE',  ( 0.000000000000000000, 115.4999999999999574, 0.000000000000000000 ) ) ;
#25314 = CARTESIAN_POINT ( 'NONE',  ( -126.9570736234661723, 9.058813317711329915, -2.943386871421373119 ) ) ;
#25315 = ORIENTED_EDGE ( 'NONE', *, *, #29632, .T. ) ;
#25316 = ORIENTED_EDGE ( 'NONE', *, *, #24694, .F. ) ;
#25317 = AXIS2_PLACEMENT_3D ( 'NONE', #8295, #68775, #57510 ) ;
#25318 = AXIS2_PLACEMENT_3D ( 'NONE', #37606, #5179, #6550 ) ;
#25319 = LINE ( 'NONE', #52083, #9657 ) ;
#25320 = CARTESIAN_POINT ( 'NONE',  ( -3.094860106618432471, 151.5949999999999989, -9.525000000000000355 ) ) ;
#25321 = DIRECTION ( 'NONE',  ( 1.000000000000000000, 0.000000000000000000, 0.000000000000000000 ) ) ;
#25322 = EDGE_LOOP ( 'NONE', ( #63022, #7701, #17141, #32102 ) ) ;
#25323 = EDGE_CURVE ( 'NONE', #25898, #33970, #36559, .T. ) ;
#25324 = CARTESIAN_POINT ( 'NONE',  ( 8.102448949553179958, 148.5049999999999955, 5.886773742842750679 ) ) ;
#25325 = CARTESIAN_POINT ( 'NONE',  ( 17.00000000000000711, 25.24999999999998224, -4.000000000000000000 ) ) ;
#25326 = FACE_OUTER_BOUND ( 'NONE', #67988, .T. ) ;
#25327 = EDGE_CURVE ( 'NONE', #29227, #37744, #40656, .T. ) ;
#25328 = ORIENTED_EDGE ( 'NONE', *, *, #65117, .T. ) ;
#25329 = CARTESIAN_POINT ( 'NONE',  ( -8.437984349512095861, 111.6929263765338192, -5.166775262442723748E-16 ) ) ;
#25330 = FILL_AREA_STYLE_COLOUR ( '', #38629 ) ;
#25331 = FACE_OUTER_BOUND ( 'NONE', #18836, .T. ) ;
#25332 = EDGE_CURVE ( 'NONE', #4733, #22405, #9215, .T. ) ;
#25333 = DIRECTION ( 'NONE',  ( 0.000000000000000000, -1.000000000000000000, 0.000000000000000000 ) ) ;
#25334 = VECTOR ( 'NONE', #29552, 1000.000000000000000 ) ;
#25335 = CARTESIAN_POINT ( 'NONE',  ( 16.00000000000001776, 42.00000000000000000, 29.68999999999999417 ) ) ;
#25336 = EDGE_CURVE ( 'NONE', #34757, #9284, #19264, .T. ) ;
#25337 = ORIENTED_EDGE ( 'NONE', *, *, #28891, .T. ) ;
#25338 = CARTESIAN_POINT ( 'NONE',  ( -6.062177826491071286, 3.500000000000000888, 0.000000000000000000 ) ) ;
#25339 = VERTEX_POINT ( 'NONE', #19962 ) ;
#25340 = CARTESIAN_POINT ( 'NONE',  ( -61.94292637653379785, 0.000000000000000000, 9.524999999999991473 ) ) ;
#25341 = CARTESIAN_POINT ( 'NONE',  ( -6.062177826491072175, -3.499999999999998668, 0.000000000000000000 ) ) ;
#25342 = CARTESIAN_POINT ( 'NONE',  ( -154.4050000000000011, -2.607480562269069768, 8.024999999999991473 ) ) ;
#25343 = EDGE_LOOP ( 'NONE', ( #35296, #41352, #62628, #55307 ) ) ;
#25344 = DIRECTION ( 'NONE',  ( -0.000000000000000000, -0.000000000000000000, 1.000000000000000000 ) ) ;
#25345 = CIRCLE ( 'NONE', #6207, 0.2500000000000002220 ) ;
#25346 = EDGE_CURVE ( 'NONE', #47500, #11929, #47584, .T. ) ;
#25347 = AXIS2_PLACEMENT_3D ( 'NONE', #48349, #39, #21573 ) ;
#25348 = DIRECTION ( 'NONE',  ( 0.000000000000000000, 0.000000000000000000, -1.000000000000000000 ) ) ;
#25349 = CARTESIAN_POINT ( 'NONE',  ( -53.83246130318194389, -9.718525487688895126, 3.069079019093576388 ) ) ;
#25350 = CARTESIAN_POINT ( 'NONE',  ( 74.63815776008151204, 19.81286551027082155, 6.251809480268890162 ) ) ;
#25351 = ORIENTED_EDGE ( 'NONE', *, *, #12209, .T. ) ;
#25353 = EDGE_CURVE ( 'NONE', #58654, #35727, #32741, .T. ) ;
#25352 = ORIENTED_EDGE ( 'NONE', *, *, #22101, .T. ) ;
#25354 = CARTESIAN_POINT ( 'NONE',  ( 22.29420333151774614, 25.82372757702023236, 27.50001041218374453 ) ) ;
#25355 = CARTESIAN_POINT ( 'NONE',  ( -62.30499999999997840, 8.437984349512085203, -1.550032578732815448E-15 ) ) ;
#25356 = ORIENTED_EDGE ( 'NONE', *, *, #8239, .F. ) ;
#25357 = DIRECTION ( 'NONE',  ( 0.000000000000000000, 0.000000000000000000, -1.000000000000000000 ) ) ;
#25358 = CARTESIAN_POINT ( 'NONE',  ( -123.4429263765338192, -1.166476076187852838E-15, -9.524999999999991473 ) ) ;
#25359 = DIRECTION ( 'NONE',  ( 0.000000000000000000, -1.000000000000000000, 3.469446951953613794E-15 ) ) ;
#25360 = VERTEX_POINT ( 'NONE', #1134 ) ;
#25361 = AXIS2_PLACEMENT_3D ( 'NONE', #38563, #22335, #16052 ) ;
#25362 = CARTESIAN_POINT ( 'NONE',  ( -33.14152459314272647, -9.158144248744079619, -2.873992752689456864 ) ) ;
#25363 = CARTESIAN_POINT ( 'NONE',  ( 66.24999999999998579, 33.99999999999999289, -4.000000000000000000 ) ) ;
#25365 = CARTESIAN_POINT ( 'NONE',  ( 53.00000000000000000, 25.24999999999998579, -3.750000000000000000 ) ) ;
#25364 = FACE_OUTER_BOUND ( 'NONE', #66079, .T. ) ;
#25366 = VECTOR ( 'NONE', #37024, 1000.000000000000000 ) ;
#25367 = CARTESIAN_POINT ( 'NONE',  ( 8.102448949553183510, 150.9950000000000045, -5.886773742842746238 ) ) ;
#25368 = CARTESIAN_POINT ( 'NONE',  ( -93.89499999999998181, 6.826472737025116366, 4.959722759717898555 ) ) ;
#25369 = VECTOR ( 'NONE', #65391, 1000.000000000000000 ) ;
#25370 = MECHANICAL_DESIGN_GEOMETRIC_PRESENTATION_REPRESENTATION (  '', ( #68073 ), #13015 ) ;
#25371 = CARTESIAN_POINT ( 'NONE',  ( -52.50000000000000000, -2.024042244987997205E-14, 11.50000000000000000 ) ) ;
#25372 = EDGE_CURVE ( 'NONE', #12385, #11851, #54666, .T. ) ;
#25373 = CARTESIAN_POINT ( 'NONE',  ( -71.09292637653381064, 3.094860106618433360, 9.524999999999991473 ) ) ;
#25374 = ORIENTED_EDGE ( 'NONE', *, *, #43825, .F. ) ;
#25375 = CARTESIAN_POINT ( 'NONE',  ( -145.3429263765338249, -9.058813317711329915, 2.943386871421371787 ) ) ;
#25376 =( NAMED_UNIT ( * ) PLANE_ANGLE_UNIT ( ) SI_UNIT ( $, .RADIAN. ) );
#25377 = CARTESIAN_POINT ( 'NONE',  ( -33.77766424705443882, -9.706441239724112435, -3.029717036663232221 ) ) ;
#25378 = CARTESIAN_POINT ( 'NONE',  ( -158.8449999999999989, -7.632228543268599452, 2.479861379858951054 ) ) ;
#25379 =( NAMED_UNIT ( * ) PLANE_ANGLE_UNIT ( ) SI_UNIT ( $, .RADIAN. ) );
#25380 = CIRCLE ( 'NONE', #19810, 111.0000000000000142 ) ;
#25381 = LINE ( 'NONE', #8862, #24729 ) ;
#25382 = CIRCLE ( 'NONE', #6297, 12.50000000000000000 ) ;
#25383 = DIRECTION ( 'NONE',  ( -1.000000000000000000, -0.000000000000000000, -0.000000000000000000 ) ) ;
#25384 = CARTESIAN_POINT ( 'NONE',  ( -133.9429263765338192, 0.000000000000000000, 9.524999999999991473 ) ) ;
#25385 = EDGE_LOOP ( 'NONE', ( #6182, #66858, #65825, #46201 ) ) ;
#25386 = SURFACE_STYLE_USAGE ( .BOTH. , #59724 ) ;
#25387 = ORIENTED_EDGE ( 'NONE', *, *, #10981, .F. ) ;
#25388 = AXIS2_PLACEMENT_3D ( 'NONE', #68942, #37664, #20750 ) ;
#25389 = PRESENTATION_STYLE_ASSIGNMENT (( #3915 ) ) ;
#25390 = CARTESIAN_POINT ( 'NONE',  ( -2.607480562269115509, 117.0929263765338249, -8.024999999999970157 ) ) ;
#25391 = DIRECTION ( 'NONE',  ( -0.000000000000000000, -0.000000000000000000, -1.000000000000000000 ) ) ;
#25392 = CARTESIAN_POINT ( 'NONE',  ( -109.8570736234661780, -5.598654528085803328, -7.705886871421366635 ) ) ;
#25393 = ORIENTED_EDGE ( 'NONE', *, *, #49865, .F. ) ;
#25394 = CARTESIAN_POINT ( 'NONE',  ( -161.7549999999999955, 4.716976649647091513, -6.492361379858946790 ) ) ;
#25395 = ORIENTED_EDGE ( 'NONE', *, *, #50273, .T. ) ;
#25396 = LINE ( 'NONE', #40567, #39191 ) ;
#25397 = DIRECTION ( 'NONE',  ( -1.000000000000000000, 0.000000000000000000, 0.000000000000000000 ) ) ;
#25398 = ORIENTED_EDGE ( 'NONE', *, *, #13048, .T. ) ;
#25399 = DIRECTION ( 'NONE',  ( 0.000000000000000000, 0.000000000000000000, -1.000000000000000000 ) ) ;
#25400 = CARTESIAN_POINT ( 'NONE',  ( 36.00000000000002842, 5.000000000000000000, 32.00402776293825724 ) ) ;
#25401 = CARTESIAN_POINT ( 'NONE',  ( 8.102448949553183510, 111.9949999999999761, -5.886773742842746238 ) ) ;
#25402 = AXIS2_PLACEMENT_3D ( 'NONE', #23565, #34812, #45076 ) ;
#25403 = ORIENTED_EDGE ( 'NONE', *, *, #63528, .T. ) ;
#25404 = EDGE_CURVE ( 'NONE', #5753, #35195, #43812, .T. ) ;
#25405 = CARTESIAN_POINT ( 'NONE',  ( -4.041451884327381450, 7.000000000000006217, 1.082903768654761345 ) ) ;
#25406 = CARTESIAN_POINT ( 'NONE',  ( 8.102448949553181734, 125.1049999999999613, -5.886773742842746238 ) ) ;
#25407 = CARTESIAN_POINT ( 'NONE',  ( -69.65499999999998693, -7.632228543268600340, -2.479861379858950166 ) ) ;
#25408 = CARTESIAN_POINT ( 'NONE',  ( -80.30707362346618083, -10.01517768586948698, 6.132527647946031529E-16 ) ) ;
#25409 = PRODUCT_DEFINITION_SHAPE ( 'NONE', 'NONE',  #67906 ) ;
#25410 = ORIENTED_EDGE ( 'NONE', *, *, #34166, .F. ) ;
#25411 = CARTESIAN_POINT ( 'NONE',  ( 3.094860106618431583, 139.2050000000000125, 9.525000000000000355 ) ) ;
#25412 = CARTESIAN_POINT ( 'NONE',  ( 65.00000000000000000, 1.797044900979284448E-15, 6.999999999999988454 ) ) ;
#25413 = DIRECTION ( 'NONE',  ( -0.000000000000000000, -0.000000000000000000, -1.000000000000000000 ) ) ;
#25414 = AXIS2_PLACEMENT_3D ( 'NONE', #37243, #36558, #9792 ) ;
#25415 = EDGE_CURVE ( 'NONE', #37645, #39091, #13662, .T. ) ;
#25416 = CARTESIAN_POINT ( 'NONE',  ( -58.75000000000000000, -8.499999999999992895, 18.10000000000000497 ) ) ;
#25417 = CIRCLE ( 'NONE', #2920, 0.4999999999999990563 ) ;
#25418 = PRESENTATION_LAYER_ASSIGNMENT (  '', '', ( #44597 ) ) ;
#25419 = ORIENTED_EDGE ( 'NONE', *, *, #35122, .F. ) ;
#25420 = PLANE ( 'NONE',  #46430 ) ;
#25421 = CARTESIAN_POINT ( 'NONE',  ( 20.57648123223228254, 154.9999999999999716, -10.27659574468085069 ) ) ;
#25422 = CARTESIAN_POINT ( 'NONE',  ( -177.8049999999999784, -8.437984349512085203, 5.166775262442717831E-16 ) ) ;
#25423 = VERTEX_POINT ( 'NONE', #68881 ) ;
#25424 = CARTESIAN_POINT ( 'NONE',  ( 7.255760115451125536, 111.6477319965992763, -4.196031671614247394 ) ) ;
#25425 = CARTESIAN_POINT ( 'NONE',  ( 43.75000000000000000, 18.74999999999998224, -4.000000000000000000 ) ) ;
#25426 = DIRECTION ( 'NONE',  ( 0.000000000000000000, 1.000000000000000000, 0.000000000000000000 ) ) ;
#25427 = VERTEX_POINT ( 'NONE', #20682 ) ;
#25428 = SURFACE_STYLE_FILL_AREA ( #41641 ) ;
#25429 = CARTESIAN_POINT ( 'NONE',  ( -45.00000000000000000, 0.000000000000000000, 9.525000000000000355 ) ) ;
#25430 = VERTEX_POINT ( 'NONE', #33563 ) ;
#25431 = EDGE_CURVE ( 'NONE', #39125, #28212, #456, .T. ) ;
#25432 = CARTESIAN_POINT ( 'NONE',  ( -12.74999999999999822, 0.000000000000000000, 6.000000000000001776 ) ) ;
#25433 = AXIS2_PLACEMENT_3D ( 'NONE', #63889, #57595, #10455 ) ;
#25434 = CARTESIAN_POINT ( 'NONE',  ( 60.00000000000000000, 1.797044900979284448E-15, 10.00000000000000000 ) ) ;
#25435 = CARTESIAN_POINT ( 'NONE',  ( -92.90499999999997272, 2.607480562269068880, -8.024999999999993250 ) ) ;
#25436 = ORIENTED_EDGE ( 'NONE', *, *, #49443, .F. ) ;
#25437 =( LENGTH_UNIT ( ) NAMED_UNIT ( * ) SI_UNIT ( .MILLI., .METRE. ) );
#25438 = CARTESIAN_POINT ( 'NONE',  ( 5.000000000000000000, 6.123233995736766282E-16, 7.500000000000000000 ) ) ;
#25439 = CARTESIAN_POINT ( 'NONE',  ( -140.1570736234661751, -9.058813317711329915, -2.943386871421370898 ) ) ;
#25440 =( LENGTH_UNIT ( ) NAMED_UNIT ( * ) SI_UNIT ( .MILLI., .METRE. ) );
#25441 = SURFACE_STYLE_FILL_AREA ( #37446 ) ;
#25442 = CARTESIAN_POINT ( 'NONE',  ( -77.00707362346616947, -8.102448949553172852, -5.886773742842741797 ) ) ;
#25443 = VERTEX_POINT ( 'NONE', #39222 ) ;
#25444 = CARTESIAN_POINT ( 'NONE',  ( -16.14263016465302414, -10.96720793458296939, 4.870483257825171997 ) ) ;
#25446 = CARTESIAN_POINT ( 'NONE',  ( -6.418790567836330396, 2.472216779103305395, 2.882328613363590808 ) ) ;
#25445 =( LENGTH_UNIT ( ) NAMED_UNIT ( * ) SI_UNIT ( .MILLI., .METRE. ) );
#25447 = CARTESIAN_POINT ( 'NONE',  ( -115.7049999999999983, 2.607480562269073321, 8.024999999999991473 ) ) ;
#25449 = ADVANCED_FACE ( 'NONE', ( #42191 ), #44519, .F. ) ;
#25448 = CARTESIAN_POINT ( 'NONE',  ( 16.00000000000001776, 15.00000000000000000, -29.68999999999999417 ) ) ;
#25450 = CARTESIAN_POINT ( 'NONE',  ( -10.01517768586949231, 119.1949999999999932, -6.132527647946036459E-16 ) ) ;
#25451 = CARTESIAN_POINT ( 'NONE',  ( -127.9449999999999790, -9.827790563157499189E-16, -8.024999999999991473 ) ) ;
#25452 = SURFACE_STYLE_FILL_AREA ( #8599 ) ;
#25453 = EDGE_CURVE ( 'NONE', #8679, #1837, #22711, .T. ) ;
#25454 = SURFACE_STYLE_FILL_AREA ( #68049 ) ;
#25455 = CYLINDRICAL_SURFACE ( 'NONE', #39129, 0.5000000000000004441 ) ;
#25456 = ORIENTED_EDGE ( 'NONE', *, *, #67206, .F. ) ;
#25457 = DIRECTION ( 'NONE',  ( 1.000000000000000000, 0.000000000000000000, 0.000000000000000000 ) ) ;
#25458 = CARTESIAN_POINT ( 'NONE',  ( -173.8429263765338249, 9.058813317711329915, -2.943386871421373119 ) ) ;
#25459 = DIRECTION ( 'NONE',  ( -0.000000000000000000, -0.000000000000000000, -1.000000000000000000 ) ) ;
#25460 = VECTOR ( 'NONE', #21990, 1000.000000000000000 ) ;
#25461 = VECTOR ( 'NONE', #44080, 1000.000000000000000 ) ;
#25462 = AXIS2_PLACEMENT_3D ( 'NONE', #9175, #3848, #26012 ) ;
#25463 = DIRECTION ( 'NONE',  ( 0.000000000000000000, 0.000000000000000000, 1.000000000000000000 ) ) ;
#25464 = SURFACE_SIDE_STYLE ('',( #26497 ) ) ;
#25465 = ORIENTED_EDGE ( 'NONE', *, *, #56534, .F. ) ;
#25466 = CARTESIAN_POINT ( 'NONE',  ( -81.59292637653378222, -3.094860106618431139, -9.524999999999991473 ) ) ;
#25467 = CONTEXT_DEPENDENT_SHAPE_REPRESENTATION ( #35696, #32888 ) ;
#25468 = LINE ( 'NONE', #52582, #26002 ) ;
#25469 = CARTESIAN_POINT ( 'NONE',  ( 6.826472737025121695, 152.4929263765338305, -4.959722759717905660 ) ) ;
#25470 = PLANE ( 'NONE',  #30383 ) ;
#25471 = MECHANICAL_DESIGN_GEOMETRIC_PRESENTATION_REPRESENTATION (  '', ( #58041 ), #661 ) ;
#25472 = DIRECTION ( 'NONE',  ( -0.000000000000000000, 0.000000000000000000, 1.000000000000000000 ) ) ;
#25473 = VERTEX_POINT ( 'NONE', #6141 ) ;
#25474 = DIRECTION ( 'NONE',  ( -1.000000000000000000, 0.000000000000000000, 0.000000000000000000 ) ) ;
#25475 = EDGE_CURVE ( 'NONE', #69517, #39729, #6821, .T. ) ;
#25476 = ORIENTED_EDGE ( 'NONE', *, *, #45318, .T. ) ;
#25477 = DIRECTION ( 'NONE',  ( 0.000000000000000000, -1.000000000000000000, 0.000000000000000000 ) ) ;
#25478 = LINE ( 'NONE', #14961, #26329 ) ;
#25479 = CARTESIAN_POINT ( 'NONE',  ( 2.607480562269076430, 129.9070736234661467, -8.025000000000000355 ) ) ;
#25480 =( LENGTH_UNIT ( ) NAMED_UNIT ( * ) SI_UNIT ( .MILLI., .METRE. ) );
#25481 = ORIENTED_EDGE ( 'NONE', *, *, #34479, .F. ) ;
#25482 = CARTESIAN_POINT ( 'NONE',  ( -101.3070736234661808, -10.01517768586948698, 6.132527647946031529E-16 ) ) ;
#25483 = CARTESIAN_POINT ( 'NONE',  ( -101.6049999999999898, 6.826472737025113702, -4.959722759717902107 ) ) ;
#25484 = DIRECTION ( 'NONE',  ( 0.9486832980505138790, 0.3162277660168378857, -0.000000000000000000 ) ) ;
#25485 = ORIENTED_EDGE ( 'NONE', *, *, #25557, .F. ) ;
#25486 = CARTESIAN_POINT ( 'NONE',  ( 3.542752237027634976, -1.835478060177116566, -9.000000000000007105 ) ) ;
#25487 = EDGE_CURVE ( 'NONE', #3527, #32747, #27902, .T. ) ;
#25488 = DIRECTION ( 'NONE',  ( 0.000000000000000000, 0.000000000000000000, 1.000000000000000000 ) ) ;
#25489 = DIRECTION ( 'NONE',  ( 0.000000000000000000, 0.000000000000000000, 1.000000000000000000 ) ) ;
#25490 = ORIENTED_EDGE ( 'NONE', *, *, #56144, .T. ) ;
#25491 = ADVANCED_FACE ( 'NONE', ( #21987 ), #60620, .T. ) ;
#25492 = DIRECTION ( 'NONE',  ( 0.000000000000000000, -1.000000000000000000, 0.000000000000000000 ) ) ;
#25493 = CARTESIAN_POINT ( 'NONE',  ( -74.24499999999999034, -4.716976649647093289, -6.492361379858945902 ) ) ;
#25494 = ORIENTED_EDGE ( 'NONE', *, *, #61347, .F. ) ;
#25495 = CARTESIAN_POINT ( 'NONE',  ( 22.99999999999998934, 0.000000000000000000, 37.00402776293825724 ) ) ;
#25496 =( NAMED_UNIT ( * ) PLANE_ANGLE_UNIT ( ) SI_UNIT ( $, .RADIAN. ) );
#25497 = UNCERTAINTY_MEASURE_WITH_UNIT (LENGTH_MEASURE( 1.000000000000000082E-05 ), #41734, 'distance_accuracy_value', 'NONE');
#25498 = ORIENTED_EDGE ( 'NONE', *, *, #23659, .F. ) ;
#25499 = CARTESIAN_POINT ( 'NONE',  ( 20.42000000000000526, 0.000000000000000000, 12.50000000000000000 ) ) ;
#25500 = CARTESIAN_POINT ( 'NONE',  ( -74.99999999999998579, 50.00000000000000000, -11.50000000000000000 ) ) ;
#25501 = PRESENTATION_LAYER_ASSIGNMENT (  '', '', ( #51330 ) ) ;
#25502 = EDGE_CURVE ( 'NONE', #41266, #44352, #59753, .T. ) ;
#25503 =( NAMED_UNIT ( * ) SI_UNIT ( $, .STERADIAN. ) SOLID_ANGLE_UNIT ( ) );
#25504 = SPHERICAL_SURFACE ( 'NONE', #66034, 0.5000000000000000000 ) ;
#25505 = ORIENTED_EDGE ( 'NONE', *, *, #64872, .T. ) ;
#25506 = PRESENTATION_LAYER_ASSIGNMENT (  '', '', ( #37971 ) ) ;
#25507 = VERTEX_POINT ( 'NONE', #60296 ) ;
#25508 =( NAMED_UNIT ( * ) PLANE_ANGLE_UNIT ( ) SI_UNIT ( $, .RADIAN. ) );
#25509 = FACE_OUTER_BOUND ( 'NONE', #30775, .T. ) ;
#25510 = CARTESIAN_POINT ( 'NONE',  ( -41.06080360525773187, 107.9551383427286737, 3.682527553402528131 ) ) ;
#25511 = CARTESIAN_POINT ( 'NONE',  ( -165.9570736234661865, 9.058813317711329915, -2.943386871421373119 ) ) ;
#25512 = CARTESIAN_POINT ( 'NONE',  ( 8.102448949553181734, 126.9949999999999903, -5.886773742842746238 ) ) ;
#25513 = CARTESIAN_POINT ( 'NONE',  ( -101.9070736234661609, -3.094860106618429807, 9.524999999999991473 ) ) ;
#25514 = CARTESIAN_POINT ( 'NONE',  ( 2.607480562269055113, 113.7929263765338277, -8.025000000000016342 ) ) ;
#25515 = CARTESIAN_POINT ( 'NONE',  ( 8.000000000000035527, 5.000000000000000000, -77.00402776293825013 ) ) ;
#25516 = ORIENTED_EDGE ( 'NONE', *, *, #49556, .F. ) ;
#25517 =( BOUNDED_CURVE ( )  B_SPLINE_CURVE ( 2, ( #44688, #66800, #22853, #39741, #17593, #44349, #61480, #65409, #17909, #39058, #23871 ),
 .UNSPECIFIED., .F., .F. ) 
 B_SPLINE_CURVE_WITH_KNOTS ( ( 3, 2, 2, 2, 2, 3 ),
 ( 0.5434782608695525319, 0.5456521739130306692, 0.5478260869565089175, 0.5499999999999871658, 0.5521739130434654141, 0.5543478260869435514 ),
 .UNSPECIFIED. ) 
 CURVE ( )  GEOMETRIC_REPRESENTATION_ITEM ( )  RATIONAL_B_SPLINE_CURVE ( ( 1.000000000000284883, 0.9510565162948685369, 1.000000000000000000, 0.9510565162951535312, 1.000000000000000000, 0.9510565162951535312, 1.000000000000000000, 0.9510565162951535312, 1.000000000000000000, 0.9510565162954459639, 0.9999999999997075673 ) ) 
 REPRESENTATION_ITEM ( '' )  );
#25518 = SURFACE_STYLE_FILL_AREA ( #57182 ) ;
#25520 =( NAMED_UNIT ( * ) PLANE_ANGLE_UNIT ( ) SI_UNIT ( $, .RADIAN. ) );
#25519 = FACE_OUTER_BOUND ( 'NONE', #55106, .T. ) ;
#25521 = CIRCLE ( 'NONE', #29994, 3.100000000000000533 ) ;
#25522 = CARTESIAN_POINT ( 'NONE',  ( -149.3049999999999500, 8.437984349512085203, -1.550032578732815448E-15 ) ) ;
#25523 = PRESENTATION_STYLE_ASSIGNMENT (( #30101 ) ) ;
#25524 = CARTESIAN_POINT ( 'NONE',  ( -8.443929654699774190, 111.5904618153164449, 0.06143411491520953116 ) ) ;
#25525 = CARTESIAN_POINT ( 'NONE',  ( -154.0449999999999875, 7.632228543268600340, 2.479861379858949277 ) ) ;
#25526 = CARTESIAN_POINT ( 'NONE',  ( -150.8950000000000102, 6.826472737025115478, 4.959722759717899443 ) ) ;
#25527 = ORIENTED_EDGE ( 'NONE', *, *, #24861, .T. ) ;
#25528 = LINE ( 'NONE', #68821, #32450 ) ;
#25529 =( LENGTH_UNIT ( ) NAMED_UNIT ( * ) SI_UNIT ( .MILLI., .METRE. ) );
#25530 = UNCERTAINTY_MEASURE_WITH_UNIT (LENGTH_MEASURE( 1.000000000000000082E-05 ), #48368, 'distance_accuracy_value', 'NONE');
#25531 = CARTESIAN_POINT ( 'NONE',  ( -59.15499999999998693, 7.632228543268600340, 2.479861379858949277 ) ) ;
#25532 = CARTESIAN_POINT ( 'NONE',  ( -60.14499999999998892, -4.716976649647092401, 6.492361379858946790 ) ) ;
#25533 = CARTESIAN_POINT ( 'NONE',  ( -8.102448949553181734, 153.6049999999999898, 5.886773742842747126 ) ) ;
#25534 = DIRECTION ( 'NONE',  ( -0.000000000000000000, -0.000000000000000000, -1.000000000000000000 ) ) ;
#25535 = CARTESIAN_POINT ( 'NONE',  ( 0.000000000000000000, 1.000000000000000222, -3.000000000000000000 ) ) ;
#25536 = UNCERTAINTY_MEASURE_WITH_UNIT (LENGTH_MEASURE( 1.000000000000000082E-05 ), #21640, 'distance_accuracy_value', 'NONE');
#25537 = CARTESIAN_POINT ( 'NONE',  ( -6.669484432086554726, 110.5589211602357267, 6.756431230639685204 ) ) ;
#25538 = LINE ( 'NONE', #47055, #4549 ) ;
#25539 = AXIS2_PLACEMENT_3D ( 'NONE', #16466, #31552, #9784 ) ;
#25540 = VECTOR ( 'NONE', #48149, 1000.000000000000000 ) ;
#25541 = LINE ( 'NONE', #47056, #10254 ) ;
#25542 = MECHANICAL_DESIGN_GEOMETRIC_PRESENTATION_REPRESENTATION (  '', ( #4193 ), #7660 ) ;
#25543 = CARTESIAN_POINT ( 'NONE',  ( -27.87363414264613937, -7.580382958994807296, -0.06854651313594288531 ) ) ;
#25544 = ADVANCED_FACE ( 'NONE', ( #19460 ), #28951, .T. ) ;
#25545 = DIRECTION ( 'NONE',  ( -1.156482317317870344E-15, 1.000000000000000000, 0.000000000000000000 ) ) ;
#25546 = ORIENTED_EDGE ( 'NONE', *, *, #15888, .F. ) ;
#25547 = ORIENTED_EDGE ( 'NONE', *, *, #30734, .F. ) ;
#25548 = EDGE_CURVE ( 'NONE', #52546, #61196, #40963, .T. ) ;
#25549 = ADVANCED_FACE ( 'NONE', ( #19097 ), #3234, .F. ) ;
#25550 = CARTESIAN_POINT ( 'NONE',  ( -20.86748625714523087, 115.0277251398784273, 10.00000000000000000 ) ) ;
#25551 = CARTESIAN_POINT ( 'NONE',  ( 22.29422224269975672, 26.00000000000000355, -27.50000000000000711 ) ) ;
#25552 = VERTEX_POINT ( 'NONE', #40249 ) ;
#25553 = ORIENTED_EDGE ( 'NONE', *, *, #31362, .T. ) ;
#25554 = CARTESIAN_POINT ( 'NONE',  ( -108.0570736234661666, 0.000000000000000000, 9.524999999999991473 ) ) ;
#25555 = PRESENTATION_LAYER_ASSIGNMENT (  '', '', ( #58136 ) ) ;
#25556 = LINE ( 'NONE', #63886, #1617 ) ;
#25557 = EDGE_CURVE ( 'NONE', #43604, #52539, #45293, .T. ) ;
#25558 = VERTEX_POINT ( 'NONE', #8234 ) ;
#25559 = CARTESIAN_POINT ( 'NONE',  ( 8.102448949553181734, 118.5049999999999955, 5.886773742842750679 ) ) ;
#25560 = LINE ( 'NONE', #5152, #49032 ) ;
#25561 = VERTEX_POINT ( 'NONE', #39925 ) ;
#25562 = EDGE_CURVE ( 'NONE', #31257, #40876, #53042, .T. ) ;
#25563 = EDGE_CURVE ( 'NONE', #29661, #4018, #33899, .T. ) ;
#25564 = CARTESIAN_POINT ( 'NONE',  ( -30.38025804287905629, -8.499999999999996447, 0.06931351858032895608 ) ) ;
#25565 = CARTESIAN_POINT ( 'NONE',  ( -96.89499999999998181, 6.826472737025116366, 4.959722759717898555 ) ) ;
#25566 = ORIENTED_EDGE ( 'NONE', *, *, #13916, .T. ) ;
#25567 = LINE ( 'NONE', #51628, #58025 ) ;
#25568 = CARTESIAN_POINT ( 'NONE',  ( -164.4570736234661865, -9.058813317711329915, 2.943386871421371787 ) ) ;
#25569 = ADVANCED_FACE ( 'NONE', ( #24721 ), #51944, .T. ) ;
#25570 = CARTESIAN_POINT ( 'NONE',  ( -178.8570736234661638, -5.598654528085803328, -7.705886871421366635 ) ) ;
#25571 = VERTEX_POINT ( 'NONE', #13480 ) ;
#25572 = CARTESIAN_POINT ( 'NONE',  ( -4.716976649647097730, 159.2429263765338021, -6.492361379858953896 ) ) ;
#25573 =( NAMED_UNIT ( * ) SI_UNIT ( $, .STERADIAN. ) SOLID_ANGLE_UNIT ( ) );
#25574 =( NAMED_UNIT ( * ) SI_UNIT ( $, .STERADIAN. ) SOLID_ANGLE_UNIT ( ) );
#25575 = ORIENTED_EDGE ( 'NONE', *, *, #52985, .T. ) ;
#25576 = CARTESIAN_POINT ( 'NONE',  ( -62.15707362346617515, -9.058813317711329915, -2.943386871421370898 ) ) ;
#25577 = VERTEX_POINT ( 'NONE', #2894 ) ;
#25578 =( LENGTH_UNIT ( ) NAMED_UNIT ( * ) SI_UNIT ( .MILLI., .METRE. ) );
#25579 =( NAMED_UNIT ( * ) SI_UNIT ( $, .STERADIAN. ) SOLID_ANGLE_UNIT ( ) );
#25580 = CARTESIAN_POINT ( 'NONE',  ( -120.2049999999999983, -2.607480562269071545, -8.024999999999991473 ) ) ;
#25581 = CARTESIAN_POINT ( 'NONE',  ( -184.0000000000000568, -7.022622464067349135, 3.903023461144195405 ) ) ;
#25582 = CARTESIAN_POINT ( 'NONE',  ( 6.826472737025119919, 141.0070736234661410, 4.959722759717908325 ) ) ;
#25583 = DIRECTION ( 'NONE',  ( -0.000000000000000000, -0.000000000000000000, -1.000000000000000000 ) ) ;
#25584 = CIRCLE ( 'NONE', #28939, 3.100000000000000533 ) ;
#25585 = SURFACE_STYLE_FILL_AREA ( #26285 ) ;
#25586 = CARTESIAN_POINT ( 'NONE',  ( -74.99999999999998579, 36.00000000000000711, 9.500000000000001776 ) ) ;
#25587 = DIRECTION ( 'NONE',  ( 0.000000000000000000, 0.000000000000000000, -1.000000000000000000 ) ) ;
#25588 = DIRECTION ( 'NONE',  ( 0.000000000000000000, -1.000000000000000000, 0.000000000000000000 ) ) ;
#25589 = ORIENTED_EDGE ( 'NONE', *, *, #46548, .F. ) ;
#25590 = AXIS2_PLACEMENT_3D ( 'NONE', #58914, #41721, #10390 ) ;
#25591 = ORIENTED_EDGE ( 'NONE', *, *, #24679, .F. ) ;
#25592 = AXIS2_PLACEMENT_3D ( 'NONE', #13937, #45648, #67399 ) ;
#25593 = DIRECTION ( 'NONE',  ( 1.000000000000000000, 0.000000000000000000, 0.000000000000000000 ) ) ;
#25594 = DIRECTION ( 'NONE',  ( -1.000000000000000000, 0.000000000000000000, 0.000000000000000000 ) ) ;
#25595 = CARTESIAN_POINT ( 'NONE',  ( 0.000000000000000000, 115.0570736234661666, -8.025000000000000355 ) ) ;
#25596 = ORIENTED_EDGE ( 'NONE', *, *, #54386, .F. ) ;
#25597 = FACE_OUTER_BOUND ( 'NONE', #66802, .T. ) ;
#25598 = CARTESIAN_POINT ( 'NONE',  ( -181.7050000000000125, 2.607480562269073321, 8.024999999999991473 ) ) ;
#25599 = CARTESIAN_POINT ( 'NONE',  ( -7.794228634059948035, 2.500000000000000000, 4.499999999999999112 ) ) ;
#25600 = LINE ( 'NONE', #35135, #54923 ) ;
#25601 = CARTESIAN_POINT ( 'NONE',  ( -183.4449999999999932, 0.000000000000000000, 8.024999999999991473 ) ) ;
#25602 = CARTESIAN_POINT ( 'NONE',  ( -177.7449999999999761, 4.716976649647094177, 6.492361379858945902 ) ) ;
#25603 = CARTESIAN_POINT ( 'NONE',  ( 48.00000000000000000, 14.49137674618942562, -9.500000000000000000 ) ) ;
#25604 = ORIENTED_EDGE ( 'NONE', *, *, #41585, .T. ) ;
#25605 = CARTESIAN_POINT ( 'NONE',  ( 71.62068965517239860, 36.41396814395972115, -7.500000000000000000 ) ) ;
#25606 = CARTESIAN_POINT ( 'NONE',  ( 0.000000000000000000, 118.0570736234661524, -8.025000000000000355 ) ) ;
#25607 = CARTESIAN_POINT ( 'NONE',  ( -13.37809012747797865, 11.02455069633067275, 4.741122039576717739 ) ) ;
#25608 = CARTESIAN_POINT ( 'NONE',  ( -95.60499999999998977, 6.826472737025113702, -4.959722759717902107 ) ) ;
#25609 = FILL_AREA_STYLE ('',( #31585 ) ) ;
#25611 = CARTESIAN_POINT ( 'NONE',  ( -75.31874094084331261, 36.08947156080473206, -9.789663200461481196 ) ) ;
#25610 = MECHANICAL_DESIGN_GEOMETRIC_PRESENTATION_REPRESENTATION (  '', ( #43600 ), #61554 ) ;
#25612 = MECHANICAL_DESIGN_GEOMETRIC_PRESENTATION_REPRESENTATION (  '', ( #6437 ), #17766 ) ;
#25613 = CARTESIAN_POINT ( 'NONE',  ( -89.69499999999997897, -8.437984349512086979, 5.166775262442717831E-16 ) ) ;
#25614 = CARTESIAN_POINT ( 'NONE',  ( -9.058813317711338797, 126.4549999999999841, 2.943386871421373563 ) ) ;
#25615 = CARTESIAN_POINT ( 'NONE',  ( -71.69499999999999318, -8.437984349512085203, 5.166775262442717831E-16 ) ) ;
#25616 = CARTESIAN_POINT ( 'NONE',  ( -15.48999599679679662, 118.4999999999999716, -7.500000000000000000 ) ) ;
#25617 = CARTESIAN_POINT ( 'NONE',  ( -56.15707362346616804, -9.058813317711329915, -2.943386871421370898 ) ) ;
#25618 = DIRECTION ( 'NONE',  ( 1.000000000000000000, 0.000000000000000000, -0.000000000000000000 ) ) ;
#25619 = UNCERTAINTY_MEASURE_WITH_UNIT (LENGTH_MEASURE( 1.000000000000000082E-05 ), #36213, 'distance_accuracy_value', 'NONE');
#25620 =( LENGTH_UNIT ( ) NAMED_UNIT ( * ) SI_UNIT ( .MILLI., .METRE. ) );
#25621 = SURFACE_STYLE_FILL_AREA ( #3084 ) ;
#25622 = EDGE_LOOP ( 'NONE', ( #51210, #11555, #1601, #15096 ) ) ;
#25623 = CARTESIAN_POINT ( 'NONE',  ( -100.4929263765337879, -8.102448949553172852, 5.886773742842742685 ) ) ;
#25624 = CARTESIAN_POINT ( 'NONE',  ( -131.2450000000000045, -4.716976649647093289, -6.492361379858945902 ) ) ;
#25625 = CARTESIAN_POINT ( 'NONE',  ( -9.827790563157511022E-16, 146.5570736234661524, 8.025000000000000355 ) ) ;
#25626 = EDGE_CURVE ( 'NONE', #5088, #52924, #67660, .T. ) ;
#25627 = ADVANCED_FACE ( 'NONE', ( #50441 ), #51147, .T. ) ;
#25629 = CARTESIAN_POINT ( 'NONE',  ( -84.49999999999998579, -3.499999999999999556, 0.000000000000000000 ) ) ;
#25628 = CARTESIAN_POINT ( 'NONE',  ( -132.4429263765338192, -1.166476076187852838E-15, -9.524999999999991473 ) ) ;
#25630 = ORIENTED_EDGE ( 'NONE', *, *, #52972, .F. ) ;
#25631 =( GEOMETRIC_REPRESENTATION_CONTEXT ( 3 ) GLOBAL_UNCERTAINTY_ASSIGNED_CONTEXT ( ( #34854 ) ) GLOBAL_UNIT_ASSIGNED_CONTEXT ( ( #64770, #2050, #11297 ) ) REPRESENTATION_CONTEXT ( 'NONE', 'WORKASPACE' ) );
#25632 = ORIENTED_EDGE ( 'NONE', *, *, #49116, .T. ) ;
#25633 = CARTESIAN_POINT ( 'NONE',  ( -1.011095968855053334E-15, -8.500000000000000000, 21.00000000000000000 ) ) ;
#25634 = ADVANCED_FACE ( 'NONE', ( #4667 ), #32849, .T. ) ;
#25635 =( BOUNDED_SURFACE ( )  B_SPLINE_SURFACE ( 3, 2, ( 
 ( #611, #43628, #65024 ),
 ( #33041, #8722, #13641 ),
 ( #3389, #35104, #46040 ),
 ( #24524, #62520, #66779 ),
 ( #30151, #51289, #40402 ),
 ( #67818, #51632, #18594 ) ),
 .UNSPECIFIED., .F., .F., .F. ) 
 B_SPLINE_SURFACE_WITH_KNOTS ( ( 4, 2, 4 ),
 ( 3, 3 ),
 ( 0.03640205491000769733, 0.03794596731985258597, 0.03948987972969747462 ),
 ( 0.000000000000000000, 0.3658361493744603510 ),
 .UNSPECIFIED. ) 
 GEOMETRIC_REPRESENTATION_ITEM ( )  RATIONAL_B_SPLINE_SURFACE ( (
 ( 1.000000000000000000, 0.9724907272181566587, 0.9651092272895156476),
 ( 1.000000000000000000, 0.9724900729383123554, 0.9651083974482648209),
 ( 1.000000000000000000, 0.9723552707549931728, 0.9649374241049719636),
 ( 1.000000000000000000, 0.9718243316192900494, 0.9642640192914814223),
 ( 1.000000000000000000, 0.9714236478976183697, 0.9637558210278448501),
 ( 1.000000000000000000, 0.9708971511394390852, 0.9630880506048271616) ) ) 
 REPRESENTATION_ITEM ( '' )  SURFACE ( )  );
#25636 = DIRECTION ( 'NONE',  ( -0.000000000000000000, -1.000000000000000000, -0.000000000000000000 ) ) ;
#25637 = CARTESIAN_POINT ( 'NONE',  ( -71.99999999999998579, 64.07124727947029896, -7.500000000000000000 ) ) ;
#25638 = CIRCLE ( 'NONE', #63810, 4.499999999999976019 ) ;
#25639 = SURFACE_STYLE_FILL_AREA ( #56974 ) ;
#25641 = DIRECTION ( 'NONE',  ( 0.000000000000000000, 0.000000000000000000, 1.000000000000000000 ) ) ;
#25640 = MECHANICAL_DESIGN_GEOMETRIC_PRESENTATION_REPRESENTATION (  '', ( #49277 ), #35762 ) ;
#25642 = EDGE_LOOP ( 'NONE', ( #49640, #4566, #12613, #2366 ) ) ;
#25643 = CARTESIAN_POINT ( 'NONE',  ( -123.3549999999999898, -4.716976649647093289, -6.492361379858945902 ) ) ;
#25644 = VERTEX_POINT ( 'NONE', #20142 ) ;
#25645 = FILL_AREA_STYLE ('',( #21413 ) ) ;
#25646 = CARTESIAN_POINT ( 'NONE',  ( -124.1070736234661638, 8.102448949553171076, -5.886773742842744461 ) ) ;
#25647 = VERTEX_POINT ( 'NONE', #21187 ) ;
#25648 = DIRECTION ( 'NONE',  ( 0.000000000000000000, 0.000000000000000000, -1.000000000000000000 ) ) ;
#25649 = EDGE_LOOP ( 'NONE', ( #3036, #34387, #1562, #9806, #7331, #65232 ) ) ;
#25650 = EDGE_CURVE ( 'NONE', #12327, #38988, #69062, .T. ) ;
#25651 = AXIS2_PLACEMENT_3D ( 'NONE', #42399, #68387, #36426 ) ;
#25652 = FILL_AREA_STYLE_COLOUR ( '', #16395 ) ;
#25653 = CARTESIAN_POINT ( 'NONE',  ( -8.102448949553181734, 149.4949999999999761, 5.886773742842747126 ) ) ;
#25654 =( LENGTH_UNIT ( ) NAMED_UNIT ( * ) SI_UNIT ( .MILLI., .METRE. ) );
#25655 = COLOUR_RGB ( '', 0.72549020, 0.75294118, 0.79215686) ;
#25656 = ORIENTED_EDGE ( 'NONE', *, *, #15680, .T. ) ;
#25657 = PRESENTATION_STYLE_ASSIGNMENT (( #20393 ) ) ;
#25658 = CARTESIAN_POINT ( 'NONE',  ( 3.094860106618431583, 145.2049999999999557, 9.525000000000000355 ) ) ;
#25659 = ADVANCED_FACE ( 'NONE', ( #20511 ), #25094, .F. ) ;
#25660 = DIRECTION ( 'NONE',  ( -0.000000000000000000, -0.000000000000000000, 1.000000000000000000 ) ) ;
#25661 = VERTEX_POINT ( 'NONE', #51842 ) ;
#25662 = CARTESIAN_POINT ( 'NONE',  ( -4.716976649647098618, 127.1429263765338220, 6.492361379858953008 ) ) ;
#25663 = CARTESIAN_POINT ( 'NONE',  ( 10.57623092156539535, 58.31681314173471975, 6.349999999999996092 ) ) ;
#25664 = UNCERTAINTY_MEASURE_WITH_UNIT (LENGTH_MEASURE( 1.000000000000000082E-05 ), #46318, 'distance_accuracy_value', 'NONE');
#25665 = CARTESIAN_POINT ( 'NONE',  ( -47.45707362346615810, -9.058813317711329915, 2.943386871421371787 ) ) ;
#25666 = CIRCLE ( 'NONE', #9980, 0.2500000000000002220 ) ;
#25667 = CARTESIAN_POINT ( 'NONE',  ( 45.64107345563336793, 10.15688972729204487, 6.260993343996500649 ) ) ;
#25668 = ORIENTED_EDGE ( 'NONE', *, *, #61941, .T. ) ;
#25669 = CARTESIAN_POINT ( 'NONE',  ( 26.00000000000001776, 43.00000000000000000, 36.50000000000000000 ) ) ;
#25670 = VERTEX_POINT ( 'NONE', #25774 ) ;
#25671 = CARTESIAN_POINT ( 'NONE',  ( -59.69292637653379785, 10.01517768586948698, -1.839758294383808571E-15 ) ) ;
#25672 = CARTESIAN_POINT ( 'NONE',  ( -5.185928986913077132, -5.017707510222358280, 0.2088670156639313991 ) ) ;
#25673 = CARTESIAN_POINT ( 'NONE',  ( -148.7049999999999841, 2.607480562269073321, 8.024999999999991473 ) ) ;
#25674 = VERTEX_POINT ( 'NONE', #58157 ) ;
#25675 = CARTESIAN_POINT ( 'NONE',  ( -22.75000000000000711, 36.75000000000000000, -3.750000000000000000 ) ) ;
#25676 = UNCERTAINTY_MEASURE_WITH_UNIT (LENGTH_MEASURE( 1.000000000000000082E-05 ), #28297, 'distance_accuracy_value', 'NONE');
#25677 = PRESENTATION_LAYER_ASSIGNMENT (  '', '', ( #15576 ) ) ;
#25678 = CARTESIAN_POINT ( 'NONE',  ( 57.49999999999999289, 28.24999999999998934, 3.750000000000000000 ) ) ;
#25679 =( LENGTH_UNIT ( ) NAMED_UNIT ( * ) SI_UNIT ( .MILLI., .METRE. ) );
#25680 = ORIENTED_EDGE ( 'NONE', *, *, #47785, .F. ) ;
#25681 = EDGE_LOOP ( 'NONE', ( #28666, #39370, #65975, #68071, #37750, #6303, #16039 ) ) ;
#25682 = DIRECTION ( 'NONE',  ( 1.000000000000000000, 0.000000000000000000, 0.000000000000000000 ) ) ;
#25683 = VECTOR ( 'NONE', #18361, 1000.000000000000000 ) ;
#25684 = CARTESIAN_POINT ( 'NONE',  ( -68.00499999999998124, 6.826472737025116366, 4.959722759717898555 ) ) ;
#25685 = EDGE_LOOP ( 'NONE', ( #48892, #62241, #1003, #53397 ) ) ;
#25686 = SURFACE_SIDE_STYLE ('',( #57022 ) ) ;
#25687 = COLOUR_RGB ( '', 0.08235294, 0.09019608, 0.10196078) ;
#25688 = AXIS2_PLACEMENT_3D ( 'NONE', #66502, #40836, #66861 ) ;
#25689 = CARTESIAN_POINT ( 'NONE',  ( 5.000000000000000000, 6.123233995736766282E-16, 1.000000000000000000 ) ) ;
#25690 = DIRECTION ( 'NONE',  ( -0.000000000000000000, -1.000000000000000000, -0.000000000000000000 ) ) ;
#25691 = AXIS2_PLACEMENT_3D ( 'NONE', #44934, #33640, #45283 ) ;
#25692 = ORIENTED_EDGE ( 'NONE', *, *, #25869, .T. ) ;
#25693 = EDGE_CURVE ( 'NONE', #57903, #9427, #11452, .T. ) ;
#25694 = CARTESIAN_POINT ( 'NONE',  ( -75.00000000000000000, 8.092291901769643303, -5.807866024088082391 ) ) ;
#25695 = LINE ( 'NONE', #21124, #38327 ) ;
#25696 = LINE ( 'NONE', #29328, #1553 ) ;
#25697 = TOROIDAL_SURFACE ( 'NONE', #63901, 0.5000000000000000000, 0.2500000000000000000 ) ;
#25699 = CARTESIAN_POINT ( 'NONE',  ( -9.827790563157511022E-16, 125.5570736234661524, 8.025000000000000355 ) ) ;
#25698 = CARTESIAN_POINT ( 'NONE',  ( 44.99999999999999289, 10.00000000000000533, 4.000000000000000000 ) ) ;
#25700 = CARTESIAN_POINT ( 'NONE',  ( 5.598654528085805993, 144.2449999999999761, 7.705886871421374629 ) ) ;
#25701 = CARTESIAN_POINT ( 'NONE',  ( -95.69499999999997897, -8.437984349512085203, 5.166775262442717831E-16 ) ) ;
#25702 = FILL_AREA_STYLE_COLOUR ( '', #3766 ) ;
#25703 = UNCERTAINTY_MEASURE_WITH_UNIT (LENGTH_MEASURE( 1.000000000000000082E-05 ), #23943, 'distance_accuracy_value', 'NONE');
#25704 = MECHANICAL_DESIGN_GEOMETRIC_PRESENTATION_REPRESENTATION (  '', ( #44891 ), #59440 ) ;
#25705 = DIRECTION ( 'NONE',  ( -1.000000000000000000, 0.000000000000000000, 0.000000000000000000 ) ) ;
#25706 = EDGE_LOOP ( 'NONE', ( #7606, #664, #38029, #9086 ) ) ;
#25707 = CARTESIAN_POINT ( 'NONE',  ( -137.6929263765337623, 10.01517768586948698, -1.839758294383808571E-15 ) ) ;
#25708 = FILL_AREA_STYLE ('',( #27083 ) ) ;
#25709 = LINE ( 'NONE', #47944, #62421 ) ;
#25710 = CARTESIAN_POINT ( 'NONE',  ( -155.3950000000000102, -6.826472737025115478, -4.959722759717899443 ) ) ;
#25711 = CIRCLE ( 'NONE', #48214, 0.5000000000000004441 ) ;
#25712 = EDGE_CURVE ( 'NONE', #68025, #38153, #26472, .T. ) ;
#25713 = ADVANCED_FACE ( 'NONE', ( #9276 ), #36247, .F. ) ;
#25714 = DIRECTION ( 'NONE',  ( 0.000000000000000000, 1.000000000000000000, -0.000000000000000000 ) ) ;
#25715 = FILL_AREA_STYLE ('',( #69006 ) ) ;
#25716 = CARTESIAN_POINT ( 'NONE',  ( -133.7929263765344956, -3.094860106607741468, 9.525000000007759482 ) ) ;
#25717 = ORIENTED_EDGE ( 'NONE', *, *, #13993, .F. ) ;
#25718 = SURFACE_SIDE_STYLE ('',( #31005 ) ) ;
#25719 = ORIENTED_EDGE ( 'NONE', *, *, #67033, .F. ) ;
#25720 = UNCERTAINTY_MEASURE_WITH_UNIT (LENGTH_MEASURE( 1.000000000000000082E-05 ), #7268, 'distance_accuracy_value', 'NONE');
#25721 = EDGE_CURVE ( 'NONE', #33218, #28673, #33942, .T. ) ;
#25722 = AXIS2_PLACEMENT_3D ( 'NONE', #68904, #15785, #47120 ) ;
#25723 = FACE_OUTER_BOUND ( 'NONE', #17054, .T. ) ;
#25724 = CARTESIAN_POINT ( 'NONE',  ( -45.90428468476780210, 9.387774908331767421, 6.120769290545535313 ) ) ;
#25725 = CARTESIAN_POINT ( 'NONE',  ( -109.7070736234670534, -3.094860106633489316, -9.524999999989050892 ) ) ;
#25726 = ADVANCED_FACE ( 'NONE', ( #47287, #47655 ), #68359, .T. ) ;
#25727 = FACE_OUTER_BOUND ( 'NONE', #14506, .T. ) ;
#25728 = AXIS2_PLACEMENT_3D ( 'NONE', #28346, #61406, #13222 ) ;
#25729 = ORIENTED_EDGE ( 'NONE', *, *, #55980, .F. ) ;
#25730 = CARTESIAN_POINT ( 'NONE',  ( -147.2050000000000125, -2.607480562269071545, -8.024999999999991473 ) ) ;
#25731 = VERTEX_POINT ( 'NONE', #43060 ) ;
#25732 = DIRECTION ( 'NONE',  ( 0.000000000000000000, 0.000000000000000000, 1.000000000000000000 ) ) ;
#25733 = DIRECTION ( 'NONE',  ( 0.000000000000000000, 1.000000000000000000, 0.000000000000000000 ) ) ;
#25734 = ORIENTED_EDGE ( 'NONE', *, *, #1933, .T. ) ;
#25735 = AXIS2_PLACEMENT_3D ( 'NONE', #13157, #34975, #56426 ) ;
#25736 = EDGE_CURVE ( 'NONE', #14037, #69269, #51990, .T. ) ;
#25737 = AXIS2_PLACEMENT_3D ( 'NONE', #48057, #25848, #30411 ) ;
#25738 = CARTESIAN_POINT ( 'NONE',  ( -10.74999999999999645, 4.336808689942018722E-16, 19.00000000000000000 ) ) ;
#25739 = CARTESIAN_POINT ( 'NONE',  ( -121.9429263765338050, 0.000000000000000000, 9.524999999999991473 ) ) ;
#25740 = CARTESIAN_POINT ( 'NONE',  ( -5.598654528085808657, 119.6449999999999818, 7.705886871421373741 ) ) ;
#25741 =( GEOMETRIC_REPRESENTATION_CONTEXT ( 3 ) GLOBAL_UNCERTAINTY_ASSIGNED_CONTEXT ( ( #54581 ) ) GLOBAL_UNIT_ASSIGNED_CONTEXT ( ( #12438, #17423, #1843 ) ) REPRESENTATION_CONTEXT ( 'NONE', 'WORKASPACE' ) );
#25742 = ORIENTED_EDGE ( 'NONE', *, *, #31299, .T. ) ;
#25743 = CARTESIAN_POINT ( 'NONE',  ( -58.64292637653378648, -5.598654528085801552, 7.705886871421367523 ) ) ;
#25744 = CARTESIAN_POINT ( 'NONE',  ( 3.094860106618435136, 122.4049999999999727, -9.525000000000000355 ) ) ;
#25745 = CARTESIAN_POINT ( 'NONE',  ( -67.70499999999999829, 2.607480562269072433, 8.024999999999991473 ) ) ;
#25746 = EDGE_CURVE ( 'NONE', #5856, #59351, #59810, .T. ) ;
#25747 = FACE_OUTER_BOUND ( 'NONE', #38009, .T. ) ;
#25748 = ORIENTED_EDGE ( 'NONE', *, *, #65861, .F. ) ;
#25749 = CARTESIAN_POINT ( 'NONE',  ( 9.058813317711337021, 136.6550000000000011, 2.943386871421375783 ) ) ;
#25750 = UNCERTAINTY_MEASURE_WITH_UNIT (LENGTH_MEASURE( 1.000000000000000082E-05 ), #56227, 'distance_accuracy_value', 'NONE');
#25751 = STYLED_ITEM ( 'NONE', ( #50652 ), #51411 ) ;
#25752 = DIRECTION ( 'NONE',  ( -1.000000000000000000, -0.000000000000000000, -0.000000000000000000 ) ) ;
#25753 = DIRECTION ( 'NONE',  ( 0.000000000000000000, 0.000000000000000000, -1.000000000000000000 ) ) ;
#25754 = CARTESIAN_POINT ( 'NONE',  ( -41.11302593432306196, 107.5810679765800444, 3.326249178529583350 ) ) ;
#25755 = DIRECTION ( 'NONE',  ( 1.000000000000000000, 0.000000000000000000, -1.300977106640442040E-16 ) ) ;
#25756 = EDGE_LOOP ( 'NONE', ( #7327, #5318, #13663, #58143 ) ) ;
#25757 = VECTOR ( 'NONE', #52213, 1000.000000000000000 ) ;
#25758 = CARTESIAN_POINT ( 'NONE',  ( -51.50000000000000000, -2.024042244987997205E-14, 10.00000000000000000 ) ) ;
#25759 = DIRECTION ( 'NONE',  ( 1.156482317317873451E-16, 1.000000000000000000, -0.000000000000000000 ) ) ;
#25760 = CARTESIAN_POINT ( 'NONE',  ( -47.09499999999999886, -2.607480562269071545, -8.024999999999991473 ) ) ;
#25761 = ORIENTED_EDGE ( 'NONE', *, *, #68873, .T. ) ;
#25762 = CARTESIAN_POINT ( 'NONE',  ( 7.398101581744993993, 111.6353782664878764, -3.965660541892887636 ) ) ;
#25763 =( GEOMETRIC_REPRESENTATION_CONTEXT ( 3 ) GLOBAL_UNCERTAINTY_ASSIGNED_CONTEXT ( ( #49584 ) ) GLOBAL_UNIT_ASSIGNED_CONTEXT ( ( #36125, #5365, #53910 ) ) REPRESENTATION_CONTEXT ( 'NONE', 'WORKASPACE' ) );
#25764 = SURFACE_STYLE_FILL_AREA ( #20502 ) ;
#25765 = FACE_OUTER_BOUND ( 'NONE', #35642, .T. ) ;
#25766 = ORIENTED_EDGE ( 'NONE', *, *, #52543, .T. ) ;
#25767 = DIRECTION ( 'NONE',  ( 0.000000000000000000, 0.000000000000000000, 1.000000000000000000 ) ) ;
#25768 = DIRECTION ( 'NONE',  ( 0.000000000000000000, 1.000000000000000000, 0.000000000000000000 ) ) ;
#25769 = EDGE_LOOP ( 'NONE', ( #53856, #52328, #2454, #44755, #43377, #2127, #66863, #4714, #33031, #20931, #57460, #9888, #40479, #14512, #59875, #9235, #67306, #56124, #28841, #10757, #42850, #22669, #26662, #43636, #14150, #58245, #67886, #63566, #64169, #8090, #28055, #29312, #53101, #3852, #54291, #49329, #58290, #25315, #20326, #56893, #5918, #50349, #52859, #35125, #26920, #62069, #6605, #28794, #6212, #43698, #64448, #45109, #19762, #66757, #17774, #57719, #53524, #39631, #33472, #25395, #33663, #10906, #34822, #10273, #5936, #39707, #22740, #8048, #37736, #14291, #47654, #17260, #35206, #31568, #54966, #3030, #68664, #52200, #49705, #20217, #49138, #19068, #18822, #50927, #46938, #40267, #9083, #31114, #40955, #10544, #54811, #66249, #23424, #48814, #8548, #55181 ) ) ;
#25770 = VECTOR ( 'NONE', #42121, 1000.000000000000000 ) ;
#25771 = CARTESIAN_POINT ( 'NONE',  ( -128.4570736234661865, -9.058813317711329915, 2.943386871421371787 ) ) ;
#25772 = CARTESIAN_POINT ( 'NONE',  ( -98.45499999999998408, 7.632228543268599452, -2.479861379858951942 ) ) ;
#25773 = ORIENTED_EDGE ( 'NONE', *, *, #16727, .F. ) ;
#25774 = CARTESIAN_POINT ( 'NONE',  ( -75.00000000000000000, 33.00000000000000000, -6.500000000000000000 ) ) ;
#25775 =( NAMED_UNIT ( * ) SI_UNIT ( $, .STERADIAN. ) SOLID_ANGLE_UNIT ( ) );
#25776 = CARTESIAN_POINT ( 'NONE',  ( -128.6070736234661638, -8.102448949553172852, 5.886773742842742685 ) ) ;
#25777 = COLOUR_RGB ( '', 0.31764706, 0.68627451, 0.89019608) ;
#25778 = AXIS2_PLACEMENT_3D ( 'NONE', #34338, #55786, #7595 ) ;
#25779 = CYLINDRICAL_SURFACE ( 'NONE', #29457, 4.999999999999997335 ) ;
#25780 = CARTESIAN_POINT ( 'NONE',  ( 10.01517768586949408, 147.6949999999999932, 1.839758294383810543E-15 ) ) ;
#25781 = CARTESIAN_POINT ( 'NONE',  ( -75.20707362346614389, 3.094860106618433360, 9.524999999999991473 ) ) ;
#25782 = EDGE_CURVE ( 'NONE', #20781, #6242, #11685, .T. ) ;
#25783 = VECTOR ( 'NONE', #14554, 1000.000000000000000 ) ;
#25784 = CARTESIAN_POINT ( 'NONE',  ( -92.54292637653379927, 9.058813317711329915, 2.943386871421369566 ) ) ;
#25785 = ORIENTED_EDGE ( 'NONE', *, *, #11098, .F. ) ;
#25786 = CARTESIAN_POINT ( 'NONE',  ( -34.99999999999992895, 109.9999999999999858, -9.500000000000000000 ) ) ;
#25787 = CARTESIAN_POINT ( 'NONE',  ( -19.33312911335796969, -11.73659741771296794, -2.515642419290914145 ) ) ;
#25788 = CARTESIAN_POINT ( 'NONE',  ( -99.44292637653380496, -1.166476076187852838E-15, -9.524999999999991473 ) ) ;
#25789 = PRESENTATION_LAYER_ASSIGNMENT (  '', '', ( #48271 ) ) ;
#25790 = CARTESIAN_POINT ( 'NONE',  ( -112.2549999999999955, -4.716976649647092401, 6.492361379858946790 ) ) ;
#25791 = CARTESIAN_POINT ( 'NONE',  ( 3.094860106618431583, 117.0949999999999989, 9.525000000000000355 ) ) ;
#25792 = CARTESIAN_POINT ( 'NONE',  ( -130.4950000000000045, 6.826472737025113702, -4.959722759717902107 ) ) ;
#25793 = VECTOR ( 'NONE', #13052, 1000.000000000000000 ) ;
#25794 = STYLED_ITEM ( 'NONE', ( #50398 ), #33954 ) ;
#25795 = COLOUR_RGB ( '', 0.66274510, 0.83137255, 0.94901961) ;
#25796 = TOROIDAL_SURFACE ( 'NONE', #62838, 0.5000000000000000000, 0.2500000000000000000 ) ;
#25797 = FILL_AREA_STYLE_COLOUR ( '', #7637 ) ;
#25798 = ADVANCED_FACE ( 'NONE', ( #22595 ), #38117, .F. ) ;
#25799 = ORIENTED_EDGE ( 'NONE', *, *, #49735, .T. ) ;
#25800 = CARTESIAN_POINT ( 'NONE',  ( -164.5429263765338135, 9.058813317711329915, 2.943386871421369566 ) ) ;
#25801 = SURFACE_STYLE_FILL_AREA ( #27162 ) ;
#25802 =( NAMED_UNIT ( * ) SI_UNIT ( $, .STERADIAN. ) SOLID_ANGLE_UNIT ( ) );
#25803 = EDGE_CURVE ( 'NONE', #34770, #49320, #32991, .T. ) ;
#25804 = EDGE_CURVE ( 'NONE', #40233, #6517, #50829, .T. ) ;
#25805 = SURFACE_STYLE_USAGE ( .BOTH. , #62408 ) ;
#25806 = DIRECTION ( 'NONE',  ( 0.000000000000000000, 0.000000000000000000, 1.000000000000000000 ) ) ;
#25807 = FILL_AREA_STYLE ('',( #26496 ) ) ;
#25808 = ORIENTED_EDGE ( 'NONE', *, *, #47413, .T. ) ;
#25809 = CARTESIAN_POINT ( 'NONE',  ( -90.59292637653381064, -3.094860106618431139, -9.524999999999991473 ) ) ;
#25810 = ITEM_DEFINED_TRANSFORMATION ( 'NONE', 'NONE', #51752,  #42840 ) ;
#25811 = FACE_OUTER_BOUND ( 'NONE', #14340, .T. ) ;
#25812 = EDGE_CURVE ( 'NONE', #20191, #13722, #58839, .T. ) ;
#25813 = DIRECTION ( 'NONE',  ( 1.000000000000000000, 0.000000000000000000, 0.000000000000000000 ) ) ;
#25814 = CARTESIAN_POINT ( 'NONE',  ( 66.74999999999998579, 36.75000000000000000, 3.750000000000000000 ) ) ;
#25815 = PRESENTATION_LAYER_ASSIGNMENT (  '', '', ( #56136 ) ) ;
#25816 = EDGE_CURVE ( 'NONE', #43736, #53241, #47513, .T. ) ;
#25817 = CARTESIAN_POINT ( 'NONE',  ( -181.4049999999999727, -2.607480562269069768, 8.024999999999991473 ) ) ;
#25818 = VERTEX_POINT ( 'NONE', #53563 ) ;
#25819 = LINE ( 'NONE', #46651, #58938 ) ;
#25820 = CARTESIAN_POINT ( 'NONE',  ( -74.15707362346617515, -9.058813317711329915, -2.943386871421370898 ) ) ;
#25821 = ORIENTED_EDGE ( 'NONE', *, *, #16246, .F. ) ;
#25822 = CARTESIAN_POINT ( 'NONE',  ( -110.2429263765338021, 5.598654528085804216, 7.705886871421366635 ) ) ;
#25823 = MECHANICAL_DESIGN_GEOMETRIC_PRESENTATION_REPRESENTATION (  '', ( #46103 ), #55038 ) ;
#25824 = DIRECTION ( 'NONE',  ( -0.000000000000000000, -0.000000000000000000, 1.000000000000000000 ) ) ;
#25825 = CARTESIAN_POINT ( 'NONE',  ( -4.716976649647097730, 145.3570736234661638, -6.492361379858953896 ) ) ;
#25826 = ORIENTED_EDGE ( 'NONE', *, *, #30630, .T. ) ;
#25827 = AXIS2_PLACEMENT_3D ( 'NONE', #11620, #65067, #33086 ) ;
#25828 = LINE ( 'NONE', #47341, #40637 ) ;
#25829 = CARTESIAN_POINT ( 'NONE',  ( -104.6049999999999898, 6.826472737025113702, -4.959722759717902107 ) ) ;
#25830 = UNCERTAINTY_MEASURE_WITH_UNIT (LENGTH_MEASURE( 1.000000000000000082E-05 ), #3612, 'distance_accuracy_value', 'NONE');
#25831 = SURFACE_STYLE_USAGE ( .BOTH. , #4348 ) ;
#25832 = ORIENTED_EDGE ( 'NONE', *, *, #8868, .F. ) ;
#25833 = DIRECTION ( 'NONE',  ( 0.000000000000000000, 0.000000000000000000, -1.000000000000000000 ) ) ;
#25834 = DIRECTION ( 'NONE',  ( -0.6216216216216311485, -0.7833176619561784682, 0.000000000000000000 ) ) ;
#25835 = ADVANCED_FACE ( 'NONE', ( #5692 ), #23904, .T. ) ;
#25836 = CARTESIAN_POINT ( 'NONE',  ( -83.90707362346614673, -3.094860106618429807, 9.524999999999991473 ) ) ;
#25837 = CARTESIAN_POINT ( 'NONE',  ( 0.000000000000000000, 42.00000000000000000, 36.50000000000000000 ) ) ;
#25838 = CIRCLE ( 'NONE', #65154, 0.2500000000000002220 ) ;
#25839 = VERTEX_POINT ( 'NONE', #21906 ) ;
#25840 = CARTESIAN_POINT ( 'NONE',  ( 24.75000000000000355, 36.75000000000000000, 3.000000000000000000 ) ) ;
#25841 = EDGE_CURVE ( 'NONE', #25004, #29393, #21549, .T. ) ;
#25842 = CARTESIAN_POINT ( 'NONE',  ( -72.59499999999998465, 2.607480562269073321, 8.024999999999991473 ) ) ;
#25844 = EDGE_LOOP ( 'NONE', ( #64522, #68249, #29526, #6520 ) ) ;
#25843 = AXIS2_PLACEMENT_3D ( 'NONE', #47247, #64058, #16267 ) ;
#25845 = LINE ( 'NONE', #30405, #31643 ) ;
#25846 = VECTOR ( 'NONE', #25714, 1000.000000000000000 ) ;
#25847 = VERTEX_POINT ( 'NONE', #56684 ) ;
#25848 = DIRECTION ( 'NONE',  ( -0.000000000000000000, -1.000000000000000000, -0.000000000000000000 ) ) ;
#25849 = CARTESIAN_POINT ( 'NONE',  ( 0.9999999999999991118, 50.00000000000000000, 60.00000000000000000 ) ) ;
#25850 = DIRECTION ( 'NONE',  ( 1.000000000000000000, 9.251858538542971828E-16, 0.000000000000000000 ) ) ;
#25851 = CARTESIAN_POINT ( 'NONE',  ( -15.98999599679679839, 118.4999999999999716, -7.500000000000000000 ) ) ;
#25852 = ORIENTED_EDGE ( 'NONE', *, *, #46548, .T. ) ;
#25853 = CARTESIAN_POINT ( 'NONE',  ( 0.000000000000000000, -3.000000000000000000, 18.00000000000000000 ) ) ;
#25854 = ORIENTED_EDGE ( 'NONE', *, *, #67014, .T. ) ;
#25855 = FACE_OUTER_BOUND ( 'NONE', #62255, .T. ) ;
#25856 = CYLINDRICAL_SURFACE ( 'NONE', #29662, 0.2500000000000002220 ) ;
#25857 = CIRCLE ( 'NONE', #15796, 0.2500000000000002220 ) ;
#25858 = CARTESIAN_POINT ( 'NONE',  ( -160.7070736234661865, -3.094860106618431139, -9.524999999999991473 ) ) ;
#25859 =( GEOMETRIC_REPRESENTATION_CONTEXT ( 3 ) GLOBAL_UNCERTAINTY_ASSIGNED_CONTEXT ( ( #62925 ) ) GLOBAL_UNIT_ASSIGNED_CONTEXT ( ( #18196, #17857, #33341 ) ) REPRESENTATION_CONTEXT ( 'NONE', 'WORKASPACE' ) );
#25860 = CARTESIAN_POINT ( 'NONE',  ( -9.058813317711338797, 119.3449999999999989, 2.943386871421373563 ) ) ;
#25861 = CARTESIAN_POINT ( 'NONE',  ( -104.7570736234661695, -5.598654528085801552, 7.705886871421367523 ) ) ;
#25862 = ORIENTED_EDGE ( 'NONE', *, *, #29960, .F. ) ;
#25863 = AXIS2_PLACEMENT_3D ( 'NONE', #68129, #40351, #41409 ) ;
#25865 = DIRECTION ( 'NONE',  ( -0.000000000000000000, -1.000000000000000000, -0.000000000000000000 ) ) ;
#25864 = CARTESIAN_POINT ( 'NONE',  ( -12.34222745343792127, 114.9999999999999574, 10.18181818181818166 ) ) ;
#25866 = CARTESIAN_POINT ( 'NONE',  ( -135.9549999999999841, -7.632228543268599452, 2.479861379858951054 ) ) ;
#25867 = CARTESIAN_POINT ( 'NONE',  ( 15.48999599679679662, 117.9999999999999716, -7.500000000000000000 ) ) ;
#25868 = CARTESIAN_POINT ( 'NONE',  ( 21.25000000000001066, 24.74999999999998224, 4.000000000000000000 ) ) ;
#25869 = EDGE_CURVE ( 'NONE', #51601, #4575, #5912, .T. ) ;
#25870 = CARTESIAN_POINT ( 'NONE',  ( -156.1450000000000102, -4.716976649647092401, 6.492361379858946790 ) ) ;
#25871 = CARTESIAN_POINT ( 'NONE',  ( -136.9449999999999932, -9.827790563157499189E-16, -8.024999999999991473 ) ) ;
#25872 = CIRCLE ( 'NONE', #38282, 18.50000000000000355 ) ;
#25873 = EDGE_LOOP ( 'NONE', ( #20396, #59125, #18698, #39887 ) ) ;
#25874 = FACE_OUTER_BOUND ( 'NONE', #62724, .T. ) ;
#25875 = AXIS2_PLACEMENT_3D ( 'NONE', #37279, #215, #47858 ) ;
#25876 = EDGE_CURVE ( 'NONE', #12107, #9513, #60941, .T. ) ;
#25878 = CIRCLE ( 'NONE', #61980, 23.00000000000000000 ) ;
#25877 = DIRECTION ( 'NONE',  ( 1.000000000000000000, 0.000000000000000000, 0.000000000000000000 ) ) ;
#25879 = CARTESIAN_POINT ( 'NONE',  ( -50.15499999999997982, 7.632228543268600340, 2.479861379858949277 ) ) ;
#25880 = LINE ( 'NONE', #67773, #13509 ) ;
#25881 = ADVANCED_FACE ( 'NONE', ( #23285 ), #45810, .F. ) ;
#25882 = CARTESIAN_POINT ( 'NONE',  ( 9.058813317711337021, 151.6549999999999727, 2.943386871421375783 ) ) ;
#25883 = CARTESIAN_POINT ( 'NONE',  ( -52.34292637653378932, -9.058813317711329915, 2.943386871421371787 ) ) ;
#25884 = CIRCLE ( 'NONE', #65201, 8.000000000000000000 ) ;
#25885 = STYLED_ITEM ( 'NONE', ( #4848 ), #11468 ) ;
#25886 = PRESENTATION_LAYER_ASSIGNMENT (  '', '', ( #55055 ) ) ;
#25887 = SURFACE_STYLE_FILL_AREA ( #4412 ) ;
#25888 = CONICAL_SURFACE ( 'NONE', #45029, 7.000000000000000888, 0.7853981633974500554 ) ;
#25889 = CARTESIAN_POINT ( 'NONE',  ( -81.80707362346616662, 10.01517768586948698, -1.839758294383808966E-15 ) ) ;
#25890 = DIRECTION ( 'NONE',  ( 0.000000000000000000, 0.000000000000000000, -1.000000000000000000 ) ) ;
#25891 = MECHANICAL_DESIGN_GEOMETRIC_PRESENTATION_REPRESENTATION (  '', ( #12431 ), #29255 ) ;
#25892 = EDGE_CURVE ( 'NONE', #44595, #43189, #33992, .T. ) ;
#25893 = CARTESIAN_POINT ( 'NONE',  ( -4.500000000000002665, 24.74999999999998579, -3.750000000000000000 ) ) ;
#25894 = CARTESIAN_POINT ( 'NONE',  ( -28.91790128120562997, -7.668906119302852709, -0.3459828814411498032 ) ) ;
#25895 = CARTESIAN_POINT ( 'NONE',  ( 0.000000000000000000, 114.9999999999999574, 0.000000000000000000 ) ) ;
#25896 = FACE_OUTER_BOUND ( 'NONE', #67149, .T. ) ;
#25897 = ORIENTED_EDGE ( 'NONE', *, *, #6761, .T. ) ;
#25898 = VERTEX_POINT ( 'NONE', #28881 ) ;
#25899 = PRESENTATION_STYLE_ASSIGNMENT (( #64227 ) ) ;
#25900 = CARTESIAN_POINT ( 'NONE',  ( 2.418047948276647041, -2.101261491285135286, -7.000000000000002665 ) ) ;
#25901 = PRODUCT_DEFINITION_FORMATION_WITH_SPECIFIED_SOURCE ( 'ANY', '', #47375, .NOT_KNOWN. ) ;
#25902 = CYLINDRICAL_SURFACE ( 'NONE', #63000, 0.2500000000000002220 ) ;
#25903 = LINE ( 'NONE', #48110, #15988 ) ;
#25904 = VERTEX_POINT ( 'NONE', #65853 ) ;
#25905 = ORIENTED_EDGE ( 'NONE', *, *, #30461, .F. ) ;
#25906 = CYLINDRICAL_SURFACE ( 'NONE', #3966, 0.2500000000000002220 ) ;
#25907 =( LENGTH_UNIT ( ) NAMED_UNIT ( * ) SI_UNIT ( .MILLI., .METRE. ) );
#25908 = CARTESIAN_POINT ( 'NONE',  ( 1.189524669241243060E-16, -7.500000000000000888, 23.00000000000000000 ) ) ;
#25909 = ORIENTED_EDGE ( 'NONE', *, *, #64239, .F. ) ;
#25910 = CARTESIAN_POINT ( 'NONE',  ( -3.094860106618434248, 120.9049999999999869, 9.525000000000000355 ) ) ;
#25911 = VECTOR ( 'NONE', #11012, 1000.000000000000000 ) ;
#25912 = DIRECTION ( 'NONE',  ( 5.782411586589351722E-16, -1.000000000000000000, -0.000000000000000000 ) ) ;
#25913 = CARTESIAN_POINT ( 'NONE',  ( -102.8949999999999960, 6.826472737025116366, 4.959722759717898555 ) ) ;
#25914 = ORIENTED_EDGE ( 'NONE', *, *, #21511, .T. ) ;
#25915 = DIRECTION ( 'NONE',  ( 0.000000000000000000, 0.5877852522924733591, -0.8090169943749472292 ) ) ;
#25916 = PRESENTATION_LAYER_ASSIGNMENT (  '', '', ( #4586 ) ) ;
#25917 = VECTOR ( 'NONE', #3425, 1000.000000000000000 ) ;
#25918 = SURFACE_STYLE_USAGE ( .BOTH. , #37927 ) ;
#25919 = ORIENTED_EDGE ( 'NONE', *, *, #53695, .T. ) ;
#25920 = CARTESIAN_POINT ( 'NONE',  ( -9.827790563157511022E-16, 154.4429263765338192, 8.025000000000000355 ) ) ;
#25921 =( BOUNDED_CURVE ( )  B_SPLINE_CURVE ( 2, ( #35757, #19566, #57554, #4772, #31847, #36493, #3699, #63518, #58247, #9382, #53335 ),
 .UNSPECIFIED., .F., .F. ) 
 B_SPLINE_CURVE_WITH_KNOTS ( ( 3, 2, 2, 2, 2, 3 ),
 ( 0.01086956521739105945, 0.01304347826086927134, 0.01521739130434748496, 0.01739130434782569512, 0.01956521739130390874, 0.02173913043478211890 ),
 .UNSPECIFIED. ) 
 CURVE ( )  GEOMETRIC_REPRESENTATION_ITEM ( )  RATIONAL_B_SPLINE_CURVE ( ( 1.000000000000005551, 0.9510565162951480911, 1.000000000000000000, 0.9510565162951535312, 1.000000000000000000, 0.9510565162951535312, 1.000000000000000000, 0.9510565162951535312, 1.000000000000000000, 0.9510565162951645224, 0.9999999999999890088 ) ) 
 REPRESENTATION_ITEM ( '' )  );
#25922 = AXIS2_PLACEMENT_3D ( 'NONE', #27678, #17536, #54434 ) ;
#25923 = DIRECTION ( 'NONE',  ( 0.000000000000000000, 0.000000000000000000, -1.000000000000000000 ) ) ;
#25924 = ORIENTED_EDGE ( 'NONE', *, *, #67353, .T. ) ;
#25925 = CIRCLE ( 'NONE', #55146, 0.5000000000000004441 ) ;
#25926 = CARTESIAN_POINT ( 'NONE',  ( 20.58979310427664444, 114.8389001175783051, -9.999999999999879208 ) ) ;
#25927 = VERTEX_POINT ( 'NONE', #45126 ) ;
#25928 = PRESENTATION_STYLE_ASSIGNMENT (( #63236 ) ) ;
#25929 = CARTESIAN_POINT ( 'NONE',  ( 57.00000000000000000, 16.00000000000000000, 55.00402776293826435 ) ) ;
#25930 = FACE_OUTER_BOUND ( 'NONE', #27556, .T. ) ;
#25931 = FACE_OUTER_BOUND ( 'NONE', #15188, .T. ) ;
#25932 = CARTESIAN_POINT ( 'NONE',  ( -184.0000000000000853, -6.613845720572140152, 4.561563678776720643 ) ) ;
#25933 = AXIS2_PLACEMENT_3D ( 'NONE', #36446, #14246, #20201 ) ;
#25934 = CARTESIAN_POINT ( 'NONE',  ( 69.99999999999998579, 8.572527594031471415E-15, 4.000000000000000000 ) ) ;
#25935 = AXIS2_PLACEMENT_3D ( 'NONE', #51962, #9754, #19586 ) ;
#25936 = CARTESIAN_POINT ( 'NONE',  ( -4.716976649647097730, 120.2429263765338163, -6.492361379858953896 ) ) ;
#25937 = DIRECTION ( 'NONE',  ( 0.000000000000000000, 0.000000000000000000, 1.000000000000000000 ) ) ;
#25938 = ORIENTED_EDGE ( 'NONE', *, *, #52333, .F. ) ;
#25939 = EDGE_LOOP ( 'NONE', ( #14480, #46565, #1899, #54616, #48717, #36897 ) ) ;
#25940 = DIRECTION ( 'NONE',  ( -1.000000000000000000, 0.000000000000000000, 0.000000000000000000 ) ) ;
#25941 = SURFACE_STYLE_FILL_AREA ( #30518 ) ;
#25942 = CARTESIAN_POINT ( 'NONE',  ( -181.9429263765338192, 0.000000000000000000, 9.524999999999991473 ) ) ;
#25943 = DIRECTION ( 'NONE',  ( -0.000000000000000000, -1.000000000000000000, -0.000000000000000000 ) ) ;
#25944 = VERTEX_POINT ( 'NONE', #2821 ) ;
#25945 = FILL_AREA_STYLE ('',( #4130 ) ) ;
#25946 = CARTESIAN_POINT ( 'NONE',  ( -167.7549999999999955, 4.716976649647091513, -6.492361379858946790 ) ) ;
#25947 = CARTESIAN_POINT ( 'NONE',  ( -11.24540022918535698, 52.49282396394303873, -2.000000000000000000 ) ) ;
#25948 = CARTESIAN_POINT ( 'NONE',  ( -147.2070736234666697, 3.094860106625827445, 9.524999999994619770 ) ) ;
#25949 = AXIS2_PLACEMENT_3D ( 'NONE', #13650, #1986, #23506 ) ;
#25950 = EDGE_CURVE ( 'NONE', #22828, #51066, #17686, .T. ) ;
#25951 = CARTESIAN_POINT ( 'NONE',  ( -183.2949999999999307, -2.607480562269069768, 8.024999999999991473 ) ) ;
#25952 = CARTESIAN_POINT ( 'NONE',  ( -178.9449999999999932, -9.827790563157499189E-16, -8.024999999999991473 ) ) ;
#25953 = VERTEX_POINT ( 'NONE', #29593 ) ;
#25954 = CARTESIAN_POINT ( 'NONE',  ( 0.000000000000000000, -2.500000000000000000, 9.000000000000000000 ) ) ;
#25955 = DIRECTION ( 'NONE',  ( -1.000000000000000000, 0.000000000000000000, 0.000000000000000000 ) ) ;
#25956 = CARTESIAN_POINT ( 'NONE',  ( -92.75499999999999545, 4.716976649647091513, -6.492361379858946790 ) ) ;
#25957 = DIRECTION ( 'NONE',  ( 1.000000000000000000, 0.000000000000000000, 0.000000000000000000 ) ) ;
#25958 = VECTOR ( 'NONE', #69636, 1000.000000000000000 ) ;
#25959 = EDGE_CURVE ( 'NONE', #22693, #19997, #12358, .T. ) ;
#25960 = CARTESIAN_POINT ( 'NONE',  ( -87.74499999999999034, 4.716976649647094177, 6.492361379858945902 ) ) ;
#25961 = CARTESIAN_POINT ( 'NONE',  ( 9.058813317711338797, 127.9549999999999841, -2.943386871421372675 ) ) ;
#25962 = CARTESIAN_POINT ( 'NONE',  ( -59.69499999999997897, -8.437984349512085203, 5.166775262442717831E-16 ) ) ;
#25963 = ADVANCED_FACE ( 'NONE', ( #7107 ), #53095, .T. ) ;
#25964 = DIRECTION ( 'NONE',  ( 0.000000000000000000, 1.000000000000000000, 0.000000000000000000 ) ) ;
#25965 = CARTESIAN_POINT ( 'NONE',  ( -170.2429263765338305, 5.598654528085804216, 7.705886871421366635 ) ) ;
#25966 = PRESENTATION_LAYER_ASSIGNMENT (  '', '', ( #9184 ) ) ;
#25967 = EDGE_CURVE ( 'NONE', #28083, #12316, #50367, .T. ) ;
#25968 = CARTESIAN_POINT ( 'NONE',  ( -7.794228634059947147, -2.500000000000000000, -4.500000000000000000 ) ) ;
#25969 = DIRECTION ( 'NONE',  ( 0.000000000000000000, 0.000000000000000000, -1.000000000000000000 ) ) ;
#25970 =( NAMED_UNIT ( * ) SI_UNIT ( $, .STERADIAN. ) SOLID_ANGLE_UNIT ( ) );
#25972 = ORIENTED_EDGE ( 'NONE', *, *, #10731, .F. ) ;
#25971 = VECTOR ( 'NONE', #60683, 1000.000000000000000 ) ;
#25973 = ADVANCED_FACE ( 'NONE', ( #15528 ), #14949, .T. ) ;
#25974 = PRODUCT ( '1. Base', '1. Base', '', ( #45914 ) ) ;
#25975 = CARTESIAN_POINT ( 'NONE',  ( 23.50000000000001776, -3.148064030671221758, -29.68999999999999417 ) ) ;
#25976 =( GEOMETRIC_REPRESENTATION_CONTEXT ( 3 ) GLOBAL_UNCERTAINTY_ASSIGNED_CONTEXT ( ( #34178 ) ) GLOBAL_UNIT_ASSIGNED_CONTEXT ( ( #19106, #30022, #46248 ) ) REPRESENTATION_CONTEXT ( 'NONE', 'WORKASPACE' ) );
#25977 = EDGE_CURVE ( 'NONE', #28945, #44738, #66590, .T. ) ;
#25979 = LINE ( 'NONE', #42559, #59537 ) ;
#25978 = CARTESIAN_POINT ( 'NONE',  ( -40.99999999999997868, 10.49999999999998401, 3.500000000000000000 ) ) ;
#25980 = CARTESIAN_POINT ( 'NONE',  ( 71.99999999999998579, 64.07124727947029896, 7.500000000000000000 ) ) ;
#25981 = ORIENTED_EDGE ( 'NONE', *, *, #33451, .T. ) ;
#25982 = ORIENTED_EDGE ( 'NONE', *, *, #54155, .F. ) ;
#25983 = DIRECTION ( 'NONE',  ( 1.000000000000000000, 0.000000000000000000, 0.000000000000000000 ) ) ;
#25984 = VECTOR ( 'NONE', #63806, 1000.000000000000000 ) ;
#25985 = CARTESIAN_POINT ( 'NONE',  ( -134.2429263765338305, 5.598654528085804216, 7.705886871421366635 ) ) ;
#25986 = VECTOR ( 'NONE', #24492, 1000.000000000000000 ) ;
#25987 = DIRECTION ( 'NONE',  ( -1.000000000000000000, 0.000000000000000000, 0.000000000000000000 ) ) ;
#25988 =( GEOMETRIC_REPRESENTATION_CONTEXT ( 3 ) GLOBAL_UNCERTAINTY_ASSIGNED_CONTEXT ( ( #57391 ) ) GLOBAL_UNIT_ASSIGNED_CONTEXT ( ( #33937, #12474, #49791 ) ) REPRESENTATION_CONTEXT ( 'NONE', 'WORKASPACE' ) );
#25989 = PRESENTATION_STYLE_ASSIGNMENT (( #36944 ) ) ;
#25990 = DIRECTION ( 'NONE',  ( 0.000000000000000000, -1.000000000000000000, 0.000000000000000000 ) ) ;
#25991 = EDGE_LOOP ( 'NONE', ( #59750, #24231, #45119, #6738, #4533, #44812, #62250, #51024, #10631, #8313, #25419, #28561, #63334 ) ) ;
#25992 = CARTESIAN_POINT ( 'NONE',  ( -117.6550000000000011, -7.632228543268600340, -2.479861379858950166 ) ) ;
#25993 = ORIENTED_EDGE ( 'NONE', *, *, #6076, .F. ) ;
#25994 = CARTESIAN_POINT ( 'NONE',  ( 34.99999999999999289, 99.99999999999997158, 10.00000000000000000 ) ) ;
#25995 = CARTESIAN_POINT ( 'NONE',  ( 2.607480562269093305, 128.7070736234661865, 8.024999999999986144 ) ) ;
#25996 = ORIENTED_EDGE ( 'NONE', *, *, #20248, .T. ) ;
#25997 = CARTESIAN_POINT ( 'NONE',  ( 23.21231517720797655, 117.4999999999999716, 9.500000000000000000 ) ) ;
#25998 = EDGE_LOOP ( 'NONE', ( #15108, #15862, #61465, #6018 ) ) ;
#25999 = PRESENTATION_LAYER_ASSIGNMENT (  '', '', ( #12541 ) ) ;
#26000 = CARTESIAN_POINT ( 'NONE',  ( 8.102448949553181734, 147.3950000000000102, 5.886773742842750679 ) ) ;
#26001 = CARTESIAN_POINT ( 'NONE',  ( 33.00000000000002132, 13.00000000000000178, 80.00402776293826435 ) ) ;
#26002 = VECTOR ( 'NONE', #68753, 1000.000000000000000 ) ;
#26003 = VERTEX_POINT ( 'NONE', #47210 ) ;
#26004 = VECTOR ( 'NONE', #20321, 1000.000000000000000 ) ;
#26005 = CARTESIAN_POINT ( 'NONE',  ( 3.094860106618431583, 154.2049999999999272, 9.525000000000000355 ) ) ;
#26006 =( NAMED_UNIT ( * ) SI_UNIT ( $, .STERADIAN. ) SOLID_ANGLE_UNIT ( ) );
#26007 = CARTESIAN_POINT ( 'NONE',  ( 48.00000000000000000, 99.99999999999992895, -9.500000000000000000 ) ) ;
#26008 = ORIENTED_EDGE ( 'NONE', *, *, #43959, .F. ) ;
#26009 = CARTESIAN_POINT ( 'NONE',  ( -2.607480562269073765, 129.0929263765338249, -8.025000000000000355 ) ) ;
#26010 = CARTESIAN_POINT ( 'NONE',  ( -8.082903768654761123, 2.500000000000000000, -1.781658826789683271E-15 ) ) ;
#26011 = CIRCLE ( 'NONE', #37363, 8.525000000000000355 ) ;
#26012 = DIRECTION ( 'NONE',  ( -1.000000000000000000, 0.000000000000000000, 0.000000000000000000 ) ) ;
#26013 = DIRECTION ( 'NONE',  ( 0.6842105263157866046, -0.7292845505553195995, 0.000000000000000000 ) ) ;
#26014 = ORIENTED_EDGE ( 'NONE', *, *, #38403, .T. ) ;
#26015 = DIRECTION ( 'NONE',  ( -0.000000000000000000, 1.000000000000000000, -0.000000000000000000 ) ) ;
#26016 = EDGE_LOOP ( 'NONE', ( #69553, #14322, #60175, #19903 ) ) ;
#26017 = CARTESIAN_POINT ( 'NONE',  ( -54.29292637653379927, 3.094860106618428031, -9.524999999999993250 ) ) ;
#26018 = CARTESIAN_POINT ( 'NONE',  ( -4.682380833558966948, -5.889878495889163013, 0.4967607073414698760 ) ) ;
#26020 = CARTESIAN_POINT ( 'NONE',  ( -154.8549999999999898, 4.716976649647094177, 6.492361379858945902 ) ) ;
#26019 = STYLED_ITEM ( 'NONE', ( #41869 ), #60505 ) ;
#26021 = EDGE_LOOP ( 'NONE', ( #28858, #44502, #55637, #48906 ) ) ;
#26022 = COLOUR_RGB ( '', 0.31764706, 0.68627451, 0.89019608) ;
#26023 = VECTOR ( 'NONE', #33589, 1000.000000000000000 ) ;
#26024 = CARTESIAN_POINT ( 'NONE',  ( 57.49999999999999289, 27.99999999999998934, 3.750000000000000000 ) ) ;
#26025 = CARTESIAN_POINT ( 'NONE',  ( 74.99999999999998579, 19.84496280275742564, 6.370902851337289619 ) ) ;
#26026 = CYLINDRICAL_SURFACE ( 'NONE', #47788, 1.000000000000000888 ) ;
#26027 = B_SPLINE_CURVE_WITH_KNOTS ( 'NONE', 1,
 ( #13402, #57018 ),
 .UNSPECIFIED., .F., .F.,
 ( 2, 2 ),
 ( 0.000000000000000000, 1.000000000000000000 ),
 .UNSPECIFIED. ) ;
#26028 = ORIENTED_EDGE ( 'NONE', *, *, #5783, .F. ) ;
#26029 = AXIS2_PLACEMENT_3D ( 'NONE', #43547, #39286, #16457 ) ;
#26030 = ORIENTED_EDGE ( 'NONE', *, *, #42705, .T. ) ;
#26031 = CARTESIAN_POINT ( 'NONE',  ( 22.49375942073035617, 25.15171118985935550, 27.39868845849637324 ) ) ;
#26032 = VECTOR ( 'NONE', #15877, 1000.000000000000000 ) ;
#26033 =( NAMED_UNIT ( * ) SI_UNIT ( $, .STERADIAN. ) SOLID_ANGLE_UNIT ( ) );
#26034 = CARTESIAN_POINT ( 'NONE',  ( -64.55499999999999261, 0.000000000000000000, 8.024999999999991473 ) ) ;
#26035 = ORIENTED_EDGE ( 'NONE', *, *, #54561, .T. ) ;
#26036 = DIRECTION ( 'NONE',  ( 0.000000000000000000, 0.000000000000000000, -1.000000000000000000 ) ) ;
#26037 = DIRECTION ( 'NONE',  ( 0.000000000000000000, -1.000000000000000000, 0.000000000000000000 ) ) ;
#26038 = AXIS2_PLACEMENT_3D ( 'NONE', #52663, #15729, #43536 ) ;
#26039 = EDGE_CURVE ( 'NONE', #14945, #58906, #50877, .T. ) ;
#26040 = CARTESIAN_POINT ( 'NONE',  ( -91.10707362346617799, 8.102448949553172852, -5.886773742842744461 ) ) ;
#26041 = DIRECTION ( 'NONE',  ( -1.000000000000000000, 0.000000000000000000, -0.000000000000000000 ) ) ;
#26043 = ADVANCED_FACE ( 'NONE', ( #67950 ), #12703, .F. ) ;
#26042 = ORIENTED_EDGE ( 'NONE', *, *, #58964, .T. ) ;
#26044 = CIRCLE ( 'NONE', #65363, 0.2500000000000002220 ) ;
#26045 = DIRECTION ( 'NONE',  ( 0.000000000000000000, 0.000000000000000000, -1.000000000000000000 ) ) ;
#26046 = CARTESIAN_POINT ( 'NONE',  ( 59.00000000000000000, 11.99999999999999822, 4.000000000000000000 ) ) ;
#26047 = SURFACE_STYLE_FILL_AREA ( #4589 ) ;
#26048 = CIRCLE ( 'NONE', #22541, 0.2500000000000002220 ) ;
#26050 = CARTESIAN_POINT ( 'NONE',  ( 1.000000000000000000, 36.74999999999999289, -4.000000000000000000 ) ) ;
#26049 = DIRECTION ( 'NONE',  ( -1.000000000000000000, -0.000000000000000000, -0.000000000000000000 ) ) ;
#26051 = EDGE_CURVE ( 'NONE', #54496, #55122, #54230, .T. ) ;
#26052 = CIRCLE ( 'NONE', #65375, 4.999999999999997335 ) ;
#26053 = CARTESIAN_POINT ( 'NONE',  ( -124.0449999999999875, 7.632228543268600340, 2.479861379858949277 ) ) ;
#26054 = CARTESIAN_POINT ( 'NONE',  ( -9.058813317711337021, 149.0449999999999875, -2.943386871421374895 ) ) ;
#26055 = CARTESIAN_POINT ( 'NONE',  ( -92.69499999999996476, -8.437984349512085203, 5.166775262442717831E-16 ) ) ;
#26056 = EDGE_CURVE ( 'NONE', #52256, #27282, #58764, .T. ) ;
#26057 = CARTESIAN_POINT ( 'NONE',  ( -58.75000000000000000, -8.499999999999992895, 15.00000000000000178 ) ) ;
#26058 = CARTESIAN_POINT ( 'NONE',  ( 29.00000000000002842, 35.42594141563417054, 80.00402776293826435 ) ) ;
#26059 =( BOUNDED_CURVE ( )  B_SPLINE_CURVE ( 2, ( #39103, #49989, #28482, #61210, #65803, #45081, #34131, #27782, #60172, #34476, #60850 ),
 .UNSPECIFIED., .F., .F. ) 
 B_SPLINE_CURVE_WITH_KNOTS ( ( 3, 2, 2, 2, 2, 3 ),
 ( 0.3695652173912956084, 0.3717391304347738568, 0.3739130434782520496, 0.3760869565217301869, 0.3782608695652083797, 0.3804347826086866280 ),
 .UNSPECIFIED. ) 
 CURVE ( )  GEOMETRIC_REPRESENTATION_ITEM ( )  RATIONAL_B_SPLINE_CURVE ( ( 1.000000000000196287, 0.9510565162949573548, 1.000000000000000000, 0.9510565162951535312, 1.000000000000000000, 0.9510565162951535312, 1.000000000000000000, 0.9510565162951535312, 1.000000000000000000, 0.9510565162953572571, 0.9999999999997962741 ) ) 
 REPRESENTATION_ITEM ( '' )  );
#26060 = MECHANICAL_DESIGN_GEOMETRIC_PRESENTATION_REPRESENTATION (  '', ( #57555 ), #65384 ) ;
#26061 = VERTEX_POINT ( 'NONE', #35583 ) ;
#26062 = EDGE_CURVE ( 'NONE', #24423, #51540, #2566, .T. ) ;
#26063 = CARTESIAN_POINT ( 'NONE',  ( -132.5929263765337964, -3.094860106618431139, -9.524999999999991473 ) ) ;
#26064 = CARTESIAN_POINT ( 'NONE',  ( -195.0000000000000000, 0.000000000000000000, 0.000000000000000000 ) ) ;
#26065 = CARTESIAN_POINT ( 'NONE',  ( -157.0449999999999875, 7.632228543268600340, 2.479861379858949277 ) ) ;
#26066 = DIRECTION ( 'NONE',  ( 0.000000000000000000, 0.000000000000000000, -1.000000000000000000 ) ) ;
#26067 = AXIS2_PLACEMENT_3D ( 'NONE', #5085, #3663, #52947 ) ;
#26068 = DIRECTION ( 'NONE',  ( 0.000000000000000000, -1.000000000000000000, 0.000000000000000000 ) ) ;
#26069 = ORIENTED_EDGE ( 'NONE', *, *, #58695, .F. ) ;
#26070 = VERTEX_POINT ( 'NONE', #19734 ) ;
#26071 = SURFACE_SIDE_STYLE ('',( #16262 ) ) ;
#26072 = AXIS2_PLACEMENT_3D ( 'NONE', #11316, #6720, #12009 ) ;
#26073 = AXIS2_PLACEMENT_3D ( 'NONE', #65068, #17284, #38750 ) ;
#26074 = CARTESIAN_POINT ( 'NONE',  ( -7.632228543268607446, 117.5429263765338135, -2.479861379858953718 ) ) ;
#26075 = CARTESIAN_POINT ( 'NONE',  ( -45.00000000000000000, 9.291225313367151628, 6.640072787442719005 ) ) ;
#26076 = CARTESIAN_POINT ( 'NONE',  ( -130.1070736234661922, 8.102448949553172852, -5.886773742842744461 ) ) ;
#26077 = CIRCLE ( 'NONE', #31706, 1.000000000000000888 ) ;
#26078 = CARTESIAN_POINT ( 'NONE',  ( -58.07111477172493608, -7.714422322210367611, -0.5225021303434840281 ) ) ;
#26079 = EDGE_LOOP ( 'NONE', ( #33140, #46948, #9227, #2724 ) ) ;
#26080 = CARTESIAN_POINT ( 'NONE',  ( -150.3549999999999898, -4.716976649647093289, -6.492361379858945902 ) ) ;
#26081 = EDGE_LOOP ( 'NONE', ( #37356, #35701, #57336 ) ) ;
#26082 = DIRECTION ( 'NONE',  ( -1.000000000000000000, 0.000000000000000000, 0.000000000000000000 ) ) ;
#26083 = VECTOR ( 'NONE', #47969, 1000.000000000000000 ) ;
#26084 = ORIENTED_EDGE ( 'NONE', *, *, #11167, .T. ) ;
#26085 = AXIS2_PLACEMENT_3D ( 'NONE', #35463, #31187, #4100 ) ;
#26086 = CYLINDRICAL_SURFACE ( 'NONE', #68048, 0.2500000000000002220 ) ;
#26087 = CARTESIAN_POINT ( 'NONE',  ( 5.598654528085805993, 120.2449999999999903, 7.705886871421374629 ) ) ;
#26088 = LINE ( 'NONE', #38078, #26083 ) ;
#26089 = EDGE_CURVE ( 'NONE', #50403, #26109, #27284, .T. ) ;
#26090 = COLOUR_RGB ( '', 0.08235294, 0.09019608, 0.10196078) ;
#26091 = ORIENTED_EDGE ( 'NONE', *, *, #17862, .T. ) ;
#26092 = CARTESIAN_POINT ( 'NONE',  ( -58.94292637653381206, 0.000000000000000000, 9.524999999999991473 ) ) ;
#26093 = CARTESIAN_POINT ( 'NONE',  ( -9.058813317711338797, 120.4549999999999983, 2.943386871421373563 ) ) ;
#26094 = CARTESIAN_POINT ( 'NONE',  ( -63.50499999999998124, -6.826472737025113702, -4.959722759717900331 ) ) ;
#26095 = CARTESIAN_POINT ( 'NONE',  ( -80.90707362346616094, -3.094860106618429807, 9.524999999999991473 ) ) ;
#26096 = ORIENTED_EDGE ( 'NONE', *, *, #334, .F. ) ;
#26097 = CARTESIAN_POINT ( 'NONE',  ( 3.094860106618435136, 149.4049999999999443, -9.525000000000000355 ) ) ;
#26098 = CARTESIAN_POINT ( 'NONE',  ( 6.999798566743336004, 53.02677333163759243, 6.907879333238360786 ) ) ;
#26099 = CARTESIAN_POINT ( 'NONE',  ( -41.45364736693642982, 107.0151787721003842, 3.500000000000000444 ) ) ;
#26100 =( GEOMETRIC_REPRESENTATION_CONTEXT ( 3 ) GLOBAL_UNCERTAINTY_ASSIGNED_CONTEXT ( ( #3178 ) ) GLOBAL_UNIT_ASSIGNED_CONTEXT ( ( #48494, #12179, #37948 ) ) REPRESENTATION_CONTEXT ( 'NONE', 'WORKASPACE' ) );
#26101 = SPHERICAL_SURFACE ( 'NONE', #22792, 0.5000000000000000000 ) ;
#26102 = ORIENTED_EDGE ( 'NONE', *, *, #36879, .F. ) ;
#26103 =( NAMED_UNIT ( * ) SI_UNIT ( $, .STERADIAN. ) SOLID_ANGLE_UNIT ( ) );
#26104 = CYLINDRICAL_SURFACE ( 'NONE', #64354, 5.000000000000004441 ) ;
#26105 = CARTESIAN_POINT ( 'NONE',  ( -176.7549999999999955, 4.716976649647091513, -6.492361379858946790 ) ) ;
#26106 = ORIENTED_EDGE ( 'NONE', *, *, #37229, .T. ) ;
#26107 = CARTESIAN_POINT ( 'NONE',  ( 5.461490429277590763, 111.1023334488693735, 7.076668351203547758 ) ) ;
#26108 = CARTESIAN_POINT ( 'NONE',  ( -60.00000000000000000, -2.024042244987997205E-14, -11.50000000000000000 ) ) ;
#26109 = VERTEX_POINT ( 'NONE', #41228 ) ;
#26110 = DIRECTION ( 'NONE',  ( 0.000000000000000000, 0.000000000000000000, 1.000000000000000000 ) ) ;
#26111 = CARTESIAN_POINT ( 'NONE',  ( -40.99999999999997868, 10.49999999999998224, -3.000000000000000444 ) ) ;
#26112 = VERTEX_POINT ( 'NONE', #20790 ) ;
#26113 = VECTOR ( 'NONE', #58480, 1000.000000000000000 ) ;
#26114 = CARTESIAN_POINT ( 'NONE',  ( -127.5570736234661950, -1.166476076187852838E-15, -9.524999999999991473 ) ) ;
#26115 = ADVANCED_FACE ( 'NONE', ( #62629 ), #46879, .F. ) ;
#26116 = FILL_AREA_STYLE_COLOUR ( '', #60575 ) ;
#26117 = CARTESIAN_POINT ( 'NONE',  ( -92.45499999999998408, 7.632228543268599452, -2.479861379858951942 ) ) ;
#26118 = ORIENTED_EDGE ( 'NONE', *, *, #57202, .T. ) ;
#26119 = EDGE_CURVE ( 'NONE', #64812, #57523, #28385, .T. ) ;
#26120 = DIRECTION ( 'NONE',  ( 0.000000000000000000, 1.000000000000000000, 0.000000000000000000 ) ) ;
#26121 = CYLINDRICAL_SURFACE ( 'NONE', #16791, 1.000000000000000888 ) ;
#26122 = CARTESIAN_POINT ( 'NONE',  ( -134.6070736234661638, -8.102448949553172852, 5.886773742842742685 ) ) ;
#26123 = STYLED_ITEM ( 'NONE', ( #7098 ), #47136 ) ;
#26124 =( GEOMETRIC_REPRESENTATION_CONTEXT ( 3 ) GLOBAL_UNCERTAINTY_ASSIGNED_CONTEXT ( ( #46811 ) ) GLOBAL_UNIT_ASSIGNED_CONTEXT ( ( #27617, #12845, #66671 ) ) REPRESENTATION_CONTEXT ( 'NONE', 'WORKASPACE' ) );
#26125 = CARTESIAN_POINT ( 'NONE',  ( 10.01517768586949408, 150.6949999999999648, 1.839758294383810543E-15 ) ) ;
#26126 = CARTESIAN_POINT ( 'NONE',  ( -74.30707362346615241, -10.01517768586948698, 6.132527647946031529E-16 ) ) ;
#26127 = ADVANCED_FACE ( 'NONE', ( #68984 ), #64023, .T. ) ;
#26128 = CARTESIAN_POINT ( 'NONE',  ( 34.99999999999999289, 99.99999999999998579, -9.500000000000000000 ) ) ;
#26129 = ORIENTED_EDGE ( 'NONE', *, *, #30147, .T. ) ;
#26130 = DIRECTION ( 'NONE',  ( 0.000000000000000000, 0.000000000000000000, 1.000000000000000000 ) ) ;
#26131 =( NAMED_UNIT ( * ) SI_UNIT ( $, .STERADIAN. ) SOLID_ANGLE_UNIT ( ) );
#26133 = FILL_AREA_STYLE_COLOUR ( '', #47152 ) ;
#26132 = PRESENTATION_STYLE_ASSIGNMENT (( #14921 ) ) ;
#26134 = CARTESIAN_POINT ( 'NONE',  ( -111.0549999999999926, -9.827790563157499189E-16, -8.024999999999991473 ) ) ;
#26135 = CLOSED_SHELL ( 'NONE', ( #57830, #54863, #45267, #38808, #27699, #60414 ) ) ;
#26136 = CARTESIAN_POINT ( 'NONE',  ( -1.166476076187854022E-15, 116.9449999999999932, 9.525000000000000355 ) ) ;
#26137 = CARTESIAN_POINT ( 'NONE',  ( -129.5949999999999989, 2.607480562269073321, 8.024999999999991473 ) ) ;
#26138 = EDGE_CURVE ( 'NONE', #44039, #2827, #46450, .T. ) ;
#26139 = VECTOR ( 'NONE', #12698, 1000.000000000000000 ) ;
#26140 = LINE ( 'NONE', #20883, #21249 ) ;
#26141 = AXIS2_PLACEMENT_3D ( 'NONE', #10977, #54224, #69384 ) ;
#26142 = FILL_AREA_STYLE ('',( #25797 ) ) ;
#26143 = ORIENTED_EDGE ( 'NONE', *, *, #65528, .T. ) ;
#26144 = EDGE_CURVE ( 'NONE', #8462, #58922, #11252, .T. ) ;
#26145 = CARTESIAN_POINT ( 'NONE',  ( -159.5929263765337680, -3.094860106618431139, -9.524999999999991473 ) ) ;
#26146 = CARTESIAN_POINT ( 'NONE',  ( -71.62068965517239860, 36.41396814395972115, 7.500000000000000000 ) ) ;
#26147 = AXIS2_PLACEMENT_3D ( 'NONE', #50038, #13069, #29597 ) ;
#26148 =( GEOMETRIC_REPRESENTATION_CONTEXT ( 3 ) GLOBAL_UNCERTAINTY_ASSIGNED_CONTEXT ( ( #51606 ) ) GLOBAL_UNIT_ASSIGNED_CONTEXT ( ( #11068, #467, #37170 ) ) REPRESENTATION_CONTEXT ( 'NONE', 'WORKASPACE' ) );
#26149 = LINE ( 'NONE', #47685, #14693 ) ;
#26150 = LINE ( 'NONE', #9998, #64970 ) ;
#26151 = DIRECTION ( 'NONE',  ( 0.000000000000000000, -1.000000000000000000, 0.000000000000000000 ) ) ;
#26152 = VERTEX_POINT ( 'NONE', #37351 ) ;
#26153 = CARTESIAN_POINT ( 'NONE',  ( -74.69292637653379074, 10.01517768586948698, -1.839758294383808571E-15 ) ) ;
#26154 = ITEM_DEFINED_TRANSFORMATION ( 'NONE', 'NONE', #46194,  #42840 ) ;
#26155 = CARTESIAN_POINT ( 'NONE',  ( 0.000000000000000000, 2.299999999999999822, 0.000000000000000000 ) ) ;
#26156 = FILL_AREA_STYLE_COLOUR ( '', #65331 ) ;
#26157 = VECTOR ( 'NONE', #5269, 1000.000000000000000 ) ;
#26158 =( NAMED_UNIT ( * ) SI_UNIT ( $, .STERADIAN. ) SOLID_ANGLE_UNIT ( ) );
#26159 = FACE_OUTER_BOUND ( 'NONE', #837, .T. ) ;
#26160 = CARTESIAN_POINT ( 'NONE',  ( -175.5549999999999784, 0.000000000000000000, 8.024999999999991473 ) ) ;
#26161 = EDGE_LOOP ( 'NONE', ( #9450, #40057, #52442, #19339 ) ) ;
#26162 = FILL_AREA_STYLE_COLOUR ( '', #16843 ) ;
#26163 = DIRECTION ( 'NONE',  ( -0.000000000000000000, -0.000000000000000000, -1.000000000000000000 ) ) ;
#26164 = CARTESIAN_POINT ( 'NONE',  ( -74.90707362346617515, -3.094860106618429807, 9.524999999999991473 ) ) ;
#26165 = ORIENTED_EDGE ( 'NONE', *, *, #53376, .F. ) ;
#26166 = CARTESIAN_POINT ( 'NONE',  ( 7.335726704534224041, -2.464278740834329184, 5.294148637306918204 ) ) ;
#26167 = AXIS2_PLACEMENT_3D ( 'NONE', #15320, #32472, #32844 ) ;
#26168 = DIRECTION ( 'NONE',  ( 1.300977106640434891E-16, -0.000000000000000000, 1.000000000000000000 ) ) ;
#26169 = CARTESIAN_POINT ( 'NONE',  ( 6.826472737025119919, 147.0070736234661695, 4.959722759717908325 ) ) ;
#26170 = EDGE_CURVE ( 'NONE', #14584, #29977, #59902, .T. ) ;
#26171 = AXIS2_PLACEMENT_3D ( 'NONE', #31899, #55355, #23342 ) ;
#26172 = ORIENTED_EDGE ( 'NONE', *, *, #49865, .T. ) ;
#26173 = FACE_OUTER_BOUND ( 'NONE', #3831, .T. ) ;
#26174 = CARTESIAN_POINT ( 'NONE',  ( -90.50499999999998124, -6.826472737025113702, -4.959722759717900331 ) ) ;
#26175 = SURFACE_STYLE_USAGE ( .BOTH. , #53943 ) ;
#26176 = VERTEX_POINT ( 'NONE', #5608 ) ;
#26177 =( NAMED_UNIT ( * ) PLANE_ANGLE_UNIT ( ) SI_UNIT ( $, .RADIAN. ) );
#26178 = CARTESIAN_POINT ( 'NONE',  ( 10.00000000000000533, 50.00000000000000000, -46.00000000000000000 ) ) ;
#26179 = DIRECTION ( 'NONE',  ( 0.000000000000000000, 0.000000000000000000, -1.000000000000000000 ) ) ;
#26180 = CARTESIAN_POINT ( 'NONE',  ( -75.75000000000000000, -0.4142135623730948124, 19.00000000000000000 ) ) ;
#26181 = ORIENTED_EDGE ( 'NONE', *, *, #31787, .F. ) ;
#26182 = CIRCLE ( 'NONE', #7119, 14.49999999999999822 ) ;
#26183 = CARTESIAN_POINT ( 'NONE',  ( -73.04499999999998749, 7.632228543268600340, 2.479861379858949277 ) ) ;
#26184 = ORIENTED_EDGE ( 'NONE', *, *, #51315, .F. ) ;
#26185 = DIRECTION ( 'NONE',  ( -1.000000000000000000, 0.000000000000000000, 0.000000000000000000 ) ) ;
#26186 = CIRCLE ( 'NONE', #32935, 113.0000000000000284 ) ;
#26187 = EDGE_CURVE ( 'NONE', #23284, #35896, #14542, .T. ) ;
#26188 = FILL_AREA_STYLE_COLOUR ( '', #44735 ) ;
#26189 = DIRECTION ( 'NONE',  ( -1.239088197126290817E-16, 0.000000000000000000, -1.000000000000000000 ) ) ;
#26190 = VECTOR ( 'NONE', #1372, 1000.000000000000000 ) ;
#26191 = ORIENTED_EDGE ( 'NONE', *, *, #32554, .T. ) ;
#26192 = LINE ( 'NONE', #3669, #39285 ) ;
#26193 = CARTESIAN_POINT ( 'NONE',  ( 93.00000000000000000, 0.9999999999999991118, 0.000000000000000000 ) ) ;
#26194 =( GEOMETRIC_REPRESENTATION_CONTEXT ( 3 ) GLOBAL_UNCERTAINTY_ASSIGNED_CONTEXT ( ( #5340 ) ) GLOBAL_UNIT_ASSIGNED_CONTEXT ( ( #45102, #66149, #28142 ) ) REPRESENTATION_CONTEXT ( 'NONE', 'WORKASPACE' ) );
#26195 = EDGE_CURVE ( 'NONE', #25944, #22594, #27411, .T. ) ;
#26196 =( NAMED_UNIT ( * ) PLANE_ANGLE_UNIT ( ) SI_UNIT ( $, .RADIAN. ) );
#26197 = CARTESIAN_POINT ( 'NONE',  ( -175.5570736234661808, -1.166476076187852838E-15, -9.524999999999991473 ) ) ;
#26198 = ORIENTED_EDGE ( 'NONE', *, *, #49490, .T. ) ;
#26199 = EDGE_CURVE ( 'NONE', #61564, #46540, #54505, .T. ) ;
#26200 = DIRECTION ( 'NONE',  ( 1.000000000000000000, 0.000000000000000000, 0.000000000000000000 ) ) ;
#26201 = ORIENTED_EDGE ( 'NONE', *, *, #4506, .T. ) ;
#26202 = DIRECTION ( 'NONE',  ( -1.000000000000000000, 0.000000000000000000, 0.000000000000000000 ) ) ;
#26203 = CARTESIAN_POINT ( 'NONE',  ( -149.0929263765342228, 3.094860106625894947, 9.524999999994570032 ) ) ;
#26204 = LINE ( 'NONE', #52285, #56894 ) ;
#26205 = CARTESIAN_POINT ( 'NONE',  ( -163.1070736234661354, 8.102448949553171076, -5.886773742842744461 ) ) ;
#26206 = CARTESIAN_POINT ( 'NONE',  ( -5.598654528085808657, 125.6449999999999818, 7.705886871421373741 ) ) ;
#26207 = CARTESIAN_POINT ( 'NONE',  ( -99.20707362346618652, 3.094860106618433360, 9.524999999999991473 ) ) ;
#26208 = CIRCLE ( 'NONE', #42041, 1.000000000000000000 ) ;
#26209 = AXIS2_PLACEMENT_3D ( 'NONE', #47777, #36848, #42832 ) ;
#26210 = EDGE_CURVE ( 'NONE', #67943, #49467, #27746, .T. ) ;
#26211 = ORIENTED_EDGE ( 'NONE', *, *, #39911, .F. ) ;
#26212 = FACE_OUTER_BOUND ( 'NONE', #36456, .T. ) ;
#26213 = ADVANCED_FACE ( 'NONE', ( #26392 ), #16905, .F. ) ;
#26214 = CARTESIAN_POINT ( 'NONE',  ( -11.74999999999999645, -4.000000000000000000, 7.000000000000001776 ) ) ;
#26215 = CARTESIAN_POINT ( 'NONE',  ( 0.000000000000000000, 130.0570736234661524, -8.025000000000000355 ) ) ;
#26216 = CARTESIAN_POINT ( 'NONE',  ( -140.7549999999999955, 4.716976649647091513, -6.492361379858946790 ) ) ;
#26217 = CARTESIAN_POINT ( 'NONE',  ( -74.99999999999998579, 50.00000000000000000, 7.000000000000000000 ) ) ;
#26218 = FACE_OUTER_BOUND ( 'NONE', #69193, .T. ) ;
#26219 = CARTESIAN_POINT ( 'NONE',  ( -150.2949999999999875, -2.607480562269069768, 8.024999999999991473 ) ) ;
#26220 =( GEOMETRIC_REPRESENTATION_CONTEXT ( 3 ) GLOBAL_UNCERTAINTY_ASSIGNED_CONTEXT ( ( #26892 ) ) GLOBAL_UNIT_ASSIGNED_CONTEXT ( ( #67394, #2973, #33993 ) ) REPRESENTATION_CONTEXT ( 'NONE', 'WORKASPACE' ) );
#26222 = AXIS2_PLACEMENT_3D ( 'NONE', #22649, #12076, #17052 ) ;
#26221 = AXIS2_PLACEMENT_3D ( 'NONE', #59368, #54456, #17217 ) ;
#26223 = CARTESIAN_POINT ( 'NONE',  ( -134.2450000000000045, -4.716976649647093289, -6.492361379858945902 ) ) ;
#26224 = EDGE_LOOP ( 'NONE', ( #68672, #60280, #16678 ) ) ;
#26225 = CARTESIAN_POINT ( 'NONE',  ( 44.15219150100328704, 9.717397167001077918, -3.137420992959917054 ) ) ;
#26226 =( REPRESENTATION_RELATIONSHIP ('NONE','NONE', #5102, #10054 ) REPRESENTATION_RELATIONSHIP_WITH_TRANSFORMATION ( #25127 )SHAPE_REPRESENTATION_RELATIONSHIP( ) );
#26227 =( GEOMETRIC_REPRESENTATION_CONTEXT ( 3 ) GLOBAL_UNCERTAINTY_ASSIGNED_CONTEXT ( ( #10760 ) ) GLOBAL_UNIT_ASSIGNED_CONTEXT ( ( #45869, #67652, #51469 ) ) REPRESENTATION_CONTEXT ( 'NONE', 'WORKASPACE' ) );
#26228 = MECHANICAL_DESIGN_GEOMETRIC_PRESENTATION_REPRESENTATION (  '', ( #17288 ), #4969 ) ;
#26229 = DIRECTION ( 'NONE',  ( -1.000000000000000000, 0.000000000000000000, 0.000000000000000000 ) ) ;
#26230 = UNCERTAINTY_MEASURE_WITH_UNIT (LENGTH_MEASURE( 1.000000000000000082E-05 ), #29303, 'distance_accuracy_value', 'NONE');
#26231 = CARTESIAN_POINT ( 'NONE',  ( -55.40499999999997982, -2.607480562269069768, 8.024999999999991473 ) ) ;
#26232 = SURFACE_STYLE_USAGE ( .BOTH. , #5803 ) ;
#26233 = PRESENTATION_LAYER_ASSIGNMENT (  '', '', ( #15028 ) ) ;
#26234 = CARTESIAN_POINT ( 'NONE',  ( -139.9429263765337907, 0.000000000000000000, 9.524999999999991473 ) ) ;
#26235 =( NAMED_UNIT ( * ) SI_UNIT ( $, .STERADIAN. ) SOLID_ANGLE_UNIT ( ) );
#26236 = COLOUR_RGB ( '', 0.40784314, 0.44705882, 0.49803922) ;
#26237 = FACE_OUTER_BOUND ( 'NONE', #57193, .T. ) ;
#26238 = ADVANCED_FACE ( 'NONE', ( #10577 ), #53488, .T. ) ;
#26239 = UNCERTAINTY_MEASURE_WITH_UNIT (LENGTH_MEASURE( 1.000000000000000082E-05 ), #43170, 'distance_accuracy_value', 'NONE');
#26240 = DIRECTION ( 'NONE',  ( 1.734723475976807094E-16, -0.9873505073845698643, -0.1585527532634883885 ) ) ;
#26241 = AXIS2_PLACEMENT_3D ( 'NONE', #35733, #50867, #2965 ) ;
#26242 = CARTESIAN_POINT ( 'NONE',  ( 7.794228634059946259, -2.500000000000000000, -4.500000000000001776 ) ) ;
#26243 = COLOUR_RGB ( '', 0.09019608, 0.27058824, 0.51372549) ;
#26244 = CARTESIAN_POINT ( 'NONE',  ( 3.000000000000002665, 42.00000000000000000, -89.00000000000000000 ) ) ;
#26245 = CARTESIAN_POINT ( 'NONE',  ( -178.7929263765338703, -3.094860106617228102, 9.525000000000863665 ) ) ;
#26246 = AXIS2_PLACEMENT_3D ( 'NONE', #67815, #51993, #41447 ) ;
#26247 = CIRCLE ( 'NONE', #18388, 0.5000000000000004441 ) ;
#26248 = DIRECTION ( 'NONE',  ( 0.000000000000000000, 1.000000000000000000, 0.000000000000000000 ) ) ;
#26249 = CARTESIAN_POINT ( 'NONE',  ( 23.50000000000001776, 42.00000000000000000, -29.68999999999999417 ) ) ;
#26250 = LINE ( 'NONE', #21310, #67714 ) ;
#26251 = EDGE_LOOP ( 'NONE', ( #39152, #23759, #20583, #19355 ) ) ;
#26252 = CARTESIAN_POINT ( 'NONE',  ( 7.632228543268607446, 111.1570736234661609, 2.479861379858954606 ) ) ;
#26253 =( BOUNDED_CURVE ( )  B_SPLINE_CURVE ( 2, ( #60142, #15873, #32027, #64730, #27415, #11603, #69654, #21467, #21826, #54837, #641 ),
 .UNSPECIFIED., .F., .F. ) 
 B_SPLINE_CURVE_WITH_KNOTS ( ( 3, 2, 2, 2, 2, 3 ),
 ( 0.6304347826086806883, 0.6326086956521589366, 0.6347826086956371849, 0.6369565217391153222, 0.6391304347825935706, 0.6413043478260718189 ),
 .UNSPECIFIED. ) 
 CURVE ( )  GEOMETRIC_REPRESENTATION_ITEM ( )  RATIONAL_B_SPLINE_CURVE ( ( 1.000000000000337508, 0.9510565162948161344, 1.000000000000000000, 0.9510565162951535312, 1.000000000000000000, 0.9510565162951535312, 1.000000000000000000, 0.9510565162951535312, 1.000000000000000000, 0.9510565162954934815, 0.9999999999996600497 ) ) 
 REPRESENTATION_ITEM ( '' )  );
#26254 = COLOUR_RGB ( '', 0.09019608, 0.27058824, 0.51372549) ;
#26255 = CIRCLE ( 'NONE', #55435, 1.999999999999999112 ) ;
#26256 =( LENGTH_UNIT ( ) NAMED_UNIT ( * ) SI_UNIT ( .MILLI., .METRE. ) );
#26257 = EDGE_LOOP ( 'NONE', ( #48555, #38111, #25292, #57531, #54889, #24772 ) ) ;
#26258 = ORIENTED_EDGE ( 'NONE', *, *, #44149, .T. ) ;
#26259 = CARTESIAN_POINT ( 'NONE',  ( 2.999999999999998668, 5.000000000000000000, -37.00402776293829277 ) ) ;
#26260 = CIRCLE ( 'NONE', #7203, 0.5000000000000000000 ) ;
#26261 = SURFACE_STYLE_FILL_AREA ( #10790 ) ;
#26262 = VERTEX_POINT ( 'NONE', #37702 ) ;
#26263 = CARTESIAN_POINT ( 'NONE',  ( -10.01517768586949231, 120.3049999999999784, -6.132527647946036459E-16 ) ) ;
#26264 = CARTESIAN_POINT ( 'NONE',  ( 1.802043943559349604, 2.359472279213374435, -9.000000000000007105 ) ) ;
#26265 = CARTESIAN_POINT ( 'NONE',  ( 45.00000000000000000, 10.69371294336137623, 6.585786437626905077 ) ) ;
#26266 =( GEOMETRIC_REPRESENTATION_CONTEXT ( 3 ) GLOBAL_UNCERTAINTY_ASSIGNED_CONTEXT ( ( #4504 ) ) GLOBAL_UNIT_ASSIGNED_CONTEXT ( ( #53360, #16449, #38603 ) ) REPRESENTATION_CONTEXT ( 'NONE', 'WORKASPACE' ) );
#26267 = DIRECTION ( 'NONE',  ( 1.000000000000000000, 0.000000000000000000, 0.000000000000000000 ) ) ;
#26268 = CARTESIAN_POINT ( 'NONE',  ( -97.94499999999999318, -9.827790563157499189E-16, -8.024999999999991473 ) ) ;
#26269 = EDGE_LOOP ( 'NONE', ( #50104, #21056, #53274, #10030 ) ) ;
#26270 = CYLINDRICAL_SURFACE ( 'NONE', #52413, 1.000000000000000888 ) ;
#26271 = ADVANCED_FACE ( 'NONE', ( #32351 ), #36359, .T. ) ;
#26272 = ORIENTED_EDGE ( 'NONE', *, *, #57166, .T. ) ;
#26273 = CARTESIAN_POINT ( 'NONE',  ( -8.437984349512095861, 153.6929263765337907, -5.166775262442723748E-16 ) ) ;
#26274 = DIRECTION ( 'NONE',  ( -1.099520432716498623E-15, 1.000000000000000000, 1.099520432716498623E-15 ) ) ;
#26275 = EDGE_CURVE ( 'NONE', #3117, #36574, #50623, .T. ) ;
#26276 = VECTOR ( 'NONE', #42650, 1000.000000000000000 ) ;
#26277 = CARTESIAN_POINT ( 'NONE',  ( -61.85707362346616378, -5.598654528085803328, -7.705886871421366635 ) ) ;
#26278 = ORIENTED_EDGE ( 'NONE', *, *, #55820, .F. ) ;
#26279 = SURFACE_STYLE_FILL_AREA ( #35811 ) ;
#26280 = DIRECTION ( 'NONE',  ( 0.000000000000000000, 1.000000000000000000, 0.000000000000000000 ) ) ;
#26281 = DIRECTION ( 'NONE',  ( 1.000000000000000000, 0.000000000000000000, 0.000000000000000000 ) ) ;
#26282 =( GEOMETRIC_REPRESENTATION_CONTEXT ( 3 ) GLOBAL_UNCERTAINTY_ASSIGNED_CONTEXT ( ( #352 ) ) GLOBAL_UNIT_ASSIGNED_CONTEXT ( ( #2968, #56127, #40684 ) ) REPRESENTATION_CONTEXT ( 'NONE', 'WORKASPACE' ) );
#26283 = CARTESIAN_POINT ( 'NONE',  ( 0.000000000000000000, 0.000000000000000000, 42.50000000000000000 ) ) ;
#26284 = COLOUR_RGB ( '', 0.72549020, 0.75294118, 0.79215686) ;
#26285 = FILL_AREA_STYLE ('',( #41462 ) ) ;
#26286 = PRESENTATION_LAYER_ASSIGNMENT (  '', '', ( #1540 ) ) ;
#26287 = CARTESIAN_POINT ( 'NONE',  ( 20.57648123223228254, 154.9999999999999716, 10.27659574468085069 ) ) ;
#26288 = DIRECTION ( 'NONE',  ( 1.000000000000000000, 0.000000000000000000, 0.000000000000000000 ) ) ;
#26289 = ORIENTED_EDGE ( 'NONE', *, *, #68333, .T. ) ;
#26290 = ORIENTED_EDGE ( 'NONE', *, *, #55663, .F. ) ;
#26291 = CARTESIAN_POINT ( 'NONE',  ( -22.75000000000000711, 36.75000000000000000, 3.750000000000000000 ) ) ;
#26292 = EDGE_CURVE ( 'NONE', #47180, #16387, #55548, .T. ) ;
#26293 = CARTESIAN_POINT ( 'NONE',  ( -170.6070736234661922, -8.102448949553174629, 5.886773742842742685 ) ) ;
#26294 = DIRECTION ( 'NONE',  ( 0.000000000000000000, 0.000000000000000000, 1.000000000000000000 ) ) ;
#26295 = ORIENTED_EDGE ( 'NONE', *, *, #38092, .F. ) ;
#26296 = CARTESIAN_POINT ( 'NONE',  ( -167.1550000000000011, 7.632228543268600340, 2.479861379858949277 ) ) ;
#26297 = FACE_OUTER_BOUND ( 'NONE', #57087, .T. ) ;
#26298 = DIRECTION ( 'NONE',  ( -1.000000000000000000, 0.000000000000000000, 0.000000000000000000 ) ) ;
#26299 = CARTESIAN_POINT ( 'NONE',  ( -179.9950000000000045, -6.826472737025115478, 4.959722759717900331 ) ) ;
#26300 = CARTESIAN_POINT ( 'NONE',  ( -167.9949999999999761, -6.826472737025113702, 4.959722759717902107 ) ) ;
#26301 = ORIENTED_EDGE ( 'NONE', *, *, #31340, .T. ) ;
#26302 = CYLINDRICAL_SURFACE ( 'NONE', #17863, 0.5000000000000004441 ) ;
#26303 = CARTESIAN_POINT ( 'NONE',  ( 57.00000000000000000, 5.000000000000000000, -60.00402776293827145 ) ) ;
#26304 =( NAMED_UNIT ( * ) PLANE_ANGLE_UNIT ( ) SI_UNIT ( $, .RADIAN. ) );
#26305 = CARTESIAN_POINT ( 'NONE',  ( -81.50499999999999545, -6.826472737025115478, -4.959722759717899443 ) ) ;
#26306 = CARTESIAN_POINT ( 'NONE',  ( -195.0000000000000000, 1.166476076187852838E-15, -9.524999999999991473 ) ) ;
#26307 = DIRECTION ( 'NONE',  ( -1.000000000000000000, -0.000000000000000000, -0.000000000000000000 ) ) ;
#26308 = AXIS2_PLACEMENT_3D ( 'NONE', #15531, #25690, #37001 ) ;
#26309 = CARTESIAN_POINT ( 'NONE',  ( -85.34499999999998465, 7.632228543268599452, -2.479861379858951942 ) ) ;
#26310 = CARTESIAN_POINT ( 'NONE',  ( 3.094860106618435136, 128.4049999999999443, -9.525000000000000355 ) ) ;
#26311 = CARTESIAN_POINT ( 'NONE',  ( 20.57648123223228254, 114.4999999999999574, -10.27659574468085069 ) ) ;
#26312 = CIRCLE ( 'NONE', #30832, 1.000000000000000888 ) ;
#26313 = CARTESIAN_POINT ( 'NONE',  ( -171.8070736234661808, 10.01517768586948698, -1.839758294383808966E-15 ) ) ;
#26314 = ADVANCED_FACE ( 'NONE', ( #18932 ), #35157, .F. ) ;
#26315 = UNCERTAINTY_MEASURE_WITH_UNIT (LENGTH_MEASURE( 1.000000000000000082E-05 ), #3529, 'distance_accuracy_value', 'NONE');
#26316 =( NAMED_UNIT ( * ) PLANE_ANGLE_UNIT ( ) SI_UNIT ( $, .RADIAN. ) );
#26317 = DIRECTION ( 'NONE',  ( 1.000000000000000000, 0.000000000000000000, 0.000000000000000000 ) ) ;
#26318 = VERTEX_POINT ( 'NONE', #44699 ) ;
#26319 = DIRECTION ( 'NONE',  ( 0.7071067811865352493, 0.000000000000000000, 0.7071067811865597852 ) ) ;
#26320 = CONICAL_SURFACE ( 'NONE', #13984, 3.000000000000000444, 0.7853981633974517207 ) ;
#26321 = FACE_OUTER_BOUND ( 'NONE', #592, .T. ) ;
#26323 = CARTESIAN_POINT ( 'NONE',  ( -69.99999999999998579, 50.00000000000000000, 11.50000000000003730 ) ) ;
#26322 = LINE ( 'NONE', #4878, #46547 ) ;
#26324 = CARTESIAN_POINT ( 'NONE',  ( -7.632228543268608334, 136.9570736234661581, 2.479861379858952830 ) ) ;
#26325 = ORIENTED_EDGE ( 'NONE', *, *, #19130, .F. ) ;
#26326 = EDGE_LOOP ( 'NONE', ( #51140, #39619 ) ) ;
#26327 = AXIS2_PLACEMENT_3D ( 'NONE', #42794, #5420, #37160 ) ;
#26328 = CARTESIAN_POINT ( 'NONE',  ( -174.0570736234661808, 0.000000000000000000, 9.524999999999991473 ) ) ;
#26330 = UNCERTAINTY_MEASURE_WITH_UNIT (LENGTH_MEASURE( 1.000000000000000082E-05 ), #32350, 'distance_accuracy_value', 'NONE');
#26329 = VECTOR ( 'NONE', #14591, 1000.000000000000000 ) ;
#26331 = AXIS2_PLACEMENT_3D ( 'NONE', #21052, #15120, #62906 ) ;
#26332 = CARTESIAN_POINT ( 'NONE',  ( -7.632228543268607446, 147.5429263765338135, -2.479861379858953718 ) ) ;
#26333 = SURFACE_STYLE_FILL_AREA ( #63636 ) ;
#26334 =( BOUNDED_CURVE ( )  B_SPLINE_CURVE ( 2, ( #32142, #10357, #68756, #20547, #63795, #52919, #47695, #54952, #22273, #34552, #13093 ),
 .UNSPECIFIED., .F., .F. ) 
 B_SPLINE_CURVE_WITH_KNOTS ( ( 3, 2, 2, 2, 2, 3 ),
 ( 0.7352941176470586537, 0.7411764705882351034, 0.7470588235294115531, 0.7529411764705881138, 0.7588235294117645635, 0.7647058823529410132 ),
 .UNSPECIFIED. ) 
 CURVE ( )  GEOMETRIC_REPRESENTATION_ITEM ( )  RATIONAL_B_SPLINE_CURVE ( ( 1.000000000000001776, 0.9510565162951516438, 1.000000000000000000, 0.9510565162951535312, 1.000000000000000000, 0.9510565162951535312, 1.000000000000000000, 0.9510565162951535312, 1.000000000000000000, 0.9510565162951544194, 0.9999999999999991118 ) ) 
 REPRESENTATION_ITEM ( '' )  );
#26335 = CARTESIAN_POINT ( 'NONE',  ( 16.00000000000001776, 15.00000000000000000, -29.68999999999999417 ) ) ;
#26336 = CARTESIAN_POINT ( 'NONE',  ( 66.74999999999998579, 36.75000000000000000, -4.000000000000000000 ) ) ;
#26337 = ORIENTED_EDGE ( 'NONE', *, *, #6896, .T. ) ;
#26338 = CARTESIAN_POINT ( 'NONE',  ( -120.5049999999999670, -6.826472737025113702, -4.959722759717900331 ) ) ;
#26339 = ORIENTED_EDGE ( 'NONE', *, *, #23423, .F. ) ;
#26340 = AXIS2_PLACEMENT_3D ( 'NONE', #28483, #29896, #29544 ) ;
#26341 = FACE_BOUND ( 'NONE', #1157, .T. ) ;
#26342 = FACE_OUTER_BOUND ( 'NONE', #16851, .T. ) ;
#26343 = ORIENTED_EDGE ( 'NONE', *, *, #28671, .F. ) ;
#26344 = SURFACE_STYLE_FILL_AREA ( #4537 ) ;
#26345 = CARTESIAN_POINT ( 'NONE',  ( 6.759171781091399822, 2.392512705203733603, 2.292771058063876488 ) ) ;
#26346 = EDGE_LOOP ( 'NONE', ( #24882, #45365, #26289, #41794 ) ) ;
#26347 = EDGE_CURVE ( 'NONE', #32128, #53024, #7017, .T. ) ;
#26348 = CARTESIAN_POINT ( 'NONE',  ( 9.058813317711338797, 147.8449999999999989, -2.943386871421372675 ) ) ;
#26349 = DIRECTION ( 'NONE',  ( 0.000000000000000000, -0.000000000000000000, -1.000000000000000000 ) ) ;
#26350 = AXIS2_PLACEMENT_3D ( 'NONE', #10584, #10922, #33413 ) ;
#26351 = EDGE_LOOP ( 'NONE', ( #58266, #53891, #38385 ) ) ;
#26352 = CIRCLE ( 'NONE', #67908, 0.2500000000000002220 ) ;
#26353 = PLANE ( 'NONE',  #42351 ) ;
#26354 = CARTESIAN_POINT ( 'NONE',  ( 0.000000000000000000, 149.5550000000000068, -9.525000000000000355 ) ) ;
#26355 = CARTESIAN_POINT ( 'NONE',  ( -135.6570736234661751, 9.058813317711329915, 2.943386871421369566 ) ) ;
#26356 = CARTESIAN_POINT ( 'NONE',  ( -195.0000000000000000, 0.000000000000000000, 0.000000000000000000 ) ) ;
#26357 = ORIENTED_EDGE ( 'NONE', *, *, #45497, .F. ) ;
#26358 = CARTESIAN_POINT ( 'NONE',  ( -4.716976649647097730, 129.2429263765338021, -6.492361379858953896 ) ) ;
#26359 = LINE ( 'NONE', #47897, #26655 ) ;
#26360 = UNCERTAINTY_MEASURE_WITH_UNIT (LENGTH_MEASURE( 1.000000000000000082E-05 ), #9467, 'distance_accuracy_value', 'NONE');
#26361 = CYLINDRICAL_SURFACE ( 'NONE', #66956, 1.000000000000000000 ) ;
#26362 = AXIS2_PLACEMENT_3D ( 'NONE', #20069, #5274, #22163 ) ;
#26363 = EDGE_CURVE ( 'NONE', #6589, #58485, #1449, .T. ) ;
#26364 =( LENGTH_UNIT ( ) NAMED_UNIT ( * ) SI_UNIT ( .MILLI., .METRE. ) );
#26365 = ORIENTED_EDGE ( 'NONE', *, *, #25353, .F. ) ;
#26366 = LINE ( 'NONE', #25669, #50906 ) ;
#26367 = VERTEX_POINT ( 'NONE', #55184 ) ;
#26368 = CARTESIAN_POINT ( 'NONE',  ( -58.79292637653379927, -3.094860106618429807, 9.524999999999991473 ) ) ;
#26369 = STYLED_ITEM ( 'NONE', ( #11738 ), #62457 ) ;
#26370 = CARTESIAN_POINT ( 'NONE',  ( 13.75000000000000355, 28.24999999999998934, 3.750000000000000000 ) ) ;
#26371 = CARTESIAN_POINT ( 'NONE',  ( -71.50000000000000000, 14.49137674618942562, -10.00000000000000000 ) ) ;
#26372 = PRESENTATION_LAYER_ASSIGNMENT (  '', '', ( #28620 ) ) ;
#26373 = CARTESIAN_POINT ( 'NONE',  ( -156.9549999999999841, -7.632228543268599452, 2.479861379858951054 ) ) ;
#26374 = EDGE_CURVE ( 'NONE', #52933, #25180, #39406, .T. ) ;
#26375 = CARTESIAN_POINT ( 'NONE',  ( 3.749999999999999556, 33.99999999999998579, -3.750000000000000000 ) ) ;
#26376 = PRESENTATION_STYLE_ASSIGNMENT (( #32686 ) ) ;
#26377 = UNCERTAINTY_MEASURE_WITH_UNIT (LENGTH_MEASURE( 1.000000000000000082E-05 ), #55393, 'distance_accuracy_value', 'NONE');
#26378 = EDGE_CURVE ( 'NONE', #30878, #59688, #47142, .T. ) ;
#26379 = CARTESIAN_POINT ( 'NONE',  ( -7.500000000000000000, 0.000000000000000000, 1.000000000000000000 ) ) ;
#26380 = FILL_AREA_STYLE ('',( #32690 ) ) ;
#26381 = CARTESIAN_POINT ( 'NONE',  ( 41.08036663239563069, 107.6296822352908009, 3.281244196345447062 ) ) ;
#26382 = VERTEX_POINT ( 'NONE', #25268 ) ;
#26383 = EDGE_LOOP ( 'NONE', ( #41916, #39582, #2533, #220, #27000 ) ) ;
#26384 = CARTESIAN_POINT ( 'NONE',  ( 22.70969830132048628, 24.88211553739179394, 27.31720690014012121 ) ) ;
#26385 = EDGE_CURVE ( 'NONE', #21325, #15190, #63255, .T. ) ;
#26386 = DIRECTION ( 'NONE',  ( 0.000000000000000000, 0.000000000000000000, 1.000000000000000000 ) ) ;
#26387 = CARTESIAN_POINT ( 'NONE',  ( -65.15499999999998693, 7.632228543268600340, 2.479861379858949277 ) ) ;
#26389 = ORIENTED_EDGE ( 'NONE', *, *, #61146, .T. ) ;
#26388 = STYLED_ITEM ( 'NONE', ( #22280 ), #38897 ) ;
#26390 = CARTESIAN_POINT ( 'NONE',  ( 6.999798566743339556, 49.77026365512251971, 7.251305755767526229 ) ) ;
#26391 = DIRECTION ( 'NONE',  ( 0.000000000000000000, 0.000000000000000000, -1.000000000000000000 ) ) ;
#26392 = FACE_OUTER_BOUND ( 'NONE', #56361, .T. ) ;
#26393 = AXIS2_PLACEMENT_3D ( 'NONE', #11390, #53947, #65553 ) ;
#26394 = SURFACE_SIDE_STYLE ('',( #32353 ) ) ;
#26395 = AXIS2_PLACEMENT_3D ( 'NONE', #26516, #11732, #54637 ) ;
#26396 = VERTEX_POINT ( 'NONE', #4480 ) ;
#26397 = VECTOR ( 'NONE', #51953, 1000.000000000000000 ) ;
#26398 =( NAMED_UNIT ( * ) SI_UNIT ( $, .STERADIAN. ) SOLID_ANGLE_UNIT ( ) );
#26399 = CARTESIAN_POINT ( 'NONE',  ( 74.99999999999998579, 119.9999999999997584, 10.00000000000000000 ) ) ;
#26400 =( LENGTH_UNIT ( ) NAMED_UNIT ( * ) SI_UNIT ( .MILLI., .METRE. ) );
#26401 = CARTESIAN_POINT ( 'NONE',  ( -122.2449999999999903, -4.716976649647093289, -6.492361379858945902 ) ) ;
#26402 = CARTESIAN_POINT ( 'NONE',  ( -10.01517768586949231, 152.1949999999999932, -6.132527647946036459E-16 ) ) ;
#26403 = CARTESIAN_POINT ( 'NONE',  ( -87.89499999999998181, 6.826472737025116366, 4.959722759717898555 ) ) ;
#26404 = DIRECTION ( 'NONE',  ( 0.000000000000000000, 0.000000000000000000, 1.000000000000000000 ) ) ;
#26405 = UNCERTAINTY_MEASURE_WITH_UNIT (LENGTH_MEASURE( 1.000000000000000082E-05 ), #27549, 'distance_accuracy_value', 'NONE');
#26406 = AXIS2_PLACEMENT_3D ( 'NONE', #5198, #26978, #5889 ) ;
#26407 = FILL_AREA_STYLE_COLOUR ( '', #21333 ) ;
#26408 = AXIS2_PLACEMENT_3D ( 'NONE', #57631, #10138, #4128 ) ;
#26409 = VERTEX_POINT ( 'NONE', #68537 ) ;
#26410 = CARTESIAN_POINT ( 'NONE',  ( -131.9929263765338305, 8.102448949553171076, -5.886773742842744461 ) ) ;
#26411 = CARTESIAN_POINT ( 'NONE',  ( 44.91886116991580735, 9.999999999999980460, -3.201362207699240514 ) ) ;
#26412 = CARTESIAN_POINT ( 'NONE',  ( -147.5949999999999704, 2.607480562269073321, 8.024999999999991473 ) ) ;
#26413 = DIRECTION ( 'NONE',  ( 0.000000000000000000, -1.000000000000000000, 1.156482317317871478E-16 ) ) ;
#26414 = VECTOR ( 'NONE', #33258, 1000.000000000000000 ) ;
#26415 = CIRCLE ( 'NONE', #45560, 16.99999999999998579 ) ;
#26416 = DIRECTION ( 'NONE',  ( 0.000000000000000000, 0.000000000000000000, -1.000000000000000000 ) ) ;
#26417 = ORIENTED_EDGE ( 'NONE', *, *, #9856, .F. ) ;
#26418 = ORIENTED_EDGE ( 'NONE', *, *, #3718, .F. ) ;
#26419 = CIRCLE ( 'NONE', #15276, 0.2500000000000002220 ) ;
#26420 = DIRECTION ( 'NONE',  ( 0.000000000000000000, 0.000000000000000000, 1.000000000000000000 ) ) ;
#26421 = DIRECTION ( 'NONE',  ( 1.000000000000000000, -0.000000000000000000, -0.000000000000000000 ) ) ;
#26422 = CARTESIAN_POINT ( 'NONE',  ( -71.74137931034479720, 63.10081643261027295, 9.500000000000000000 ) ) ;
#26423 = CARTESIAN_POINT ( 'NONE',  ( -59.24292637653380211, 5.598654528085804216, 7.705886871421366635 ) ) ;
#26424 =( NAMED_UNIT ( * ) SI_UNIT ( $, .STERADIAN. ) SOLID_ANGLE_UNIT ( ) );
#26425 = VERTEX_POINT ( 'NONE', #15104 ) ;
#26426 = CARTESIAN_POINT ( 'NONE',  ( -151.1049999999999613, -6.826472737025113702, 4.959722759717902107 ) ) ;
#26427 = AXIS2_PLACEMENT_3D ( 'NONE', #62343, #57414, #14166 ) ;
#26428 = EDGE_LOOP ( 'NONE', ( #14384, #36204 ) ) ;
#26429 = CARTESIAN_POINT ( 'NONE',  ( -24.21231517720798010, 112.9999999999999858, -7.500000000000000000 ) ) ;
#26430 = CARTESIAN_POINT ( 'NONE',  ( -141.6570736234662036, 9.058813317711329915, 2.943386871421369566 ) ) ;
#26431 = VERTEX_POINT ( 'NONE', #8751 ) ;
#26432 = EDGE_CURVE ( 'NONE', #46838, #9321, #22868, .T. ) ;
#26433 = FILL_AREA_STYLE_COLOUR ( '', #38325 ) ;
#26434 = SURFACE_SIDE_STYLE ('',( #64774 ) ) ;
#26435 = CARTESIAN_POINT ( 'NONE',  ( -5.598654528085808657, 116.6449999999999818, 7.705886871421373741 ) ) ;
#26436 = CARTESIAN_POINT ( 'NONE',  ( 48.49999999999999289, 24.74999999999998579, -3.750000000000000000 ) ) ;
#26437 = AXIS2_PLACEMENT_3D ( 'NONE', #678, #22209, #47619 ) ;
#26438 = EDGE_CURVE ( 'NONE', #65525, #8699, #57996, .T. ) ;
#26439 = VERTEX_POINT ( 'NONE', #24911 ) ;
#26440 = EDGE_CURVE ( 'NONE', #65467, #66860, #20644, .T. ) ;
#26441 = FILL_AREA_STYLE_COLOUR ( '', #10606 ) ;
#26442 = CARTESIAN_POINT ( 'NONE',  ( 9.058813317711338797, 124.9549999999999841, -2.943386871421372675 ) ) ;
#26443 = CARTESIAN_POINT ( 'NONE',  ( -63.20499999999998408, -2.607480562269071545, -8.024999999999991473 ) ) ;
#26444 = DIRECTION ( 'NONE',  ( -1.000000000000000000, -0.000000000000000000, -0.000000000000000000 ) ) ;
#26445 = ORIENTED_EDGE ( 'NONE', *, *, #64751, .T. ) ;
#26446 = CARTESIAN_POINT ( 'NONE',  ( -10.01517768586949231, 147.3049999999999500, -6.132527647946036459E-16 ) ) ;
#26447 = UNCERTAINTY_MEASURE_WITH_UNIT (LENGTH_MEASURE( 1.000000000000000082E-05 ), #59536, 'distance_accuracy_value', 'NONE');
#26448 = EDGE_CURVE ( 'NONE', #29261, #17063, #19645, .T. ) ;
#26449 = CARTESIAN_POINT ( 'NONE',  ( 72.00000000000000000, 36.32520566882265456, -7.000000000000000000 ) ) ;
#26450 = CARTESIAN_POINT ( 'NONE',  ( -75.00000000000000000, -2.215169945516535778E-14, 9.500000000000000000 ) ) ;
#26451 = EDGE_CURVE ( 'NONE', #25847, #25839, #26208, .T. ) ;
#26452 = CARTESIAN_POINT ( 'NONE',  ( 12.25000000000000355, 30.99999999999998579, 3.750000000000000000 ) ) ;
#26453 = EDGE_CURVE ( 'NONE', #53612, #45556, #39682, .T. ) ;
#26454 = CARTESIAN_POINT ( 'NONE',  ( -15.48999599679679662, 118.4999999999999716, -7.000000000000000000 ) ) ;
#26455 = VERTEX_POINT ( 'NONE', #56587 ) ;
#26456 =( LENGTH_UNIT ( ) NAMED_UNIT ( * ) SI_UNIT ( .MILLI., .METRE. ) );
#26457 = CARTESIAN_POINT ( 'NONE',  ( 23.21231517720798010, 112.9999999999999858, -10.00000000000000000 ) ) ;
#26458 = CARTESIAN_POINT ( 'NONE',  ( -182.4550000000000125, 7.632228543268599452, -2.479861379858951942 ) ) ;
#26460 = ORIENTED_EDGE ( 'NONE', *, *, #45415, .T. ) ;
#26459 = ADVANCED_FACE ( 'NONE', ( #20337 ), #68918, .T. ) ;
#26461 = CARTESIAN_POINT ( 'NONE',  ( -88.10707362346616378, 8.102448949553172852, -5.886773742842744461 ) ) ;
#26462 = CIRCLE ( 'NONE', #18586, 0.5000000000000004441 ) ;
#26463 = SURFACE_SIDE_STYLE ('',( #69390 ) ) ;
#26464 = EDGE_CURVE ( 'NONE', #33977, #28720, #9457, .T. ) ;
#26465 =( NAMED_UNIT ( * ) SI_UNIT ( $, .STERADIAN. ) SOLID_ANGLE_UNIT ( ) );
#26466 = ORIENTED_EDGE ( 'NONE', *, *, #64673, .T. ) ;
#26467 = DIRECTION ( 'NONE',  ( 1.000000000000000000, 7.709882115452469292E-16, 0.000000000000000000 ) ) ;
#26468 = ORIENTED_EDGE ( 'NONE', *, *, #5371, .T. ) ;
#26469 = DIRECTION ( 'NONE',  ( 0.000000000000000000, -0.9984713486292863260, 0.05527174654752588234 ) ) ;
#26470 = CARTESIAN_POINT ( 'NONE',  ( -90.95499999999999829, -7.632228543268599452, 2.479861379858951054 ) ) ;
#26471 = ORIENTED_EDGE ( 'NONE', *, *, #52052, .F. ) ;
#26472 = LINE ( 'NONE', #36393, #6982 ) ;
#26473 = CIRCLE ( 'NONE', #25317, 0.5000000000000004441 ) ;
#26474 = CARTESIAN_POINT ( 'NONE',  ( -128.1570736234661751, -9.058813317711329915, -2.943386871421370898 ) ) ;
#26475 = FILL_AREA_STYLE_COLOUR ( '', #4763 ) ;
#26476 = CARTESIAN_POINT ( 'NONE',  ( 9.058813317711337021, 153.5449999999999875, 2.943386871421375783 ) ) ;
#26477 = CARTESIAN_POINT ( 'NONE',  ( -63.65707362346617515, 9.058813317711329915, 2.943386871421369566 ) ) ;
#26478 = CYLINDRICAL_SURFACE ( 'NONE', #30234, 1.000000000000000888 ) ;
#26479 = ORIENTED_EDGE ( 'NONE', *, *, #15850, .F. ) ;
#26480 = DIRECTION ( 'NONE',  ( -1.000000000000000000, -0.000000000000000000, -0.000000000000000000 ) ) ;
#26481 = SURFACE_SIDE_STYLE ('',( #1692 ) ) ;
#26483 = FACE_OUTER_BOUND ( 'NONE', #61782, .T. ) ;
#26482 = DIRECTION ( 'NONE',  ( -0.000000000000000000, -0.000000000000000000, 1.000000000000000000 ) ) ;
#26484 = CARTESIAN_POINT ( 'NONE',  ( -110.3049999999999926, 8.437984349512085203, -1.550032578732815448E-15 ) ) ;
#26485 = CARTESIAN_POINT ( 'NONE',  ( 3.094860106618431583, 120.0949999999999704, 9.525000000000000355 ) ) ;
#26486 = CARTESIAN_POINT ( 'NONE',  ( -118.3449999999999989, 7.632228543268599452, -2.479861379858951942 ) ) ;
#26487 = VECTOR ( 'NONE', #46135, 1000.000000000000000 ) ;
#26488 = EDGE_CURVE ( 'NONE', #7947, #27455, #21725, .T. ) ;
#26490 = CARTESIAN_POINT ( 'NONE',  ( -45.00000000000000000, 0.000000000000000000, 0.000000000000000000 ) ) ;
#26489 = SURFACE_SIDE_STYLE ('',( #5364 ) ) ;
#26491 = VERTEX_POINT ( 'NONE', #64284 ) ;
#26492 = CARTESIAN_POINT ( 'NONE',  ( -161.9929263765337737, 8.102448949553171076, -5.886773742842744461 ) ) ;
#26493 = CARTESIAN_POINT ( 'NONE',  ( -182.9949999999999761, -6.826472737025115478, 4.959722759717900331 ) ) ;
#26494 = DIRECTION ( 'NONE',  ( 0.9418169057949938860, 0.000000000000000000, 0.3361263392814427542 ) ) ;
#26495 = FACE_OUTER_BOUND ( 'NONE', #20742, .T. ) ;
#26496 = FILL_AREA_STYLE_COLOUR ( '', #20027 ) ;
#26497 = SURFACE_STYLE_FILL_AREA ( #37815 ) ;
#26498 = ORIENTED_EDGE ( 'NONE', *, *, #33973, .T. ) ;
#26499 = CARTESIAN_POINT ( 'NONE',  ( -74.09292637653381064, 3.094860106618433360, 9.524999999999991473 ) ) ;
#26500 = DIRECTION ( 'NONE',  ( 0.000000000000000000, 0.000000000000000000, -1.000000000000000000 ) ) ;
#26501 =( NAMED_UNIT ( * ) PLANE_ANGLE_UNIT ( ) SI_UNIT ( $, .RADIAN. ) );
#26502 = PRESENTATION_LAYER_ASSIGNMENT (  '', '', ( #60213 ) ) ;
#26503 =( LENGTH_UNIT ( ) NAMED_UNIT ( * ) SI_UNIT ( .MILLI., .METRE. ) );
#26504 = SURFACE_SIDE_STYLE ('',( #59195 ) ) ;
#26505 = CARTESIAN_POINT ( 'NONE',  ( -6.667623377008404795, -6.451337545287478825, 0.2685431138779681981 ) ) ;
#26506 = AXIS2_PLACEMENT_3D ( 'NONE', #52004, #8732, #12962 ) ;
#26507 = CARTESIAN_POINT ( 'NONE',  ( -177.8049999999999500, -8.437984349512086979, 5.166775262442717831E-16 ) ) ;
#26508 = EDGE_CURVE ( 'NONE', #46008, #43417, #3727, .T. ) ;
#26509 = ORIENTED_EDGE ( 'NONE', *, *, #35664, .F. ) ;
#26510 = DIRECTION ( 'NONE',  ( -0.000000000000000000, -0.000000000000000000, 1.000000000000000000 ) ) ;
#26511 = DIRECTION ( 'NONE',  ( -1.000000000000000000, 0.000000000000000000, 0.000000000000000000 ) ) ;
#26512 = DIRECTION ( 'NONE',  ( -0.000000000000000000, -0.000000000000000000, 1.000000000000000000 ) ) ;
#26513 = CIRCLE ( 'NONE', #65855, 5.000000000000000000 ) ;
#26514 =( NAMED_UNIT ( * ) PLANE_ANGLE_UNIT ( ) SI_UNIT ( $, .RADIAN. ) );
#26515 = AXIS2_PLACEMENT_3D ( 'NONE', #18220, #1648, #39362 ) ;
#26516 = CARTESIAN_POINT ( 'NONE',  ( 60.00000000000000000, 1.797044900979284448E-15, -6.500000000000000000 ) ) ;
#26517 = CARTESIAN_POINT ( 'NONE',  ( -6.826472737025120807, 146.1070736234661354, 4.959722759717906548 ) ) ;
#26518 = EDGE_CURVE ( 'NONE', #31530, #2782, #5513, .T. ) ;
#26519 = ORIENTED_EDGE ( 'NONE', *, *, #2960, .T. ) ;
#26520 = FACE_BOUND ( 'NONE', #53047, .T. ) ;
#26521 = CARTESIAN_POINT ( 'NONE',  ( -97.85499999999998977, 4.716976649647094177, 6.492361379858945902 ) ) ;
#26522 = UNCERTAINTY_MEASURE_WITH_UNIT (LENGTH_MEASURE( 1.000000000000000082E-05 ), #42779, 'distance_accuracy_value', 'NONE');
#26523 = PLANE ( 'NONE',  #31948 ) ;
#26524 = ORIENTED_EDGE ( 'NONE', *, *, #9812, .T. ) ;
#26525 = CYLINDRICAL_SURFACE ( 'NONE', #17561, 0.5000000000000004441 ) ;
#26526 = AXIS2_PLACEMENT_3D ( 'NONE', #44995, #30486, #46384 ) ;
#26527 = CARTESIAN_POINT ( 'NONE',  ( 2.607480562268992941, 143.7929263765338419, -8.025000000000060751 ) ) ;
#26528 = DIRECTION ( 'NONE',  ( 0.000000000000000000, 0.000000000000000000, -1.000000000000000000 ) ) ;
#26529 = CARTESIAN_POINT ( 'NONE',  ( 30.99999999999999289, 0.000000000000000000, 24.00402776293822171 ) ) ;
#26530 = EDGE_CURVE ( 'NONE', #24348, #57711, #59954, .T. ) ;
#26531 = COLOUR_RGB ( '', 0.31764706, 0.68627451, 0.89019608) ;
#26532 = ORIENTED_EDGE ( 'NONE', *, *, #30740, .F. ) ;
#26533 = CARTESIAN_POINT ( 'NONE',  ( -13.75000000000000355, 28.24999999999998934, 3.750000000000000000 ) ) ;
#26534 = CARTESIAN_POINT ( 'NONE',  ( -73.49499999999999034, 6.826472737025113702, -4.959722759717902107 ) ) ;
#26535 = ORIENTED_EDGE ( 'NONE', *, *, #48945, .T. ) ;
#26536 = SURFACE_SIDE_STYLE ('',( #20218 ) ) ;
#26537 = DIRECTION ( 'NONE',  ( -0.000000000000000000, -0.000000000000000000, 1.000000000000000000 ) ) ;
#26538 = CARTESIAN_POINT ( 'NONE',  ( -125.4570736234661723, -9.058813317711329915, 2.943386871421371787 ) ) ;
#26539 = EDGE_CURVE ( 'NONE', #823, #37329, #31929, .T. ) ;
#26540 = VERTEX_POINT ( 'NONE', #22413 ) ;
#26541 = DIRECTION ( 'NONE',  ( 0.000000000000000000, 0.000000000000000000, -1.000000000000000000 ) ) ;
#26542 = CARTESIAN_POINT ( 'NONE',  ( -195.0000000000000000, 1.166476076187852838E-15, -9.524999999999991473 ) ) ;
#26543 = ORIENTED_EDGE ( 'NONE', *, *, #46986, .F. ) ;
#26544 = FILL_AREA_STYLE_COLOUR ( '', #26284 ) ;
#26545 = VERTEX_POINT ( 'NONE', #27664 ) ;
#26546 = FACE_OUTER_BOUND ( 'NONE', #60026, .T. ) ;
#26547 = DIRECTION ( 'NONE',  ( -0.000000000000000000, -0.000000000000000000, -1.000000000000000000 ) ) ;
#26548 = CARTESIAN_POINT ( 'NONE',  ( -157.7070736234661865, -3.094860106618431139, -9.524999999999991473 ) ) ;
#26549 = CARTESIAN_POINT ( 'NONE',  ( -5.598654528085808657, 122.6449999999999960, 7.705886871421373741 ) ) ;
#26550 = CARTESIAN_POINT ( 'NONE',  ( -95.60707362346617799, -8.102448949553172852, 5.886773742842742685 ) ) ;
#26551 = CARTESIAN_POINT ( 'NONE',  ( 57.00000000000000000, 0.000000000000000000, -60.00402776293825724 ) ) ;
#26552 = PRODUCT ( '12. Washer', '12. Washer', '', ( #12132 ) ) ;
#26553 = ORIENTED_EDGE ( 'NONE', *, *, #53078, .F. ) ;
#26555 = FACE_BOUND ( 'NONE', #25158, .T. ) ;
#26554 = DIRECTION ( 'NONE',  ( 1.224646799147353207E-16, 1.000000000000000000, -0.000000000000000000 ) ) ;
#26556 = AXIS2_PLACEMENT_3D ( 'NONE', #56484, #45285, #7952 ) ;
#26557 = CARTESIAN_POINT ( 'NONE',  ( -137.0049999999999670, 6.826472737025116366, 4.959722759717898555 ) ) ;
#26558 = FACE_OUTER_BOUND ( 'NONE', #3668, .T. ) ;
#26559 = CARTESIAN_POINT ( 'NONE',  ( -83.49999999999998579, 4.336808689942018722E-16, -0.000000000000000000 ) ) ;
#26560 = CARTESIAN_POINT ( 'NONE',  ( -158.5449999999999875, -7.632228543268600340, -2.479861379858950166 ) ) ;
#26561 = MECHANICAL_DESIGN_GEOMETRIC_PRESENTATION_REPRESENTATION (  '', ( #56902 ), #22059 ) ;
#26562 = CARTESIAN_POINT ( 'NONE',  ( -137.3949999999999818, -6.826472737025113702, -4.959722759717900331 ) ) ;
#26563 = ORIENTED_EDGE ( 'NONE', *, *, #59471, .F. ) ;
#26564 = EDGE_CURVE ( 'NONE', #38988, #31454, #11510, .T. ) ;
#26565 = LINE ( 'NONE', #57194, #5534 ) ;
#26566 = DIRECTION ( 'NONE',  ( 0.000000000000000000, 1.000000000000000000, -0.000000000000000000 ) ) ;
#26567 = CARTESIAN_POINT ( 'NONE',  ( -57.05499999999999261, -9.827790563157499189E-16, -8.024999999999991473 ) ) ;
#26568 = SURFACE_STYLE_FILL_AREA ( #11438 ) ;
#26569 = STYLED_ITEM ( 'NONE', ( #22377 ), #40225 ) ;
#26570 = DIRECTION ( 'NONE',  ( 0.000000000000000000, 0.000000000000000000, 1.000000000000000000 ) ) ;
#26571 = FILL_AREA_STYLE_COLOUR ( '', #24176 ) ;
#26572 = CARTESIAN_POINT ( 'NONE',  ( -155.3070736234661524, -10.01517768586948698, 6.132527647946031529E-16 ) ) ;
#26573 = CARTESIAN_POINT ( 'NONE',  ( -168.0570736234661808, 0.000000000000000000, 9.524999999999991473 ) ) ;
#26574 = CARTESIAN_POINT ( 'NONE',  ( 5.196152422706628471, -1.107695154586738173, -9.000000000000005329 ) ) ;
#26575 = CARTESIAN_POINT ( 'NONE',  ( -13.25000000000000355, 27.99999999999998934, -3.750000000000000000 ) ) ;
#26576 = VECTOR ( 'NONE', #37499, 1000.000000000000000 ) ;
#26577 = EDGE_CURVE ( 'NONE', #55407, #42594, #4872, .T. ) ;
#26578 = EDGE_CURVE ( 'NONE', #20367, #23192, #37956, .T. ) ;
#26579 = CARTESIAN_POINT ( 'NONE',  ( -2.607480562269157254, 138.0929263765337680, -8.024999999999939959 ) ) ;
#26580 = CARTESIAN_POINT ( 'NONE',  ( 6.999798566743339556, 49.77026365512251971, -7.251305755767528005 ) ) ;
#26581 = ORIENTED_EDGE ( 'NONE', *, *, #702, .T. ) ;
#26582 = CYLINDRICAL_SURFACE ( 'NONE', #15121, 1.000000000000000000 ) ;
#26583 = CARTESIAN_POINT ( 'NONE',  ( 8.437984349512095861, 111.3070736234661524, 1.550032578732817026E-15 ) ) ;
#26584 = EDGE_CURVE ( 'NONE', #57697, #27775, #42891, .T. ) ;
#26585 = LINE ( 'NONE', #15728, #6807 ) ;
#26586 = CARTESIAN_POINT ( 'NONE',  ( 3.749999999999999556, 34.24999999999998579, 3.750000000000000000 ) ) ;
#26587 = DIRECTION ( 'NONE',  ( 0.000000000000000000, 0.000000000000000000, -1.000000000000000000 ) ) ;
#26588 = ADVANCED_FACE ( 'NONE', ( #38292 ), #69236, .T. ) ;
#26589 = EDGE_LOOP ( 'NONE', ( #19444, #32779, #46029, #56820 ) ) ;
#26590 = ORIENTED_EDGE ( 'NONE', *, *, #39502, .F. ) ;
#26591 = STYLED_ITEM ( 'NONE', ( #25006 ), #65394 ) ;
#26592 = CARTESIAN_POINT ( 'NONE',  ( -108.5070736234661695, 8.102448949553176405, 5.886773742842740909 ) ) ;
#26593 = FACE_OUTER_BOUND ( 'NONE', #39885, .T. ) ;
#26594 = CARTESIAN_POINT ( 'NONE',  ( -100.9429263765338050, 0.000000000000000000, 9.524999999999991473 ) ) ;
#26595 = ORIENTED_EDGE ( 'NONE', *, *, #57470, .F. ) ;
#26596 = CARTESIAN_POINT ( 'NONE',  ( 8.102448949553181734, 121.5049999999999670, 5.886773742842750679 ) ) ;
#26597 = SURFACE_STYLE_FILL_AREA ( #42170 ) ;
#26598 = PRESENTATION_LAYER_ASSIGNMENT (  '', '', ( #6381 ) ) ;
#26599 = CARTESIAN_POINT ( 'NONE',  ( 68.99999999999998579, 8.572527594031471415E-15, -3.000000000000000000 ) ) ;
#26600 = ADVANCED_FACE ( 'NONE', ( #32271 ), #55433, .F. ) ;
#26601 = LINE ( 'NONE', #10458, #14862 ) ;
#26602 = CARTESIAN_POINT ( 'NONE',  ( -99.74499999999999034, 4.716976649647094177, 6.492361379858945902 ) ) ;
#26603 = VERTEX_POINT ( 'NONE', #36906 ) ;
#26604 = CARTESIAN_POINT ( 'NONE',  ( 7.971717394532119805, 153.6808681617074228, -3.522481101206686560 ) ) ;
#26605 = DIRECTION ( 'NONE',  ( -0.000000000000000000, -0.000000000000000000, -1.000000000000000000 ) ) ;
#26606 = EDGE_CURVE ( 'NONE', #17311, #60451, #44239, .T. ) ;
#26607 = ORIENTED_EDGE ( 'NONE', *, *, #68287, .F. ) ;
#26608 = CARTESIAN_POINT ( 'NONE',  ( -6.826472737025120807, 159.3929263765338362, -4.959722759717907437 ) ) ;
#26609 =( LENGTH_UNIT ( ) NAMED_UNIT ( * ) SI_UNIT ( .MILLI., .METRE. ) );
#26610 = VECTOR ( 'NONE', #16290, 1000.000000000000000 ) ;
#26611 = SURFACE_STYLE_USAGE ( .BOTH. , #48131 ) ;
#26612 = CARTESIAN_POINT ( 'NONE',  ( 20.99026508940074010, 114.7786387612191703, -10.00000000000000000 ) ) ;
#26613 = VERTEX_POINT ( 'NONE', #15778 ) ;
#26614 = DIRECTION ( 'NONE',  ( 0.000000000000000000, -1.000000000000000000, 0.000000000000000000 ) ) ;
#26615 = LINE ( 'NONE', #10812, #31907 ) ;
#26616 = CARTESIAN_POINT ( 'NONE',  ( -31.68092575729820126, -8.628515624790352945, 6.048998428370452984 ) ) ;
#26617 = DIRECTION ( 'NONE',  ( -0.3361263392814427542, 0.000000000000000000, 0.9418169057949938860 ) ) ;
#26618 = CARTESIAN_POINT ( 'NONE',  ( 17.25000000000000711, 24.74999999999997868, 4.000000000000000000 ) ) ;
#26619 = DIRECTION ( 'NONE',  ( 0.000000000000000000, 1.000000000000000000, -0.000000000000000000 ) ) ;
#26620 = CARTESIAN_POINT ( 'NONE',  ( 2.607480562269034241, 116.7929263765338135, -8.025000000000032330 ) ) ;
#26621 = CARTESIAN_POINT ( 'NONE',  ( -8.154247983011970291, 153.6870150848094170, 3.079081823141356367 ) ) ;
#26622 = ORIENTED_EDGE ( 'NONE', *, *, #56688, .T. ) ;
#26623 = ORIENTED_EDGE ( 'NONE', *, *, #18006, .T. ) ;
#26624 = DIRECTION ( 'NONE',  ( 1.000000000000000000, -0.000000000000000000, 0.000000000000000000 ) ) ;
#26625 = DIRECTION ( 'NONE',  ( -0.000000000000000000, -1.000000000000000000, -0.000000000000000000 ) ) ;
#26626 = CARTESIAN_POINT ( 'NONE',  ( -74.99999999999998579, 50.00000000000000000, -12.00000000000000000 ) ) ;
#26627 = DIRECTION ( 'NONE',  ( -0.000000000000000000, -0.000000000000000000, -1.000000000000000000 ) ) ;
#26628 = ORIENTED_EDGE ( 'NONE', *, *, #41034, .F. ) ;
#26629 = CARTESIAN_POINT ( 'NONE',  ( -165.5049999999999955, -6.826472737025115478, -4.959722759717899443 ) ) ;
#26630 = SURFACE_STYLE_USAGE ( .BOTH. , #48153 ) ;
#26631 = CARTESIAN_POINT ( 'NONE',  ( 0.000000000000000000, 2.500000000000000000, 0.000000000000000000 ) ) ;
#26632 = CARTESIAN_POINT ( 'NONE',  ( -180.4449999999999932, 0.000000000000000000, 8.024999999999991473 ) ) ;
#26633 = CARTESIAN_POINT ( 'NONE',  ( -165.2949999999999591, -2.607480562269069768, 8.024999999999991473 ) ) ;
#26634 = VERTEX_POINT ( 'NONE', #58320 ) ;
#26635 = EDGE_CURVE ( 'NONE', #25571, #16642, #13868, .T. ) ;
#26636 = CARTESIAN_POINT ( 'NONE',  ( 9.985360875542992787, 0.7048476316490956961, 0.9853608755428859833 ) ) ;
#26637 = CARTESIAN_POINT ( 'NONE',  ( -37.58704975911827262, -10.98121406184487192, 3.676737808024616694 ) ) ;
#26638 = DIRECTION ( 'NONE',  ( 1.000000000000000000, -0.000000000000000000, 0.000000000000000000 ) ) ;
#26639 = CARTESIAN_POINT ( 'NONE',  ( -87.50499999999995282, -6.826472737025115478, -4.959722759717899443 ) ) ;
#26640 = CARTESIAN_POINT ( 'NONE',  ( 23.67249405129376072, 27.44083605074020937, 27.18966959687858775 ) ) ;
#26641 = CARTESIAN_POINT ( 'NONE',  ( -75.47338799120147712, 36.01293665759187235, -9.580134848782680734 ) ) ;
#26642 = PRESENTATION_LAYER_ASSIGNMENT (  '', '', ( #62605 ) ) ;
#26643 = VECTOR ( 'NONE', #3773, 1000.000000000000000 ) ;
#26644 = CARTESIAN_POINT ( 'NONE',  ( -77.39499999999999602, -6.826472737025113702, -4.959722759717900331 ) ) ;
#26645 = CARTESIAN_POINT ( 'NONE',  ( -10.01517768586949231, 138.3049999999999500, -6.132527647946036459E-16 ) ) ;
#26646 = STYLED_ITEM ( 'NONE', ( #67930 ), #3751 ) ;
#26647 = PLANE ( 'NONE',  #12887 ) ;
#26648 = FACE_OUTER_BOUND ( 'NONE', #11166, .T. ) ;
#26649 = CARTESIAN_POINT ( 'NONE',  ( -74.99292637653380211, 8.102448949553172852, -5.886773742842744461 ) ) ;
#26650 = EDGE_LOOP ( 'NONE', ( #11728, #9670, #3229, #35176 ) ) ;
#26651 = EDGE_CURVE ( 'NONE', #12948, #35810, #17271, .T. ) ;
#26652 = CARTESIAN_POINT ( 'NONE',  ( 7.441974819423174736, -2.003239292658530513, -1.110121504110836987 ) ) ;
#26653 = COLOUR_RGB ( '', 0.08235294, 0.09019608, 0.10196078) ;
#26654 = ADVANCED_FACE ( 'NONE', ( #6236 ), #64432, .F. ) ;
#26655 = VECTOR ( 'NONE', #42589, 1000.000000000000000 ) ;
#26656 = ADVANCED_FACE ( 'NONE', ( #26297 ), #66689, .T. ) ;
#26657 = PRESENTATION_STYLE_ASSIGNMENT (( #4515 ) ) ;
#26658 = ADVANCED_FACE ( 'NONE', ( #22075 ), #54328, .F. ) ;
#26660 = CARTESIAN_POINT ( 'NONE',  ( 5.590169943749474513, 0.000000000000000000, 4.999999999999999112 ) ) ;
#26659 = CARTESIAN_POINT ( 'NONE',  ( -15.79964225816357626, 58.31681314173472686, -6.349999999999996092 ) ) ;
#26661 = ORIENTED_EDGE ( 'NONE', *, *, #51084, .T. ) ;
#26662 = ORIENTED_EDGE ( 'NONE', *, *, #11446, .T. ) ;
#26663 = CARTESIAN_POINT ( 'NONE',  ( -71.49999999999998579, 64.07124727947029896, -9.500000000000000000 ) ) ;
#26664 = CARTESIAN_POINT ( 'NONE',  ( -134.9929263765338021, 8.102448949553172852, -5.886773742842744461 ) ) ;
#26665 = CARTESIAN_POINT ( 'NONE',  ( -120.0570736234661808, 0.000000000000000000, 9.524999999999991473 ) ) ;
#26666 = CARTESIAN_POINT ( 'NONE',  ( 60.00000000000000000, 117.4999999999999716, -9.500000000000000000 ) ) ;
#26667 = DIRECTION ( 'NONE',  ( -1.000000000000000000, 0.000000000000000000, 0.000000000000000000 ) ) ;
#26668 = EDGE_CURVE ( 'NONE', #23152, #1324, #39318, .T. ) ;
#26669 = ORIENTED_EDGE ( 'NONE', *, *, #60219, .F. ) ;
#26670 = CARTESIAN_POINT ( 'NONE',  ( -124.2549999999999955, -4.716976649647092401, 6.492361379858946790 ) ) ;
#26671 = ORIENTED_EDGE ( 'NONE', *, *, #51536, .T. ) ;
#26672 =( LENGTH_UNIT ( ) NAMED_UNIT ( * ) SI_UNIT ( .MILLI., .METRE. ) );
#26673 = CARTESIAN_POINT ( 'NONE',  ( 20.77811424250900174, 115.1386898118646656, -10.00000000000000000 ) ) ;
#26674 = ORIENTED_EDGE ( 'NONE', *, *, #68161, .F. ) ;
#26675 = CARTESIAN_POINT ( 'NONE',  ( -71.18918918918917882, 14.09971791521133255, -7.000000000000000000 ) ) ;
#26676 = CARTESIAN_POINT ( 'NONE',  ( -15.98999599679679839, 146.4999999999999716, -7.500000000000000000 ) ) ;
#26677 = ORIENTED_EDGE ( 'NONE', *, *, #42934, .F. ) ;
#26678 = SURFACE_STYLE_USAGE ( .BOTH. , #69610 ) ;
#26679 = CARTESIAN_POINT ( 'NONE',  ( 3.094860106618431583, 150.0949999999999420, 9.525000000000000355 ) ) ;
#26680 = DIRECTION ( 'NONE',  ( -1.000000000000000000, 0.000000000000000000, 0.000000000000000000 ) ) ;
#26681 = VERTEX_POINT ( 'NONE', #54746 ) ;
#26682 = CARTESIAN_POINT ( 'NONE',  ( -1.804616585955809649, 2.331456807317426438, 9.000000000000000000 ) ) ;
#26683 = DIRECTION ( 'NONE',  ( -1.000000000000000000, 0.000000000000000000, 0.000000000000000000 ) ) ;
#26684 = PRESENTATION_LAYER_ASSIGNMENT (  '', '', ( #3047 ) ) ;
#26685 = CYLINDRICAL_SURFACE ( 'NONE', #67844, 9.524999999999991473 ) ;
#26686 = ORIENTED_EDGE ( 'NONE', *, *, #3633, .F. ) ;
#26687 = CARTESIAN_POINT ( 'NONE',  ( -4.716976649647098618, 130.1429263765338362, 6.492361379858953008 ) ) ;
#26688 = DIRECTION ( 'NONE',  ( 1.000000000000000000, 0.000000000000000000, 0.000000000000000000 ) ) ;
#26689 = CARTESIAN_POINT ( 'NONE',  ( -74.69171475799898019, 36.40799980539631520, -10.00000000000000000 ) ) ;
#26690 = CONICAL_SURFACE ( 'NONE', #22251, 4.999999999999997335, 0.7853981633974587151 ) ;
#26691 = DIRECTION ( 'NONE',  ( 0.000000000000000000, -1.000000000000000000, 0.000000000000000000 ) ) ;
#26692 = FILL_AREA_STYLE_COLOUR ( '', #56830 ) ;
#26693 = EDGE_CURVE ( 'NONE', #9552, #33374, #20704, .T. ) ;
#26694 = ORIENTED_EDGE ( 'NONE', *, *, #45647, .F. ) ;
#26695 = DIRECTION ( 'NONE',  ( -0.000000000000000000, 1.000000000000000000, -0.000000000000000000 ) ) ;
#26696 = ORIENTED_EDGE ( 'NONE', *, *, #44376, .F. ) ;
#26697 = CARTESIAN_POINT ( 'NONE',  ( -51.44292637653380496, -1.166476076187852838E-15, -9.524999999999991473 ) ) ;
#26698 = DIRECTION ( 'NONE',  ( 1.000000000000000000, 0.000000000000000000, 0.000000000000000000 ) ) ;
#26699 = LINE ( 'NONE', #30600, #38599 ) ;
#26700 = CONICAL_SURFACE ( 'NONE', #51430, 3.000000000000000444, 0.7853981633974517207 ) ;
#26701 = CARTESIAN_POINT ( 'NONE',  ( -143.9050000000000011, 2.607480562269068880, -8.024999999999993250 ) ) ;
#26702 = DIRECTION ( 'NONE',  ( 0.000000000000000000, 0.000000000000000000, -1.000000000000000000 ) ) ;
#26703 = EDGE_CURVE ( 'NONE', #10139, #8806, #65669, .T. ) ;
#26704 =( NAMED_UNIT ( * ) SI_UNIT ( $, .STERADIAN. ) SOLID_ANGLE_UNIT ( ) );
#26705 = DIRECTION ( 'NONE',  ( -0.000000000000000000, 1.000000000000000000, -0.000000000000000000 ) ) ;
#26706 = CYLINDRICAL_SURFACE ( 'NONE', #36139, 13.00000000000000178 ) ;
#26707 = DIRECTION ( 'NONE',  ( -0.000000000000000000, 0.000000000000000000, -1.000000000000000000 ) ) ;
#26708 = VERTEX_POINT ( 'NONE', #61081 ) ;
#26709 = CIRCLE ( 'NONE', #66033, 0.5000000000000004441 ) ;
#26710 = ORIENTED_EDGE ( 'NONE', *, *, #48415, .T. ) ;
#26711 = DIRECTION ( 'NONE',  ( 0.000000000000000000, 0.000000000000000000, 1.000000000000000000 ) ) ;
#26712 = PRESENTATION_LAYER_ASSIGNMENT (  '', '', ( #21112 ) ) ;
#26713 = CARTESIAN_POINT ( 'NONE',  ( -4.357963766315032572, 1.733608113333017453, 6.451785339198141678 ) ) ;
#26714 = CARTESIAN_POINT ( 'NONE',  ( -59.00499999999998124, 6.826472737025116366, 4.959722759717898555 ) ) ;
#26715 = ORIENTED_EDGE ( 'NONE', *, *, #63830, .T. ) ;
#26716 = CYLINDRICAL_SURFACE ( 'NONE', #5635, 0.2500000000000002220 ) ;
#26717 = CARTESIAN_POINT ( 'NONE',  ( -28.03849660521344234, -8.499999999999996447, 0.9189689155263818243 ) ) ;
#26718 = DIRECTION ( 'NONE',  ( -0.000000000000000000, -1.000000000000000000, -0.000000000000000000 ) ) ;
#26719 = LINE ( 'NONE', #48596, #41929 ) ;
#26720 = CARTESIAN_POINT ( 'NONE',  ( -128.0929263765345070, 3.094860106630465957, 9.524999999991248245 ) ) ;
#26721 = VERTEX_POINT ( 'NONE', #7613 ) ;
#26722 =( NAMED_UNIT ( * ) SI_UNIT ( $, .STERADIAN. ) SOLID_ANGLE_UNIT ( ) );
#26723 =( NAMED_UNIT ( * ) PLANE_ANGLE_UNIT ( ) SI_UNIT ( $, .RADIAN. ) );
#26724 = CARTESIAN_POINT ( 'NONE',  ( 7.632228543268608334, 126.4570736234661723, -2.479861379858951942 ) ) ;
#26725 = CARTESIAN_POINT ( 'NONE',  ( -111.5949999999999704, 2.607480562269072433, 8.024999999999991473 ) ) ;
#26726 = CARTESIAN_POINT ( 'NONE',  ( -9.058813317711337021, 158.0449999999999875, -2.943386871421374895 ) ) ;
#26727 = CARTESIAN_POINT ( 'NONE',  ( -86.84499999999998465, -7.632228543268599452, 2.479861379858951054 ) ) ;
#26728 = ADVANCED_FACE ( 'NONE', ( #49859 ), #35256, .T. ) ;
#26729 = CARTESIAN_POINT ( 'NONE',  ( 29.00000000000000000, 43.00000000000000000, -89.00000000000000000 ) ) ;
#26730 = CYLINDRICAL_SURFACE ( 'NONE', #19036, 9.524999999999991473 ) ;
#26731 = CARTESIAN_POINT ( 'NONE',  ( -190.0000000000000000, 0.000000000000000000, 5.499999999999984901 ) ) ;
#26732 = VERTEX_POINT ( 'NONE', #60046 ) ;
#26733 = EDGE_CURVE ( 'NONE', #529, #20746, #6927, .T. ) ;
#26734 = CARTESIAN_POINT ( 'NONE',  ( -135.2929263765337851, 3.094860106618428031, -9.524999999999993250 ) ) ;
#26735 =( LENGTH_UNIT ( ) NAMED_UNIT ( * ) SI_UNIT ( .MILLI., .METRE. ) );
#26736 = CARTESIAN_POINT ( 'NONE',  ( -148.3449999999999989, 7.632228543268599452, -2.479861379858951942 ) ) ;
#26737 = CARTESIAN_POINT ( 'NONE',  ( -195.0000000000000000, 0.000000000000000000, 0.000000000000000000 ) ) ;
#26738 = AXIS2_PLACEMENT_3D ( 'NONE', #54906, #59156, #38465 ) ;
#26739 = MECHANICAL_DESIGN_GEOMETRIC_PRESENTATION_REPRESENTATION (  '', ( #866 ), #44789 ) ;
#26740 = EDGE_CURVE ( 'NONE', #55502, #12157, #28714, .T. ) ;
#26741 = CARTESIAN_POINT ( 'NONE',  ( -48.59499999999997044, 2.607480562269072433, 8.024999999999991473 ) ) ;
#26742 = SURFACE_STYLE_USAGE ( .BOTH. , #1363 ) ;
#26743 = VERTEX_POINT ( 'NONE', #56142 ) ;
#26744 = AXIS2_PLACEMENT_3D ( 'NONE', #56797, #18798, #34296 ) ;
#26745 = ORIENTED_EDGE ( 'NONE', *, *, #33508, .F. ) ;
#26746 = PRESENTATION_LAYER_ASSIGNMENT (  '', '', ( #39164 ) ) ;
#26747 = DIRECTION ( 'NONE',  ( 1.000000000000000000, 0.000000000000000000, 0.000000000000000000 ) ) ;
#26748 = LINE ( 'NONE', #9925, #65256 ) ;
#26749 = AXIS2_PLACEMENT_3D ( 'NONE', #11949, #22864, #49951 ) ;
#26750 = SURFACE_SIDE_STYLE ('',( #38428 ) ) ;
#26752 = EDGE_CURVE ( 'NONE', #8903, #37997, #34148, .T. ) ;
#26751 = SURFACE_STYLE_FILL_AREA ( #5647 ) ;
#26753 = ORIENTED_EDGE ( 'NONE', *, *, #37615, .F. ) ;
#26754 = CARTESIAN_POINT ( 'NONE',  ( -148.1049999999999898, -6.826472737025113702, 4.959722759717902107 ) ) ;
#26755 = EDGE_LOOP ( 'NONE', ( #18345, #14802, #52507, #61455 ) ) ;
#26756 = CARTESIAN_POINT ( 'NONE',  ( 4.358330484967979146, 6.451150163859158404, 0.7660251680141578756 ) ) ;
#26757 = CARTESIAN_POINT ( 'NONE',  ( -141.9570736234661865, 9.058813317711329915, -2.943386871421373119 ) ) ;
#26758 = ORIENTED_EDGE ( 'NONE', *, *, #27279, .F. ) ;
#26759 = SURFACE_STYLE_USAGE ( .BOTH. , #42664 ) ;
#26760 = CARTESIAN_POINT ( 'NONE',  ( 45.07697505292422591, 10.02565835097472480, 3.091949714863343246 ) ) ;
#26761 = CARTESIAN_POINT ( 'NONE',  ( -10.01517768586949231, 122.1949999999999648, -6.132527647946036459E-16 ) ) ;
#26762 = ORIENTED_EDGE ( 'NONE', *, *, #43270, .F. ) ;
#26763 = CARTESIAN_POINT ( 'NONE',  ( 5.598654528085809545, 122.2549999999999955, -7.705886871421373741 ) ) ;
#26764 = CARTESIAN_POINT ( 'NONE',  ( -68.00499999999998124, 6.826472737025115478, 4.959722759717899443 ) ) ;
#26765 = CIRCLE ( 'NONE', #41429, 0.5000000000000004441 ) ;
#26766 = CARTESIAN_POINT ( 'NONE',  ( -118.3449999999999989, 7.632228543268599452, -2.479861379858951942 ) ) ;
#26767 = CARTESIAN_POINT ( 'NONE',  ( -40.99999999999998579, 107.7459666924148394, -3.000000000000003109 ) ) ;
#26768 = ORIENTED_EDGE ( 'NONE', *, *, #14530, .F. ) ;
#26769 = CARTESIAN_POINT ( 'NONE',  ( 9.058813317711337021, 145.6549999999999727, 2.943386871421375783 ) ) ;
#26770 = DIRECTION ( 'NONE',  ( 1.000000000000000000, 0.000000000000000000, 0.000000000000000000 ) ) ;
#26771 = FACE_OUTER_BOUND ( 'NONE', #63956, .T. ) ;
#26772 = CIRCLE ( 'NONE', #44811, 12.50000000000000178 ) ;
#26773 = SURFACE_STYLE_FILL_AREA ( #58137 ) ;
#26774 = FILL_AREA_STYLE_COLOUR ( '', #28679 ) ;
#26775 = ORIENTED_EDGE ( 'NONE', *, *, #30807, .T. ) ;
#26776 = VECTOR ( 'NONE', #10276, 1000.000000000000000 ) ;
#26777 = CARTESIAN_POINT ( 'NONE',  ( -33.70169882663748950, -9.480064694312421381, -3.454096298675830123 ) ) ;
#26778 = SURFACE_STYLE_FILL_AREA ( #58825 ) ;
#26779 = CARTESIAN_POINT ( 'NONE',  ( -169.8550000000000182, 4.716976649647094177, 6.492361379858945902 ) ) ;
#26780 = ORIENTED_EDGE ( 'NONE', *, *, #23669, .T. ) ;
#26781 = CARTESIAN_POINT ( 'NONE',  ( 0.9728900412908074724, 111.9999999999999858, -7.965808808122197604 ) ) ;
#26782 = MECHANICAL_DESIGN_GEOMETRIC_PRESENTATION_REPRESENTATION (  '', ( #9958 ), #35797 ) ;
#26783 = DIRECTION ( 'NONE',  ( 0.000000000000000000, -0.000000000000000000, 1.000000000000000000 ) ) ;
#26784 = CARTESIAN_POINT ( 'NONE',  ( 7.794228634059945371, -2.500000000000000000, 4.500000000000000888 ) ) ;
#26785 = LINE ( 'NONE', #64799, #6253 ) ;
#26786 = ORIENTED_EDGE ( 'NONE', *, *, #6524, .F. ) ;
#26787 = MECHANICAL_DESIGN_GEOMETRIC_PRESENTATION_REPRESENTATION (  '', ( #39199 ), #11088 ) ;
#26788 = CARTESIAN_POINT ( 'NONE',  ( -97.25499999999999545, -4.716976649647092401, 6.492361379858946790 ) ) ;
#26789 = ORIENTED_EDGE ( 'NONE', *, *, #64526, .T. ) ;
#26790 = DIRECTION ( 'NONE',  ( 0.000000000000000000, -1.000000000000000000, 0.000000000000000000 ) ) ;
#26791 = CARTESIAN_POINT ( 'NONE',  ( -44.99999999999998579, 119.9999999999999716, -10.00000000000000000 ) ) ;
#26792 = CARTESIAN_POINT ( 'NONE',  ( -129.3570736234661922, 5.598654528085804216, 7.705886871421366635 ) ) ;
#26793 = CARTESIAN_POINT ( 'NONE',  ( -24.21231517720798010, 113.4999999999999858, 7.500000000000000000 ) ) ;
#26794 = CARTESIAN_POINT ( 'NONE',  ( -65.90707362346617515, -3.094860106618429807, 9.524999999999991473 ) ) ;
#26795 = CARTESIAN_POINT ( 'NONE',  ( -48.00000000000000000, 14.49137674618942562, -7.500000000000000000 ) ) ;
#26796 = ORIENTED_EDGE ( 'NONE', *, *, #40763, .F. ) ;
#26797 = CARTESIAN_POINT ( 'NONE',  ( 15.48999599679679662, 118.4999999999999716, 7.500000000000000000 ) ) ;
#26798 = TOROIDAL_SURFACE ( 'NONE', #27947, 0.5000000000000000000, 0.2500000000000000000 ) ;
#26800 = DIRECTION ( 'NONE',  ( -1.000000000000000000, 0.000000000000000000, 0.000000000000000000 ) ) ;
#26799 =( NAMED_UNIT ( * ) SI_UNIT ( $, .STERADIAN. ) SOLID_ANGLE_UNIT ( ) );
#26801 = CARTESIAN_POINT ( 'NONE',  ( -108.8049999999999784, -8.437984349512085203, 5.166775262442717831E-16 ) ) ;
#26802 = CARTESIAN_POINT ( 'NONE',  ( 0.000000000000000000, 124.4449999999999932, -9.525000000000000355 ) ) ;
#26803 = CARTESIAN_POINT ( 'NONE',  ( -113.2449999999999903, -4.716976649647093289, -6.492361379858945902 ) ) ;
#26804 = ADVANCED_FACE ( 'NONE', ( #18536 ), #22771, .T. ) ;
#26805 = PRESENTATION_STYLE_ASSIGNMENT (( #16329 ) ) ;
#26806 = ORIENTED_EDGE ( 'NONE', *, *, #52842, .F. ) ;
#26807 = CARTESIAN_POINT ( 'NONE',  ( -166.0429263765338135, -9.058813317711329915, -2.943386871421370898 ) ) ;
#26808 = CARTESIAN_POINT ( 'NONE',  ( -171.7450000000000045, 4.716976649647094177, 6.492361379858945902 ) ) ;
#26809 = ADVANCED_FACE ( 'NONE', ( #60381 ), #53254, .T. ) ;
#26810 = VECTOR ( 'NONE', #6150, 1000.000000000000000 ) ;
#26811 = ADVANCED_FACE ( 'NONE', ( #44270 ), #29414, .T. ) ;
#26812 = CARTESIAN_POINT ( 'NONE',  ( -151.9429263765338192, 0.000000000000000000, 9.524999999999991473 ) ) ;
#26813 = EDGE_CURVE ( 'NONE', #32066, #51449, #60692, .T. ) ;
#26814 = MECHANICAL_DESIGN_GEOMETRIC_PRESENTATION_REPRESENTATION (  '', ( #54895 ), #34668 ) ;
#26815 = AXIS2_PLACEMENT_3D ( 'NONE', #67537, #9160, #55939 ) ;
#26816 = DIRECTION ( 'NONE',  ( -1.000000000000000000, 0.000000000000000000, 0.000000000000000000 ) ) ;
#26817 = CARTESIAN_POINT ( 'NONE',  ( 71.50000000000000000, 35.92875272052971525, 7.500000000000000000 ) ) ;
#26818 = ORIENTED_EDGE ( 'NONE', *, *, #46986, .T. ) ;
#26819 = EDGE_CURVE ( 'NONE', #32974, #11830, #46557, .T. ) ;
#26820 = CARTESIAN_POINT ( 'NONE',  ( -76.94292637653380496, 0.000000000000000000, 9.524999999999991473 ) ) ;
#26821 = ITEM_DEFINED_TRANSFORMATION ( 'NONE', 'NONE', #9052,  #42840 ) ;
#26822 = CIRCLE ( 'NONE', #12219, 5.500000000000005329 ) ;
#26823 = DIRECTION ( 'NONE',  ( 1.000000000000000000, -1.189524669241239115E-16, 0.000000000000000000 ) ) ;
#26824 =( NAMED_UNIT ( * ) SI_UNIT ( $, .STERADIAN. ) SOLID_ANGLE_UNIT ( ) );
#26825 = EDGE_CURVE ( 'NONE', #15954, #41524, #8352, .T. ) ;
#26826 = CARTESIAN_POINT ( 'NONE',  ( -84.49999999999998579, -2.499999999999999556, 24.00000000000000000 ) ) ;
#26827 = CARTESIAN_POINT ( 'NONE',  ( 39.74999999999999289, 18.74999999999997868, 3.750000000000000000 ) ) ;
#26828 = CARTESIAN_POINT ( 'NONE',  ( -74.75000000000000000, -0.9999999999999995559, 7.000000000000001776 ) ) ;
#26829 = PRESENTATION_LAYER_ASSIGNMENT (  '', '', ( #25751 ) ) ;
#26830 = ORIENTED_EDGE ( 'NONE', *, *, #46109, .T. ) ;
#26831 = CARTESIAN_POINT ( 'NONE',  ( -74.75707362346616947, -5.598654528085801552, 7.705886871421367523 ) ) ;
#26832 = SURFACE_SIDE_STYLE ('',( #32845 ) ) ;
#26833 = CARTESIAN_POINT ( 'NONE',  ( 7.632228543268607446, 147.1570736234661751, 2.479861379858954606 ) ) ;
#26834 = ORIENTED_EDGE ( 'NONE', *, *, #12485, .T. ) ;
#26835 = CARTESIAN_POINT ( 'NONE',  ( 44.79289321881345387, 10.55564175590368059, -3.499999999999999112 ) ) ;
#26836 = CARTESIAN_POINT ( 'NONE',  ( -93.50499999999999545, -6.826472737025113702, -4.959722759717900331 ) ) ;
#26837 = AXIS2_PLACEMENT_3D ( 'NONE', #66276, #49431, #11782 ) ;
#26838 =( LENGTH_UNIT ( ) NAMED_UNIT ( * ) SI_UNIT ( .MILLI., .METRE. ) );
#26839 = EDGE_LOOP ( 'NONE', ( #14490, #64288, #44048, #47391 ) ) ;
#26840 = DIRECTION ( 'NONE',  ( 0.000000000000000000, 0.000000000000000000, 1.000000000000000000 ) ) ;
#26841 = CARTESIAN_POINT ( 'NONE',  ( 108.3664351561509278, 1.000000000000000000, 18.43563588791581509 ) ) ;
#26842 = SURFACE_STYLE_FILL_AREA ( #54647 ) ;
#26843 = DIRECTION ( 'NONE',  ( 1.000000000000000000, -0.000000000000000000, -1.300977106640434891E-16 ) ) ;
#26844 = MANIFOLD_SOLID_BREP ( 'Fillet1', #14923 ) ;
#26845 = CARTESIAN_POINT ( 'NONE',  ( 23.50000000000001776, 27.44010416289936316, -27.18999999999999417 ) ) ;
#26846 = EDGE_LOOP ( 'NONE', ( #15809, #54266, #45269, #25589 ) ) ;
#26847 = AXIS2_PLACEMENT_3D ( 'NONE', #23099, #44588, #50180 ) ;
#26849 = CARTESIAN_POINT ( 'NONE',  ( -76.49500000000000455, 6.826472737025113702, -4.959722759717902107 ) ) ;
#26848 = MECHANICAL_DESIGN_GEOMETRIC_PRESENTATION_REPRESENTATION (  '', ( #53843 ), #3285 ) ;
#26850 = EDGE_LOOP ( 'NONE', ( #61119, #66143, #19760, #1364 ) ) ;
#26851 = CARTESIAN_POINT ( 'NONE',  ( 15.48999599679679662, 117.9999999999999716, -9.500000000000000000 ) ) ;
#26852 = LINE ( 'NONE', #81, #61106 ) ;
#26853 = PRESENTATION_LAYER_ASSIGNMENT (  '', '', ( #52774 ) ) ;
#26854 = ORIENTED_EDGE ( 'NONE', *, *, #3541, .T. ) ;
#26855 = SURFACE_STYLE_USAGE ( .BOTH. , #53959 ) ;
#26856 = LINE ( 'NONE', #33558, #58424 ) ;
#26857 = CARTESIAN_POINT ( 'NONE',  ( -4.250000000000001776, 21.74999999999998579, -4.000000000000000000 ) ) ;
#26858 = CARTESIAN_POINT ( 'NONE',  ( -123.3549999999999898, -4.716976649647093289, -6.492361379858945902 ) ) ;
#26859 = ORIENTED_EDGE ( 'NONE', *, *, #62333, .F. ) ;
#26860 = CARTESIAN_POINT ( 'NONE',  ( -73.19292637653379074, -10.01517768586948698, 6.132527647946031529E-16 ) ) ;
#26861 = VERTEX_POINT ( 'NONE', #35753 ) ;
#26862 = AXIS2_PLACEMENT_3D ( 'NONE', #66727, #1930, #40349 ) ;
#26863 = CARTESIAN_POINT ( 'NONE',  ( 0.000000000000000000, 2.500000000000000000, 0.000000000000000000 ) ) ;
#26864 = CARTESIAN_POINT ( 'NONE',  ( -24.75000000000000355, 37.00000000000000000, 3.000000000000000000 ) ) ;
#26865 = PRESENTATION_STYLE_ASSIGNMENT (( #37520 ) ) ;
#26866 = AXIS2_PLACEMENT_3D ( 'NONE', #56898, #14326, #40062 ) ;
#26867 = CARTESIAN_POINT ( 'NONE',  ( -163.4070736234661467, 3.094860106618428031, -9.524999999999993250 ) ) ;
#26868 = CIRCLE ( 'NONE', #63952, 0.2500000000000002220 ) ;
#26869 = CARTESIAN_POINT ( 'NONE',  ( -8.102448949553179958, 122.4949999999999903, 5.886773742842747126 ) ) ;
#26870 = AXIS2_PLACEMENT_3D ( 'NONE', #18773, #36394, #52203 ) ;
#26871 = CARTESIAN_POINT ( 'NONE',  ( -92.15707362346617515, -9.058813317711329915, -2.943386871421370898 ) ) ;
#26872 = CIRCLE ( 'NONE', #60573, 0.2500000000000002220 ) ;
#26873 = AXIS2_PLACEMENT_3D ( 'NONE', #12091, #54992, #33895 ) ;
#26874 = ORIENTED_EDGE ( 'NONE', *, *, #728, .T. ) ;
#26875 = SURFACE_SIDE_STYLE ('',( #48075 ) ) ;
#26877 = FACE_OUTER_BOUND ( 'NONE', #2512, .T. ) ;
#26876 = DIRECTION ( 'NONE',  ( 0.000000000000000000, 0.000000000000000000, -1.000000000000000000 ) ) ;
#26878 = CARTESIAN_POINT ( 'NONE',  ( 74.49999999999998579, 119.9999999999997584, -9.500000000000000000 ) ) ;
#26879 = CARTESIAN_POINT ( 'NONE',  ( -141.2050000000000125, -2.607480562269071545, -8.024999999999991473 ) ) ;
#26880 = PRESENTATION_STYLE_ASSIGNMENT (( #5111 ) ) ;
#26881 = CARTESIAN_POINT ( 'NONE',  ( 26.00000000000001776, 42.00000000000000000, 34.49999999999999289 ) ) ;
#26882 = CARTESIAN_POINT ( 'NONE',  ( 0.000000000000000000, 115.4999999999999574, 0.000000000000000000 ) ) ;
#26883 = CARTESIAN_POINT ( 'NONE',  ( -141.7450000000000045, 4.716976649647094177, 6.492361379858945902 ) ) ;
#26884 = ADVANCED_FACE ( 'NONE', ( #19195 ), #46705, .T. ) ;
#26885 =( GEOMETRIC_REPRESENTATION_CONTEXT ( 3 ) GLOBAL_UNCERTAINTY_ASSIGNED_CONTEXT ( ( #941 ) ) GLOBAL_UNIT_ASSIGNED_CONTEXT ( ( #61585, #35591, #51416 ) ) REPRESENTATION_CONTEXT ( 'NONE', 'WORKASPACE' ) );
#26886 = CARTESIAN_POINT ( 'NONE',  ( -139.6449999999999818, 4.716976649647091513, -6.492361379858946790 ) ) ;
#26887 = ORIENTED_EDGE ( 'NONE', *, *, #30301, .T. ) ;
#26888 = VECTOR ( 'NONE', #19910, 1000.000000000000000 ) ;
#26889 = EDGE_CURVE ( 'NONE', #18076, #15891, #30773, .T. ) ;
#26890 =( NAMED_UNIT ( * ) SI_UNIT ( $, .STERADIAN. ) SOLID_ANGLE_UNIT ( ) );
#26891 = CARTESIAN_POINT ( 'NONE',  ( -22.75000000000000711, 36.75000000000000000, 3.750000000000000000 ) ) ;
#26892 = UNCERTAINTY_MEASURE_WITH_UNIT (LENGTH_MEASURE( 1.000000000000000082E-05 ), #67394, 'distance_accuracy_value', 'NONE');
#26893 = CARTESIAN_POINT ( 'NONE',  ( -53.00500000000000256, 6.826472737025116366, 4.959722759717898555 ) ) ;
#26894 = PRESENTATION_LAYER_ASSIGNMENT (  '', '', ( #17947 ) ) ;
#26895 =( LENGTH_UNIT ( ) NAMED_UNIT ( * ) SI_UNIT ( .MILLI., .METRE. ) );
#26896 = LINE ( 'NONE', #38582, #51121 ) ;
#26897 = EDGE_CURVE ( 'NONE', #53553, #59113, #69483, .T. ) ;
#26898 = CARTESIAN_POINT ( 'NONE',  ( -6.021969435454500363, -1.863712308906140258, 7.569642976165947168 ) ) ;
#26899 = AXIS2_PLACEMENT_3D ( 'NONE', #63673, #42288, #46870 ) ;
#26900 = CARTESIAN_POINT ( 'NONE',  ( -108.4429263765338050, -1.166476076187852838E-15, -9.524999999999991473 ) ) ;
#26901 = DIRECTION ( 'NONE',  ( -1.132643588934172738E-16, 1.000000000000000000, -1.473213661637684397E-17 ) ) ;
#26902 = CARTESIAN_POINT ( 'NONE',  ( -152.2429263765338021, 5.598654528085804216, 7.705886871421366635 ) ) ;
#26903 = AXIS2_PLACEMENT_3D ( 'NONE', #46173, #20078, #47224 ) ;
#26904 = EDGE_CURVE ( 'NONE', #31124, #5413, #10564, .T. ) ;
#26905 = CARTESIAN_POINT ( 'NONE',  ( -65.49999999999998579, 50.00000000000000000, 10.50000000000000000 ) ) ;
#26906 = CARTESIAN_POINT ( 'NONE',  ( -99.65707362346617515, 9.058813317711329915, 2.943386871421369566 ) ) ;
#26907 =( NAMED_UNIT ( * ) PLANE_ANGLE_UNIT ( ) SI_UNIT ( $, .RADIAN. ) );
#26908 = VECTOR ( 'NONE', #3088, 1000.000000000000000 ) ;
#26909 = CARTESIAN_POINT ( 'NONE',  ( 60.00000000000000000, 1.797044900979284448E-15, 12.00000000000000000 ) ) ;
#26910 = VECTOR ( 'NONE', #59454, 1000.000000000000000 ) ;
#26911 = ORIENTED_EDGE ( 'NONE', *, *, #31186, .F. ) ;
#26912 = FACE_OUTER_BOUND ( 'NONE', #50201, .T. ) ;
#26913 = AXIS2_PLACEMENT_3D ( 'NONE', #9926, #32743, #32380 ) ;
#26914 = CARTESIAN_POINT ( 'NONE',  ( -8.437984349512095861, 112.8070736234661524, -5.166775262442723748E-16 ) ) ;
#26915 =( GEOMETRIC_REPRESENTATION_CONTEXT ( 3 ) GLOBAL_UNCERTAINTY_ASSIGNED_CONTEXT ( ( #6718 ) ) GLOBAL_UNIT_ASSIGNED_CONTEXT ( ( #26995, #11188, #43599 ) ) REPRESENTATION_CONTEXT ( 'NONE', 'WORKASPACE' ) );
#26916 = CARTESIAN_POINT ( 'NONE',  ( 7.632228543268608334, 138.4570736234661581, -2.479861379858951942 ) ) ;
#26917 = CIRCLE ( 'NONE', #6765, 0.5000000000000004441 ) ;
#26918 = FACE_OUTER_BOUND ( 'NONE', #59450, .T. ) ;
#26919 = ORIENTED_EDGE ( 'NONE', *, *, #44390, .F. ) ;
#26920 = ORIENTED_EDGE ( 'NONE', *, *, #13085, .T. ) ;
#26921 = CARTESIAN_POINT ( 'NONE',  ( 45.00000000000000000, 9.639620389971918613, -6.999999999999999112 ) ) ;
#26922 = CARTESIAN_POINT ( 'NONE',  ( -195.0000000000000000, 0.000000000000000000, 0.000000000000000000 ) ) ;
#26923 = CARTESIAN_POINT ( 'NONE',  ( 6.123233995736766282E-16, -2.500000000000000000, -5.000000000000000000 ) ) ;
#26924 = ORIENTED_EDGE ( 'NONE', *, *, #47656, .T. ) ;
#26925 = CARTESIAN_POINT ( 'NONE',  ( 8.102448949553181734, 133.5049999999999670, 5.886773742842750679 ) ) ;
#26926 = CYLINDRICAL_SURFACE ( 'NONE', #33322, 13.00000000000000533 ) ;
#26927 = DIRECTION ( 'NONE',  ( 0.9486832980505138790, 0.3162277660168378857, -0.000000000000000000 ) ) ;
#26928 = SURFACE_STYLE_USAGE ( .BOTH. , #36168 ) ;
#26929 = CARTESIAN_POINT ( 'NONE',  ( -97.04499999999998749, 7.632228543268600340, 2.479861379858949277 ) ) ;
#26930 = VERTEX_POINT ( 'NONE', #37534 ) ;
#26931 = COLOUR_RGB ( '', 0.09019608, 0.27058824, 0.51372549) ;
#26932 = EDGE_CURVE ( 'NONE', #7058, #23699, #20607, .T. ) ;
#26933 = CARTESIAN_POINT ( 'NONE',  ( 7.896365267660146792, 153.2229155959258549, 2.416370546020021770 ) ) ;
#26934 = DIRECTION ( 'NONE',  ( 0.000000000000000000, 0.000000000000000000, -1.000000000000000000 ) ) ;
#26935 = ORIENTED_EDGE ( 'NONE', *, *, #53607, .T. ) ;
#26936 = CARTESIAN_POINT ( 'NONE',  ( -4.716976649647098618, 154.1429263765338078, 6.492361379858953008 ) ) ;
#26937 = SURFACE_SIDE_STYLE ('',( #36549 ) ) ;
#26938 = CIRCLE ( 'NONE', #5616, 9.000000000000000000 ) ;
#26939 = FACE_OUTER_BOUND ( 'NONE', #62920, .T. ) ;
#26940 = CARTESIAN_POINT ( 'NONE',  ( 20.57648123223228254, 114.4999999999999574, -10.27659574468085069 ) ) ;
#26941 = ORIENTED_EDGE ( 'NONE', *, *, #22347, .F. ) ;
#26942 = CARTESIAN_POINT ( 'NONE',  ( -74.99999999999998579, 50.00000000000000000, 6.500000000000000000 ) ) ;
#26943 = DIRECTION ( 'NONE',  ( 0.000000000000000000, 0.000000000000000000, 1.000000000000000000 ) ) ;
#26944 = FACE_OUTER_BOUND ( 'NONE', #35970, .T. ) ;
#26945 = CARTESIAN_POINT ( 'NONE',  ( 57.00000000000000000, 16.00000000000000000, 60.00402776293825724 ) ) ;
#26946 =( BOUNDED_CURVE ( )  B_SPLINE_CURVE ( 2, ( #6945, #55482, #6576, #5896, #22093, #28021, #55117, #17194, #12555, #23144, #34023 ),
 .UNSPECIFIED., .F., .F. ) 
 B_SPLINE_CURVE_WITH_KNOTS ( ( 3, 2, 2, 2, 2, 3 ),
 ( 0.05434782608695527817, 0.05652173913043349179, 0.05869565217391169848, 0.06086956521738991210, 0.06304347826086811879, 0.06521739130434632548 ),
 .UNSPECIFIED. ) 
 CURVE ( )  GEOMETRIC_REPRESENTATION_ITEM ( )  RATIONAL_B_SPLINE_CURVE ( ( 1.000000000000027978, 0.9510565162951255536, 1.000000000000000000, 0.9510565162951535312, 1.000000000000000000, 0.9510565162951535312, 1.000000000000000000, 0.9510565162951535312, 1.000000000000000000, 0.9510565162951872820, 0.9999999999999662492 ) ) 
 REPRESENTATION_ITEM ( '' )  );
#26947 = CARTESIAN_POINT ( 'NONE',  ( 3.000000000000000000, 5.000000000000000000, -72.00402776293822171 ) ) ;
#26948 = PRESENTATION_LAYER_ASSIGNMENT (  '', '', ( #16925 ) ) ;
#26949 = CARTESIAN_POINT ( 'NONE',  ( -74.99999999999998579, 50.00000000000000000, -7.500000000000000000 ) ) ;
#26950 = DIRECTION ( 'NONE',  ( -0.000000000000000000, -0.000000000000000000, 1.000000000000000000 ) ) ;
#26951 = FACE_OUTER_BOUND ( 'NONE', #17568, .T. ) ;
#26952 = DIRECTION ( 'NONE',  ( 0.000000000000000000, 0.000000000000000000, 1.000000000000000000 ) ) ;
#26953 = EDGE_LOOP ( 'NONE', ( #20254, #5145, #41631, #21337 ) ) ;
#26954 = ORIENTED_EDGE ( 'NONE', *, *, #1440, .T. ) ;
#26955 = CARTESIAN_POINT ( 'NONE',  ( -48.80707362346616662, 10.01517768586948698, -1.839758294383808966E-15 ) ) ;
#26956 = CARTESIAN_POINT ( 'NONE',  ( -87.50000000000000000, -3.500000000000000000, 0.000000000000000000 ) ) ;
#26957 = CARTESIAN_POINT ( 'NONE',  ( 60.00000000000000000, 1.797044900979284448E-15, -6.500000000000000000 ) ) ;
#26958 = EDGE_CURVE ( 'NONE', #20549, #60894, #53986, .T. ) ;
#26959 = CYLINDRICAL_SURFACE ( 'NONE', #39962, 0.5000000000000004441 ) ;
#26960 = EDGE_LOOP ( 'NONE', ( #5831, #68376, #58050, #46567 ) ) ;
#26961 = DIRECTION ( 'NONE',  ( 1.000000000000000000, 0.000000000000000000, 0.000000000000000000 ) ) ;
#26962 = CARTESIAN_POINT ( 'NONE',  ( -173.3049999999999500, 8.437984349512085203, -1.550032578732815448E-15 ) ) ;
#26963 = EDGE_CURVE ( 'NONE', #27344, #50401, #19525, .T. ) ;
#26964 = DIRECTION ( 'NONE',  ( -1.000000000000000000, 0.000000000000000000, 0.000000000000000000 ) ) ;
#26965 = CARTESIAN_POINT ( 'NONE',  ( 0.000000000000000000, -2.500000000000000000, 0.000000000000000000 ) ) ;
#26966 = VECTOR ( 'NONE', #9137, 1000.000000000000000 ) ;
#26967 = CARTESIAN_POINT ( 'NONE',  ( -176.5450000000000159, -7.632228543268600340, -2.479861379858950166 ) ) ;
#26968 = COLOUR_RGB ( '', 0.72549020, 0.75294118, 0.79215686) ;
#26969 = CARTESIAN_POINT ( 'NONE',  ( -163.3449999999999989, 7.632228543268599452, -2.479861379858951942 ) ) ;
#26970 = PRESENTATION_LAYER_ASSIGNMENT (  '', '', ( #47290 ) ) ;
#26971 = ORIENTED_EDGE ( 'NONE', *, *, #46976, .F. ) ;
#26972 = CARTESIAN_POINT ( 'NONE',  ( -89.09292637653379643, 3.094860106618433360, 9.524999999999991473 ) ) ;
#26973 = ADVANCED_FACE ( 'NONE', ( #26558 ), #15693, .T. ) ;
#26974 = SURFACE_SIDE_STYLE ('',( #37962 ) ) ;
#26975 = VECTOR ( 'NONE', #47410, 1000.000000000000000 ) ;
#26976 = CARTESIAN_POINT ( 'NONE',  ( -10.16381930648914711, 11.93252338341607910, -1.311443076476738856 ) ) ;
#26977 = CARTESIAN_POINT ( 'NONE',  ( -80.15499999999998693, 7.632228543268600340, 2.479861379858949277 ) ) ;
#26978 = DIRECTION ( 'NONE',  ( 0.000000000000000000, 0.000000000000000000, 1.000000000000000000 ) ) ;
#26979 = LINE ( 'NONE', #27333, #10168 ) ;
#26980 = MECHANICAL_DESIGN_GEOMETRIC_PRESENTATION_REPRESENTATION (  '', ( #30349 ), #47343 ) ;
#26981 = CARTESIAN_POINT ( 'NONE',  ( -77.69499999999999318, -8.437984349512086979, 5.166775262442717831E-16 ) ) ;
#26982 = CARTESIAN_POINT ( 'NONE',  ( -5.598654528085808657, 141.7549999999999955, 7.705886871421373741 ) ) ;
#26983 = FACE_OUTER_BOUND ( 'NONE', #18583, .T. ) ;
#26984 = EDGE_CURVE ( 'NONE', #47261, #8699, #40336, .T. ) ;
#26985 = CARTESIAN_POINT ( 'NONE',  ( 179.4361977533518484, 5.000000000000000000, 103.7004518695275550 ) ) ;
#26986 = CARTESIAN_POINT ( 'NONE',  ( 74.50000000000000000, 20.36037961002804053, -6.000000000000000000 ) ) ;
#26987 = UNCERTAINTY_MEASURE_WITH_UNIT (LENGTH_MEASURE( 1.000000000000000082E-05 ), #22106, 'distance_accuracy_value', 'NONE');
#26988 =( GEOMETRIC_REPRESENTATION_CONTEXT ( 3 ) GLOBAL_UNCERTAINTY_ASSIGNED_CONTEXT ( ( #53094 ) ) GLOBAL_UNIT_ASSIGNED_CONTEXT ( ( #61105, #34027, #65691 ) ) REPRESENTATION_CONTEXT ( 'NONE', 'WORKASPACE' ) );
#26990 = SURFACE_SIDE_STYLE ('',( #37634 ) ) ;
#26989 = STYLED_ITEM ( 'NONE', ( #66478 ), #5971 ) ;
#26991 = CARTESIAN_POINT ( 'NONE',  ( 0.000000000000000000, 0.000000000000000000, -12.50000000000000000 ) ) ;
#26992 = ORIENTED_EDGE ( 'NONE', *, *, #55340, .T. ) ;
#26993 = ADVANCED_FACE ( 'NONE', ( #20960 ), #29730, .T. ) ;
#26994 = CARTESIAN_POINT ( 'NONE',  ( -7.632228543268607446, 132.5429263765338135, -2.479861379858953718 ) ) ;
#26995 =( LENGTH_UNIT ( ) NAMED_UNIT ( * ) SI_UNIT ( .MILLI., .METRE. ) );
#26996 =( LENGTH_UNIT ( ) NAMED_UNIT ( * ) SI_UNIT ( .MILLI., .METRE. ) );
#26998 = SURFACE_SIDE_STYLE ('',( #37290 ) ) ;
#26997 = DIRECTION ( 'NONE',  ( -0.000000000000000000, -0.000000000000000000, 1.000000000000000000 ) ) ;
#26999 = DIRECTION ( 'NONE',  ( 0.000000000000000000, 1.000000000000000000, -0.000000000000000000 ) ) ;
#27000 = ORIENTED_EDGE ( 'NONE', *, *, #3124, .T. ) ;
#27001 = ORIENTED_EDGE ( 'NONE', *, *, #28972, .T. ) ;
#27002 = CARTESIAN_POINT ( 'NONE',  ( 0.000000000000000000, 13.00000000000000178, -36.49999999999999289 ) ) ;
#27003 = MECHANICAL_DESIGN_GEOMETRIC_PRESENTATION_REPRESENTATION (  '', ( #34920 ), #56253 ) ;
#27004 = VECTOR ( 'NONE', #17609, 1000.000000000000000 ) ;
#27005 = DIRECTION ( 'NONE',  ( 1.000000000000000000, 0.000000000000000000, 0.000000000000000000 ) ) ;
#27006 = CARTESIAN_POINT ( 'NONE',  ( 6.826472737025121695, 140.4929263765338021, -4.959722759717905660 ) ) ;
#27007 = EDGE_LOOP ( 'NONE', ( #55872, #22114, #4804, #7319, #5503, #37726, #66880 ) ) ;
#27008 = CARTESIAN_POINT ( 'NONE',  ( -112.7049999999999699, 2.607480562269072433, 8.024999999999991473 ) ) ;
#27009 = VERTEX_POINT ( 'NONE', #42454 ) ;
#27010 = DIRECTION ( 'NONE',  ( 0.000000000000000000, 1.000000000000000000, 0.000000000000000000 ) ) ;
#27011 = CARTESIAN_POINT ( 'NONE',  ( -195.0000000000000000, 0.000000000000000000, 0.000000000000000000 ) ) ;
#27012 = ORIENTED_EDGE ( 'NONE', *, *, #42275, .F. ) ;
#27013 = DIRECTION ( 'NONE',  ( 0.000000000000000000, 0.000000000000000000, -1.000000000000000000 ) ) ;
#27014 = DIRECTION ( 'NONE',  ( 0.000000000000000000, 0.000000000000000000, 1.000000000000000000 ) ) ;
#27015 = ORIENTED_EDGE ( 'NONE', *, *, #40790, .T. ) ;
#27016 = COLOUR_RGB ( '', 0.31764706, 0.68627451, 0.89019608) ;
#27017 = SURFACE_STYLE_USAGE ( .BOTH. , #42579 ) ;
#27018 =( GEOMETRIC_REPRESENTATION_CONTEXT ( 3 ) GLOBAL_UNCERTAINTY_ASSIGNED_CONTEXT ( ( #67203 ) ) GLOBAL_UNIT_ASSIGNED_CONTEXT ( ( #25480, #31098, #63476 ) ) REPRESENTATION_CONTEXT ( 'NONE', 'WORKASPACE' ) );
#27019 = CARTESIAN_POINT ( 'NONE',  ( 8.102448949553183510, 159.9950000000000330, -5.886773742842746238 ) ) ;
#27020 = DIRECTION ( 'NONE',  ( 0.000000000000000000, 0.000000000000000000, -1.000000000000000000 ) ) ;
#27021 = EDGE_CURVE ( 'NONE', #41519, #49984, #53295, .T. ) ;
#27022 = CIRCLE ( 'NONE', #54011, 5.000000000000004441 ) ;
#27023 = ORIENTED_EDGE ( 'NONE', *, *, #6351, .F. ) ;
#27024 = PRESENTATION_STYLE_ASSIGNMENT (( #5577 ) ) ;
#27025 = CARTESIAN_POINT ( 'NONE',  ( -136.5570736234661808, -1.166476076187852838E-15, -9.524999999999991473 ) ) ;
#27026 = CARTESIAN_POINT ( 'NONE',  ( -181.4929263765337737, -8.102448949553174629, 5.886773742842742685 ) ) ;
#27027 = ORIENTED_EDGE ( 'NONE', *, *, #26089, .F. ) ;
#27028 = CARTESIAN_POINT ( 'NONE',  ( -9.827790563157511022E-16, 124.4429263765338192, 8.025000000000000355 ) ) ;
#27029 = CARTESIAN_POINT ( 'NONE',  ( 57.74999999999998579, 30.74999999999999289, 3.750000000000000000 ) ) ;
#27030 = CARTESIAN_POINT ( 'NONE',  ( -48.05707362346617373, 0.000000000000000000, 9.524999999999991473 ) ) ;
#27031 = PRESENTATION_LAYER_ASSIGNMENT (  '', '', ( #57397 ) ) ;
#27032 = CARTESIAN_POINT ( 'NONE',  ( 3.542013698345610972, -9.000000000000003553, 0.6642442188400904390 ) ) ;
#27033 = CARTESIAN_POINT ( 'NONE',  ( -43.75000000000000000, 0.000000000000000000, -2.000000000000000000 ) ) ;
#27034 = ORIENTED_EDGE ( 'NONE', *, *, #12332, .F. ) ;
#27035 = CARTESIAN_POINT ( 'NONE',  ( 4.041451884327379673, -7.000000000000002665, 1.082903768654758903 ) ) ;
#27036 = ORIENTED_EDGE ( 'NONE', *, *, #49727, .F. ) ;
#27037 = CARTESIAN_POINT ( 'NONE',  ( -52.94292637653380496, 0.000000000000000000, 9.524999999999991473 ) ) ;
#27038 = FACE_OUTER_BOUND ( 'NONE', #1685, .T. ) ;
#27039 = DIRECTION ( 'NONE',  ( -1.000000000000000000, 0.000000000000000000, -0.000000000000000000 ) ) ;
#27040 = CARTESIAN_POINT ( 'NONE',  ( -144.6549999999999727, -7.632228543268600340, -2.479861379858950166 ) ) ;
#27041 = CARTESIAN_POINT ( 'NONE',  ( -175.5570736234661808, -1.166476076187852838E-15, -9.524999999999991473 ) ) ;
#27042 = UNCERTAINTY_MEASURE_WITH_UNIT (LENGTH_MEASURE( 1.000000000000000082E-05 ), #23627, 'distance_accuracy_value', 'NONE');
#27043 = AXIS2_PLACEMENT_3D ( 'NONE', #11451, #12479, #44209 ) ;
#27044 = EDGE_CURVE ( 'NONE', #3787, #68105, #40757, .T. ) ;
#27045 = CARTESIAN_POINT ( 'NONE',  ( -4.716976649647097730, 115.3570736234661638, -6.492361379858953896 ) ) ;
#27046 = CARTESIAN_POINT ( 'NONE',  ( 41.12443333818617930, 107.5641524110674112, 3.336502945398295950 ) ) ;
#27047 = EDGE_LOOP ( 'NONE', ( #46452, #49485, #58406, #22763, #33432, #43622, #38900 ) ) ;
#27048 = EDGE_LOOP ( 'NONE', ( #47345, #20788, #19118, #40151 ) ) ;
#27049 = DIRECTION ( 'NONE',  ( -1.000000000000000000, -0.000000000000000000, -0.000000000000000000 ) ) ;
#27050 = CARTESIAN_POINT ( 'NONE',  ( 1.000000000000000888, 13.00000000000000178, -60.00402776293827145 ) ) ;
#27051 = EDGE_CURVE ( 'NONE', #1324, #56729, #17362, .T. ) ;
#27052 = CARTESIAN_POINT ( 'NONE',  ( -56.30499999999999972, 8.437984349512085203, -1.550032578732815448E-15 ) ) ;
#27053 = EDGE_LOOP ( 'NONE', ( #43484, #59844, #62861, #64401 ) ) ;
#27054 = DIRECTION ( 'NONE',  ( 0.000000000000000000, 0.000000000000000000, 1.000000000000000000 ) ) ;
#27055 = CARTESIAN_POINT ( 'NONE',  ( 48.74999999999999289, 24.99999999999998579, 4.000000000000000000 ) ) ;
#27056 = ADVANCED_FACE ( 'NONE', ( #50127 ), #22688, .F. ) ;
#27057 = DIRECTION ( 'NONE',  ( -0.000000000000000000, 1.000000000000000000, -0.000000000000000000 ) ) ;
#27058 = DIRECTION ( 'NONE',  ( 0.000000000000000000, 0.000000000000000000, 1.000000000000000000 ) ) ;
#27059 = VECTOR ( 'NONE', #22439, 1000.000000000000114 ) ;
#27060 =( NAMED_UNIT ( * ) PLANE_ANGLE_UNIT ( ) SI_UNIT ( $, .RADIAN. ) );
#27061 = CARTESIAN_POINT ( 'NONE',  ( -128.2429263765338021, 5.598654528085804216, 7.705886871421366635 ) ) ;
#27062 = ORIENTED_EDGE ( 'NONE', *, *, #66709, .F. ) ;
#27063 =( BOUNDED_CURVE ( )  B_SPLINE_CURVE ( 2, ( #36057, #57137, #62429, #10015, #14958, #41699, #57499, #36782, #63121, #57863, #19856 ),
 .UNSPECIFIED., .F., .F. ) 
 B_SPLINE_CURVE_WITH_KNOTS ( ( 3, 2, 2, 2, 2, 3 ),
 ( 0.5869565217391164991, 0.5891304347825947474, 0.5913043478260728847, 0.5934782608695511330, 0.5956521739130292703, 0.5978260869565075186 ),
 .UNSPECIFIED. ) 
 CURVE ( )  GEOMETRIC_REPRESENTATION_ITEM ( )  RATIONAL_B_SPLINE_CURVE ( ( 1.000000000000314859, 0.9510565162948385609, 1.000000000000000000, 0.9510565162951535312, 1.000000000000000000, 0.9510565162951535312, 1.000000000000000000, 0.9510565162951535312, 1.000000000000000000, 0.9510565162954734975, 0.9999999999996800337 ) ) 
 REPRESENTATION_ITEM ( '' )  );
#27064 = AXIS2_PLACEMENT_3D ( 'NONE', #43542, #42167, #59290 ) ;
#27065 = EDGE_CURVE ( 'NONE', #68529, #57180, #7239, .T. ) ;
#27066 = AXIS2_PLACEMENT_3D ( 'NONE', #47394, #26566, #20617 ) ;
#27067 = LINE ( 'NONE', #15202, #54840 ) ;
#27068 = DIRECTION ( 'NONE',  ( 0.000000000000000000, 0.000000000000000000, 1.000000000000000000 ) ) ;
#27069 = DIRECTION ( 'NONE',  ( -0.000000000000000000, 1.000000000000000000, 0.000000000000000000 ) ) ;
#27070 =( NAMED_UNIT ( * ) PLANE_ANGLE_UNIT ( ) SI_UNIT ( $, .RADIAN. ) );
#27071 = ADVANCED_FACE ( 'NONE', ( #66639 ), #9521, .T. ) ;
#27072 = CARTESIAN_POINT ( 'NONE',  ( -112.4949999999999761, 6.826472737025113702, -4.959722759717902107 ) ) ;
#27073 = CARTESIAN_POINT ( 'NONE',  ( -1.166476076187854022E-15, 112.0549999999999926, 9.525000000000000355 ) ) ;
#27074 = CARTESIAN_POINT ( 'NONE',  ( -88.94499999999997897, -9.827790563157499189E-16, -8.024999999999991473 ) ) ;
#27075 = AXIS2_PLACEMENT_3D ( 'NONE', #67891, #61527, #3822 ) ;
#27076 = CARTESIAN_POINT ( 'NONE',  ( 71.49999999999998579, 64.07124727947029896, 7.000000000000000000 ) ) ;
#27077 = AXIS2_PLACEMENT_3D ( 'NONE', #45253, #13900, #40300 ) ;
#27078 = DIRECTION ( 'NONE',  ( -6.938893903907222067E-15, 1.000000000000000000, 0.000000000000000000 ) ) ;
#27079 = UNCERTAINTY_MEASURE_WITH_UNIT (LENGTH_MEASURE( 1.000000000000000082E-05 ), #36697, 'distance_accuracy_value', 'NONE');
#27080 = VECTOR ( 'NONE', #13178, 1000.000000000000000 ) ;
#27081 = ORIENTED_EDGE ( 'NONE', *, *, #25095, .T. ) ;
#27082 = CARTESIAN_POINT ( 'NONE',  ( -124.4929263765337879, -8.102448949553172852, 5.886773742842742685 ) ) ;
#27083 = FILL_AREA_STYLE_COLOUR ( '', #40516 ) ;
#27084 = CARTESIAN_POINT ( 'NONE',  ( -150.5949999999999989, 2.607480562269073321, 8.024999999999991473 ) ) ;
#27086 =( NAMED_UNIT ( * ) PLANE_ANGLE_UNIT ( ) SI_UNIT ( $, .RADIAN. ) );
#27085 = AXIS2_PLACEMENT_3D ( 'NONE', #12831, #65610, #23733 ) ;
#27087 = AXIS2_PLACEMENT_3D ( 'NONE', #52694, #15424, #14008 ) ;
#27088 = FACE_OUTER_BOUND ( 'NONE', #25385, .T. ) ;
#27089 = CARTESIAN_POINT ( 'NONE',  ( 36.00000000000002842, 5.000000000000000000, 77.00402776293825013 ) ) ;
#27090 = EDGE_LOOP ( 'NONE', ( #10684, #65405, #36384 ) ) ;
#27091 = ORIENTED_EDGE ( 'NONE', *, *, #20909, .T. ) ;
#27092 = EDGE_CURVE ( 'NONE', #23198, #25944, #13150, .T. ) ;
#27093 =( GEOMETRIC_REPRESENTATION_CONTEXT ( 3 ) GLOBAL_UNCERTAINTY_ASSIGNED_CONTEXT ( ( #68577 ) ) GLOBAL_UNIT_ASSIGNED_CONTEXT ( ( #15638, #26501, #5379 ) ) REPRESENTATION_CONTEXT ( 'NONE', 'WORKASPACE' ) );
#27094 = DIRECTION ( 'NONE',  ( 0.000000000000000000, 1.000000000000000000, 0.000000000000000000 ) ) ;
#27095 = CARTESIAN_POINT ( 'NONE',  ( -74.99999999999998579, 50.00000000000000000, -6.999999999999988454 ) ) ;
#27096 =( NAMED_UNIT ( * ) PLANE_ANGLE_UNIT ( ) SI_UNIT ( $, .RADIAN. ) );
#27097 = CARTESIAN_POINT ( 'NONE',  ( -45.00000000000000000, 8.537325437491110947, 6.129378421684276823 ) ) ;
#27098 = CARTESIAN_POINT ( 'NONE',  ( -129.9570736234661865, 9.058813317711329915, -2.943386871421373119 ) ) ;
#27099 = ORIENTED_EDGE ( 'NONE', *, *, #51697, .T. ) ;
#27100 = CARTESIAN_POINT ( 'NONE',  ( -152.6049999999999898, 6.826472737025113702, -4.959722759717902107 ) ) ;
#27101 = ORIENTED_EDGE ( 'NONE', *, *, #52902, .F. ) ;
#27102 = CARTESIAN_POINT ( 'NONE',  ( 5.185928986913072691, 5.017707510222363609, 0.2088670156639309550 ) ) ;
#27103 = CARTESIAN_POINT ( 'NONE',  ( -141.0570736234661808, 0.000000000000000000, 9.524999999999991473 ) ) ;
#27104 = ORIENTED_EDGE ( 'NONE', *, *, #31768, .T. ) ;
#27105 = LINE ( 'NONE', #38076, #46162 ) ;
#27106 =( NAMED_UNIT ( * ) PLANE_ANGLE_UNIT ( ) SI_UNIT ( $, .RADIAN. ) );
#27107 = CARTESIAN_POINT ( 'NONE',  ( 3.094860106618435136, 121.2949999999999733, -9.525000000000000355 ) ) ;
#27108 = ORIENTED_EDGE ( 'NONE', *, *, #66472, .T. ) ;
#27109 = PRESENTATION_LAYER_ASSIGNMENT (  '', '', ( #30475 ) ) ;
#27110 = CARTESIAN_POINT ( 'NONE',  ( -95.45707362346617231, -9.058813317711329915, 2.943386871421371787 ) ) ;
#27111 = CARTESIAN_POINT ( 'NONE',  ( -9.058813317711338797, 129.4549999999999841, 2.943386871421373563 ) ) ;
#27112 = AXIS2_PLACEMENT_3D ( 'NONE', #4775, #47766, #57557 ) ;
#27113 = CARTESIAN_POINT ( 'NONE',  ( -60.95499999999998408, -7.632228543268599452, 2.479861379858951054 ) ) ;
#27114 = CARTESIAN_POINT ( 'NONE',  ( -122.2449999999999903, -4.716976649647093289, -6.492361379858945902 ) ) ;
#27115 = CARTESIAN_POINT ( 'NONE',  ( -41.49999999999998579, 106.9282032302754999, -3.500000000000000888 ) ) ;
#27116 = PRODUCT_DEFINITION_SHAPE ( 'NONE', 'NONE',  #64860 ) ;
#27117 = ORIENTED_EDGE ( 'NONE', *, *, #58444, .F. ) ;
#27118 = CARTESIAN_POINT ( 'NONE',  ( 3.094860106618431583, 145.2049999999999272, 9.525000000000000355 ) ) ;
#27119 = FILL_AREA_STYLE_COLOUR ( '', #31089 ) ;
#27120 = UNCERTAINTY_MEASURE_WITH_UNIT (LENGTH_MEASURE( 1.000000000000000082E-05 ), #2942, 'distance_accuracy_value', 'NONE');
#27121 =( LENGTH_UNIT ( ) NAMED_UNIT ( * ) SI_UNIT ( .MILLI., .METRE. ) );
#27122 = DIRECTION ( 'NONE',  ( 1.000000000000000000, 0.000000000000000000, 0.000000000000000000 ) ) ;
#27123 = SURFACE_SIDE_STYLE ('',( #10297 ) ) ;
#27124 = EDGE_CURVE ( 'NONE', #39296, #34249, #22961, .T. ) ;
#27125 = DIRECTION ( 'NONE',  ( 1.156482317317870344E-15, 1.000000000000000000, 0.000000000000000000 ) ) ;
#27126 = ORIENTED_EDGE ( 'NONE', *, *, #5792, .F. ) ;
#27127 = SURFACE_SIDE_STYLE ('',( #54576 ) ) ;
#27128 = FACE_OUTER_BOUND ( 'NONE', #60886, .T. ) ;
#27129 = CARTESIAN_POINT ( 'NONE',  ( -174.6550000000000011, -7.632228543268600340, -2.479861379858950166 ) ) ;
#27131 = ORIENTED_EDGE ( 'NONE', *, *, #1699, .T. ) ;
#27130 =( GEOMETRIC_REPRESENTATION_CONTEXT ( 3 ) GLOBAL_UNCERTAINTY_ASSIGNED_CONTEXT ( ( #21522 ) ) GLOBAL_UNIT_ASSIGNED_CONTEXT ( ( #33376, #53456, #27377 ) ) REPRESENTATION_CONTEXT ( 'NONE', 'WORKASPACE' ) );
#27132 = FILL_AREA_STYLE_COLOUR ( '', #67656 ) ;
#27133 = UNCERTAINTY_MEASURE_WITH_UNIT (LENGTH_MEASURE( 1.000000000000000082E-05 ), #69280, 'distance_accuracy_value', 'NONE');
#27134 = COLOUR_RGB ( '', 0.66274510, 0.83137255, 0.94901961) ;
#27135 = EDGE_CURVE ( 'NONE', #26930, #22912, #1856, .T. ) ;
#27136 = CYLINDRICAL_SURFACE ( 'NONE', #36381, 16.00000000000000000 ) ;
#27137 = DIRECTION ( 'NONE',  ( 1.000000000000000000, 0.000000000000000000, 0.000000000000000000 ) ) ;
#27138 = COLOUR_RGB ( '', 0.09019608, 0.27058824, 0.51372549) ;
#27139 = ORIENTED_EDGE ( 'NONE', *, *, #17608, .F. ) ;
#27140 = CARTESIAN_POINT ( 'NONE',  ( -45.91046102236034443, 9.422706725342738565, -3.407293203743047005 ) ) ;
#27142 = EDGE_CURVE ( 'NONE', #24348, #35681, #31935, .T. ) ;
#27141 = DIRECTION ( 'NONE',  ( -1.000000000000000000, 0.000000000000000000, 0.000000000000000000 ) ) ;
#27143 = CONICAL_SURFACE ( 'NONE', #54112, 6.999999999999997335, 0.7853981633974500554 ) ;
#27144 = CARTESIAN_POINT ( 'NONE',  ( -81.95499999999998408, -7.632228543268599452, 2.479861379858951054 ) ) ;
#27145 = ORIENTED_EDGE ( 'NONE', *, *, #58223, .T. ) ;
#27146 = FACE_OUTER_BOUND ( 'NONE', #4208, .T. ) ;
#27147 = SURFACE_SIDE_STYLE ('',( #53565 ) ) ;
#27148 = CARTESIAN_POINT ( 'NONE',  ( 98.00000000000000000, 16.00000000000000000, 12.50000000000000178 ) ) ;
#27149 = CARTESIAN_POINT ( 'NONE',  ( -65.75707362346616947, -5.598654528085801552, 7.705886871421367523 ) ) ;
#27150 = DIRECTION ( 'NONE',  ( 1.000000000000000000, 0.000000000000000000, 0.000000000000000000 ) ) ;
#27151 = EDGE_LOOP ( 'NONE', ( #3962, #15145, #24513, #66202 ) ) ;
#27152 = PRESENTATION_STYLE_ASSIGNMENT (( #53242 ) ) ;
#27153 = FILL_AREA_STYLE_COLOUR ( '', #5496 ) ;
#27154 = AXIS2_PLACEMENT_3D ( 'NONE', #68783, #10389, #31111 ) ;
#27155 = EDGE_CURVE ( 'NONE', #10026, #4254, #11781, .T. ) ;
#27156 = CARTESIAN_POINT ( 'NONE',  ( -102.6549999999999869, -7.632228543268600340, -2.479861379858950166 ) ) ;
#27157 = CARTESIAN_POINT ( 'NONE',  ( 5.598654528085809545, 133.1449999999999818, -7.705886871421373741 ) ) ;
#27158 = CARTESIAN_POINT ( 'NONE',  ( -115.3449999999999847, 7.632228543268599452, -2.479861379858951942 ) ) ;
#27159 = CIRCLE ( 'NONE', #44056, 0.5000000000000004441 ) ;
#27160 = CARTESIAN_POINT ( 'NONE',  ( 0.000000000000000000, 87.30187232391182306, 0.000000000000000000 ) ) ;
#27161 = CARTESIAN_POINT ( 'NONE',  ( -162.8929263765338078, -8.102448949553172852, -5.886773742842741797 ) ) ;
#27162 = FILL_AREA_STYLE ('',( #15300 ) ) ;
#27163 = CARTESIAN_POINT ( 'NONE',  ( -179.9950000000000045, -6.826472737025115478, 4.959722759717900331 ) ) ;
#27164 = AXIS2_PLACEMENT_3D ( 'NONE', #17886, #56187, #3739 ) ;
#27165 = CARTESIAN_POINT ( 'NONE',  ( 72.50000000000000000, 35.92875272052971525, -9.500000000000000000 ) ) ;
#27166 = DIRECTION ( 'NONE',  ( 1.000000000000000000, 0.000000000000000000, 0.000000000000000000 ) ) ;
#27167 = ORIENTED_EDGE ( 'NONE', *, *, #40616, .T. ) ;
#27168 = LINE ( 'NONE', #53921, #16755 ) ;
#27169 = DIRECTION ( 'NONE',  ( 0.000000000000000000, 0.000000000000000000, 1.000000000000000000 ) ) ;
#27170 = ORIENTED_EDGE ( 'NONE', *, *, #3127, .F. ) ;
#27171 = STYLED_ITEM ( 'NONE', ( #27889 ), #35666 ) ;
#27172 = CARTESIAN_POINT ( 'NONE',  ( -72.74292637653380211, -5.598654528085803328, -7.705886871421366635 ) ) ;
#27173 = ADVANCED_FACE ( 'NONE', ( #33578 ), #33243, .T. ) ;
#27174 = DIRECTION ( 'NONE',  ( -0.000000000000000000, -0.000000000000000000, -1.000000000000000000 ) ) ;
#27175 = FILL_AREA_STYLE_COLOUR ( '', #14625 ) ;
#27176 = SPHERICAL_SURFACE ( 'NONE', #32619, 0.2500000000000000000 ) ;
#27177 = FILL_AREA_STYLE ('',( #54277 ) ) ;
#27178 = CARTESIAN_POINT ( 'NONE',  ( -6.020204320972967871, -7.572700244129130454, 0.6386920474458009922 ) ) ;
#27179 = ORIENTED_EDGE ( 'NONE', *, *, #19415, .T. ) ;
#27180 = CARTESIAN_POINT ( 'NONE',  ( -180.5049999999999670, -6.826472737025113702, -4.959722759717900331 ) ) ;
#27181 = ORIENTED_EDGE ( 'NONE', *, *, #54064, .F. ) ;
#27182 = AXIS2_PLACEMENT_3D ( 'NONE', #68624, #41561, #36656 ) ;
#27183 = CARTESIAN_POINT ( 'NONE',  ( -17.41962728626436530, -0.1139526552317604857, 2.000000000000000000 ) ) ;
#27184 =( NAMED_UNIT ( * ) SI_UNIT ( $, .STERADIAN. ) SOLID_ANGLE_UNIT ( ) );
#27185 = DIRECTION ( 'NONE',  ( -0.000000000000000000, 0.000000000000000000, -1.000000000000000000 ) ) ;
#27186 = CARTESIAN_POINT ( 'NONE',  ( 6.826472737025121695, 144.6070736234661638, -4.959722759717905660 ) ) ;
#27187 = EDGE_LOOP ( 'NONE', ( #24815, #45015, #3754 ) ) ;
#27188 = FACE_OUTER_BOUND ( 'NONE', #1417, .T. ) ;
#27189 = CARTESIAN_POINT ( 'NONE',  ( -92.30499999999997840, 8.437984349512086979, -1.550032578732815448E-15 ) ) ;
#27190 = UNCERTAINTY_MEASURE_WITH_UNIT (LENGTH_MEASURE( 1.000000000000000082E-05 ), #43620, 'distance_accuracy_value', 'NONE');
#27191 = CIRCLE ( 'NONE', #1302, 0.5000000000000004441 ) ;
#27192 = DIRECTION ( 'NONE',  ( 9.811390859391774840E-17, -1.000000000000000000, 0.000000000000000000 ) ) ;
#27193 = ORIENTED_EDGE ( 'NONE', *, *, #17603, .T. ) ;
#27194 = CYLINDRICAL_SURFACE ( 'NONE', #52361, 0.5000000000000004441 ) ;
#27195 = CARTESIAN_POINT ( 'NONE',  ( 8.750000000000001776, 25.24999999999998934, -3.750000000000000000 ) ) ;
#27196 = FACE_OUTER_BOUND ( 'NONE', #67924, .T. ) ;
#27197 = ADVANCED_FACE ( 'NONE', ( #17768 ), #47727, .T. ) ;
#27198 = MANIFOLD_SOLID_BREP ( 'Revolve1', #11523 ) ;
#27199 = CARTESIAN_POINT ( 'NONE',  ( 4.383776131304280455, -1.496531397472844693, 9.000000000000003553 ) ) ;
#27200 = ORIENTED_EDGE ( 'NONE', *, *, #53544, .F. ) ;
#27201 = SURFACE_STYLE_USAGE ( .BOTH. , #17056 ) ;
#27202 = CARTESIAN_POINT ( 'NONE',  ( -58.79499999999998749, 2.607480562269068880, -8.024999999999993250 ) ) ;
#27203 = ORIENTED_EDGE ( 'NONE', *, *, #14385, .T. ) ;
#27204 =( LENGTH_UNIT ( ) NAMED_UNIT ( * ) SI_UNIT ( .MILLI., .METRE. ) );
#27205 = AXIS2_PLACEMENT_3D ( 'NONE', #5584, #16546, #38006 ) ;
#27206 = CARTESIAN_POINT ( 'NONE',  ( -74.99999999999998579, 50.00000000000000000, -9.500000000000001776 ) ) ;
#27207 = CARTESIAN_POINT ( 'NONE',  ( -45.00000000000000000, 8.700918745341869709, -5.871692373102996854 ) ) ;
#27208 = ORIENTED_EDGE ( 'NONE', *, *, #56521, .F. ) ;
#27209 = EDGE_LOOP ( 'NONE', ( #37985, #22473, #52827, #2359 ) ) ;
#27210 = AXIS2_PLACEMENT_3D ( 'NONE', #441, #39207, #16374 ) ;
#27211 = FILL_AREA_STYLE_COLOUR ( '', #38227 ) ;
#27212 = EDGE_CURVE ( 'NONE', #43779, #69071, #8403, .T. ) ;
#27213 = CARTESIAN_POINT ( 'NONE',  ( -113.9049999999999869, 2.607480562269068880, -8.024999999999993250 ) ) ;
#27214 = ORIENTED_EDGE ( 'NONE', *, *, #791, .F. ) ;
#27215 = DIRECTION ( 'NONE',  ( -9.376883653928687363E-17, -1.000000000000000000, -0.000000000000000000 ) ) ;
#27216 = CARTESIAN_POINT ( 'NONE',  ( 23.50000000000001776, 13.99999999999999822, 26.18999999999999417 ) ) ;
#27217 = DIRECTION ( 'NONE',  ( 1.000000000000000000, -5.782411586589351722E-16, 0.000000000000000000 ) ) ;
#27218 = FILL_AREA_STYLE_COLOUR ( '', #62556 ) ;
#27219 = CARTESIAN_POINT ( 'NONE',  ( -164.6070736234661922, -8.102448949553172852, 5.886773742842742685 ) ) ;
#27221 = EDGE_CURVE ( 'NONE', #8394, #14677, #69330, .T. ) ;
#27220 = COLOUR_RGB ( '', 0.40784314, 0.44705882, 0.49803922) ;
#27222 = CARTESIAN_POINT ( 'NONE',  ( 8.102448949553181734, 129.9950000000000045, -5.886773742842746238 ) ) ;
#27223 = CARTESIAN_POINT ( 'NONE',  ( -93.20707362346615810, 3.094860106618433360, 9.524999999999991473 ) ) ;
#27224 = CIRCLE ( 'NONE', #10444, 18.50000000000000355 ) ;
#27225 = EDGE_CURVE ( 'NONE', #28040, #17222, #27443, .T. ) ;
#27226 = DIRECTION ( 'NONE',  ( 1.000000000000000000, 0.000000000000000000, 0.000000000000000000 ) ) ;
#27227 = VERTEX_POINT ( 'NONE', #58416 ) ;
#27228 = CARTESIAN_POINT ( 'NONE',  ( -60.00000000000000000, -2.024042244987997205E-14, 12.00000000000000000 ) ) ;
#27229 = FACE_OUTER_BOUND ( 'NONE', #5505, .T. ) ;
#27231 = AXIS2_PLACEMENT_3D ( 'NONE', #1213, #11828, #27976 ) ;
#27230 =( NAMED_UNIT ( * ) PLANE_ANGLE_UNIT ( ) SI_UNIT ( $, .RADIAN. ) );
#27232 = ADVANCED_FACE ( 'NONE', ( #34605 ), #47583, .T. ) ;
#27233 = CIRCLE ( 'NONE', #3620, 0.5000000000000004441 ) ;
#27234 = CARTESIAN_POINT ( 'NONE',  ( -142.2549999999999955, -4.716976649647092401, 6.492361379858946790 ) ) ;
#27235 = DIRECTION ( 'NONE',  ( 0.000000000000000000, 0.000000000000000000, -1.000000000000000000 ) ) ;
#27236 = DIRECTION ( 'NONE',  ( 0.000000000000000000, -1.000000000000000000, 0.000000000000000000 ) ) ;
#27237 = DIRECTION ( 'NONE',  ( 0.000000000000000000, 0.000000000000000000, 1.000000000000000000 ) ) ;
#27238 = CARTESIAN_POINT ( 'NONE',  ( -143.2449999999999761, -4.716976649647093289, -6.492361379858945902 ) ) ;
#27239 = CARTESIAN_POINT ( 'NONE',  ( -137.8449999999999989, -7.632228543268599452, 2.479861379858951054 ) ) ;
#27240 = VERTEX_POINT ( 'NONE', #68991 ) ;
#27241 = CARTESIAN_POINT ( 'NONE',  ( 44.67254323996785104, 10.47540843667308508, -3.522617369932422804 ) ) ;
#27242 = AXIS2_PLACEMENT_3D ( 'NONE', #49017, #12030, #27498 ) ;
#27243 = SURFACE_STYLE_USAGE ( .BOTH. , #33587 ) ;
#27244 = CARTESIAN_POINT ( 'NONE',  ( 60.49999999999998579, 50.00000000000000000, 7.500000000000000000 ) ) ;
#27245 = CARTESIAN_POINT ( 'NONE',  ( -51.35499999999998266, -4.716976649647093289, -6.492361379858945902 ) ) ;
#27246 =( GEOMETRIC_REPRESENTATION_CONTEXT ( 3 ) GLOBAL_UNCERTAINTY_ASSIGNED_CONTEXT ( ( #54642 ) ) GLOBAL_UNIT_ASSIGNED_CONTEXT ( ( #57357, #35212, #62288 ) ) REPRESENTATION_CONTEXT ( 'NONE', 'WORKASPACE' ) );
#27247 = CARTESIAN_POINT ( 'NONE',  ( -59.54499999999998749, -7.632228543268600340, -2.479861379858950166 ) ) ;
#27248 = CARTESIAN_POINT ( 'NONE',  ( -139.3429263765337964, -9.058813317711329915, 2.943386871421371787 ) ) ;
#27249 = B_SPLINE_CURVE_WITH_KNOTS ( 'NONE', 3,
 ( #22294, #37498, #48380, #16707, #5403, #38170 ),
 .UNSPECIFIED., .F., .F.,
 ( 4, 2, 4 ),
 ( 5.235446031985231014E-16, 0.0007919337925127429125, 0.001583867585024962155 ),
 .UNSPECIFIED. ) ;
#27250 = CARTESIAN_POINT ( 'NONE',  ( -9.827790563157511022E-16, 152.5570736234661524, 8.025000000000000355 ) ) ;
#27251 = COLOUR_RGB ( '', 0.08235294, 0.09019608, 0.10196078) ;
#27252 = VECTOR ( 'NONE', #2936, 1000.000000000000000 ) ;
#27253 = CARTESIAN_POINT ( 'NONE',  ( -56.05026940434684946, -8.611541138641610971, -0.7530887220977782182 ) ) ;
#27254 = CARTESIAN_POINT ( 'NONE',  ( -106.9429263765337907, 0.000000000000000000, 9.524999999999991473 ) ) ;
#27255 = DIRECTION ( 'NONE',  ( 3.624511343395739411E-17, -0.3420201433256632173, -0.9396926207859106484 ) ) ;
#27256 = CARTESIAN_POINT ( 'NONE',  ( 10.00000000000001954, 43.00000000000000000, -28.38386403503541899 ) ) ;
#27257 = CIRCLE ( 'NONE', #254, 10.00000000000000533 ) ;
#27258 = DIRECTION ( 'NONE',  ( 0.000000000000000000, -0.9944852160011111719, -0.1048768571002353378 ) ) ;
#27259 = ORIENTED_EDGE ( 'NONE', *, *, #24223, .T. ) ;
#27260 = DIRECTION ( 'NONE',  ( 0.000000000000000000, 0.000000000000000000, -1.000000000000000000 ) ) ;
#27261 = FILL_AREA_STYLE_COLOUR ( '', #45302 ) ;
#27262 = ORIENTED_EDGE ( 'NONE', *, *, #7684, .F. ) ;
#27263 = CIRCLE ( 'NONE', #14978, 0.2500000000000002220 ) ;
#27264 = CARTESIAN_POINT ( 'NONE',  ( -7.632228543268608334, 109.9570736234661581, 2.479861379858952830 ) ) ;
#27265 = STYLED_ITEM ( 'NONE', ( #67461 ), #55549 ) ;
#27266 = CARTESIAN_POINT ( 'NONE',  ( -19.89974874213240597, 115.4999999999999574, 10.00000000000000000 ) ) ;
#27267 = PRESENTATION_STYLE_ASSIGNMENT (( #10786 ) ) ;
#27268 = VERTEX_POINT ( 'NONE', #15205 ) ;
#27269 = ORIENTED_EDGE ( 'NONE', *, *, #7488, .F. ) ;
#27270 = AXIS2_PLACEMENT_3D ( 'NONE', #686, #6033, #64440 ) ;
#27271 = DIRECTION ( 'NONE',  ( 0.000000000000000000, 0.000000000000000000, -1.000000000000000000 ) ) ;
#27272 = DIRECTION ( 'NONE',  ( 0.000000000000000000, 0.000000000000000000, -1.000000000000000000 ) ) ;
#27273 = PLANE ( 'NONE',  #54040 ) ;
#27274 = EDGE_LOOP ( 'NONE', ( #8327, #17631, #7351, #42198 ) ) ;
#27275 = CARTESIAN_POINT ( 'NONE',  ( -3.094860106618432471, 125.7049999999999841, -9.525000000000000355 ) ) ;
#27276 = CARTESIAN_POINT ( 'NONE',  ( 12.72792206135785698, 114.9999999999999574, 10.50000000000000000 ) ) ;
#27277 = DIRECTION ( 'NONE',  ( -1.000000000000000000, -0.000000000000000000, -0.000000000000000000 ) ) ;
#27278 = AXIS2_PLACEMENT_3D ( 'NONE', #17762, #50805, #45212 ) ;
#27279 = EDGE_CURVE ( 'NONE', #58312, #40048, #25696, .T. ) ;
#27280 = CARTESIAN_POINT ( 'NONE',  ( 16.00000000000001776, 14.00000000000000000, -29.68999999999999417 ) ) ;
#27281 = CARTESIAN_POINT ( 'NONE',  ( -88.94499999999997897, -9.827790563157499189E-16, -8.024999999999991473 ) ) ;
#27282 = VERTEX_POINT ( 'NONE', #50807 ) ;
#27283 = EDGE_CURVE ( 'NONE', #29672, #44704, #19740, .T. ) ;
#27284 = CIRCLE ( 'NONE', #54275, 4.999999999999997335 ) ;
#27285 = CARTESIAN_POINT ( 'NONE',  ( 6.422934014168398598, 153.0000000000000000, 4.811085495980990778 ) ) ;
#27286 = EDGE_CURVE ( 'NONE', #65459, #29444, #46613, .T. ) ;
#27287 = CARTESIAN_POINT ( 'NONE',  ( 12.75000000000000533, 27.99999999999998224, -3.750000000000000000 ) ) ;
#27288 = ORIENTED_EDGE ( 'NONE', *, *, #12983, .T. ) ;
#27289 = CARTESIAN_POINT ( 'NONE',  ( -23.71231517720798365, 117.9999999999999716, -9.500000000000000000 ) ) ;
#27290 = SURFACE_SIDE_STYLE ('',( #524 ) ) ;
#27291 = EDGE_CURVE ( 'NONE', #15615, #49912, #36506, .T. ) ;
#27292 = CARTESIAN_POINT ( 'NONE',  ( 6.938426666069066329, -1.982292489777644828, 0.2088670156639322040 ) ) ;
#27293 = SURFACE_STYLE_USAGE ( .BOTH. , #58992 ) ;
#27294 = ADVANCED_FACE ( 'NONE', ( #62635 ), #9567, .F. ) ;
#27295 = EDGE_LOOP ( 'NONE', ( #36542, #43688, #17261 ) ) ;
#27296 = DIRECTION ( 'NONE',  ( 0.000000000000000000, 0.000000000000000000, 1.000000000000000000 ) ) ;
#27297 = ADVANCED_FACE ( 'NONE', ( #65428 ), #11261, .F. ) ;
#27298 = ORIENTED_EDGE ( 'NONE', *, *, #31912, .T. ) ;
#27299 = CARTESIAN_POINT ( 'NONE',  ( -165.5070736234661695, 8.102448949553176405, 5.886773742842740909 ) ) ;
#27300 = CARTESIAN_POINT ( 'NONE',  ( 8.000000000000030198, 0.000000000000000000, -29.00402776293826079 ) ) ;
#27301 = CARTESIAN_POINT ( 'NONE',  ( -44.99999999999998579, 119.9999999999999716, -10.00000000000000000 ) ) ;
#27302 = DIRECTION ( 'NONE',  ( 0.000000000000000000, 1.000000000000000000, 0.000000000000000000 ) ) ;
#27303 = STYLED_ITEM ( 'NONE', ( #43907 ), #47812 ) ;
#27304 = SURFACE_SIDE_STYLE ('',( #11144 ) ) ;
#27305 = CARTESIAN_POINT ( 'NONE',  ( -12.94269599874522214, 56.39257344741367461, -6.552927311739624727 ) ) ;
#27306 = CARTESIAN_POINT ( 'NONE',  ( 17.15973193263811680, -3.000000000000000000, -2.000000000000000000 ) ) ;
#27307 = EDGE_CURVE ( 'NONE', #17714, #52764, #54421, .T. ) ;
#27308 = LINE ( 'NONE', #26287, #66295 ) ;
#27309 = CARTESIAN_POINT ( 'NONE',  ( -7.255760115451132641, 153.3522680034007237, -4.196031671614308678 ) ) ;
#27310 = ORIENTED_EDGE ( 'NONE', *, *, #17580, .T. ) ;
#27311 = SURFACE_STYLE_USAGE ( .BOTH. , #43570 ) ;
#27312 = FACE_OUTER_BOUND ( 'NONE', #56853, .T. ) ;
#27313 = CARTESIAN_POINT ( 'NONE',  ( -5.196152422706634688, 9.000000000000008882, 7.500000000000000000 ) ) ;
#27314 = ORIENTED_EDGE ( 'NONE', *, *, #54905, .F. ) ;
#27315 = DIRECTION ( 'NONE',  ( 0.000000000000000000, 1.000000000000000000, 0.000000000000000000 ) ) ;
#27316 = COLOUR_RGB ( '', 0.72549020, 0.75294118, 0.79215686) ;
#27317 = CARTESIAN_POINT ( 'NONE',  ( -171.8050000000000068, -8.437984349512085203, 5.166775262442717831E-16 ) ) ;
#27318 = DIRECTION ( 'NONE',  ( 0.000000000000000000, 0.000000000000000000, -1.000000000000000000 ) ) ;
#27319 = DIRECTION ( 'NONE',  ( 0.000000000000000000, 0.000000000000000000, 1.000000000000000000 ) ) ;
#27320 = MANIFOLD_SOLID_BREP ( 'Mirror1', #45260 ) ;
#27321 = CARTESIAN_POINT ( 'NONE',  ( -172.3449999999999989, 7.632228543268599452, -2.479861379858951942 ) ) ;
#27322 = STYLED_ITEM ( 'NONE', ( #38973 ), #36751 ) ;
#27323 = CARTESIAN_POINT ( 'NONE',  ( -168.5949999999999989, 2.607480562269072433, 8.024999999999991473 ) ) ;
#27324 = EDGE_LOOP ( 'NONE', ( #32861, #55062, #42440, #8757 ) ) ;
#27325 = AXIS2_PLACEMENT_3D ( 'NONE', #33307, #6535, #66336 ) ;
#27326 = FILL_AREA_STYLE_COLOUR ( '', #15629 ) ;
#27327 = CARTESIAN_POINT ( 'NONE',  ( -35.65778776279520912, -8.171052631578938019, 2.722470280083845395 ) ) ;
#27328 = CARTESIAN_POINT ( 'NONE',  ( 71.99999999999998579, 119.9999999999997868, 7.000000000000000000 ) ) ;
#27329 = CARTESIAN_POINT ( 'NONE',  ( -7.632228543268607446, 150.5429263765338135, -2.479861379858953718 ) ) ;
#27330 = VECTOR ( 'NONE', #66396, 1000.000000000000000 ) ;
#27331 = CARTESIAN_POINT ( 'NONE',  ( -85.55499999999999261, 0.000000000000000000, 8.024999999999991473 ) ) ;
#27332 = CARTESIAN_POINT ( 'NONE',  ( 1.000000000000000000, 14.00000000000000000, 79.00402776293826435 ) ) ;
#27333 = CARTESIAN_POINT ( 'NONE',  ( 62.24999999999998579, 33.74999999999999289, -4.000000000000000000 ) ) ;
#27334 = AXIS2_PLACEMENT_3D ( 'NONE', #48560, #42267, #64703 ) ;
#27335 = CARTESIAN_POINT ( 'NONE',  ( -81.74499999999999034, 4.716976649647094177, 6.492361379858945902 ) ) ;
#27336 = CARTESIAN_POINT ( 'NONE',  ( 5.598654528085805993, 139.3549999999999898, 7.705886871421374629 ) ) ;
#27337 = CARTESIAN_POINT ( 'NONE',  ( -2.607480562269074653, 127.2929263765337993, 8.025000000000000355 ) ) ;
#27338 = LINE ( 'NONE', #38666, #5732 ) ;
#27339 = EDGE_CURVE ( 'NONE', #51702, #25674, #27755, .T. ) ;
#27340 =( GEOMETRIC_REPRESENTATION_CONTEXT ( 3 ) GLOBAL_UNCERTAINTY_ASSIGNED_CONTEXT ( ( #34927 ) ) GLOBAL_UNIT_ASSIGNED_CONTEXT ( ( #38990, #34687, #66720 ) ) REPRESENTATION_CONTEXT ( 'NONE', 'WORKASPACE' ) );
#27341 = FILL_AREA_STYLE ('',( #54437 ) ) ;
#27342 =( NAMED_UNIT ( * ) SI_UNIT ( $, .STERADIAN. ) SOLID_ANGLE_UNIT ( ) );
#27343 = VECTOR ( 'NONE', #60670, 1000.000000000000000 ) ;
#27344 = VERTEX_POINT ( 'NONE', #53818 ) ;
#27345 = CARTESIAN_POINT ( 'NONE',  ( -24.21231517720798010, 112.9999999999999858, 9.500000000000000000 ) ) ;
#27346 = STYLED_ITEM ( 'NONE', ( #58999 ), #62726 ) ;
#27347 = SURFACE_SIDE_STYLE ('',( #36333 ) ) ;
#27348 = DIRECTION ( 'NONE',  ( 1.000000000000000000, -3.469446951953611033E-15, 0.000000000000000000 ) ) ;
#27349 = CARTESIAN_POINT ( 'NONE',  ( 0.000000000000000000, 1.999999999999998668, 0.000000000000000000 ) ) ;
#27350 = ORIENTED_EDGE ( 'NONE', *, *, #65266, .F. ) ;
#27351 = ORIENTED_EDGE ( 'NONE', *, *, #60049, .T. ) ;
#27352 = COLOUR_RGB ( '', 0.72549020, 0.75294118, 0.79215686) ;
#27353 =( NAMED_UNIT ( * ) SI_UNIT ( $, .STERADIAN. ) SOLID_ANGLE_UNIT ( ) );
#27354 =( GEOMETRIC_REPRESENTATION_CONTEXT ( 3 ) GLOBAL_UNCERTAINTY_ASSIGNED_CONTEXT ( ( #36122 ) ) GLOBAL_UNIT_ASSIGNED_CONTEXT ( ( #50703, #13757, #29930 ) ) REPRESENTATION_CONTEXT ( 'NONE', 'WORKASPACE' ) );
#27355 =( NAMED_UNIT ( * ) SI_UNIT ( $, .STERADIAN. ) SOLID_ANGLE_UNIT ( ) );
#27356 = DIRECTION ( 'NONE',  ( 0.000000000000000000, 1.000000000000000000, 0.000000000000000000 ) ) ;
#27357 = DIRECTION ( 'NONE',  ( -0.000000000000000000, -0.000000000000000000, 1.000000000000000000 ) ) ;
#27358 = FILL_AREA_STYLE_COLOUR ( '', #22880 ) ;
#27359 = VERTEX_POINT ( 'NONE', #59799 ) ;
#27360 = CARTESIAN_POINT ( 'NONE',  ( -112.8550000000000040, 4.716976649647094177, 6.492361379858945902 ) ) ;
#27361 = ORIENTED_EDGE ( 'NONE', *, *, #21290, .T. ) ;
#27362 = DIRECTION ( 'NONE',  ( 0.000000000000000000, 0.000000000000000000, 1.000000000000000000 ) ) ;
#27363 = CIRCLE ( 'NONE', #376, 5.000000000000004441 ) ;
#27364 = EDGE_CURVE ( 'NONE', #48200, #43100, #3896, .T. ) ;
#27365 = VERTEX_POINT ( 'NONE', #69659 ) ;
#27366 = CARTESIAN_POINT ( 'NONE',  ( -72.00000000000000000, 35.92875272052971525, 7.500000000000000000 ) ) ;
#27367 = CARTESIAN_POINT ( 'NONE',  ( 44.99999999999977973, 146.9999999999999716, -7.000000000000000000 ) ) ;
#27368 = ORIENTED_EDGE ( 'NONE', *, *, #22553, .F. ) ;
#27369 = FILL_AREA_STYLE ('',( #31267 ) ) ;
#27370 =( BOUNDED_SURFACE ( )  B_SPLINE_SURFACE ( 1, 2, ( 
 ( #50622, #66812, #18264, #12978, #2361, #18623, #68536, #62544, #51316, #57275, #9106, #36206, #67849, #67484, #8415, #35132, #24224, #18931, #8750, #25598, #9808, #31218, #25267, #47114, #3061, #2731, #24551, #45729, #41839, #19644, #56586, #30176, #67141, #30523, #46424, #46066, #62205, #29848, #51662, #3417, #20336, #63254, #19279, #36576, #3779, #40430, #40786, #61843, #15103, #14029, #57634, #35489, #57994, #56936, #68195, #13672, #24910, #41139, #14359, #9456, #35829, #52023, #46790, #19973, #62885, #41472, #14732, #30883, #52381, #4131, #15777, #54067, #16491, #58660, #37955, #26962, #4479, #31573, #64967, #20695, #5874, #47473, #43238, #37259, #64283, #27317, #59015, #48850, #63597, #64642, #547, #47837, #42207, #32602, #21724, #22074, #69235, #10489, #21363, #63928, #58319, #43575, #48500, #16819, #31928, #4850, #59690, #15441, #69560, #42890, #10828, #53406, #25946, #38291, #68896, #32270, #26296, #5185, #11508, #21031, #52712, #37612, #59329, #199, #53055, #36905, #16135, #26629, #53721, #42529, #10140, #5512, #48152, #11158, #66719, #50545, #44269, #39317, #23443, #55808, #54415, #18535, #33656, #40022, #28001, #61411, #55099, #17514, #32980, #44948, #11859, #38989, #65667, #22770, #45298, #6554, #6926, #2267, #23797, #50202, #7611, #1596, #17839, #28351, #23123, #6235, #27663, #29047, #55463, #28713, #1924, #60380, #49171, #872, #22412, #43914, #65326, #17170, #49511, #1239, #7286, #66354, #60720, #38643, #60045, #44615, #49858, #18175, #33324, #66012, #12538, #34002, #12185, #39659, #54745, #61080, #12895, #34359, #8331, #45976, #7967, #40703, #46704, #67758, #35752, #56859, #13579, #4057, #51575, #2644, #24822, #9374, #35409, #56496, #36109, #19558, #20249, #41052, #51936, #13941, #3690, #41753, #62469, #57188, #9018, #45649, #67401, #19193, #67068, #14286, #62115, #40341, #30798, #8674, #61751, #25522, #24143, #50885, #34685, #68117, #57546, #47035, #3332, #13228, #30100, #52299, #46337, #35048, #30435, #25187, #19898, #41395, #29774, #18847, #51236, #56141, #29413, #62803, #68450, #2982, #24471, #14645, #16407, #63513, #471, #15368, #22001, #32521, #58582, #47384, #20959, #63174, #48080, #37174, #36823, #52971, #68816, #42453, #63846, #37881, #53985, #10063, #27234, #64197, #15010, #20606, #52635, #5786, #4764, #26879, #58240, #11071, #26216, #58939, #4392, #31140, #36485, #47757, #109, #48770, #31839, #42120, #10751, #53645, #69152, #57908, #42810, #15692, #10411, #69482, #48418, #32198, #53328, #9732, #5110, #5432, #31487, #26557, #21277, #16053, #21638, #37533, #43155, #64562, #25866, #59249, #7537, #60992, #54678, #49773, #33916, #66274, #64890, #28966, #44188, #50457, #38565, #2185, #65587, #27917, #43502, #55382, #22336, #49429, #6478, #33242, #55733, #17090, #17438, #12811, #34277, #60638, #18098, #12114, #28265, #38904, #33577, #16738, #38205, #39588, #65937, #39238, #12453, #1150, #59609, #11425, #32901, #54337, #6155, #27587, #59963, #11780, #17767, #7204, #1512, #49105, #792, #55013, #60307, #28634, #43831, #6842, #23039, #44534, #22687, #50126, #65237, #1854, #23368, #44867, #56415, #25106, #57107, #29692, #8931, #67673, #45214, #2557, #36023, #61339, #46622, #18454, #14212, #8250, #35325, #68040, #30027, #19826, #34604, #35674, #41315, #18782, #13149, #3603, #62395, #62718, #40261, #51162, #62031, #34967, #29327, #14548, #19475, #57465, #2907, #45570, #30710, #56063, #40615, #13860, #51489, #24397, #66638, #9289, #39938, #3248, #66990, #45892, #52215, #61663, #23716, #8593, #30352, #40976, #24066, #7879, #56779, #67321, #24736, #13494, #50806, #46253, #19109, #51856, #21561, #36750, #69411, #14922, #41666, #25447, #63440, #10666, #37800, #42382, #9649, #21199, #64120, #15287, #64480, #53248, #31402, #52896, #58505, #58858, #42723, #9982, #16323, #69076, #15973, #31065, #58167, #68730, #25790, #32120, #5034, #20878, #4681, #59175, #37455, #20526, #26134, #68369, #47671, #53573, #10329, #26484, #63771, #4306, #11002, #15620, #63084, #37094, #27, #31757, #47303, #26801, #48009, #32440, #5360, #48334, #43074, #3977, #46961, #20159, #36409, #57823, #52560, #42036, #59879, #16663, #61180, #16996, #11343, #50980, #11698, #32811, #67153, #64816, #21921, #5706, #18632, #8063, #45738, #22606, #13685, #27839, #2742, #44109, #54251, #39765, #12991, #40111, #49342, #49033, #59523, #38128, #27156, #392, #33167, #29516, #61858, #53901, #7707, #24237, #6071, #48685, #27506, #43431, #18941, #1062, #721, #54603, #22254, #34446, #66457, #43750, #65151, #38488, #6408, #18278, #40442, #55905, #29147, #50633, #2371, #23891, #45402, #66823, #61499, #13325, #34787, #56239, #36587, #68548, #41152, #20345, #9469, #56599, #14041, #47483, #3072, #58007, #29862, #25608, #19656, #46801, #9818, #41482, #31228, #46076, #47122, #52722, #30185, #24564, #15114, #4140, #4491, #51677, #62552, #3791, #46437, #40800, #25956, #30895, #68907, #67863, #56945, #42218, #67494, #52036, #25280, #62898, #14370, #8428, #20707, #51326, #14743, #8762, #35842, #63608, #3426, #35144, #19982, #41849, #52394, #35502, #19294, #68205, #57285, #36219, #24923, #62216, #57643, #9118, #30535, #63267, #32992, #26639, #21736, #5888, #38303, #36916, #49180, #16144, #22424, #10501, #882, #37623, #69571, #43925, #27331, #63940, #21376, #48163, #5197, #27672, #58670, #59026, #54425, #6245, #32617, #59704, #53732, #206, #10838, #5525, #15451, #58327, #11519, #37964, #11172, #54080, #42899, #10153, #31584, #53067, #4860, #26305, #47849, #31938, #53416, #59340, #48860, #43248, #69246, #21042, #26977, #32280, #559, #42541, #48510, #64653, #16499, #64293, #22084, #15788, #37270, #43585, #64976, #16831, #50214, #50556, #12904, #1607, #7979, #60728, #34369, #22782, #28360, #60390, #17527, #2279, #44959, #12547, #66021, #29423, #55817, #12194, #49869, #60056, #23135, #29058, #1935, #18185, #39328, #65679, #56154, #34013, #54755, #7296, #61421, #17848, #38997, #18546, #23452, #2656, #66365, #7623, #55474, #23807, #24151, #39671, #61093, #45309, #28012, #44625, #28723, #49523, #66730, #40033, #44280, #13238, #34696, #33667, #50895, #6567, #33333, #17182, #65337, #38657, #11870, #1251, #55109, #6936, #41764, #35759, #24478, #30447, #51946, #9387, #41063, #40715, #51246, #8342, #67075, #61762, #51586, #68462, #52645, #4404, #68128, #20258, #45986, #45658, #67409, #18858, #15024, #62477, #29786, #3342, #40350, #3704, #19570, #19205, #35420, #2990, #24833, #46350, #63184, #36497, #62126, #9745, #46715, #13591, #13952, #35058, #57922, #56869, #30812, #8682, #31151, #30108, #41408, #56505, #67772, #14297, #57198, #52312, #9029, #25200, #19908, #62812, #36123, #14655, #57558, #4065, #25531, #47045, #43169, #31852, #38218, #21293, #64576, #52982, #58595, #20968, #47767, #11084, #5442, #42820, #26567, #59619, #16420, #42465, #10424, #20619, #53339, #59259, #10761, #48434, #69494, #26231, #16749, #64209, #15381, #37549, #22011, #48089, #69163, #48780, #32209, #32915, #53657, #37891, #16065, #32534, #54348, #26893, #121, #21650, #58249, #5119, #58949, #10074, #54000, #5802, #4776, #43514, #27245, #63861, #11437, #36836, #63523, #47396, #481, #64902, #25879, #68824, #42131, #31498, #15703, #37185, #54687, #60650, #12467, #39602, #1524, #1164, #11790, #38576, #27597, #22348, #12125 ),
 ( #7216, #6166, #59976, #65251, #45226, #65601, #61007, #22699, #23727, #38915, #1870, #17102, #43842, #49118, #17451, #12823, #39951, #44549, #33254, #23378, #66286, #60319, #66652, #55394, #33590, #55029, #33929, #34290, #804, #18467, #6488, #28645, #49444, #6855, #55745, #44197, #13160, #50139, #44879, #18112, #27931, #28279, #23052, #49784, #7551, #65949, #61352, #28982, #34617, #17778, #39250, #50470, #2199, #62405, #46631, #9300, #7893, #20175, #56792, #63094, #51173, #41681, #8604, #40629, #14936, #68052, #34978, #62041, #67334, #45904, #68379, #29703, #30039, #3989, #25458, #3616, #30724, #24747, #40989, #51499, #46267, #46970, #56082, #52229, #8945, #51867, #25117, #13871, #50816, #29340, #2569, #24079, #45583, #67000, #2918, #24407, #30363, #19835, #14222, #18793, #40272, #67689, #3261, #41327, #61680, #19483, #35685, #57119, #19125, #62730, #56428, #13508, #35336, #8260, #14564, #57475, #36035, #42391, #36, #10676, #57835, #15299, #48696, #4314, #59180, #31074, #26807, #20888, #48015, #11008, #42733, #32446, #47315, #48345, #53912, #31412, #25800, #16333, #5367, #37810, #52904, #63782, #5043, #47680, #42045, #5715, #32129, #27161, #69085, #58175, #43440, #68742, #53259, #26492, #64132, #15627, #9665, #400, #37105, #64823, #4692, #21927, #58511, #10339, #36419, #21570, #36760, #31770, #69420, #26145, #52570, #9991, #21209, #20534, #63447, #53581, #15982, #37466, #58869, #43083, #64490, #55658, #16669, #39510, #39167, #12378, #55302, #22612, #11352, #38134, #12734, #59533, #28897, #7473, #59889, #11707, #60559, #33840, #44464, #6081, #49040, #28190, #38831, #28551, #54260, #6762, #17366, #60245, #33175, #49699, #17005, #50385, #49350, #43756, #1070, #18021, #50056, #44116, #1789, #7124, #32821, #65161, #2110, #27514, #60918, #729, #23299, #65515, #1434, #34207, #22964, #23638, #22262, #44799, #45143, #54609, #38495, #66195, #6415, #27847, #12040, #33503, #54935, #65868, #17698, #46541, #40900, #67969, #8173, #18718, #3900, #7804, #13789, #35244, #3169, #45824, #18385, #57394, #13082, #24660, #40191, #24331, #19752, #13424, #25375, #51422, #35603, #14143, #66919, #34536, #56705, #51089, #67601, #61597, #9218, #19403, #66562, #61960, #30637, #14470, #29614, #46179, #57042, #41248, #62645, #39870, #52144, #61274, #34892, #56338, #62321, #8858, #30279, #55994, #29253, #8526, #19037, #51779, #50735, #29961, #67249, #40548, #2840, #3528, #25033, #2481, #35947, #23990, #45505, #48258, #10599, #52828, #32045, #21134, #68299, #25707, #59114, #14846, #69672, #41586, #37373, #31330, #58431, #21485, #53171, #42997, #57747, #58781, #64402, #41955, #36323, #26734, #15892, #16251, #63361, #4606, #15546, #58102, #52494, #37728, #42639, #10934, #9913, #68651, #53833, #9578, #63703, #37022, #4961, #26063, #20083, #32369, #63005, #26410, #20451, #47597, #5630, #15216, #46896, #31692, #53508, #64045, #47230, #30996, #10257, #69002, #47942, #36682, #4232, #69342, #20809, #42316, #5289, #44722, #38413, #33427, #17625, #49976, #48617, #60836, #27770, #34118, #22186, #12652, #49274, #11626, #55575, #39092, #5994, #33091, #59812, #16927, #39434, #658, #982, #66115, #17943, #44385, #1711, #65440, #11970, #22531, #17289, #27082, #313, #23229, #49620, #22889, #65790, #54530, #21844, #43359, #64752, #60482, #16593, #38049, #38752, #59443, #44032, #11275, #60161, #27432, #54858, #6678, #12295, #28112, #43682, #32728, #54181, #48959, #65072, #6338, #1356, #33766, #55215, #7037, #28469, #7724, #14386, #29161, #35856, #46453, #2761, #61197, #34800, #7397, #61875, #50997, #50649, #66840, #13005, #56255, #8082, #30200, #67878, #23908, #41166, #8446, #28827, #34462, #66477, #19671, #18645, #40815, #2388, #24942, #40125, #3086, #18299, #45063, #50309, #61515, #14056, #62569, #45751, #55919, #24578, #67511, #13342, #2027, #56615, #29527, #24251, #13700, #62232, #46092, #67168, #23553, #18956, #19311, #45421, #40459, #35160, #29880, #35518, #51343, #56963, #8777, #39782, #51693, #3439, #20358, #52053, #16073, #22019, #43177, #11094, #32215, #57661, #49125, #26900, #46817, #131, #54356, #10769, #30911, #11449, #64585, #65259, #16432, #27254, #58955, #48786, #17113, #37899, #32544, #54008, #19998, #41862, #63280, #41503, #59266, #37557, #14757, #6174, #53663, #36234, #812, #68220, #25293, #64907, #22356, #48441, #62913, #5810, #486, #47141, #43851, #43522, #5451, #21658, #16757, #38228, #59629, #32923, #57303, #27607, #9132, #9489, #30551, #52407, #4153, #3808, #25623, #68567, #39259, #50826, #7560, #33598, #1534, #33264, #65955, #2207, #23385, #61016, #12476, #38925, #29347, #7225, #27940, #50149, #34629, #60658, #12131, #61361, #44889, #45591, #66296, #28989, #33938, #50478, #67010, #18122, #12832, #34297, #1173, #23060, #44557, #22708, #39610, #17785, #65612, #56089, #55400, #17457, #2581, #49452, #6497, #59982, #23734, #13170, #24088, #28652, #38588, #1877, #7903, #55757, #60326, #45233, #66660, #18475, #39956, #55040, #44205, #6864, #11795, #54695, #28289, #49792, #25809, #47323, #41338, #41688, #19137, #18801, #40638, #40282, #57849, #14232, #2926, #46280, #61691, #3628, #62414, #62048, #8614, #24415, #67698, #19492, #63105, #9671, #35345, #52579, #19843, #13518, #45913, #8270, #31083, #30047, #52238, #13879, #36429, #51507, #14574, #29714, #56438, #34989, #3268, #4325, #62741, #51179, #35694, #67342, #56800, #24756, #25126, #9311, #14946, #40996, #57126, #8954, #30370, #51875, #46639, #68058, #36043, #57484, #30735, #3995, #25466, #46979, #68389, #20182, #42402, #21219, #16679, #38143, #16344, #21939, #37477, #53592, #69429, #58879, #59544, #68751, #43449, #21578, #64499, #37817, #5052, #63458, #20542, #64833, #42054, #11364, #32830, #63791, #15635, #43091, #59189, #26820, #58183, #31419, #10685, #42741, #11015, #36770, #32136, #64138, #15992, #37115, #5375, #69094, #54270, #31782, #26153, #53268, #409, #32456, #26499, #53925, #5725, #15310, #47689, #6092, #10001, #27524, #52913, #27172, #48024, #48355, #4704, #45, #20895, #58521, #48707, #10351, #49362, #65171, #66204, #7133, #18032, #1081, #17377, #49708, #44125, #11717, #39517, #33848, #60928, #65529, #27857, #50393, #38506, #28200, #1445, #65877, #12050, #739, #55667, #43768, #17709, #22621, #60252, #12744, #38840, #2118, #44475, #28562, #55310, #54617, #17018, #22976, #33516, #60569, #6429, #54946, #33184, #7481, #59899, #6773, #22270, #1797, #34216, #28907, #39175, #49050, #12388, #50066, #23309, #44806, #15471, #67927, #63324, #63665, #30599, #57707, #62961, #41543, #64004, #25340, #4198, #69304, #21098, #68964, #4916, #42597, #35901, #15508, #9537, #47190, #57350, #30955, #10558, #36643, #25671, #52105, #14803, #9181, #52454, #68611, #26368, #15852, #68265, #37332, #52788, #51743, #3855, #41213, #58741, #36285, #36978, #46860, #3489, #20408, #47550, #62612, #19719, #24990, #41911, #58387, #46499, #15176, #20045, #20770, #42280, #58064, #14428, #31290, #9874, #4563, #26017, #10213, #31649, #53130, #47906, #27390, #935, #59079, #64713, #27037, #53789, #17246, #11575, #48920, #32680, #44340, #22487, #48571, #16552, #26697, #59400, #65398, #16888, #54483, #5947, #32337, #22842, #619, #21439, #43637, #28066, #54133, #5590, #54814, #38366, #39048, #59767, #43984, #22140, #38711, #60445, #33050 ) ),
 .UNSPECIFIED., .F., .F., .F. ) 
 B_SPLINE_SURFACE_WITH_KNOTS ( ( 2, 2 ),
 ( 3, 2, 2, 2, 2, 2, 2, 2, 2, 2, 2, 2, 2, 2, 2, 2, 2, 2, 2, 2, 2, 2, 2, 2, 2, 2, 2, 2, 2, 2, 2, 2, 2, 2, 2, 2, 2, 2, 2, 2, 2, 2, 2, 2, 2, 2, 2, 2, 2, 2, 2, 2, 2, 2, 2, 2, 2, 2, 2, 2, 2, 2, 2, 2, 2, 2, 2, 2, 2, 2, 2, 2, 2, 2, 2, 2, 2, 2, 2, 2, 2, 2, 2, 2, 2, 2, 2, 2, 2, 2, 2, 2, 2, 2, 2, 2, 2, 2, 2, 2, 2, 2, 2, 2, 2, 2, 2, 2, 2, 2, 2, 2, 2, 2, 2, 2, 2, 2, 2, 2, 2, 2, 2, 2, 2, 2, 2, 2, 2, 2, 2, 2, 2, 2, 2, 2, 2, 2, 2, 2, 2, 2, 2, 2, 2, 2, 2, 2, 2, 2, 2, 2, 2, 2, 2, 2, 2, 2, 2, 2, 2, 2, 2, 2, 2, 2, 2, 2, 2, 2, 2, 2, 2, 2, 2, 2, 2, 2, 2, 2, 2, 2, 2, 2, 2, 2, 2, 2, 2, 2, 2, 2, 2, 2, 2, 2, 2, 2, 2, 2, 2, 2, 2, 2, 2, 2, 2, 2, 2, 2, 2, 2, 2, 2, 2, 2, 2, 2, 2, 2, 2, 2, 2, 2, 2, 2, 2, 2, 2, 2, 2, 2, 2, 2, 2, 2, 2, 2, 2, 2, 2, 2, 2, 2, 2, 2, 2, 2, 2, 2, 2, 2, 2, 2, 2, 2, 2, 2, 2, 2, 2, 2, 2, 2, 2, 2, 2, 2, 2, 2, 2, 2, 2, 2, 2, 2, 2, 2, 2, 2, 2, 2, 2, 2, 2, 2, 2, 2, 2, 2, 2, 2, 2, 2, 2, 2, 2, 2, 2, 2, 2, 2, 2, 2, 2, 2, 2, 2, 2, 2, 2, 2, 2, 2, 2, 2, 2, 2, 2, 2, 2, 2, 2, 2, 2, 2, 2, 2, 2, 2, 2, 2, 2, 2, 2, 2, 2, 2, 2, 2, 2, 2, 2, 2, 2, 2, 2, 2, 2, 2, 2, 2, 2, 2, 2, 2, 2, 2, 2, 2, 2, 2, 2, 2, 2, 2, 2, 2, 2, 2, 2, 2, 2, 2, 2, 2, 2, 2, 2, 2, 2, 2, 2, 2, 2, 2, 2, 2, 2, 2, 2, 2, 2, 2, 2, 2, 2, 2, 2, 2, 2, 2, 2, 2, 2, 2, 2, 2, 2, 2, 2, 2, 2, 2, 2, 2, 2, 2, 2, 2, 2, 2, 2, 2, 2, 2, 2, 2, 2, 2, 2, 2, 2, 2, 2, 2, 2, 2, 2, 2, 2, 2, 2, 2, 2, 2, 2, 2, 2, 2, 2, 2, 2, 2, 2, 2, 3 ),
 ( 0.000000000000000000, 1.000000000000000000 ),
 ( 0.000000000000000000, 0.002173913043478260896, 0.004347826086956521792, 0.006521739130434782254, 0.008695652173913043584, 0.01086956521739130405, 0.01304347826086956451, 0.01521739130434782671, 0.01739130434782608717, 0.01956521739130434936, 0.02173913043478260809, 0.02391304347826087029, 0.02608695652173912902, 0.02826086956521739121, 0.03043478260869565341, 0.03260869565217391214, 0.03478260869565217434, 0.03695652173913043653, 0.03913043478260869873, 0.04130434782608695399, 0.04347826086956521618, 0.04565217391304347838, 0.04782608695652174058, 0.05000000000000000278, 0.05217391304347825803, 0.05434782608695652023, 0.05652173913043478243, 0.05869565217391304462, 0.06086956521739130682, 0.06304347826086956208, 0.06521739130434782428, 0.06739130434782608647, 0.06956521739130434867, 0.07173913043478261087, 0.07391304347826087306, 0.07608695652173913526, 0.07826086956521739746, 0.08043478260869564578, 0.08260869565217390798, 0.08478260869565217017, 0.08695652173913043237, 0.08913043478260869457, 0.09130434782608695676, 0.09347826086956521896, 0.09565217391304348116, 0.09782608695652174335, 0.1000000000000000056, 0.1021739130434782677, 0.1043478260869565161, 0.1065217391304347783, 0.1086956521739130405, 0.1108695652173913027, 0.1130434782608695649, 0.1152173913043478271, 0.1173913043478260892, 0.1195652173913043514, 0.1217391304347826136, 0.1239130434782608758, 0.1260869565217391242, 0.1282608695652174002, 0.1304347826086956486, 0.1326086956521739246, 0.1347826086956521729, 0.1369565217391304213, 0.1391304347826086973, 0.1413043478260869457, 0.1434782608695652217, 0.1456521739130434701, 0.1478260869565217461, 0.1499999999999999944, 0.1521739130434782705, 0.1543478260869565188, 0.1565217391304347949, 0.1586956521739130432, 0.1608695652173912916, 0.1630434782608695676, 0.1652173913043478160, 0.1673913043478260920, 0.1695652173913043403, 0.1717391304347826164, 0.1739130434782608647, 0.1760869565217391408, 0.1782608695652173891, 0.1804347826086956652, 0.1826086956521739135, 0.1847826086956521618, 0.1869565217391304379, 0.1891304347826086862, 0.1913043478260869623, 0.1934782608695652106, 0.1956521739130434867, 0.1978260869565217350, 0.2000000000000000111, 0.2021739130434782594, 0.2043478260869565355, 0.2065217391304347838, 0.2086956521739130321, 0.2108695652173913082, 0.2130434782608695565, 0.2152173913043478326, 0.2173913043478260809, 0.2195652173913043570, 0.2217391304347826053, 0.2239130434782608814, 0.2260869565217391297, 0.2282608695652173780, 0.2304347826086956541, 0.2326086956521739024, 0.2347826086956521785, 0.2369565217391304268, 0.2391304347826087029, 0.2413043478260869512, 0.2434782608695652273, 0.2456521739130434756, 0.2478260869565217517, 0.2500000000000000000, 0.2521739130434782483, 0.2543478260869564966, 0.2565217391304348005, 0.2586956521739130488, 0.2608695652173912971, 0.2630434782608695454, 0.2652173913043478493, 0.2673913043478260976, 0.2695652173913043459, 0.2717391304347825942, 0.2739130434782608425, 0.2760869565217391464, 0.2782608695652173947, 0.2804347826086956430, 0.2826086956521738913, 0.2847826086956521952, 0.2869565217391304435, 0.2891304347826086918, 0.2913043478260869401, 0.2934782608695652439, 0.2956521739130434923, 0.2978260869565217406, 0.2999999999999999889, 0.3021739130434782372, 0.3043478260869565410, 0.3065217391304347894, 0.3086956521739130377, 0.3108695652173912860, 0.3130434782608695898, 0.3152173913043478382, 0.3173913043478260865, 0.3195652173913043348, 0.3217391304347825831, 0.3239130434782608869, 0.3260869565217391353, 0.3282608695652173836, 0.3304347826086956319, 0.3326086956521739357, 0.3347826086956521840, 0.3369565217391304324, 0.3391304347826086807, 0.3413043478260869290, 0.3434782608695652328, 0.3456521739130434812, 0.3478260869565217295, 0.3499999999999999778, 0.3521739130434782816, 0.3543478260869565299, 0.3565217391304347783, 0.3586956521739130266, 0.3608695652173913304, 0.3630434782608695787, 0.3652173913043478271, 0.3673913043478260754, 0.3695652173913043237, 0.3717391304347826275, 0.3739130434782608758, 0.3760869565217391242, 0.3782608695652173725, 0.3804347826086956763, 0.3826086956521739246, 0.3847826086956521729, 0.3869565217391304213, 0.3891304347826086696, 0.3913043478260869734, 0.3934782608695652217, 0.3956521739130434701, 0.3978260869565217184, 0.4000000000000000222, 0.4021739130434782705, 0.4043478260869565188, 0.4065217391304347672, 0.4086956521739130710, 0.4108695652173913193, 0.4130434782608695676, 0.4152173913043478160, 0.4173913043478260643, 0.4195652173913043681, 0.4217391304347826164, 0.4239130434782608647, 0.4260869565217391131, 0.4282608695652174169, 0.4304347826086956652, 0.4326086956521739135, 0.4347826086956521618, 0.4369565217391304102, 0.4391304347826087140, 0.4413043478260869623, 0.4434782608695652106, 0.4456521739130434590, 0.4478260869565217628, 0.4500000000000000111, 0.4521739130434782594, 0.4543478260869565077, 0.4565217391304347561, 0.4586956521739130599, 0.4608695652173913082, 0.4630434782608695565, 0.4652173913043478048, 0.4673913043478261087, 0.4695652173913043570, 0.4717391304347826053, 0.4739130434782608536, 0.4760869565217391575, 0.4782608695652174058, 0.4804347826086956541, 0.4826086956521739024, 0.4847826086956521507, 0.4869565217391304546, 0.4891304347826087029, 0.4913043478260869512, 0.4934782608695651995, 0.4956521739130435034, 0.4978260869565217517, 0.5000000000000000000, 0.5021739130434782483, 0.5043478260869564966, 0.5065217391304347450, 0.5086956521739129933, 0.5108695652173913526, 0.5130434782608696009, 0.5152173913043478493, 0.5173913043478260976, 0.5195652173913043459, 0.5217391304347825942, 0.5239130434782608425, 0.5260869565217390909, 0.5282608695652173392, 0.5304347826086956985, 0.5326086956521739468, 0.5347826086956521952, 0.5369565217391304435, 0.5391304347826086918, 0.5413043478260869401, 0.5434782608695651884, 0.5456521739130434367, 0.5478260869565216851, 0.5500000000000000444, 0.5521739130434782927, 0.5543478260869565410, 0.5565217391304347894, 0.5586956521739130377, 0.5608695652173912860, 0.5630434782608695343, 0.5652173913043477826, 0.5673913043478261420, 0.5695652173913043903, 0.5717391304347826386, 0.5739130434782608869, 0.5760869565217391353, 0.5782608695652173836, 0.5804347826086956319, 0.5826086956521738802, 0.5847826086956521285, 0.5869565217391304879, 0.5891304347826087362, 0.5913043478260869845, 0.5934782608695652328, 0.5956521739130434812, 0.5978260869565217295, 0.5999999999999999778, 0.6021739130434782261, 0.6043478260869564744, 0.6065217391304348338, 0.6086956521739130821, 0.6108695652173913304, 0.6130434782608695787, 0.6152173913043478271, 0.6173913043478260754, 0.6195652173913043237, 0.6217391304347825720, 0.6239130434782608203, 0.6260869565217391797, 0.6282608695652174280, 0.6304347826086956763, 0.6326086956521739246, 0.6347826086956521729, 0.6369565217391304213, 0.6391304347826086696, 0.6413043478260869179, 0.6434782608695651662, 0.6456521739130435256, 0.6478260869565217739, 0.6500000000000000222, 0.6521739130434782705, 0.6543478260869565188, 0.6565217391304347672, 0.6586956521739130155, 0.6608695652173912638, 0.6630434782608695121, 0.6652173913043478715, 0.6673913043478261198, 0.6695652173913043681, 0.6717391304347826164, 0.6739130434782608647, 0.6760869565217391131, 0.6782608695652173614, 0.6804347826086956097, 0.6826086956521738580, 0.6847826086956522174, 0.6869565217391304657, 0.6891304347826087140, 0.6913043478260869623, 0.6934782608695652106, 0.6956521739130434590, 0.6978260869565217073, 0.6999999999999999556, 0.7021739130434783149, 0.7043478260869565633, 0.7065217391304348116, 0.7086956521739130599, 0.7108695652173913082, 0.7130434782608695565, 0.7152173913043478048, 0.7173913043478260532, 0.7195652173913043015, 0.7217391304347826608, 0.7239130434782609091, 0.7260869565217391575, 0.7282608695652174058, 0.7304347826086956541, 0.7326086956521739024, 0.7347826086956521507, 0.7369565217391303991, 0.7391304347826086474, 0.7413043478260870067, 0.7434782608695652550, 0.7456521739130435034, 0.7478260869565217517, 0.7500000000000000000, 0.7521739130434782483, 0.7543478260869564966, 0.7565217391304347450, 0.7586956521739129933, 0.7608695652173913526, 0.7630434782608696009, 0.7652173913043478493, 0.7673913043478260976, 0.7695652173913043459, 0.7717391304347825942, 0.7739130434782608425, 0.7760869565217390909, 0.7782608695652173392, 0.7804347826086956985, 0.7826086956521739468, 0.7847826086956521952, 0.7869565217391304435, 0.7891304347826086918, 0.7913043478260869401, 0.7934782608695651884, 0.7956521739130434367, 0.7978260869565216851, 0.8000000000000000444, 0.8021739130434782927, 0.8043478260869565410, 0.8065217391304347894, 0.8086956521739130377, 0.8108695652173912860, 0.8130434782608695343, 0.8152173913043477826, 0.8173913043478261420, 0.8195652173913043903, 0.8217391304347826386, 0.8239130434782608869, 0.8260869565217391353, 0.8282608695652173836, 0.8304347826086956319, 0.8326086956521738802, 0.8347826086956521285, 0.8369565217391304879, 0.8391304347826087362, 0.8413043478260869845, 0.8434782608695652328, 0.8456521739130434812, 0.8478260869565217295, 0.8499999999999999778, 0.8521739130434782261, 0.8543478260869564744, 0.8565217391304348338, 0.8586956521739130821, 0.8608695652173913304, 0.8630434782608695787, 0.8652173913043478271, 0.8673913043478260754, 0.8695652173913043237, 0.8717391304347825720, 0.8739130434782608203, 0.8760869565217391797, 0.8782608695652174280, 0.8804347826086956763, 0.8826086956521739246, 0.8847826086956521729, 0.8869565217391304213, 0.8891304347826086696, 0.8913043478260869179, 0.8934782608695651662, 0.8956521739130435256, 0.8978260869565217739, 0.9000000000000000222, 0.9021739130434782705, 0.9043478260869565188, 0.9065217391304347672, 0.9086956521739130155, 0.9108695652173912638, 0.9130434782608695121, 0.9152173913043478715, 0.9173913043478261198, 0.9195652173913043681, 0.9217391304347826164, 0.9239130434782608647, 0.9260869565217391131, 0.9282608695652173614, 0.9304347826086956097, 0.9326086956521738580, 0.9347826086956522174, 0.9369565217391304657, 0.9391304347826087140, 0.9413043478260869623, 0.9434782608695652106, 0.9456521739130434590, 0.9478260869565217073, 0.9499999999999999556, 0.9521739130434783149, 0.9543478260869565633, 0.9565217391304348116, 0.9586956521739130599, 0.9608695652173913082, 0.9630434782608695565, 0.9652173913043478048, 0.9673913043478260532, 0.9695652173913043015, 0.9717391304347826608, 0.9739130434782609091, 0.9760869565217391575, 0.9782608695652174058, 0.9804347826086956541, 0.9826086956521739024, 0.9847826086956521507, 0.9869565217391303991, 0.9891304347826086474, 0.9913043478260870067 ),
 .UNSPECIFIED. ) 
 GEOMETRIC_REPRESENTATION_ITEM ( )  RATIONAL_B_SPLINE_SURFACE ( (
 ( 1.000000000000000000, 0.9510565162951535312, 1.000000000000000000, 0.9510565162951535312, 1.000000000000000000, 0.9510565162951535312, 1.000000000000000000, 0.9510565162951535312, 1.000000000000000000, 0.9510565162951535312, 1.000000000000000000, 0.9510565162951535312, 1.000000000000000000, 0.9510565162951535312, 1.000000000000000000, 0.9510565162951535312, 1.000000000000000000, 0.9510565162951535312, 1.000000000000000000, 0.9510565162951535312, 1.000000000000000000, 0.9510565162951535312, 1.000000000000000000, 0.9510565162951535312, 1.000000000000000000, 0.9510565162951535312, 1.000000000000000000, 0.9510565162951535312, 1.000000000000000000, 0.9510565162951535312, 1.000000000000000000, 0.9510565162951535312, 1.000000000000000000, 0.9510565162951535312, 1.000000000000000000, 0.9510565162951535312, 1.000000000000000000, 0.9510565162951535312, 1.000000000000000000, 0.9510565162951535312, 1.000000000000000000, 0.9510565162951535312, 1.000000000000000000, 0.9510565162951535312, 1.000000000000000000, 0.9510565162951535312, 1.000000000000000000, 0.9510565162951535312, 1.000000000000000000, 0.9510565162951535312, 1.000000000000000000, 0.9510565162951535312, 1.000000000000000000, 0.9510565162951535312, 1.000000000000000000, 0.9510565162951535312, 1.000000000000000000, 0.9510565162951535312, 1.000000000000000000, 0.9510565162951535312, 1.000000000000000000, 0.9510565162951535312, 1.000000000000000000, 0.9510565162951535312, 1.000000000000000000, 0.9510565162951535312, 1.000000000000000000, 0.9510565162951535312, 1.000000000000000000, 0.9510565162951535312, 1.000000000000000000, 0.9510565162951535312, 1.000000000000000000, 0.9510565162951535312, 1.000000000000000000, 0.9510565162951535312, 1.000000000000000000, 0.9510565162951535312, 1.000000000000000000, 0.9510565162951535312, 1.000000000000000000, 0.9510565162951535312, 1.000000000000000000, 0.9510565162951535312, 1.000000000000000000, 0.9510565162951535312, 1.000000000000000000, 0.9510565162951535312, 1.000000000000000000, 0.9510565162951535312, 1.000000000000000000, 0.9510565162951535312, 1.000000000000000000, 0.9510565162951535312, 1.000000000000000000, 0.9510565162951535312, 1.000000000000000000, 0.9510565162951535312, 1.000000000000000000, 0.9510565162951535312, 1.000000000000000000, 0.9510565162951535312, 1.000000000000000000, 0.9510565162951535312, 1.000000000000000000, 0.9510565162951535312, 1.000000000000000000, 0.9510565162951535312, 1.000000000000000000, 0.9510565162951535312, 1.000000000000000000, 0.9510565162951535312, 1.000000000000000000, 0.9510565162951535312, 1.000000000000000000, 0.9510565162951535312, 1.000000000000000000, 0.9510565162951535312, 1.000000000000000000, 0.9510565162951535312, 1.000000000000000000, 0.9510565162951535312, 1.000000000000000000, 0.9510565162951535312, 1.000000000000000000, 0.9510565162951535312, 1.000000000000000000, 0.9510565162951535312, 1.000000000000000000, 0.9510565162951535312, 1.000000000000000000, 0.9510565162951535312, 1.000000000000000000, 0.9510565162951535312, 1.000000000000000000, 0.9510565162951535312, 1.000000000000000000, 0.9510565162951535312, 1.000000000000000000, 0.9510565162951535312, 1.000000000000000000, 0.9510565162951535312, 1.000000000000000000, 0.9510565162951535312, 1.000000000000000000, 0.9510565162951535312, 1.000000000000000000, 0.9510565162951535312, 1.000000000000000000, 0.9510565162951535312, 1.000000000000000000, 0.9510565162951535312, 1.000000000000000000, 0.9510565162951535312, 1.000000000000000000, 0.9510565162951535312, 1.000000000000000000, 0.9510565162951535312, 1.000000000000000000, 0.9510565162951535312, 1.000000000000000000, 0.9510565162951535312, 1.000000000000000000, 0.9510565162951535312, 1.000000000000000000, 0.9510565162951535312, 1.000000000000000000, 0.9510565162951535312, 1.000000000000000000, 0.9510565162951535312, 1.000000000000000000, 0.9510565162951535312, 1.000000000000000000, 0.9510565162951535312, 1.000000000000000000, 0.9510565162951535312, 1.000000000000000000, 0.9510565162951535312, 1.000000000000000000, 0.9510565162951535312, 1.000000000000000000, 0.9510565162951535312, 1.000000000000000000, 0.9510565162951535312, 1.000000000000000000, 0.9510565162951535312, 1.000000000000000000, 0.9510565162951535312, 1.000000000000000000, 0.9510565162951535312, 1.000000000000000000, 0.9510565162951535312, 1.000000000000000000, 0.9510565162951535312, 1.000000000000000000, 0.9510565162951535312, 1.000000000000000000, 0.9510565162951535312, 1.000000000000000000, 0.9510565162951535312, 1.000000000000000000, 0.9510565162951535312, 1.000000000000000000, 0.9510565162951535312, 1.000000000000000000, 0.9510565162951535312, 1.000000000000000000, 0.9510565162951535312, 1.000000000000000000, 0.9510565162951535312, 1.000000000000000000, 0.9510565162951535312, 1.000000000000000000, 0.9510565162951535312, 1.000000000000000000, 0.9510565162951535312, 1.000000000000000000, 0.9510565162951535312, 1.000000000000000000, 0.9510565162951535312, 1.000000000000000000, 0.9510565162951535312, 1.000000000000000000, 0.9510565162951535312, 1.000000000000000000, 0.9510565162951535312, 1.000000000000000000, 0.9510565162951535312, 1.000000000000000000, 0.9510565162951535312, 1.000000000000000000, 0.9510565162951535312, 1.000000000000000000, 0.9510565162951535312, 1.000000000000000000, 0.9510565162951535312, 1.000000000000000000, 0.9510565162951535312, 1.000000000000000000, 0.9510565162951535312, 1.000000000000000000, 0.9510565162951535312, 1.000000000000000000, 0.9510565162951535312, 1.000000000000000000, 0.9510565162951535312, 1.000000000000000000, 0.9510565162951535312, 1.000000000000000000, 0.9510565162951535312, 1.000000000000000000, 0.9510565162951535312, 1.000000000000000000, 0.9510565162951535312, 1.000000000000000000, 0.9510565162951535312, 1.000000000000000000, 0.9510565162951535312, 1.000000000000000000, 0.9510565162951535312, 1.000000000000000000, 0.9510565162951535312, 1.000000000000000000, 0.9510565162951535312, 1.000000000000000000, 0.9510565162951535312, 1.000000000000000000, 0.9510565162951535312, 1.000000000000000000, 0.9510565162951535312, 1.000000000000000000, 0.9510565162951535312, 1.000000000000000000, 0.9510565162951535312, 1.000000000000000000, 0.9510565162951535312, 1.000000000000000000, 0.9510565162951535312, 1.000000000000000000, 0.9510565162951535312, 1.000000000000000000, 0.9510565162951535312, 1.000000000000000000, 0.9510565162951535312, 1.000000000000000000, 0.9510565162951535312, 1.000000000000000000, 0.9510565162951535312, 1.000000000000000000, 0.9510565162951535312, 1.000000000000000000, 0.9510565162951535312, 1.000000000000000000, 0.9510565162951535312, 1.000000000000000000, 0.9510565162951535312, 1.000000000000000000, 0.9510565162951535312, 1.000000000000000000, 0.9510565162951535312, 1.000000000000000000, 0.9510565162951535312, 1.000000000000000000, 0.9510565162951535312, 1.000000000000000000, 0.9510565162951535312, 1.000000000000000000, 0.9510565162951535312, 1.000000000000000000, 0.9510565162951535312, 1.000000000000000000, 0.9510565162951535312, 1.000000000000000000, 0.9510565162951535312, 1.000000000000000000, 0.9510565162951535312, 1.000000000000000000, 0.9510565162951535312, 1.000000000000000000, 0.9510565162951535312, 1.000000000000000000, 0.9510565162951535312, 1.000000000000000000, 0.9510565162951535312, 1.000000000000000000, 0.9510565162951535312, 1.000000000000000000, 0.9510565162951535312, 1.000000000000000000, 0.9510565162951535312, 1.000000000000000000, 0.9510565162951535312, 1.000000000000000000, 0.9510565162951535312, 1.000000000000000000, 0.9510565162951535312, 1.000000000000000000, 0.9510565162951535312, 1.000000000000000000, 0.9510565162951535312, 1.000000000000000000, 0.9510565162951535312, 1.000000000000000000, 0.9510565162951535312, 1.000000000000000000, 0.9510565162951535312, 1.000000000000000000, 0.9510565162951535312, 1.000000000000000000, 0.9510565162951535312, 1.000000000000000000, 0.9510565162951535312, 1.000000000000000000, 0.9510565162951535312, 1.000000000000000000, 0.9510565162951535312, 1.000000000000000000, 0.9510565162951535312, 1.000000000000000000, 0.9510565162951535312, 1.000000000000000000, 0.9510565162951535312, 1.000000000000000000, 0.9510565162951535312, 1.000000000000000000, 0.9510565162951535312, 1.000000000000000000, 0.9510565162951535312, 1.000000000000000000, 0.9510565162951535312, 1.000000000000000000, 0.9510565162951535312, 1.000000000000000000, 0.9510565162951535312, 1.000000000000000000, 0.9510565162951535312, 1.000000000000000000, 0.9510565162951535312, 1.000000000000000000, 0.9510565162951535312, 1.000000000000000000, 0.9510565162951535312, 1.000000000000000000, 0.9510565162951535312, 1.000000000000000000, 0.9510565162951535312, 1.000000000000000000, 0.9510565162951535312, 1.000000000000000000, 0.9510565162951535312, 1.000000000000000000, 0.9510565162951535312, 1.000000000000000000, 0.9510565162951535312, 1.000000000000000000, 0.9510565162951535312, 1.000000000000000000, 0.9510565162951535312, 1.000000000000000000, 0.9510565162951535312, 1.000000000000000000, 0.9510565162951535312, 1.000000000000000000, 0.9510565162951535312, 1.000000000000000000, 0.9510565162951535312, 1.000000000000000000, 0.9510565162951535312, 1.000000000000000000, 0.9510565162951535312, 1.000000000000000000, 0.9510565162951535312, 1.000000000000000000, 0.9510565162951535312, 1.000000000000000000, 0.9510565162951535312, 1.000000000000000000, 0.9510565162951535312, 1.000000000000000000, 0.9510565162951535312, 1.000000000000000000, 0.9510565162951535312, 1.000000000000000000, 0.9510565162951535312, 1.000000000000000000, 0.9510565162951535312, 1.000000000000000000, 0.9510565162951535312, 1.000000000000000000, 0.9510565162951535312, 1.000000000000000000, 0.9510565162951535312, 1.000000000000000000, 0.9510565162951535312, 1.000000000000000000, 0.9510565162951535312, 1.000000000000000000, 0.9510565162951535312, 1.000000000000000000, 0.9510565162951535312, 1.000000000000000000, 0.9510565162951535312, 1.000000000000000000, 0.9510565162951535312, 1.000000000000000000, 0.9510565162951535312, 1.000000000000000000, 0.9510565162951535312, 1.000000000000000000, 0.9510565162951535312, 1.000000000000000000, 0.9510565162951535312, 1.000000000000000000, 0.9510565162951535312, 1.000000000000000000, 0.9510565162951535312, 1.000000000000000000, 0.9510565162951535312, 1.000000000000000000, 0.9510565162951535312, 1.000000000000000000, 0.9510565162951535312, 1.000000000000000000, 0.9510565162951535312, 1.000000000000000000, 0.9510565162951535312, 1.000000000000000000, 0.9510565162951535312, 1.000000000000000000, 0.9510565162951535312, 1.000000000000000000, 0.9510565162951535312, 1.000000000000000000, 0.9510565162951535312, 1.000000000000000000, 0.9510565162951535312, 1.000000000000000000, 0.9510565162951535312, 1.000000000000000000, 0.9510565162951535312, 1.000000000000000000, 0.9510565162951535312, 1.000000000000000000, 0.9510565162951535312, 1.000000000000000000, 0.9510565162951535312, 1.000000000000000000, 0.9510565162951535312, 1.000000000000000000, 0.9510565162951535312, 1.000000000000000000, 0.9510565162951535312, 1.000000000000000000, 0.9510565162951535312, 1.000000000000000000, 0.9510565162951535312, 1.000000000000000000, 0.9510565162951535312, 1.000000000000000000, 0.9510565162951535312, 1.000000000000000000, 0.9510565162951535312, 1.000000000000000000, 0.9510565162951535312, 1.000000000000000000, 0.9510565162951535312, 1.000000000000000000, 0.9510565162951535312, 1.000000000000000000, 0.9510565162951535312, 1.000000000000000000, 0.9510565162951535312, 1.000000000000000000, 0.9510565162951535312, 1.000000000000000000, 0.9510565162951535312, 1.000000000000000000, 0.9510565162951535312, 1.000000000000000000, 0.9510565162951535312, 1.000000000000000000, 0.9510565162951535312, 1.000000000000000000, 0.9510565162951535312, 1.000000000000000000, 0.9510565162951535312, 1.000000000000000000, 0.9510565162951535312, 1.000000000000000000, 0.9510565162951535312, 1.000000000000000000, 0.9510565162951535312, 1.000000000000000000, 0.9510565162951535312, 1.000000000000000000, 0.9510565162951535312, 1.000000000000000000, 0.9510565162951535312, 1.000000000000000000, 0.9510565162951535312, 1.000000000000000000, 0.9510565162951535312, 1.000000000000000000, 0.9510565162951535312, 1.000000000000000000, 0.9510565162951535312, 1.000000000000000000, 0.9510565162951535312, 1.000000000000000000, 0.9510565162951535312, 1.000000000000000000, 0.9510565162951535312, 1.000000000000000000, 0.9510565162951535312, 1.000000000000000000, 0.9510565162951535312, 1.000000000000000000, 0.9510565162951535312, 1.000000000000000000, 0.9510565162951535312, 1.000000000000000000, 0.9510565162951535312, 1.000000000000000000, 0.9510565162951535312, 1.000000000000000000, 0.9510565162951535312, 1.000000000000000000, 0.9510565162951535312, 1.000000000000000000, 0.9510565162951535312, 1.000000000000000000, 0.9510565162951535312, 1.000000000000000000, 0.9510565162951535312, 1.000000000000000000, 0.9510565162951535312, 1.000000000000000000, 0.9510565162951535312, 1.000000000000000000, 0.9510565162951535312, 1.000000000000000000, 0.9510565162951535312, 1.000000000000000000, 0.9510565162951535312, 1.000000000000000000, 0.9510565162951535312, 1.000000000000000000, 0.9510565162951535312, 1.000000000000000000, 0.9510565162951535312, 1.000000000000000000, 0.9510565162951535312, 1.000000000000000000, 0.9510565162951535312, 1.000000000000000000, 0.9510565162951535312, 1.000000000000000000, 0.9510565162951535312, 1.000000000000000000, 0.9510565162951535312, 1.000000000000000000, 0.9510565162951535312, 1.000000000000000000, 0.9510565162951535312, 1.000000000000000000, 0.9510565162951535312, 1.000000000000000000, 0.9510565162951535312, 1.000000000000000000, 0.9510565162951535312, 1.000000000000000000, 0.9510565162951535312, 1.000000000000000000, 0.9510565162951535312, 1.000000000000000000, 0.9510565162951535312, 1.000000000000000000, 0.9510565162951535312, 1.000000000000000000, 0.9510565162951535312, 1.000000000000000000, 0.9510565162951535312, 1.000000000000000000, 0.9510565162951535312, 1.000000000000000000, 0.9510565162951535312, 1.000000000000000000, 0.9510565162951535312, 1.000000000000000000, 0.9510565162951535312, 1.000000000000000000, 0.9510565162951535312, 1.000000000000000000, 0.9510565162951535312, 1.000000000000000000, 0.9510565162951535312, 1.000000000000000000, 0.9510565162951535312, 1.000000000000000000, 0.9510565162951535312, 1.000000000000000000, 0.9510565162951535312, 1.000000000000000000, 0.9510565162951535312, 1.000000000000000000, 0.9510565162951535312, 1.000000000000000000, 0.9510565162951535312, 1.000000000000000000, 0.9510565162951535312, 1.000000000000000000, 0.9510565162951535312, 1.000000000000000000, 0.9510565162951535312, 1.000000000000000000, 0.9510565162951535312, 1.000000000000000000, 0.9510565162951535312, 1.000000000000000000, 0.9510565162951535312, 1.000000000000000000, 0.9510565162951535312, 1.000000000000000000, 0.9510565162951535312, 1.000000000000000000, 0.9510565162951535312, 1.000000000000000000, 0.9510565162951535312, 1.000000000000000000, 0.9510565162951535312, 1.000000000000000000, 0.9510565162951535312, 1.000000000000000000, 0.9510565162951535312, 1.000000000000000000, 0.9510565162951535312, 1.000000000000000000, 0.9510565162951535312, 1.000000000000000000, 0.9510565162951535312, 1.000000000000000000, 0.9510565162951535312, 1.000000000000000000, 0.9510565162951535312, 1.000000000000000000, 0.9510565162951535312, 1.000000000000000000, 0.9510565162951535312, 1.000000000000000000, 0.9510565162951535312, 1.000000000000000000, 0.9510565162951535312, 1.000000000000000000, 0.9510565162951535312, 1.000000000000000000, 0.9510565162951535312, 1.000000000000000000, 0.9510565162951535312, 1.000000000000000000, 0.9510565162951535312, 1.000000000000000000, 0.9510565162951535312, 1.000000000000000000, 0.9510565162951535312, 1.000000000000000000, 0.9510565162951535312, 1.000000000000000000, 0.9510565162951535312, 1.000000000000000000, 0.9510565162951535312, 1.000000000000000000, 0.9510565162951535312, 1.000000000000000000, 0.9510565162951535312, 1.000000000000000000, 0.9510565162951535312, 1.000000000000000000, 0.9510565162951535312, 1.000000000000000000, 0.9510565162951535312, 1.000000000000000000, 0.9510565162951535312, 1.000000000000000000, 0.9510565162951535312, 1.000000000000000000, 0.9510565162951535312, 1.000000000000000000, 0.9510565162951535312, 1.000000000000000000, 0.9510565162951535312, 1.000000000000000000, 0.9510565162951535312, 1.000000000000000000, 0.9510565162951535312, 1.000000000000000000, 0.9510565162951535312, 1.000000000000000000, 0.9510565162951535312, 1.000000000000000000, 0.9510565162951535312, 1.000000000000000000, 0.9510565162951535312, 1.000000000000000000, 0.9510565162951535312, 1.000000000000000000, 0.9510565162951535312, 1.000000000000000000, 0.9510565162951535312, 1.000000000000000000, 0.9510565162951535312, 1.000000000000000000, 0.9510565162951535312, 1.000000000000000000, 0.9510565162951535312, 1.000000000000000000, 0.9510565162951535312, 1.000000000000000000, 0.9510565162951535312, 1.000000000000000000, 0.9510565162951535312, 1.000000000000000000, 0.9510565162951535312, 1.000000000000000000, 0.9510565162951535312, 1.000000000000000000, 0.9510565162951535312, 1.000000000000000000, 0.9510565162951535312, 1.000000000000000000, 0.9510565162951535312, 1.000000000000000000, 0.9510565162951535312, 1.000000000000000000, 0.9510565162951535312, 1.000000000000000000, 0.9510565162951535312, 1.000000000000000000, 0.9510565162951535312, 1.000000000000000000, 0.9510565162951535312, 1.000000000000000000, 0.9510565162951535312, 1.000000000000000000, 0.9510565162951535312, 1.000000000000000000, 0.9510565162951535312, 1.000000000000000000, 0.9510565162951535312, 1.000000000000000000, 0.9510565162951535312, 1.000000000000000000, 0.9510565162951535312, 1.000000000000000000, 0.9510565162951535312, 1.000000000000000000, 0.9510565162951535312, 1.000000000000000000, 0.9510565162951535312, 1.000000000000000000, 0.9510565162951535312, 1.000000000000000000, 0.9510565162951535312, 1.000000000000000000, 0.9510565162951535312, 1.000000000000000000, 0.9510565162951535312, 1.000000000000000000, 0.9510565162951535312, 1.000000000000000000, 0.9510565162951535312, 1.000000000000000000, 0.9510565162951535312, 1.000000000000000000, 0.9510565162951535312, 1.000000000000000000, 0.9510565162951535312, 1.000000000000000000, 0.9510565162951535312, 1.000000000000000000, 0.9510565162951535312, 1.000000000000000000, 0.9510565162951535312, 1.000000000000000000, 0.9510565162951535312, 1.000000000000000000, 0.9510565162951535312, 1.000000000000000000, 0.9510565162951535312, 1.000000000000000000, 0.9510565162951535312, 1.000000000000000000, 0.9510565162951535312, 1.000000000000000000, 0.9510565162951535312, 1.000000000000000000, 0.9510565162951535312, 1.000000000000000000, 0.9510565162951535312, 1.000000000000000000, 0.9510565162951535312, 1.000000000000000000, 0.9510565162951535312, 1.000000000000000000, 0.9510565162951535312, 1.000000000000000000, 0.9510565162951535312, 1.000000000000000000, 0.9510565162951535312, 1.000000000000000000, 0.9510565162951535312, 1.000000000000000000, 0.9510565162951535312, 1.000000000000000000, 0.9510565162951535312, 1.000000000000000000, 0.9510565162951535312, 1.000000000000000000, 0.9510565162951535312, 1.000000000000000000, 0.9510565162951535312, 1.000000000000000000, 0.9510565162951535312, 1.000000000000000000, 0.9510565162951535312, 1.000000000000000000, 0.9510565162951535312, 1.000000000000000000, 0.9510565162951535312, 1.000000000000000000, 0.9510565162951535312, 1.000000000000000000, 0.9510565162951535312, 1.000000000000000000, 0.9510565162951535312, 1.000000000000000000, 0.9510565162951535312, 1.000000000000000000, 0.9510565162951535312, 1.000000000000000000, 0.9510565162951535312, 1.000000000000000000, 0.9510565162951535312, 1.000000000000000000, 0.9510565162951535312, 1.000000000000000000, 0.9510565162951535312, 1.000000000000000000, 0.9510565162951535312, 1.000000000000000000, 0.9510565162951535312, 1.000000000000000000, 0.9510565162951535312, 1.000000000000000000, 0.9510565162951535312, 1.000000000000000000, 0.9510565162951535312, 1.000000000000000000, 0.9510565162951535312, 1.000000000000000000, 0.9510565162951535312, 1.000000000000000000, 0.9510565162951535312, 1.000000000000000000, 0.9510565162951535312, 1.000000000000000000, 0.9510565162951535312, 1.000000000000000000, 0.9510565162951535312, 1.000000000000000000, 0.9510565162951535312, 1.000000000000000000, 0.9510565162951535312, 1.000000000000000000),
 ( 1.000000000000000000, 0.9510565162951535312, 1.000000000000000000, 0.9510565162951535312, 1.000000000000000000, 0.9510565162951535312, 1.000000000000000000, 0.9510565162951535312, 1.000000000000000000, 0.9510565162951535312, 1.000000000000000000, 0.9510565162951535312, 1.000000000000000000, 0.9510565162951535312, 1.000000000000000000, 0.9510565162951535312, 1.000000000000000000, 0.9510565162951535312, 1.000000000000000000, 0.9510565162951535312, 1.000000000000000000, 0.9510565162951535312, 1.000000000000000000, 0.9510565162951535312, 1.000000000000000000, 0.9510565162951535312, 1.000000000000000000, 0.9510565162951535312, 1.000000000000000000, 0.9510565162951535312, 1.000000000000000000, 0.9510565162951535312, 1.000000000000000000, 0.9510565162951535312, 1.000000000000000000, 0.9510565162951535312, 1.000000000000000000, 0.9510565162951535312, 1.000000000000000000, 0.9510565162951535312, 1.000000000000000000, 0.9510565162951535312, 1.000000000000000000, 0.9510565162951535312, 1.000000000000000000, 0.9510565162951535312, 1.000000000000000000, 0.9510565162951535312, 1.000000000000000000, 0.9510565162951535312, 1.000000000000000000, 0.9510565162951535312, 1.000000000000000000, 0.9510565162951535312, 1.000000000000000000, 0.9510565162951535312, 1.000000000000000000, 0.9510565162951535312, 1.000000000000000000, 0.9510565162951535312, 1.000000000000000000, 0.9510565162951535312, 1.000000000000000000, 0.9510565162951535312, 1.000000000000000000, 0.9510565162951535312, 1.000000000000000000, 0.9510565162951535312, 1.000000000000000000, 0.9510565162951535312, 1.000000000000000000, 0.9510565162951535312, 1.000000000000000000, 0.9510565162951535312, 1.000000000000000000, 0.9510565162951535312, 1.000000000000000000, 0.9510565162951535312, 1.000000000000000000, 0.9510565162951535312, 1.000000000000000000, 0.9510565162951535312, 1.000000000000000000, 0.9510565162951535312, 1.000000000000000000, 0.9510565162951535312, 1.000000000000000000, 0.9510565162951535312, 1.000000000000000000, 0.9510565162951535312, 1.000000000000000000, 0.9510565162951535312, 1.000000000000000000, 0.9510565162951535312, 1.000000000000000000, 0.9510565162951535312, 1.000000000000000000, 0.9510565162951535312, 1.000000000000000000, 0.9510565162951535312, 1.000000000000000000, 0.9510565162951535312, 1.000000000000000000, 0.9510565162951535312, 1.000000000000000000, 0.9510565162951535312, 1.000000000000000000, 0.9510565162951535312, 1.000000000000000000, 0.9510565162951535312, 1.000000000000000000, 0.9510565162951535312, 1.000000000000000000, 0.9510565162951535312, 1.000000000000000000, 0.9510565162951535312, 1.000000000000000000, 0.9510565162951535312, 1.000000000000000000, 0.9510565162951535312, 1.000000000000000000, 0.9510565162951535312, 1.000000000000000000, 0.9510565162951535312, 1.000000000000000000, 0.9510565162951535312, 1.000000000000000000, 0.9510565162951535312, 1.000000000000000000, 0.9510565162951535312, 1.000000000000000000, 0.9510565162951535312, 1.000000000000000000, 0.9510565162951535312, 1.000000000000000000, 0.9510565162951535312, 1.000000000000000000, 0.9510565162951535312, 1.000000000000000000, 0.9510565162951535312, 1.000000000000000000, 0.9510565162951535312, 1.000000000000000000, 0.9510565162951535312, 1.000000000000000000, 0.9510565162951535312, 1.000000000000000000, 0.9510565162951535312, 1.000000000000000000, 0.9510565162951535312, 1.000000000000000000, 0.9510565162951535312, 1.000000000000000000, 0.9510565162951535312, 1.000000000000000000, 0.9510565162951535312, 1.000000000000000000, 0.9510565162951535312, 1.000000000000000000, 0.9510565162951535312, 1.000000000000000000, 0.9510565162951535312, 1.000000000000000000, 0.9510565162951535312, 1.000000000000000000, 0.9510565162951535312, 1.000000000000000000, 0.9510565162951535312, 1.000000000000000000, 0.9510565162951535312, 1.000000000000000000, 0.9510565162951535312, 1.000000000000000000, 0.9510565162951535312, 1.000000000000000000, 0.9510565162951535312, 1.000000000000000000, 0.9510565162951535312, 1.000000000000000000, 0.9510565162951535312, 1.000000000000000000, 0.9510565162951535312, 1.000000000000000000, 0.9510565162951535312, 1.000000000000000000, 0.9510565162951535312, 1.000000000000000000, 0.9510565162951535312, 1.000000000000000000, 0.9510565162951535312, 1.000000000000000000, 0.9510565162951535312, 1.000000000000000000, 0.9510565162951535312, 1.000000000000000000, 0.9510565162951535312, 1.000000000000000000, 0.9510565162951535312, 1.000000000000000000, 0.9510565162951535312, 1.000000000000000000, 0.9510565162951535312, 1.000000000000000000, 0.9510565162951535312, 1.000000000000000000, 0.9510565162951535312, 1.000000000000000000, 0.9510565162951535312, 1.000000000000000000, 0.9510565162951535312, 1.000000000000000000, 0.9510565162951535312, 1.000000000000000000, 0.9510565162951535312, 1.000000000000000000, 0.9510565162951535312, 1.000000000000000000, 0.9510565162951535312, 1.000000000000000000, 0.9510565162951535312, 1.000000000000000000, 0.9510565162951535312, 1.000000000000000000, 0.9510565162951535312, 1.000000000000000000, 0.9510565162951535312, 1.000000000000000000, 0.9510565162951535312, 1.000000000000000000, 0.9510565162951535312, 1.000000000000000000, 0.9510565162951535312, 1.000000000000000000, 0.9510565162951535312, 1.000000000000000000, 0.9510565162951535312, 1.000000000000000000, 0.9510565162951535312, 1.000000000000000000, 0.9510565162951535312, 1.000000000000000000, 0.9510565162951535312, 1.000000000000000000, 0.9510565162951535312, 1.000000000000000000, 0.9510565162951535312, 1.000000000000000000, 0.9510565162951535312, 1.000000000000000000, 0.9510565162951535312, 1.000000000000000000, 0.9510565162951535312, 1.000000000000000000, 0.9510565162951535312, 1.000000000000000000, 0.9510565162951535312, 1.000000000000000000, 0.9510565162951535312, 1.000000000000000000, 0.9510565162951535312, 1.000000000000000000, 0.9510565162951535312, 1.000000000000000000, 0.9510565162951535312, 1.000000000000000000, 0.9510565162951535312, 1.000000000000000000, 0.9510565162951535312, 1.000000000000000000, 0.9510565162951535312, 1.000000000000000000, 0.9510565162951535312, 1.000000000000000000, 0.9510565162951535312, 1.000000000000000000, 0.9510565162951535312, 1.000000000000000000, 0.9510565162951535312, 1.000000000000000000, 0.9510565162951535312, 1.000000000000000000, 0.9510565162951535312, 1.000000000000000000, 0.9510565162951535312, 1.000000000000000000, 0.9510565162951535312, 1.000000000000000000, 0.9510565162951535312, 1.000000000000000000, 0.9510565162951535312, 1.000000000000000000, 0.9510565162951535312, 1.000000000000000000, 0.9510565162951535312, 1.000000000000000000, 0.9510565162951535312, 1.000000000000000000, 0.9510565162951535312, 1.000000000000000000, 0.9510565162951535312, 1.000000000000000000, 0.9510565162951535312, 1.000000000000000000, 0.9510565162951535312, 1.000000000000000000, 0.9510565162951535312, 1.000000000000000000, 0.9510565162951535312, 1.000000000000000000, 0.9510565162951535312, 1.000000000000000000, 0.9510565162951535312, 1.000000000000000000, 0.9510565162951535312, 1.000000000000000000, 0.9510565162951535312, 1.000000000000000000, 0.9510565162951535312, 1.000000000000000000, 0.9510565162951535312, 1.000000000000000000, 0.9510565162951535312, 1.000000000000000000, 0.9510565162951535312, 1.000000000000000000, 0.9510565162951535312, 1.000000000000000000, 0.9510565162951535312, 1.000000000000000000, 0.9510565162951535312, 1.000000000000000000, 0.9510565162951535312, 1.000000000000000000, 0.9510565162951535312, 1.000000000000000000, 0.9510565162951535312, 1.000000000000000000, 0.9510565162951535312, 1.000000000000000000, 0.9510565162951535312, 1.000000000000000000, 0.9510565162951535312, 1.000000000000000000, 0.9510565162951535312, 1.000000000000000000, 0.9510565162951535312, 1.000000000000000000, 0.9510565162951535312, 1.000000000000000000, 0.9510565162951535312, 1.000000000000000000, 0.9510565162951535312, 1.000000000000000000, 0.9510565162951535312, 1.000000000000000000, 0.9510565162951535312, 1.000000000000000000, 0.9510565162951535312, 1.000000000000000000, 0.9510565162951535312, 1.000000000000000000, 0.9510565162951535312, 1.000000000000000000, 0.9510565162951535312, 1.000000000000000000, 0.9510565162951535312, 1.000000000000000000, 0.9510565162951535312, 1.000000000000000000, 0.9510565162951535312, 1.000000000000000000, 0.9510565162951535312, 1.000000000000000000, 0.9510565162951535312, 1.000000000000000000, 0.9510565162951535312, 1.000000000000000000, 0.9510565162951535312, 1.000000000000000000, 0.9510565162951535312, 1.000000000000000000, 0.9510565162951535312, 1.000000000000000000, 0.9510565162951535312, 1.000000000000000000, 0.9510565162951535312, 1.000000000000000000, 0.9510565162951535312, 1.000000000000000000, 0.9510565162951535312, 1.000000000000000000, 0.9510565162951535312, 1.000000000000000000, 0.9510565162951535312, 1.000000000000000000, 0.9510565162951535312, 1.000000000000000000, 0.9510565162951535312, 1.000000000000000000, 0.9510565162951535312, 1.000000000000000000, 0.9510565162951535312, 1.000000000000000000, 0.9510565162951535312, 1.000000000000000000, 0.9510565162951535312, 1.000000000000000000, 0.9510565162951535312, 1.000000000000000000, 0.9510565162951535312, 1.000000000000000000, 0.9510565162951535312, 1.000000000000000000, 0.9510565162951535312, 1.000000000000000000, 0.9510565162951535312, 1.000000000000000000, 0.9510565162951535312, 1.000000000000000000, 0.9510565162951535312, 1.000000000000000000, 0.9510565162951535312, 1.000000000000000000, 0.9510565162951535312, 1.000000000000000000, 0.9510565162951535312, 1.000000000000000000, 0.9510565162951535312, 1.000000000000000000, 0.9510565162951535312, 1.000000000000000000, 0.9510565162951535312, 1.000000000000000000, 0.9510565162951535312, 1.000000000000000000, 0.9510565162951535312, 1.000000000000000000, 0.9510565162951535312, 1.000000000000000000, 0.9510565162951535312, 1.000000000000000000, 0.9510565162951535312, 1.000000000000000000, 0.9510565162951535312, 1.000000000000000000, 0.9510565162951535312, 1.000000000000000000, 0.9510565162951535312, 1.000000000000000000, 0.9510565162951535312, 1.000000000000000000, 0.9510565162951535312, 1.000000000000000000, 0.9510565162951535312, 1.000000000000000000, 0.9510565162951535312, 1.000000000000000000, 0.9510565162951535312, 1.000000000000000000, 0.9510565162951535312, 1.000000000000000000, 0.9510565162951535312, 1.000000000000000000, 0.9510565162951535312, 1.000000000000000000, 0.9510565162951535312, 1.000000000000000000, 0.9510565162951535312, 1.000000000000000000, 0.9510565162951535312, 1.000000000000000000, 0.9510565162951535312, 1.000000000000000000, 0.9510565162951535312, 1.000000000000000000, 0.9510565162951535312, 1.000000000000000000, 0.9510565162951535312, 1.000000000000000000, 0.9510565162951535312, 1.000000000000000000, 0.9510565162951535312, 1.000000000000000000, 0.9510565162951535312, 1.000000000000000000, 0.9510565162951535312, 1.000000000000000000, 0.9510565162951535312, 1.000000000000000000, 0.9510565162951535312, 1.000000000000000000, 0.9510565162951535312, 1.000000000000000000, 0.9510565162951535312, 1.000000000000000000, 0.9510565162951535312, 1.000000000000000000, 0.9510565162951535312, 1.000000000000000000, 0.9510565162951535312, 1.000000000000000000, 0.9510565162951535312, 1.000000000000000000, 0.9510565162951535312, 1.000000000000000000, 0.9510565162951535312, 1.000000000000000000, 0.9510565162951535312, 1.000000000000000000, 0.9510565162951535312, 1.000000000000000000, 0.9510565162951535312, 1.000000000000000000, 0.9510565162951535312, 1.000000000000000000, 0.9510565162951535312, 1.000000000000000000, 0.9510565162951535312, 1.000000000000000000, 0.9510565162951535312, 1.000000000000000000, 0.9510565162951535312, 1.000000000000000000, 0.9510565162951535312, 1.000000000000000000, 0.9510565162951535312, 1.000000000000000000, 0.9510565162951535312, 1.000000000000000000, 0.9510565162951535312, 1.000000000000000000, 0.9510565162951535312, 1.000000000000000000, 0.9510565162951535312, 1.000000000000000000, 0.9510565162951535312, 1.000000000000000000, 0.9510565162951535312, 1.000000000000000000, 0.9510565162951535312, 1.000000000000000000, 0.9510565162951535312, 1.000000000000000000, 0.9510565162951535312, 1.000000000000000000, 0.9510565162951535312, 1.000000000000000000, 0.9510565162951535312, 1.000000000000000000, 0.9510565162951535312, 1.000000000000000000, 0.9510565162951535312, 1.000000000000000000, 0.9510565162951535312, 1.000000000000000000, 0.9510565162951535312, 1.000000000000000000, 0.9510565162951535312, 1.000000000000000000, 0.9510565162951535312, 1.000000000000000000, 0.9510565162951535312, 1.000000000000000000, 0.9510565162951535312, 1.000000000000000000, 0.9510565162951535312, 1.000000000000000000, 0.9510565162951535312, 1.000000000000000000, 0.9510565162951535312, 1.000000000000000000, 0.9510565162951535312, 1.000000000000000000, 0.9510565162951535312, 1.000000000000000000, 0.9510565162951535312, 1.000000000000000000, 0.9510565162951535312, 1.000000000000000000, 0.9510565162951535312, 1.000000000000000000, 0.9510565162951535312, 1.000000000000000000, 0.9510565162951535312, 1.000000000000000000, 0.9510565162951535312, 1.000000000000000000, 0.9510565162951535312, 1.000000000000000000, 0.9510565162951535312, 1.000000000000000000, 0.9510565162951535312, 1.000000000000000000, 0.9510565162951535312, 1.000000000000000000, 0.9510565162951535312, 1.000000000000000000, 0.9510565162951535312, 1.000000000000000000, 0.9510565162951535312, 1.000000000000000000, 0.9510565162951535312, 1.000000000000000000, 0.9510565162951535312, 1.000000000000000000, 0.9510565162951535312, 1.000000000000000000, 0.9510565162951535312, 1.000000000000000000, 0.9510565162951535312, 1.000000000000000000, 0.9510565162951535312, 1.000000000000000000, 0.9510565162951535312, 1.000000000000000000, 0.9510565162951535312, 1.000000000000000000, 0.9510565162951535312, 1.000000000000000000, 0.9510565162951535312, 1.000000000000000000, 0.9510565162951535312, 1.000000000000000000, 0.9510565162951535312, 1.000000000000000000, 0.9510565162951535312, 1.000000000000000000, 0.9510565162951535312, 1.000000000000000000, 0.9510565162951535312, 1.000000000000000000, 0.9510565162951535312, 1.000000000000000000, 0.9510565162951535312, 1.000000000000000000, 0.9510565162951535312, 1.000000000000000000, 0.9510565162951535312, 1.000000000000000000, 0.9510565162951535312, 1.000000000000000000, 0.9510565162951535312, 1.000000000000000000, 0.9510565162951535312, 1.000000000000000000, 0.9510565162951535312, 1.000000000000000000, 0.9510565162951535312, 1.000000000000000000, 0.9510565162951535312, 1.000000000000000000, 0.9510565162951535312, 1.000000000000000000, 0.9510565162951535312, 1.000000000000000000, 0.9510565162951535312, 1.000000000000000000, 0.9510565162951535312, 1.000000000000000000, 0.9510565162951535312, 1.000000000000000000, 0.9510565162951535312, 1.000000000000000000, 0.9510565162951535312, 1.000000000000000000, 0.9510565162951535312, 1.000000000000000000, 0.9510565162951535312, 1.000000000000000000, 0.9510565162951535312, 1.000000000000000000, 0.9510565162951535312, 1.000000000000000000, 0.9510565162951535312, 1.000000000000000000, 0.9510565162951535312, 1.000000000000000000, 0.9510565162951535312, 1.000000000000000000, 0.9510565162951535312, 1.000000000000000000, 0.9510565162951535312, 1.000000000000000000, 0.9510565162951535312, 1.000000000000000000, 0.9510565162951535312, 1.000000000000000000, 0.9510565162951535312, 1.000000000000000000, 0.9510565162951535312, 1.000000000000000000, 0.9510565162951535312, 1.000000000000000000, 0.9510565162951535312, 1.000000000000000000, 0.9510565162951535312, 1.000000000000000000, 0.9510565162951535312, 1.000000000000000000, 0.9510565162951535312, 1.000000000000000000, 0.9510565162951535312, 1.000000000000000000, 0.9510565162951535312, 1.000000000000000000, 0.9510565162951535312, 1.000000000000000000, 0.9510565162951535312, 1.000000000000000000, 0.9510565162951535312, 1.000000000000000000, 0.9510565162951535312, 1.000000000000000000, 0.9510565162951535312, 1.000000000000000000, 0.9510565162951535312, 1.000000000000000000, 0.9510565162951535312, 1.000000000000000000, 0.9510565162951535312, 1.000000000000000000, 0.9510565162951535312, 1.000000000000000000, 0.9510565162951535312, 1.000000000000000000, 0.9510565162951535312, 1.000000000000000000, 0.9510565162951535312, 1.000000000000000000, 0.9510565162951535312, 1.000000000000000000, 0.9510565162951535312, 1.000000000000000000, 0.9510565162951535312, 1.000000000000000000, 0.9510565162951535312, 1.000000000000000000, 0.9510565162951535312, 1.000000000000000000, 0.9510565162951535312, 1.000000000000000000, 0.9510565162951535312, 1.000000000000000000, 0.9510565162951535312, 1.000000000000000000, 0.9510565162951535312, 1.000000000000000000, 0.9510565162951535312, 1.000000000000000000, 0.9510565162951535312, 1.000000000000000000, 0.9510565162951535312, 1.000000000000000000, 0.9510565162951535312, 1.000000000000000000, 0.9510565162951535312, 1.000000000000000000, 0.9510565162951535312, 1.000000000000000000, 0.9510565162951535312, 1.000000000000000000, 0.9510565162951535312, 1.000000000000000000, 0.9510565162951535312, 1.000000000000000000, 0.9510565162951535312, 1.000000000000000000, 0.9510565162951535312, 1.000000000000000000, 0.9510565162951535312, 1.000000000000000000, 0.9510565162951535312, 1.000000000000000000, 0.9510565162951535312, 1.000000000000000000, 0.9510565162951535312, 1.000000000000000000, 0.9510565162951535312, 1.000000000000000000, 0.9510565162951535312, 1.000000000000000000, 0.9510565162951535312, 1.000000000000000000, 0.9510565162951535312, 1.000000000000000000, 0.9510565162951535312, 1.000000000000000000, 0.9510565162951535312, 1.000000000000000000, 0.9510565162951535312, 1.000000000000000000, 0.9510565162951535312, 1.000000000000000000, 0.9510565162951535312, 1.000000000000000000, 0.9510565162951535312, 1.000000000000000000, 0.9510565162951535312, 1.000000000000000000, 0.9510565162951535312, 1.000000000000000000, 0.9510565162951535312, 1.000000000000000000, 0.9510565162951535312, 1.000000000000000000, 0.9510565162951535312, 1.000000000000000000, 0.9510565162951535312, 1.000000000000000000, 0.9510565162951535312, 1.000000000000000000, 0.9510565162951535312, 1.000000000000000000, 0.9510565162951535312, 1.000000000000000000, 0.9510565162951535312, 1.000000000000000000, 0.9510565162951535312, 1.000000000000000000, 0.9510565162951535312, 1.000000000000000000, 0.9510565162951535312, 1.000000000000000000, 0.9510565162951535312, 1.000000000000000000, 0.9510565162951535312, 1.000000000000000000, 0.9510565162951535312, 1.000000000000000000, 0.9510565162951535312, 1.000000000000000000, 0.9510565162951535312, 1.000000000000000000, 0.9510565162951535312, 1.000000000000000000, 0.9510565162951535312, 1.000000000000000000, 0.9510565162951535312, 1.000000000000000000, 0.9510565162951535312, 1.000000000000000000, 0.9510565162951535312, 1.000000000000000000, 0.9510565162951535312, 1.000000000000000000, 0.9510565162951535312, 1.000000000000000000, 0.9510565162951535312, 1.000000000000000000, 0.9510565162951535312, 1.000000000000000000, 0.9510565162951535312, 1.000000000000000000, 0.9510565162951535312, 1.000000000000000000, 0.9510565162951535312, 1.000000000000000000, 0.9510565162951535312, 1.000000000000000000, 0.9510565162951535312, 1.000000000000000000, 0.9510565162951535312, 1.000000000000000000, 0.9510565162951535312, 1.000000000000000000, 0.9510565162951535312, 1.000000000000000000, 0.9510565162951535312, 1.000000000000000000, 0.9510565162951535312, 1.000000000000000000, 0.9510565162951535312, 1.000000000000000000, 0.9510565162951535312, 1.000000000000000000, 0.9510565162951535312, 1.000000000000000000, 0.9510565162951535312, 1.000000000000000000, 0.9510565162951535312, 1.000000000000000000, 0.9510565162951535312, 1.000000000000000000, 0.9510565162951535312, 1.000000000000000000, 0.9510565162951535312, 1.000000000000000000, 0.9510565162951535312, 1.000000000000000000, 0.9510565162951535312, 1.000000000000000000, 0.9510565162951535312, 1.000000000000000000, 0.9510565162951535312, 1.000000000000000000, 0.9510565162951535312, 1.000000000000000000, 0.9510565162951535312, 1.000000000000000000, 0.9510565162951535312, 1.000000000000000000, 0.9510565162951535312, 1.000000000000000000, 0.9510565162951535312, 1.000000000000000000, 0.9510565162951535312, 1.000000000000000000, 0.9510565162951535312, 1.000000000000000000, 0.9510565162951535312, 1.000000000000000000, 0.9510565162951535312, 1.000000000000000000) ) ) 
 REPRESENTATION_ITEM ( '' )  SURFACE ( )  );
#27371 = CARTESIAN_POINT ( 'NONE',  ( 9.058813317711338797, 159.8449999999999989, -2.943386871421372675 ) ) ;
#27372 =( NAMED_UNIT ( * ) PLANE_ANGLE_UNIT ( ) SI_UNIT ( $, .RADIAN. ) );
#27373 = VERTEX_POINT ( 'NONE', #48603 ) ;
#27374 = ADVANCED_FACE ( 'NONE', ( #28100 ), #59427, .F. ) ;
#27375 = VERTEX_POINT ( 'NONE', #33747 ) ;
#27376 = DIRECTION ( 'NONE',  ( -1.000000000000000000, -0.000000000000000000, -0.000000000000000000 ) ) ;
#27377 =( NAMED_UNIT ( * ) SI_UNIT ( $, .STERADIAN. ) SOLID_ANGLE_UNIT ( ) );
#27378 = DIRECTION ( 'NONE',  ( -0.000000000000000000, -0.000000000000000000, 1.000000000000000000 ) ) ;
#27379 = CARTESIAN_POINT ( 'NONE',  ( 5.185928986913072691, 2.291132984336067935, 5.017707510222361833 ) ) ;
#27380 = VECTOR ( 'NONE', #9908, 1000.000000000000000 ) ;
#27381 = EDGE_LOOP ( 'NONE', ( #27925, #47791, #2087, #24346 ) ) ;
#27382 = CARTESIAN_POINT ( 'NONE',  ( 0.000000000000000000, 134.9429263765338192, -8.025000000000000355 ) ) ;
#27383 = FILL_AREA_STYLE ('',( #22834 ) ) ;
#27384 = SURFACE_STYLE_USAGE ( .BOTH. , #64708 ) ;
#27385 = SURFACE_SIDE_STYLE ('',( #5941 ) ) ;
#27386 = ORIENTED_EDGE ( 'NONE', *, *, #50176, .F. ) ;
#27387 = CARTESIAN_POINT ( 'NONE',  ( -25.00000000000000355, 36.75000000000000000, -3.750000000000000000 ) ) ;
#27388 = EDGE_CURVE ( 'NONE', #66384, #13277, #66572, .T. ) ;
#27389 = ORIENTED_EDGE ( 'NONE', *, *, #7555, .F. ) ;
#27390 = CARTESIAN_POINT ( 'NONE',  ( -53.54292637653379217, 9.058813317711329915, 2.943386871421369566 ) ) ;
#27391 = CARTESIAN_POINT ( 'NONE',  ( -34.99999999999999289, 99.99999999999998579, -9.500000000000000000 ) ) ;
#27392 = CYLINDRICAL_SURFACE ( 'NONE', #64412, 9.524999999999991473 ) ;
#27393 = CARTESIAN_POINT ( 'NONE',  ( -72.49999999999998579, 64.07124727947029896, -9.500000000000000000 ) ) ;
#27394 = AXIS2_PLACEMENT_3D ( 'NONE', #67910, #19702, #68595 ) ;
#27395 = CARTESIAN_POINT ( 'NONE',  ( -143.1549999999999727, 7.632228543268600340, 2.479861379858949277 ) ) ;
#27396 = DIRECTION ( 'NONE',  ( 0.000000000000000000, 0.000000000000000000, -1.000000000000000000 ) ) ;
#27397 = FILL_AREA_STYLE ('',( #16894 ) ) ;
#27398 = MECHANICAL_DESIGN_GEOMETRIC_PRESENTATION_REPRESENTATION (  '', ( #43193 ), #39810 ) ;
#27399 = VECTOR ( 'NONE', #35649, 1000.000000000000000 ) ;
#27400 = SPHERICAL_SURFACE ( 'NONE', #67713, 1.000000000000000000 ) ;
#27401 = EDGE_CURVE ( 'NONE', #618, #48114, #42193, .T. ) ;
#27402 = DIRECTION ( 'NONE',  ( -0.000000000000000000, -0.000000000000000000, 1.000000000000000000 ) ) ;
#27403 = DIRECTION ( 'NONE',  ( 0.7833176619561811327, 0.6216216216216277068, -4.313366480807242114E-15 ) ) ;
#27404 = ORIENTED_EDGE ( 'NONE', *, *, #40958, .F. ) ;
#27405 = ORIENTED_EDGE ( 'NONE', *, *, #14888, .F. ) ;
#27406 = CARTESIAN_POINT ( 'NONE',  ( -74.99999999999998579, 64.49137674618943095, 10.00000000000000000 ) ) ;
#27407 = CYLINDRICAL_SURFACE ( 'NONE', #41314, 1.000000000000000000 ) ;
#27408 = CARTESIAN_POINT ( 'NONE',  ( -61.40499999999999403, -2.607480562269069768, 8.024999999999991473 ) ) ;
#27409 = ORIENTED_EDGE ( 'NONE', *, *, #31369, .T. ) ;
#27410 = DIRECTION ( 'NONE',  ( 0.000000000000000000, 1.000000000000000000, 0.000000000000000000 ) ) ;
#27411 = LINE ( 'NONE', #33070, #39695 ) ;
#27412 = AXIS2_PLACEMENT_3D ( 'NONE', #1886, #23395, #13534 ) ;
#27413 = AXIS2_PLACEMENT_3D ( 'NONE', #51270, #50237, #18215 ) ;
#27414 = FACE_OUTER_BOUND ( 'NONE', #16963, .T. ) ;
#27415 = CARTESIAN_POINT ( 'NONE',  ( -97.34292637653379643, -9.058813317711329915, 2.943386871421371787 ) ) ;
#27416 = ORIENTED_EDGE ( 'NONE', *, *, #50529, .T. ) ;
#27417 = DIRECTION ( 'NONE',  ( -1.000000000000000000, 0.000000000000000000, -1.982541115402069054E-16 ) ) ;
#27418 = DIRECTION ( 'NONE',  ( 0.000000000000000000, 1.000000000000000000, 0.000000000000000000 ) ) ;
#27419 = CARTESIAN_POINT ( 'NONE',  ( -195.0000000000000000, 0.000000000000000000, 0.000000000000000000 ) ) ;
#27420 = AXIS2_PLACEMENT_3D ( 'NONE', #20012, #62924, #14770 ) ;
#27421 = CARTESIAN_POINT ( 'NONE',  ( -106.7949999999999733, 2.607480562269069324, -8.024999999999993250 ) ) ;
#27422 = CARTESIAN_POINT ( 'NONE',  ( 5.598654528085805993, 159.2450000000000045, 7.705886871421374629 ) ) ;
#27423 = CARTESIAN_POINT ( 'NONE',  ( -83.09499999999999886, -2.607480562269071545, -8.024999999999991473 ) ) ;
#27424 = CARTESIAN_POINT ( 'NONE',  ( 30.99999999999999289, 5.000000000000000000, 24.00402776293822171 ) ) ;
#27425 = CARTESIAN_POINT ( 'NONE',  ( 0.000000000000000000, 112.0570736234661666, -8.025000000000000355 ) ) ;
#27426 = VECTOR ( 'NONE', #43697, 1000.000000000000000 ) ;
#27427 = DIRECTION ( 'NONE',  ( 1.000000000000000000, 0.000000000000000000, 0.000000000000000000 ) ) ;
#27428 = COLOUR_RGB ( '', 0.66274510, 0.83137255, 0.94901961) ;
#27429 = ADVANCED_FACE ( 'NONE', ( #61500 ), #19142, .T. ) ;
#27430 = CYLINDRICAL_SURFACE ( 'NONE', #57299, 0.2500000000000002220 ) ;
#27431 = ORIENTED_EDGE ( 'NONE', *, *, #766, .F. ) ;
#27432 = CARTESIAN_POINT ( 'NONE',  ( -121.7929263765337993, -3.094860106618429807, 9.524999999999991473 ) ) ;
#27433 =( LENGTH_UNIT ( ) NAMED_UNIT ( * ) SI_UNIT ( .MILLI., .METRE. ) );
#27434 = CARTESIAN_POINT ( 'NONE',  ( -143.3949999999999818, -6.826472737025115478, -4.959722759717899443 ) ) ;
#27435 = CYLINDRICAL_SURFACE ( 'NONE', #61682, 0.5000000000000004441 ) ;
#27436 = VECTOR ( 'NONE', #18968, 1000.000000000000000 ) ;
#27437 = DIRECTION ( 'NONE',  ( -0.000000000000000000, 0.9984713486292863260, 0.05527174654752588928 ) ) ;
#27438 = CARTESIAN_POINT ( 'NONE',  ( -195.0000000000000000, 1.166476076187852838E-15, -9.524999999999991473 ) ) ;
#27439 = VERTEX_POINT ( 'NONE', #12992 ) ;
#27440 = ORIENTED_EDGE ( 'NONE', *, *, #37876, .F. ) ;
#27441 = FACE_OUTER_BOUND ( 'NONE', #37835, .T. ) ;
#27442 = DIRECTION ( 'NONE',  ( -0.000000000000000000, 0.000000000000000000, -1.000000000000000000 ) ) ;
#27443 = CIRCLE ( 'NONE', #48856, 7.749999999999993783 ) ;
#27444 = PRODUCT_DEFINITION ( 'UNKNOWN', '', #32630, #53662 ) ;
#27445 = EDGE_CURVE ( 'NONE', #13795, #49593, #64587, .T. ) ;
#27446 = CARTESIAN_POINT ( 'NONE',  ( -58.94292637653381206, 0.000000000000000000, 9.524999999999991473 ) ) ;
#27447 = LINE ( 'NONE', #11982, #66781 ) ;
#27448 = FILL_AREA_STYLE ('',( #54198 ) ) ;
#27449 = ORIENTED_EDGE ( 'NONE', *, *, #5453, .T. ) ;
#27450 = CARTESIAN_POINT ( 'NONE',  ( -144.5049999999999670, -6.826472737025113702, -4.959722759717900331 ) ) ;
#27452 = EDGE_CURVE ( 'NONE', #3488, #63248, #56600, .T. ) ;
#27451 = ORIENTED_EDGE ( 'NONE', *, *, #19785, .F. ) ;
#27453 = PRESENTATION_LAYER_ASSIGNMENT (  '', '', ( #45458 ) ) ;
#27454 = EDGE_CURVE ( 'NONE', #40506, #3912, #14016, .T. ) ;
#27455 = VERTEX_POINT ( 'NONE', #29863 ) ;
#27456 = DIRECTION ( 'NONE',  ( -0.000000000000000000, -0.000000000000000000, -1.000000000000000000 ) ) ;
#27457 = FACE_OUTER_BOUND ( 'NONE', #60179, .T. ) ;
#27458 = ORIENTED_EDGE ( 'NONE', *, *, #47327, .T. ) ;
#27459 = AXIS2_PLACEMENT_3D ( 'NONE', #51360, #57320, #29901 ) ;
#27460 = MECHANICAL_DESIGN_GEOMETRIC_PRESENTATION_REPRESENTATION (  '', ( #65639 ), #36520 ) ;
#27461 = CARTESIAN_POINT ( 'NONE',  ( -1.502314598737159031E-15, 2.500000000000000000, -9.000000000000000000 ) ) ;
#27462 = FACE_OUTER_BOUND ( 'NONE', #3626, .T. ) ;
#27463 = CARTESIAN_POINT ( 'NONE',  ( 8.102448949553181734, 135.3950000000000102, 5.886773742842750679 ) ) ;
#27464 = VERTEX_POINT ( 'NONE', #40444 ) ;
#27465 = CARTESIAN_POINT ( 'NONE',  ( 34.99999999999999289, 99.99999999999998579, 9.500000000000000000 ) ) ;
#27467 = EDGE_CURVE ( 'NONE', #27560, #22750, #11105, .T. ) ;
#27466 = CARTESIAN_POINT ( 'NONE',  ( 8.102448949553181734, 131.1049999999999898, -5.886773742842746238 ) ) ;
#27468 = CARTESIAN_POINT ( 'NONE',  ( -58.70499999999996987, 2.607480562269072433, 8.024999999999991473 ) ) ;
#27469 = CARTESIAN_POINT ( 'NONE',  ( -116.0949999999999704, -2.607480562269071545, -8.024999999999991473 ) ) ;
#27470 = CARTESIAN_POINT ( 'NONE',  ( -57.11974195712093660, -8.499999999999992895, 8.000000000000000000 ) ) ;
#27471 = ORIENTED_EDGE ( 'NONE', *, *, #63585, .T. ) ;
#27472 = CARTESIAN_POINT ( 'NONE',  ( -5.598654528085808657, 156.7549999999999670, 7.705886871421373741 ) ) ;
#27473 = VECTOR ( 'NONE', #13929, 1000.000000000000000 ) ;
#27474 =( NAMED_UNIT ( * ) PLANE_ANGLE_UNIT ( ) SI_UNIT ( $, .RADIAN. ) );
#27475 = EDGE_CURVE ( 'NONE', #46401, #37912, #60096, .T. ) ;
#27476 = DIRECTION ( 'NONE',  ( 0.000000000000000000, 0.000000000000000000, 1.000000000000000000 ) ) ;
#27477 = VECTOR ( 'NONE', #68777, 1000.000000000000000 ) ;
#27478 = CARTESIAN_POINT ( 'NONE',  ( -68.49999999999998579, -1.919947267060472329E-14, -9.999999999999998224 ) ) ;
#27479 = EDGE_CURVE ( 'NONE', #6631, #8903, #51135, .T. ) ;
#27480 = EDGE_LOOP ( 'NONE', ( #3451, #63662, #21771, #9849, #63753, #26535, #66178, #3408, #13273, #59006, #63033, #61042, #62667 ) ) ;
#27481 = CARTESIAN_POINT ( 'NONE',  ( 12.75000000000000533, 27.99999999999998224, 3.750000000000000000 ) ) ;
#27482 = CARTESIAN_POINT ( 'NONE',  ( -170.9049999999999727, 2.607480562269068880, -8.024999999999993250 ) ) ;
#27483 = ORIENTED_EDGE ( 'NONE', *, *, #2299, .T. ) ;
#27484 = CARTESIAN_POINT ( 'NONE',  ( -88.25707362346616947, 5.598654528085800663, -7.705886871421367523 ) ) ;
#27485 = AXIS2_PLACEMENT_3D ( 'NONE', #13812, #46570, #24687 ) ;
#27486 =( BOUNDED_SURFACE ( )  B_SPLINE_SURFACE ( 3, 2, ( 
 ( #42507, #69213, #26940 ),
 ( #21014, #47815, #58645 ),
 ( #26612, #36553, #21702 ),
 ( #52692, #25926, #48132 ),
 ( #68875, #37239, #64260 ),
 ( #9787, #4456, #43219 ),
 ( #69540, #36185, #57970 ),
 ( #21343, #47456, #10471 ),
 ( #176, #53384, #4108 ),
 ( #57611, #52358, #9434 ) ),
 .UNSPECIFIED., .F., .F., .F. ) 
 B_SPLINE_SURFACE_WITH_KNOTS ( ( 4, 2, 2, 2, 4 ),
 ( 3, 3 ),
 ( 0.0006185862396527136518, 0.001034390655347180218, 0.001450195071041647001, 0.001865999486736113783, 0.002281803902430580566 ),
 ( 0.000000000000000000, 1.000000000000000000 ),
 .UNSPECIFIED. ) 
 GEOMETRIC_REPRESENTATION_ITEM ( )  RATIONAL_B_SPLINE_SURFACE ( (
 ( 1.000000000000000000, 0.8505317485662434729, 1.000000000000000000),
 ( 1.000000000000000000, 0.8505807179912472371, 1.000000000000000000),
 ( 1.000000000000000000, 0.8467906168084839980, 1.000000000000000000),
 ( 1.000000000000000000, 0.8327126069847174961, 1.000000000000000000),
 ( 1.000000000000000000, 0.8223235278808177506, 1.000000000000000000),
 ( 1.000000000000000000, 0.7965633808504525293, 1.000000000000000000),
 ( 1.000000000000000000, 0.7811310880225481590, 1.000000000000000000),
 ( 1.000000000000000000, 0.7464785550193693275, 1.000000000000000000),
 ( 1.000000000000000000, 0.7273804381889640291, 1.000000000000000000),
 ( 1.000000000000000000, 0.7071067811865585639, 1.000000000000000000) ) ) 
 REPRESENTATION_ITEM ( '' )  SURFACE ( )  );
#27487 = CARTESIAN_POINT ( 'NONE',  ( 0.000000000000000000, 111.9999999999999858, 0.000000000000000000 ) ) ;
#27488 = STYLED_ITEM ( 'NONE', ( #27676 ), #31854 ) ;
#27489 = SURFACE_SIDE_STYLE ('',( #17994 ) ) ;
#27490 = ADVANCED_FACE ( 'NONE', ( #3792 ), #20708, .T. ) ;
#27491 = CYLINDRICAL_SURFACE ( 'NONE', #28193, 0.5000000000000004441 ) ;
#27492 = PLANE ( 'NONE',  #11878 ) ;
#27493 = EDGE_LOOP ( 'NONE', ( #1737, #65747, #11952, #17177 ) ) ;
#27494 = CARTESIAN_POINT ( 'NONE',  ( -45.91408774410873406, 9.428127415005508993, -3.509045371196664931 ) ) ;
#27495 =( NAMED_UNIT ( * ) PLANE_ANGLE_UNIT ( ) SI_UNIT ( $, .RADIAN. ) );
#27496 = CARTESIAN_POINT ( 'NONE',  ( -86.75499999999998124, 4.716976649647091513, -6.492361379858946790 ) ) ;
#27497 = ORIENTED_EDGE ( 'NONE', *, *, #66964, .F. ) ;
#27498 = DIRECTION ( 'NONE',  ( -0.2648642316819883047, 0.9642857142857141906, 0.000000000000000000 ) ) ;
#27499 = CARTESIAN_POINT ( 'NONE',  ( 13.50000000000000355, 28.24999999999998934, -3.750000000000000000 ) ) ;
#27500 = CARTESIAN_POINT ( 'NONE',  ( -69.05707362346618083, 0.000000000000000000, 9.524999999999991473 ) ) ;
#27501 = LINE ( 'NONE', #47664, #54991 ) ;
#27502 = ORIENTED_EDGE ( 'NONE', *, *, #64592, .T. ) ;
#27503 = LINE ( 'NONE', #58851, #13620 ) ;
#27504 = SURFACE_STYLE_FILL_AREA ( #32118 ) ;
#27505 = COLOUR_RGB ( '', 0.08235294, 0.09019608, 0.10196078) ;
#27506 = CARTESIAN_POINT ( 'NONE',  ( -101.1550000000000011, 7.632228543268600340, 2.479861379858949277 ) ) ;
#27507 = CARTESIAN_POINT ( 'NONE',  ( -3.094860106618434248, 125.7949999999999733, 9.525000000000000355 ) ) ;
#27508 = CARTESIAN_POINT ( 'NONE',  ( -121.0449999999999875, 7.632228543268600340, 2.479861379858949277 ) ) ;
#27509 = AXIS2_PLACEMENT_3D ( 'NONE', #28757, #22817, #54790 ) ;
#27510 = AXIS2_PLACEMENT_3D ( 'NONE', #26922, #64605, #32566 ) ;
#27511 = CARTESIAN_POINT ( 'NONE',  ( 32.00000000000001421, 15.00000000000000000, 35.49999999999999289 ) ) ;
#27513 = CARTESIAN_POINT ( 'NONE',  ( 71.99999999999998579, 64.07124727947029896, -9.500000000000000000 ) ) ;
#27512 = CARTESIAN_POINT ( 'NONE',  ( 45.07697505292422591, 10.02565835097472480, 3.091949714863343246 ) ) ;
#27514 = CARTESIAN_POINT ( 'NONE',  ( -151.4929263765338305, -8.102448949553172852, 5.886773742842742685 ) ) ;
#27515 = CARTESIAN_POINT ( 'NONE',  ( -174.1449999999999818, -4.716976649647092401, 6.492361379858946790 ) ) ;
#27516 = AXIS2_PLACEMENT_3D ( 'NONE', #24347, #19426, #25057 ) ;
#27517 = FILL_AREA_STYLE ('',( #6084 ) ) ;
#27518 = AXIS2_PLACEMENT_3D ( 'NONE', #11317, #21528, #22225 ) ;
#27519 = CARTESIAN_POINT ( 'NONE',  ( -44.55113387769600308, -13.99226303593487408, 0.7733428766569989676 ) ) ;
#27520 = EDGE_LOOP ( 'NONE', ( #10643, #69656, #9758, #13894, #46883, #1950, #26992, #18585, #52457, #64930, #17540, #31242, #45606, #65725, #30782, #42044 ) ) ;
#27521 = CARTESIAN_POINT ( 'NONE',  ( -28.74999999999999645, -13.99999999999999822, 18.10000000000000497 ) ) ;
#27522 = DIRECTION ( 'NONE',  ( -1.000000000000000000, 0.000000000000000000, 0.000000000000000000 ) ) ;
#27523 = ORIENTED_EDGE ( 'NONE', *, *, #37709, .T. ) ;
#27524 = CARTESIAN_POINT ( 'NONE',  ( -73.04292637653379927, -9.058813317711329915, -2.943386871421370898 ) ) ;
#27525 = CONTEXT_DEPENDENT_SHAPE_REPRESENTATION ( #42009, #47495 ) ;
#27526 = STYLED_ITEM ( 'NONE', ( #6705 ), #56868 ) ;
#27527 = DIRECTION ( 'NONE',  ( 0.000000000000000000, 1.000000000000000000, 0.000000000000000000 ) ) ;
#27528 = DIRECTION ( 'NONE',  ( -0.000000000000000000, -0.000000000000000000, -1.000000000000000000 ) ) ;
#27529 = ADVANCED_FACE ( 'NONE', ( #9819 ), #30536, .T. ) ;
#27530 = CIRCLE ( 'NONE', #6259, 7.000000000000001776 ) ;
#27531 =( LENGTH_UNIT ( ) NAMED_UNIT ( * ) SI_UNIT ( .MILLI., .METRE. ) );
#27532 = DIRECTION ( 'NONE',  ( 0.7071067811865398012, 8.659560562354839181E-17, -0.7071067811865552333 ) ) ;
#27533 = ADVANCED_FACE ( 'NONE', ( #32281 ), #63941, .T. ) ;
#27534 = DIRECTION ( 'NONE',  ( 0.000000000000000000, 0.000000000000000000, 1.000000000000000000 ) ) ;
#27535 = ORIENTED_EDGE ( 'NONE', *, *, #42040, .F. ) ;
#27536 = CARTESIAN_POINT ( 'NONE',  ( -168.0550000000000068, -9.827790563157499189E-16, -8.024999999999991473 ) ) ;
#27537 = EDGE_CURVE ( 'NONE', #11058, #50024, #47822, .T. ) ;
#27538 = ORIENTED_EDGE ( 'NONE', *, *, #5693, .T. ) ;
#27539 = CARTESIAN_POINT ( 'NONE',  ( 10.99999999999999645, 11.99999999999999289, -4.000000000000000000 ) ) ;
#27540 = CARTESIAN_POINT ( 'NONE',  ( -126.3570736234661780, 5.598654528085804216, 7.705886871421366635 ) ) ;
#27541 = PRESENTATION_STYLE_ASSIGNMENT (( #27871 ) ) ;
#27542 = CARTESIAN_POINT ( 'NONE',  ( -4.716976649647097730, 148.3570736234661638, -6.492361379858953896 ) ) ;
#27543 = TOROIDAL_SURFACE ( 'NONE', #52309, 14.49999999999999822, 0.5000000000000000000 ) ;
#27544 = ORIENTED_EDGE ( 'NONE', *, *, #30980, .T. ) ;
#27545 = SURFACE_SIDE_STYLE ('',( #33535 ) ) ;
#27546 = CARTESIAN_POINT ( 'NONE',  ( -95.75499999999999545, 4.716976649647091513, -6.492361379858946790 ) ) ;
#27547 = FACE_OUTER_BOUND ( 'NONE', #34406, .T. ) ;
#27548 = ORIENTED_EDGE ( 'NONE', *, *, #13568, .F. ) ;
#27549 =( LENGTH_UNIT ( ) NAMED_UNIT ( * ) SI_UNIT ( .MILLI., .METRE. ) );
#27550 = ADVANCED_FACE ( 'NONE', ( #42900 ), #6176, .T. ) ;
#27551 = CARTESIAN_POINT ( 'NONE',  ( -168.5929263765339954, -3.094860106621758700, -9.524999999997572075 ) ) ;
#27552 = DIRECTION ( 'NONE',  ( -0.000000000000000000, -1.000000000000000000, -0.000000000000000000 ) ) ;
#27553 = PLANE ( 'NONE',  #29965 ) ;
#27554 = DIRECTION ( 'NONE',  ( 0.000000000000000000, 0.000000000000000000, -1.000000000000000000 ) ) ;
#27555 = VECTOR ( 'NONE', #68082, 1000.000000000000000 ) ;
#27556 = EDGE_LOOP ( 'NONE', ( #17405, #9310, #41733, #15319 ) ) ;
#27557 = CIRCLE ( 'NONE', #52318, 0.5000000000000004441 ) ;
#27558 = SURFACE_STYLE_FILL_AREA ( #6125 ) ;
#27559 = CARTESIAN_POINT ( 'NONE',  ( -61.04499999999998749, 7.632228543268600340, 2.479861379858949277 ) ) ;
#27560 = VERTEX_POINT ( 'NONE', #5526 ) ;
#27561 = FILL_AREA_STYLE_COLOUR ( '', #23809 ) ;
#27562 = CARTESIAN_POINT ( 'NONE',  ( 12.00000000000001776, 15.00000000000000000, 29.68999999999999417 ) ) ;
#27563 = CARTESIAN_POINT ( 'NONE',  ( -138.6570736234661751, 9.058813317711329915, 2.943386871421369566 ) ) ;
#27564 = ORIENTED_EDGE ( 'NONE', *, *, #41997, .T. ) ;
#27565 = DIRECTION ( 'NONE',  ( 0.000000000000000000, 0.000000000000000000, 1.000000000000000000 ) ) ;
#27566 = CYLINDRICAL_SURFACE ( 'NONE', #52824, 9.524999999999991473 ) ;
#27567 = ORIENTED_EDGE ( 'NONE', *, *, #13568, .T. ) ;
#27568 = PRESENTATION_LAYER_ASSIGNMENT (  '', '', ( #24220 ) ) ;
#27569 = DIRECTION ( 'NONE',  ( -0.000000000000000000, -0.000000000000000000, -1.000000000000000000 ) ) ;
#27570 = CARTESIAN_POINT ( 'NONE',  ( -119.0049999999999955, 6.826472737025116366, 4.959722759717898555 ) ) ;
#27571 = ORIENTED_EDGE ( 'NONE', *, *, #65186, .T. ) ;
#27572 = EDGE_CURVE ( 'NONE', #42065, #20640, #46657, .T. ) ;
#27573 = FILL_AREA_STYLE_COLOUR ( '', #24037 ) ;
#27574 =( GEOMETRIC_REPRESENTATION_CONTEXT ( 3 ) GLOBAL_UNCERTAINTY_ASSIGNED_CONTEXT ( ( #59439 ) ) GLOBAL_UNIT_ASSIGNED_CONTEXT ( ( #38360, #15504, #10208 ) ) REPRESENTATION_CONTEXT ( 'NONE', 'WORKASPACE' ) );
#27575 = CARTESIAN_POINT ( 'NONE',  ( -160.3429263765337964, -9.058813317711329915, 2.943386871421371787 ) ) ;
#27576 = PLANE ( 'NONE',  #426 ) ;
#27577 = CARTESIAN_POINT ( 'NONE',  ( -148.1070736234661354, 8.102448949553171076, -5.886773742842744461 ) ) ;
#27578 = ADVANCED_FACE ( 'NONE', ( #37965 ), #54081, .T. ) ;
#27579 = CARTESIAN_POINT ( 'NONE',  ( -3.094860106618434248, 128.7949999999999875, 9.525000000000000355 ) ) ;
#27580 = AXIS2_PLACEMENT_3D ( 'NONE', #2319, #4353, #63485 ) ;
#27581 = CARTESIAN_POINT ( 'NONE',  ( -98.15707362346617515, -9.058813317711329915, -2.943386871421370898 ) ) ;
#27582 = AXIS2_PLACEMENT_3D ( 'NONE', #7129, #28555, #23305 ) ;
#27583 = EDGE_LOOP ( 'NONE', ( #61969, #3920, #4037, #66219 ) ) ;
#27585 = FACE_BOUND ( 'NONE', #55621, .T. ) ;
#27584 = CARTESIAN_POINT ( 'NONE',  ( 22.00000000000000711, 50.00000000000000000, -46.00000000000000000 ) ) ;
#27586 = CARTESIAN_POINT ( 'NONE',  ( -6.826472737025120807, 130.5070736234661695, -4.959722759717907437 ) ) ;
#27587 = CARTESIAN_POINT ( 'NONE',  ( -129.2049999999999841, -2.607480562269071545, -8.024999999999991473 ) ) ;
#27588 = CARTESIAN_POINT ( 'NONE',  ( -165.1429263765338078, 5.598654528085800663, -7.705886871421367523 ) ) ;
#27589 = CARTESIAN_POINT ( 'NONE',  ( 28.00000000000000000, 34.36176364315827669, -80.00402776293830698 ) ) ;
#27590 = CARTESIAN_POINT ( 'NONE',  ( -140.9949999999999193, -6.826472737025115478, 4.959722759717900331 ) ) ;
#27591 = CARTESIAN_POINT ( 'NONE',  ( -125.6950000000000074, -8.437984349512086979, 5.166775262442717831E-16 ) ) ;
#27592 = VERTEX_POINT ( 'NONE', #69572 ) ;
#27593 = DIRECTION ( 'NONE',  ( 1.000000000000000000, 0.000000000000000000, 0.000000000000000000 ) ) ;
#27594 = STYLED_ITEM ( 'NONE', ( #69151 ), #8662 ) ;
#27595 = FILL_AREA_STYLE ('',( #49783 ) ) ;
#27596 = UNCERTAINTY_MEASURE_WITH_UNIT (LENGTH_MEASURE( 1.000000000000000082E-05 ), #6669, 'distance_accuracy_value', 'NONE');
#27597 = CARTESIAN_POINT ( 'NONE',  ( -48.05499999999998550, -9.827790563157499189E-16, -8.024999999999991473 ) ) ;
#27598 =( NAMED_UNIT ( * ) PLANE_ANGLE_UNIT ( ) SI_UNIT ( $, .RADIAN. ) );
#27599 = CARTESIAN_POINT ( 'NONE',  ( -61.49499999999998323, 6.826472737025113702, -4.959722759717902107 ) ) ;
#27600 = DIRECTION ( 'NONE',  ( 0.8946296187927070820, 0.000000000000000000, 0.4468085106382997385 ) ) ;
#27601 = CARTESIAN_POINT ( 'NONE',  ( -29.98030399291527459, 0.000000000000000000, -3.499999999999998668 ) ) ;
#27602 = SURFACE_STYLE_USAGE ( .BOTH. , #32540 ) ;
#27603 = EDGE_CURVE ( 'NONE', #10014, #41012, #54276, .T. ) ;
#27604 = AXIS2_PLACEMENT_3D ( 'NONE', #3211, #8560, #56375 ) ;
#27605 = AXIS2_PLACEMENT_3D ( 'NONE', #37325, #58380, #59070 ) ;
#27606 = DIRECTION ( 'NONE',  ( 0.8660254037844388186, 0.4999999999999998335, -0.000000000000000000 ) ) ;
#27607 = CARTESIAN_POINT ( 'NONE',  ( -101.5429263765338135, 9.058813317711329915, 2.943386871421369566 ) ) ;
#27608 = CARTESIAN_POINT ( 'NONE',  ( 32.00000000000004263, 115.6078173946807084, -15.00000000000001421 ) ) ;
#27609 = CARTESIAN_POINT ( 'NONE',  ( -162.2070736234664423, 3.094860106622869811, 9.524999999996769162 ) ) ;
#27610 = FACE_OUTER_BOUND ( 'NONE', #17096, .T. ) ;
#27611 = CARTESIAN_POINT ( 'NONE',  ( -100.1070736234661780, 8.102448949553172852, -5.886773742842744461 ) ) ;
#27612 = AXIS2_PLACEMENT_3D ( 'NONE', #53769, #52431, #63979 ) ;
#27613 = CARTESIAN_POINT ( 'NONE',  ( 15.00000000000000000, 8.000000000000000000, 3.500000000000003997 ) ) ;
#27614 = EDGE_CURVE ( 'NONE', #11014, #52425, #48861, .T. ) ;
#27615 = ORIENTED_EDGE ( 'NONE', *, *, #39881, .F. ) ;
#27616 = CARTESIAN_POINT ( 'NONE',  ( -8.437984349512095861, 138.6929263765337907, -5.166775262442723748E-16 ) ) ;
#27617 =( LENGTH_UNIT ( ) NAMED_UNIT ( * ) SI_UNIT ( .MILLI., .METRE. ) );
#27618 = CIRCLE ( 'NONE', #5135, 1.000000000000000888 ) ;
#27619 = ORIENTED_EDGE ( 'NONE', *, *, #24154, .T. ) ;
#27620 = DIRECTION ( 'NONE',  ( -1.000000000000000000, 0.000000000000000000, -0.000000000000000000 ) ) ;
#27622 = CARTESIAN_POINT ( 'NONE',  ( -2.607480562269075097, 122.4070736234661467, 8.025000000000000355 ) ) ;
#27621 =( GEOMETRIC_REPRESENTATION_CONTEXT ( 3 ) GLOBAL_UNCERTAINTY_ASSIGNED_CONTEXT ( ( #50992 ) ) GLOBAL_UNIT_ASSIGNED_CONTEXT ( ( #43295, #63983, #58720 ) ) REPRESENTATION_CONTEXT ( 'NONE', 'WORKASPACE' ) );
#27623 = FILL_AREA_STYLE ('',( #17472 ) ) ;
#27624 = B_SPLINE_CURVE_WITH_KNOTS ( 'NONE', 3,
 ( #16308, #57805, #15955, #9966, #69058, #9630, #31385, #32426 ),
 .UNSPECIFIED., .F., .F.,
 ( 4, 2, 2, 4 ),
 ( 0.008439684080927939078, 0.009486163742497470339, 0.01053264340406700160, 0.01262560272720606412 ),
 .UNSPECIFIED. ) ;
#27625 = CARTESIAN_POINT ( 'NONE',  ( -47.50000000000000000, 14.49137674618942562, -10.00000000000000000 ) ) ;
#27626 = ORIENTED_EDGE ( 'NONE', *, *, #22241, .F. ) ;
#27627 = VERTEX_POINT ( 'NONE', #69247 ) ;
#27628 =( LENGTH_UNIT ( ) NAMED_UNIT ( * ) SI_UNIT ( .MILLI., .METRE. ) );
#27629 = EDGE_CURVE ( 'NONE', #16451, #51449, #21043, .T. ) ;
#27630 = CARTESIAN_POINT ( 'NONE',  ( 10.50000000000002309, 8.000000000000000000, -4.000000000000000000 ) ) ;
#27631 = VERTEX_POINT ( 'NONE', #37271 ) ;
#27632 = PRESENTATION_STYLE_ASSIGNMENT (( #65287 ) ) ;
#27633 = DIRECTION ( 'NONE',  ( -8.391040747885011388E-17, 0.7641995406119433953, -0.6449798928094538919 ) ) ;
#27634 = CARTESIAN_POINT ( 'NONE',  ( -87.14499999999998181, -4.716976649647092401, 6.492361379858946790 ) ) ;
#27635 = EDGE_LOOP ( 'NONE', ( #61142, #6849, #46933, #46743 ) ) ;
#27636 = DIRECTION ( 'NONE',  ( -1.000000000000000000, 0.000000000000000000, 0.000000000000000000 ) ) ;
#27637 = DIRECTION ( 'NONE',  ( 1.000000000000000000, 0.000000000000000000, 0.000000000000000000 ) ) ;
#27638 = FACE_OUTER_BOUND ( 'NONE', #68, .T. ) ;
#27639 = ORIENTED_EDGE ( 'NONE', *, *, #41110, .F. ) ;
#27640 = CARTESIAN_POINT ( 'NONE',  ( 22.75000000000000711, 36.75000000000000000, 3.750000000000000000 ) ) ;
#27641 = FILL_AREA_STYLE_COLOUR ( '', #8969 ) ;
#27642 = STYLED_ITEM ( 'NONE', ( #17157 ), #64881 ) ;
#27643 = FACE_OUTER_BOUND ( 'NONE', #48303, .T. ) ;
#27644 = EDGE_LOOP ( 'NONE', ( #39107, #43232, #15743, #64704, #20057, #57960 ) ) ;
#27645 = AXIS2_PLACEMENT_3D ( 'NONE', #30854, #35462, #25915 ) ;
#27646 = CARTESIAN_POINT ( 'NONE',  ( 8.000000000000030198, 5.000000000000000000, -29.00402776293826079 ) ) ;
#27647 = ORIENTED_EDGE ( 'NONE', *, *, #9965, .F. ) ;
#27648 = CARTESIAN_POINT ( 'NONE',  ( -165.3570736234661922, 5.598654528085804216, 7.705886871421366635 ) ) ;
#27649 = AXIS2_PLACEMENT_3D ( 'NONE', #20487, #63404, #14181 ) ;
#27650 =( LENGTH_UNIT ( ) NAMED_UNIT ( * ) SI_UNIT ( .MILLI., .METRE. ) );
#27651 = PLANE ( 'NONE',  #63678 ) ;
#27652 = CARTESIAN_POINT ( 'NONE',  ( 22.99999999999995381, 5.000000000000000000, 32.00402776293825724 ) ) ;
#27653 = FILL_AREA_STYLE_COLOUR ( '', #30778 ) ;
#27654 = FILL_AREA_STYLE ('',( #10815 ) ) ;
#27655 = CARTESIAN_POINT ( 'NONE',  ( -6.780819373525727833, 153.3146089765552631, -4.862369566202410454 ) ) ;
#27656 = EDGE_LOOP ( 'NONE', ( #10300, #68497, #31623, #29808 ) ) ;
#27657 = DIRECTION ( 'NONE',  ( 0.000000000000000000, 0.000000000000000000, 1.000000000000000000 ) ) ;
#27658 = DIRECTION ( 'NONE',  ( 0.000000000000000000, 0.000000000000000000, 1.000000000000000000 ) ) ;
#27659 =( NAMED_UNIT ( * ) PLANE_ANGLE_UNIT ( ) SI_UNIT ( $, .RADIAN. ) );
#27660 = DIRECTION ( 'NONE',  ( 1.000000000000000000, 0.000000000000000000, 0.000000000000000000 ) ) ;
#27661 = EDGE_LOOP ( 'NONE', ( #37074, #12564, #39805 ) ) ;
#27662 = CARTESIAN_POINT ( 'NONE',  ( 21.25000000000001066, 24.74999999999998224, 3.750000000000000000 ) ) ;
#27663 = CARTESIAN_POINT ( 'NONE',  ( -159.6550000000000011, -7.632228543268600340, -2.479861379858950166 ) ) ;
#27664 = CARTESIAN_POINT ( 'NONE',  ( 21.50000000000001066, 24.74999999999998224, -3.750000000000000000 ) ) ;
#27665 = DIRECTION ( 'NONE',  ( 0.000000000000000000, 0.000000000000000000, 1.000000000000000000 ) ) ;
#27666 = CARTESIAN_POINT ( 'NONE',  ( -170.3950000000000102, -6.826472737025115478, -4.959722759717899443 ) ) ;
#27667 = CARTESIAN_POINT ( 'NONE',  ( -165.1449999999999818, -4.716976649647092401, 6.492361379858946790 ) ) ;
#27668 = ORIENTED_EDGE ( 'NONE', *, *, #53344, .F. ) ;
#27669 = CARTESIAN_POINT ( 'NONE',  ( -90.44292637653379074, -1.166476076187852838E-15, -9.524999999999991473 ) ) ;
#27670 = FACE_OUTER_BOUND ( 'NONE', #8798, .T. ) ;
#27671 = SURFACE_SIDE_STYLE ('',( #39327 ) ) ;
#27672 = CARTESIAN_POINT ( 'NONE',  ( -84.80499999999999261, -8.437984349512085203, 5.166775262442717831E-16 ) ) ;
#27673 = CARTESIAN_POINT ( 'NONE',  ( 24.35070397832969391, 24.94665475208109839, 27.33851719159103766 ) ) ;
#27674 = CARTESIAN_POINT ( 'NONE',  ( -84.59499999999997044, 2.607480562269072433, 8.024999999999991473 ) ) ;
#27675 = CARTESIAN_POINT ( 'NONE',  ( 10.01517768586949231, 136.8049999999999500, 1.839758294383810543E-15 ) ) ;
#27676 = PRESENTATION_STYLE_ASSIGNMENT (( #6251 ) ) ;
#27677 = ADVANCED_FACE ( 'NONE', ( #58671 ), #43298, .F. ) ;
#27678 = CARTESIAN_POINT ( 'NONE',  ( 52.75000000000000000, 24.74999999999998224, 3.750000000000000000 ) ) ;
#27679 = UNCERTAINTY_MEASURE_WITH_UNIT (LENGTH_MEASURE( 1.000000000000000082E-05 ), #458, 'distance_accuracy_value', 'NONE');
#27680 = ADVANCED_FACE ( 'NONE', ( #15265 ), #25256, .T. ) ;
#27681 = DIRECTION ( 'NONE',  ( -0.000000000000000000, -0.000000000000000000, -1.000000000000000000 ) ) ;
#27682 = EDGE_CURVE ( 'NONE', #40049, #61248, #21911, .T. ) ;
#27683 = VERTEX_POINT ( 'NONE', #14521 ) ;
#27684 = DIRECTION ( 'NONE',  ( 0.000000000000000000, 0.000000000000000000, -1.000000000000000000 ) ) ;
#27685 = DIRECTION ( 'NONE',  ( 0.000000000000000000, 0.000000000000000000, -1.000000000000000000 ) ) ;
#27686 = PRESENTATION_LAYER_ASSIGNMENT (  '', '', ( #50181 ) ) ;
#27687 = FILL_AREA_STYLE ('',( #10854 ) ) ;
#27688 = EDGE_CURVE ( 'NONE', #21029, #33110, #488, .T. ) ;
#27689 = EDGE_CURVE ( 'NONE', #58823, #31954, #20504, .T. ) ;
#27690 = DIRECTION ( 'NONE',  ( 1.000000000000000000, 0.000000000000000000, 0.000000000000000000 ) ) ;
#27691 = COLOUR_RGB ( '', 0.66274510, 0.83137255, 0.94901961) ;
#27692 =( NAMED_UNIT ( * ) PLANE_ANGLE_UNIT ( ) SI_UNIT ( $, .RADIAN. ) );
#27693 = EDGE_LOOP ( 'NONE', ( #63764, #12273, #59506, #18979 ) ) ;
#27694 = ORIENTED_EDGE ( 'NONE', *, *, #19298, .F. ) ;
#27695 = CARTESIAN_POINT ( 'NONE',  ( -9.827790563157511022E-16, 136.4429263765338192, 8.025000000000000355 ) ) ;
#27696 = ADVANCED_FACE ( 'NONE', ( #8575 ), #36385, .F. ) ;
#27697 = FILL_AREA_STYLE_COLOUR ( '', #3876 ) ;
#27698 = UNCERTAINTY_MEASURE_WITH_UNIT (LENGTH_MEASURE( 1.000000000000000082E-05 ), #36773, 'distance_accuracy_value', 'NONE');
#27699 = ADVANCED_FACE ( 'NONE', ( #15597 ), #3227, .T. ) ;
#27700 = FACE_OUTER_BOUND ( 'NONE', #15851, .T. ) ;
#27701 = SURFACE_STYLE_USAGE ( .BOTH. , #6269 ) ;
#27702 = PRESENTATION_STYLE_ASSIGNMENT (( #43285 ) ) ;
#27703 = VERTEX_POINT ( 'NONE', #37072 ) ;
#27704 = CARTESIAN_POINT ( 'NONE',  ( -107.9049999999999869, 2.607480562269069324, -8.024999999999993250 ) ) ;
#27705 = ORIENTED_EDGE ( 'NONE', *, *, #59422, .F. ) ;
#27706 = PRESENTATION_LAYER_ASSIGNMENT (  '', '', ( #58094 ) ) ;
#27707 = ORIENTED_EDGE ( 'NONE', *, *, #12199, .F. ) ;
#27708 = LINE ( 'NONE', #43615, #2021 ) ;
#27709 = CARTESIAN_POINT ( 'NONE',  ( 17.75000000000000711, 30.99999999999999289, -3.750000000000000000 ) ) ;
#27710 = ORIENTED_EDGE ( 'NONE', *, *, #33451, .F. ) ;
#27711 = CARTESIAN_POINT ( 'NONE',  ( 12.72792206135785698, 114.9999999999999574, -10.50000000000000000 ) ) ;
#27712 =( NAMED_UNIT ( * ) PLANE_ANGLE_UNIT ( ) SI_UNIT ( $, .RADIAN. ) );
#27713 =( NAMED_UNIT ( * ) SI_UNIT ( $, .STERADIAN. ) SOLID_ANGLE_UNIT ( ) );
#27714 = ORIENTED_EDGE ( 'NONE', *, *, #44257, .T. ) ;
#27715 = VERTEX_POINT ( 'NONE', #52195 ) ;
#27716 = CARTESIAN_POINT ( 'NONE',  ( -117.2070736234669965, 3.094860106632079777, 9.524999999990075850 ) ) ;
#27717 = CARTESIAN_POINT ( 'NONE',  ( 7.647808743684392674, 154.4999999999999432, 5.677732506910178500 ) ) ;
#27718 = DIRECTION ( 'NONE',  ( 0.000000000000000000, -0.000000000000000000, 1.000000000000000000 ) ) ;
#27719 = CARTESIAN_POINT ( 'NONE',  ( -180.7429263765338021, -5.598654528085803328, -7.705886871421366635 ) ) ;
#27720 = ORIENTED_EDGE ( 'NONE', *, *, #15043, .T. ) ;
#27721 = CARTESIAN_POINT ( 'NONE',  ( -6.826472737025120807, 135.9929263765337737, 4.959722759717906548 ) ) ;
#27722 = CARTESIAN_POINT ( 'NONE',  ( 22.99999999999999289, 5.000000000000000000, -37.00402776293825013 ) ) ;
#27723 =( NAMED_UNIT ( * ) PLANE_ANGLE_UNIT ( ) SI_UNIT ( $, .RADIAN. ) );
#27724 = DIRECTION ( 'NONE',  ( -0.000000000000000000, -0.000000000000000000, 1.000000000000000000 ) ) ;
#27725 = ORIENTED_EDGE ( 'NONE', *, *, #44284, .F. ) ;
#27726 = EDGE_LOOP ( 'NONE', ( #8925, #898, #25766, #62453 ) ) ;
#27727 = DIRECTION ( 'NONE',  ( 0.000000000000000000, 0.000000000000000000, 1.000000000000000000 ) ) ;
#27728 = DIRECTION ( 'NONE',  ( 0.000000000000000000, 0.000000000000000000, 1.000000000000000000 ) ) ;
#27729 = CARTESIAN_POINT ( 'NONE',  ( 15.98999599679679839, 147.4999999999999716, 9.500000000000000000 ) ) ;
#27730 = CARTESIAN_POINT ( 'NONE',  ( -165.0570736234661524, 0.000000000000000000, 9.524999999999991473 ) ) ;
#27731 = CARTESIAN_POINT ( 'NONE',  ( -143.6049999999999613, 6.826472737025113702, -4.959722759717902107 ) ) ;
#27732 = UNCERTAINTY_MEASURE_WITH_UNIT (LENGTH_MEASURE( 1.000000000000000082E-05 ), #31237, 'distance_accuracy_value', 'NONE');
#27733 = EDGE_LOOP ( 'NONE', ( #56841, #34987, #60095, #4178 ) ) ;
#27734 = CARTESIAN_POINT ( 'NONE',  ( -105.7429263765338021, -5.598654528085803328, -7.705886871421366635 ) ) ;
#27735 = FACE_OUTER_BOUND ( 'NONE', #34724, .T. ) ;
#27736 = CARTESIAN_POINT ( 'NONE',  ( 40.82744559481908908, 108.1269596360033205, 3.302666768370682515 ) ) ;
#27737 = ORIENTED_EDGE ( 'NONE', *, *, #9661, .F. ) ;
#27738 = ORIENTED_EDGE ( 'NONE', *, *, #63070, .T. ) ;
#27739 = DIRECTION ( 'NONE',  ( -7.080503983578803083E-17, 1.000000000000000000, 0.000000000000000000 ) ) ;
#27740 = AXIS2_PLACEMENT_3D ( 'NONE', #69643, #69318, #11247 ) ;
#27741 = DIRECTION ( 'NONE',  ( -0.000000000000000000, -1.000000000000000000, -0.000000000000000000 ) ) ;
#27742 = CARTESIAN_POINT ( 'NONE',  ( -53.00500000000000256, 6.826472737025116366, 4.959722759717898555 ) ) ;
#27743 = ORIENTED_EDGE ( 'NONE', *, *, #39509, .F. ) ;
#27744 = CARTESIAN_POINT ( 'NONE',  ( -15.00000000000000000, 10.90871211463571200, -5.000000000000000000 ) ) ;
#27745 = DIRECTION ( 'NONE',  ( 1.982541115402069054E-16, 0.000000000000000000, -1.000000000000000000 ) ) ;
#27747 = AXIS2_PLACEMENT_3D ( 'NONE', #6625, #17247, #65740 ) ;
#27746 = LINE ( 'NONE', #22509, #11605 ) ;
#27748 = SURFACE_SIDE_STYLE ('',( #6316 ) ) ;
#27749 = DIRECTION ( 'NONE',  ( -0.000000000000000000, 1.000000000000000000, -0.000000000000000000 ) ) ;
#27750 = FACE_OUTER_BOUND ( 'NONE', #28805, .T. ) ;
#27751 = VERTEX_POINT ( 'NONE', #20861 ) ;
#27752 = SURFACE_STYLE_USAGE ( .BOTH. , #1694 ) ;
#27753 = CARTESIAN_POINT ( 'NONE',  ( 74.99999999999998579, 50.00000000000000000, 7.000000000000000000 ) ) ;
#27755 = LINE ( 'NONE', #60148, #48905 ) ;
#27754 =( BOUNDED_CURVE ( )  B_SPLINE_CURVE ( 2, ( #36923, #69252, #43257, #48172, #52732, #10510, #42907, #64663, #25965, #47494, #68915 ),
 .UNSPECIFIED., .F., .F. ) 
 B_SPLINE_CURVE_WITH_KNOTS ( ( 3, 2, 2, 2, 2, 3 ),
 ( 0.09782608695651948127, 0.09999999999999770184, 0.1021739130434759224, 0.1043478260869541152, 0.1065217391304323358, 0.1086956521739105563 ),
 .UNSPECIFIED. ) 
 CURVE ( )  GEOMETRIC_REPRESENTATION_ITEM ( )  RATIONAL_B_SPLINE_CURVE ( ( 1.000000000000050848, 0.9510565162951025719, 1.000000000000000000, 0.9510565162951535312, 1.000000000000000000, 0.9510565162951535312, 1.000000000000000000, 0.9510565162951535312, 1.000000000000000000, 0.9510565162952094864, 0.9999999999999440448 ) ) 
 REPRESENTATION_ITEM ( '' )  );
#27756 = DIRECTION ( 'NONE',  ( -1.000000000000000000, 0.000000000000000000, 0.000000000000000000 ) ) ;
#27757 = VECTOR ( 'NONE', #19252, 1000.000000000000114 ) ;
#27758 = ADVANCED_FACE ( 'NONE', ( #36732 ), #31046, .T. ) ;
#27759 = CARTESIAN_POINT ( 'NONE',  ( -107.8449999999999989, -7.632228543268599452, 2.479861379858951054 ) ) ;
#27760 = CARTESIAN_POINT ( 'NONE',  ( -8.102448949553181734, 158.4950000000000045, 5.886773742842747126 ) ) ;
#27761 = CARTESIAN_POINT ( 'NONE',  ( -91.34499999999998465, 7.632228543268599452, -2.479861379858951942 ) ) ;
#27762 = ADVANCED_FACE ( 'NONE', ( #46235 ), #9627, .F. ) ;
#27763 = CARTESIAN_POINT ( 'NONE',  ( 12.25000000000000355, 30.74999999999998579, -3.750000000000000000 ) ) ;
#27764 = FACE_OUTER_BOUND ( 'NONE', #22819, .T. ) ;
#27765 = CARTESIAN_POINT ( 'NONE',  ( -5.185928986913076244, 2.291132984336064382, -5.017707510222360057 ) ) ;
#27766 = UNCERTAINTY_MEASURE_WITH_UNIT (LENGTH_MEASURE( 1.000000000000000082E-05 ), #24801, 'distance_accuracy_value', 'NONE');
#27767 = ADVANCED_FACE ( 'NONE', ( #62373 ), #28656, .T. ) ;
#27768 = FILL_AREA_STYLE ('',( #65786 ) ) ;
#27769 = ORIENTED_EDGE ( 'NONE', *, *, #32471, .T. ) ;
#27770 = CARTESIAN_POINT ( 'NONE',  ( -127.9429263765338192, 0.000000000000000000, 9.524999999999991473 ) ) ;
#27771 = CARTESIAN_POINT ( 'NONE',  ( -143.0949999999999704, -2.607480562269071545, -8.024999999999991473 ) ) ;
#27772 = ADVANCED_FACE ( 'NONE', ( #52879 ), #68350, .F. ) ;
#27773 = CARTESIAN_POINT ( 'NONE',  ( -66.20707362346615810, 3.094860106618433360, 9.524999999999991473 ) ) ;
#27774 = DIRECTION ( 'NONE',  ( -1.000000000000000000, -0.000000000000000000, -0.000000000000000000 ) ) ;
#27775 = VERTEX_POINT ( 'NONE', #44089 ) ;
#27776 = ORIENTED_EDGE ( 'NONE', *, *, #23613, .T. ) ;
#27777 =( BOUNDED_CURVE ( )  B_SPLINE_CURVE ( 2, ( #48898, #33366, #914, #34049, #60422, #12582, #39025, #6276, #55143, #22121, #5566 ),
 .UNSPECIFIED., .F., .F. ) 
 B_SPLINE_CURVE_WITH_KNOTS ( ( 3, 2, 2, 2, 2, 3 ),
 ( 0.9239130434782608647, 0.9260869565217391131, 0.9282608695652173614, 0.9304347826086956097, 0.9326086956521738580, 0.9347826086956522174 ),
 .UNSPECIFIED. ) 
 CURVE ( )  GEOMETRIC_REPRESENTATION_ITEM ( )  RATIONAL_B_SPLINE_CURVE ( ( 1.000000000000000000, 0.9510565162951535312, 1.000000000000000000, 0.9510565162951535312, 1.000000000000000000, 0.9510565162951535312, 1.000000000000000000, 0.9510565162951535312, 1.000000000000000000, 0.9510565162951535312, 1.000000000000000000 ) ) 
 REPRESENTATION_ITEM ( '' )  );
#27778 = DIRECTION ( 'NONE',  ( 1.000000000000000000, 0.000000000000000000, 0.000000000000000000 ) ) ;
#27779 = DIRECTION ( 'NONE',  ( -1.000000000000000000, 0.000000000000000000, 0.000000000000000000 ) ) ;
#27780 = EDGE_CURVE ( 'NONE', #52169, #46059, #10701, .T. ) ;
#27781 = DIRECTION ( 'NONE',  ( -1.000000000000000000, 0.000000000000000000, 0.000000000000000000 ) ) ;
#27782 = CARTESIAN_POINT ( 'NONE',  ( -131.0070736234661410, -8.102448949553174629, -5.886773742842741797 ) ) ;
#27783 = VECTOR ( 'NONE', #56556, 1000.000000000000000 ) ;
#27784 = DIRECTION ( 'NONE',  ( 0.000000000000000000, 0.000000000000000000, 1.000000000000000000 ) ) ;
#27785 = AXIS2_PLACEMENT_3D ( 'NONE', #38027, #58404, #10228 ) ;
#27786 = CARTESIAN_POINT ( 'NONE',  ( -45.00000000000000000, -2.024042244987997205E-14, -9.500000000000000000 ) ) ;
#27787 = ORIENTED_EDGE ( 'NONE', *, *, #33197, .F. ) ;
#27788 = CARTESIAN_POINT ( 'NONE',  ( -145.2549999999999955, -4.716976649647092401, 6.492361379858946790 ) ) ;
#27789 = ORIENTED_EDGE ( 'NONE', *, *, #33683, .T. ) ;
#27790 = ORIENTED_EDGE ( 'NONE', *, *, #39512, .F. ) ;
#27791 = DIRECTION ( 'NONE',  ( 0.000000000000000000, 0.000000000000000000, 1.000000000000000000 ) ) ;
#27792 = DIRECTION ( 'NONE',  ( -1.000000000000000000, -0.000000000000000000, -0.000000000000000000 ) ) ;
#27793 = ORIENTED_EDGE ( 'NONE', *, *, #34179, .T. ) ;
#27794 = CARTESIAN_POINT ( 'NONE',  ( -0.2278693232858696738, 2.499999999999995115, -9.000000000000007105 ) ) ;
#27795 = CARTESIAN_POINT ( 'NONE',  ( -8.102448949553181734, 131.4950000000000045, 5.886773742842747126 ) ) ;
#27796 = DIRECTION ( 'NONE',  ( 0.000000000000000000, 1.000000000000000000, -0.000000000000000000 ) ) ;
#27797 = ORIENTED_EDGE ( 'NONE', *, *, #60215, .T. ) ;
#27798 = CARTESIAN_POINT ( 'NONE',  ( 9.058813317711338797, 127.9549999999999841, -2.943386871421372675 ) ) ;
#27799 = CARTESIAN_POINT ( 'NONE',  ( -57.65499999999998693, -7.632228543268600340, -2.479861379858950166 ) ) ;
#27800 = CARTESIAN_POINT ( 'NONE',  ( -122.6949999999999790, -8.437984349512085203, 5.166775262442717831E-16 ) ) ;
#27801 = CARTESIAN_POINT ( 'NONE',  ( 31.00000000000001421, 15.00000000000000000, 36.49999999999999289 ) ) ;
#27802 = ORIENTED_EDGE ( 'NONE', *, *, #33751, .T. ) ;
#27803 = CARTESIAN_POINT ( 'NONE',  ( -5.598654528085806881, 158.8549999999999898, -7.705886871421374629 ) ) ;
#27804 = CARTESIAN_POINT ( 'NONE',  ( 3.999798566743343109, 50.36012635523414360, 7.189099757012595404 ) ) ;
#27805 = UNCERTAINTY_MEASURE_WITH_UNIT (LENGTH_MEASURE( 1.000000000000000082E-05 ), #222, 'distance_accuracy_value', 'NONE');
#27806 = VECTOR ( 'NONE', #53336, 1000.000000000000000 ) ;
#27807 = CARTESIAN_POINT ( 'NONE',  ( 57.00000000000000000, 16.00000000000000000, -60.00402776293825724 ) ) ;
#27808 = STYLED_ITEM ( 'NONE', ( #10728 ), #41578 ) ;
#27809 = DIRECTION ( 'NONE',  ( 1.000000000000000000, 0.000000000000000000, 0.000000000000000000 ) ) ;
#27810 = LINE ( 'NONE', #39824, #29800 ) ;
#27811 = CARTESIAN_POINT ( 'NONE',  ( -105.0570736234661666, 0.000000000000000000, 9.524999999999991473 ) ) ;
#27812 = ORIENTED_EDGE ( 'NONE', *, *, #66388, .T. ) ;
#27813 = CARTESIAN_POINT ( 'NONE',  ( -32.76090269711983893, -9.103122581850293216, -2.000000000000000000 ) ) ;
#27814 =( LENGTH_UNIT ( ) NAMED_UNIT ( * ) SI_UNIT ( .MILLI., .METRE. ) );
#27815 = CARTESIAN_POINT ( 'NONE',  ( -174.2050000000000125, -2.607480562269071545, -8.024999999999991473 ) ) ;
#27816 = VERTEX_POINT ( 'NONE', #38468 ) ;
#27817 = CARTESIAN_POINT ( 'NONE',  ( -87.05707362346618083, 0.000000000000000000, 9.524999999999991473 ) ) ;
#27818 = UNCERTAINTY_MEASURE_WITH_UNIT (LENGTH_MEASURE( 1.000000000000000082E-05 ), #43958, 'distance_accuracy_value', 'NONE');
#27819 = EDGE_CURVE ( 'NONE', #20640, #60418, #69392, .T. ) ;
#27820 =( NAMED_UNIT ( * ) SI_UNIT ( $, .STERADIAN. ) SOLID_ANGLE_UNIT ( ) );
#27821 = SURFACE_STYLE_USAGE ( .BOTH. , #44088 ) ;
#27822 = DIRECTION ( 'NONE',  ( -0.000000000000000000, -0.000000000000000000, -1.000000000000000000 ) ) ;
#27823 = CARTESIAN_POINT ( 'NONE',  ( -77.09292637653378222, 3.094860106618433360, 9.524999999999991473 ) ) ;
#27824 = ORIENTED_EDGE ( 'NONE', *, *, #26635, .F. ) ;
#27825 = DIRECTION ( 'NONE',  ( 0.000000000000000000, 0.000000000000000000, -1.000000000000000000 ) ) ;
#27826 = CARTESIAN_POINT ( 'NONE',  ( 22.25000000000000711, 33.74999999999999289, -4.000000000000000000 ) ) ;
#27827 = CARTESIAN_POINT ( 'NONE',  ( -83.00499999999995282, 6.826472737025116366, 4.959722759717898555 ) ) ;
#27828 = EDGE_LOOP ( 'NONE', ( #9801, #49381, #53334, #20110 ) ) ;
#27829 = DIRECTION ( 'NONE',  ( 0.000000000000000000, 1.000000000000000000, 0.000000000000000000 ) ) ;
#27830 = LINE ( 'NONE', #59515, #22967 ) ;
#27831 = CARTESIAN_POINT ( 'NONE',  ( -57.20707362346615099, 3.094860106618433360, 9.524999999999991473 ) ) ;
#27832 = CARTESIAN_POINT ( 'NONE',  ( -75.00000000000001421, 8.675277573170040668, -5.941086794572167484 ) ) ;
#27833 = ORIENTED_EDGE ( 'NONE', *, *, #58769, .F. ) ;
#27834 = PLANE ( 'NONE',  #46316 ) ;
#27835 = CIRCLE ( 'NONE', #4235, 5.000000000000004441 ) ;
#27837 = CARTESIAN_POINT ( 'NONE',  ( -16.75000000000000000, -4.000000000000000000, 19.00000000000000000 ) ) ;
#27836 =( NAMED_UNIT ( * ) PLANE_ANGLE_UNIT ( ) SI_UNIT ( $, .RADIAN. ) );
#27838 = ADVANCED_FACE ( 'NONE', ( #65488 ), #42700, .T. ) ;
#27839 = CARTESIAN_POINT ( 'NONE',  ( -104.3049999999999784, 8.437984349512085203, -1.550032578732815448E-15 ) ) ;
#27840 = EDGE_CURVE ( 'NONE', #22316, #53362, #44685, .T. ) ;
#27841 = CARTESIAN_POINT ( 'NONE',  ( 10.01517768586949231, 126.6949999999999932, 1.839758294383810543E-15 ) ) ;
#27842 = CARTESIAN_POINT ( 'NONE',  ( -117.5949999999999989, 2.607480562269073321, 8.024999999999991473 ) ) ;
#27843 = COLOUR_RGB ( '', 0.40784314, 0.44705882, 0.49803922) ;
#27844 = CYLINDRICAL_SURFACE ( 'NONE', #68474, 5.000000000000000000 ) ;
#27845 = CARTESIAN_POINT ( 'NONE',  ( -19.33136078104492483, 11.73593362212572622, -2.518815027830850539 ) ) ;
#27846 = ADVANCED_FACE ( 'NONE', ( #21541 ), #27491, .F. ) ;
#27847 = CARTESIAN_POINT ( 'NONE',  ( -149.0929263765338249, 3.094860106618433360, 9.524999999999991473 ) ) ;
#27848 = CARTESIAN_POINT ( 'NONE',  ( -177.7449999999999761, 4.716976649647094177, 6.492361379858945902 ) ) ;
#27849 = COLOUR_RGB ( '', 0.40784314, 0.44705882, 0.49803922) ;
#27850 = EDGE_CURVE ( 'NONE', #17478, #62302, #33842, .T. ) ;
#27851 = LINE ( 'NONE', #60248, #44528 ) ;
#27852 = EDGE_CURVE ( 'NONE', #31434, #19928, #39484, .T. ) ;
#27853 = DIRECTION ( 'NONE',  ( -0.000000000000000000, -1.000000000000000000, -0.000000000000000000 ) ) ;
#27854 = CARTESIAN_POINT ( 'NONE',  ( 22.75000000000000711, 37.00000000000000000, -3.750000000000000000 ) ) ;
#27855 = DIRECTION ( 'NONE',  ( 1.000000000000000000, -8.881784197001254296E-16, 0.000000000000000000 ) ) ;
#27856 = ORIENTED_EDGE ( 'NONE', *, *, #579, .F. ) ;
#27857 = CARTESIAN_POINT ( 'NONE',  ( -69.29292637653378506, 3.094860106618428031, -9.524999999999993250 ) ) ;
#27858 = DIRECTION ( 'NONE',  ( -0.000000000000000000, -0.000000000000000000, -1.000000000000000000 ) ) ;
#27859 = CYLINDRICAL_SURFACE ( 'NONE', #20390, 9.524999999999991473 ) ;
#27860 = EDGE_CURVE ( 'NONE', #41276, #53774, #37274, .T. ) ;
#27861 = CARTESIAN_POINT ( 'NONE',  ( 14.09999999999999609, 11.99999999999999289, -3.499999999999991118 ) ) ;
#27862 = CARTESIAN_POINT ( 'NONE',  ( 62.24999999999998579, 31.24999999999999289, -3.750000000000000000 ) ) ;
#27863 = CARTESIAN_POINT ( 'NONE',  ( -43.75000000000000000, 0.000000000000000000, -7.000000000000000000 ) ) ;
#27864 = ORIENTED_EDGE ( 'NONE', *, *, #28000, .T. ) ;
#27865 = CARTESIAN_POINT ( 'NONE',  ( -173.0049999999999670, 6.826472737025115478, 4.959722759717899443 ) ) ;
#27866 = ORIENTED_EDGE ( 'NONE', *, *, #20890, .T. ) ;
#27867 =( NAMED_UNIT ( * ) PLANE_ANGLE_UNIT ( ) SI_UNIT ( $, .RADIAN. ) );
#27868 = FILL_AREA_STYLE_COLOUR ( '', #68039 ) ;
#27869 = DIRECTION ( 'NONE',  ( 1.000000000000000000, 0.000000000000000000, 0.000000000000000000 ) ) ;
#27870 = COLOUR_RGB ( '', 0.66274510, 0.83137255, 0.94901961) ;
#27871 = SURFACE_STYLE_USAGE ( .BOTH. , #5392 ) ;
#27872 = CARTESIAN_POINT ( 'NONE',  ( 2.607480562269071989, 152.7070736234661297, 8.025000000000002132 ) ) ;
#27873 = VECTOR ( 'NONE', #37596, 1000.000000000000000 ) ;
#27874 =( BOUNDED_CURVE ( )  B_SPLINE_CURVE ( 2, ( #4118, #42514, #52013, #63916, #25258, #5172, #30874, #15767, #14350, #35818, #46778 ),
 .UNSPECIFIED., .F., .F. ) 
 B_SPLINE_CURVE_WITH_KNOTS ( ( 3, 2, 2, 2, 2, 3 ),
 ( 0.4239130434782507617, 0.4260869565217289545, 0.4282608695652072028, 0.4304347826086854512, 0.4326086956521636440, 0.4347826086956418368 ),
 .UNSPECIFIED. ) 
 CURVE ( )  GEOMETRIC_REPRESENTATION_ITEM ( )  RATIONAL_B_SPLINE_CURVE ( ( 1.000000000000227374, 0.9510565162949260465, 1.000000000000000000, 0.9510565162951535312, 1.000000000000000000, 0.9510565162951535312, 1.000000000000000000, 0.9510565162951535312, 1.000000000000000000, 0.9510565162953860119, 0.9999999999997675193 ) ) 
 REPRESENTATION_ITEM ( '' )  );
#27875 = ORIENTED_EDGE ( 'NONE', *, *, #32189, .T. ) ;
#27876 = CARTESIAN_POINT ( 'NONE',  ( 4.716976649647099507, 137.6429263765338078, -6.492361379858953008 ) ) ;
#27877 = CARTESIAN_POINT ( 'NONE',  ( -86.15499999999998693, 7.632228543268600340, 2.479861379858949277 ) ) ;
#27878 = UNCERTAINTY_MEASURE_WITH_UNIT (LENGTH_MEASURE( 1.000000000000000082E-05 ), #7861, 'distance_accuracy_value', 'NONE');
#27879 = CARTESIAN_POINT ( 'NONE',  ( 0.000000000000000000, 133.0570736234661524, -8.025000000000000355 ) ) ;
#27880 =( GEOMETRIC_REPRESENTATION_CONTEXT ( 3 ) GLOBAL_UNCERTAINTY_ASSIGNED_CONTEXT ( ( #10253 ) ) GLOBAL_UNIT_ASSIGNED_CONTEXT ( ( #65487, #37777, #32788 ) ) REPRESENTATION_CONTEXT ( 'NONE', 'WORKASPACE' ) );
#27881 = AXIS2_PLACEMENT_3D ( 'NONE', #45890, #67318, #56776 ) ;
#27882 = SURFACE_SIDE_STYLE ('',( #48378 ) ) ;
#27883 = FACE_OUTER_BOUND ( 'NONE', #60354, .T. ) ;
#27884 = LINE ( 'NONE', #37842, #11938 ) ;
#27885 = DIRECTION ( 'NONE',  ( 1.000000000000000000, 0.000000000000000000, 0.000000000000000000 ) ) ;
#27886 = PRESENTATION_STYLE_ASSIGNMENT (( #7168 ) ) ;
#27887 = ORIENTED_EDGE ( 'NONE', *, *, #56448, .F. ) ;
#27888 = CIRCLE ( 'NONE', #62704, 0.2500000000000002220 ) ;
#27889 = PRESENTATION_STYLE_ASSIGNMENT (( #60602 ) ) ;
#27890 = CARTESIAN_POINT ( 'NONE',  ( -59.69499999999997897, -8.437984349512085203, 5.166775262442717831E-16 ) ) ;
#27891 = EDGE_LOOP ( 'NONE', ( #36731, #15338, #43477 ) ) ;
#27892 = CARTESIAN_POINT ( 'NONE',  ( -195.0000000000000000, 0.000000000000000000, 0.000000000000000000 ) ) ;
#27893 = EDGE_CURVE ( 'NONE', #43138, #50411, #51056, .T. ) ;
#27894 = DIRECTION ( 'NONE',  ( 8.659560562354879857E-17, 0.7071067811865517916, -0.7071067811865431318 ) ) ;
#27895 = CARTESIAN_POINT ( 'NONE',  ( -45.90838419619620936, 9.403326511829279255, -6.097699930223750897 ) ) ;
#27896 = EDGE_LOOP ( 'NONE', ( #48532, #7672, #18843, #60961 ) ) ;
#27897 = DIRECTION ( 'NONE',  ( -0.000000000000000000, -1.000000000000000000, -0.000000000000000000 ) ) ;
#27898 = VERTEX_POINT ( 'NONE', #12023 ) ;
#27899 = CARTESIAN_POINT ( 'NONE',  ( -75.00000000000000000, 7.768687147774685720, 6.500000000000002665 ) ) ;
#27900 = CARTESIAN_POINT ( 'NONE',  ( -116.7549999999999812, 4.716976649647091513, -6.492361379858946790 ) ) ;
#27901 = VERTEX_POINT ( 'NONE', #50029 ) ;
#27902 = LINE ( 'NONE', #52697, #56387 ) ;
#27903 = FACE_OUTER_BOUND ( 'NONE', #43016, .T. ) ;
#27904 =( LENGTH_UNIT ( ) NAMED_UNIT ( * ) SI_UNIT ( .MILLI., .METRE. ) );
#27905 = FILL_AREA_STYLE_COLOUR ( '', #64787 ) ;
#27906 = CARTESIAN_POINT ( 'NONE',  ( -146.6070736234661922, -8.102448949553172852, 5.886773742842742685 ) ) ;
#27907 = CARTESIAN_POINT ( 'NONE',  ( -9.058813317711337021, 131.0449999999999875, -2.943386871421374895 ) ) ;
#27908 = CARTESIAN_POINT ( 'NONE',  ( -92.00707362346615525, -8.102448949553172852, -5.886773742842741797 ) ) ;
#27909 = EDGE_CURVE ( 'NONE', #25423, #52608, #60534, .T. ) ;
#27910 = TOROIDAL_SURFACE ( 'NONE', #44861, 1.000000000000000000, 0.5000000000000000000 ) ;
#27911 = DIRECTION ( 'NONE',  ( 1.000000000000000000, 0.000000000000000000, 0.000000000000000000 ) ) ;
#27912 = ORIENTED_EDGE ( 'NONE', *, *, #49254, .T. ) ;
#27913 =( NAMED_UNIT ( * ) SI_UNIT ( $, .STERADIAN. ) SOLID_ANGLE_UNIT ( ) );
#27914 =( NAMED_UNIT ( * ) PLANE_ANGLE_UNIT ( ) SI_UNIT ( $, .RADIAN. ) );
#27915 =( LENGTH_UNIT ( ) NAMED_UNIT ( * ) SI_UNIT ( .MILLI., .METRE. ) );
#27916 = ADVANCED_FACE ( 'NONE', ( #40171 ), #6735, .F. ) ;
#27917 = CARTESIAN_POINT ( 'NONE',  ( -133.7049999999999557, 2.607480562269073321, 8.024999999999991473 ) ) ;
#27918 = EDGE_CURVE ( 'NONE', #64235, #62518, #45472, .T. ) ;
#27919 = CARTESIAN_POINT ( 'NONE',  ( -145.9429263765337907, 0.000000000000000000, 9.524999999999991473 ) ) ;
#27920 =( NAMED_UNIT ( * ) SI_UNIT ( $, .STERADIAN. ) SOLID_ANGLE_UNIT ( ) );
#27921 = CARTESIAN_POINT ( 'NONE',  ( -142.1949999999999932, 8.437984349512085203, -1.550032578732815448E-15 ) ) ;
#27922 = CIRCLE ( 'NONE', #3192, 0.5000000000000004441 ) ;
#27923 = AXIS2_PLACEMENT_3D ( 'NONE', #15152, #37306, #36261 ) ;
#27924 = CARTESIAN_POINT ( 'NONE',  ( -125.2449999999999903, -4.716976649647093289, -6.492361379858945902 ) ) ;
#27925 = ORIENTED_EDGE ( 'NONE', *, *, #7543, .T. ) ;
#27926 = CARTESIAN_POINT ( 'NONE',  ( 26.25000000000001066, 18.99999999999997868, 3.750000000000000000 ) ) ;
#27927 = CIRCLE ( 'NONE', #13337, 0.5000000000000004441 ) ;
#27928 = CARTESIAN_POINT ( 'NONE',  ( 44.30330429060724384, 9.767768096869062333, -3.048789874180223070 ) ) ;
#27929 = FACE_OUTER_BOUND ( 'NONE', #43701, .T. ) ;
#27930 = EDGE_CURVE ( 'NONE', #63457, #15233, #61918, .T. ) ;
#27931 = CARTESIAN_POINT ( 'NONE',  ( -178.9429263765338192, 0.000000000000000000, 9.524999999999991473 ) ) ;
#27932 =( NAMED_UNIT ( * ) SI_UNIT ( $, .STERADIAN. ) SOLID_ANGLE_UNIT ( ) );
#27933 = CARTESIAN_POINT ( 'NONE',  ( -59.09499999999997044, -2.607480562269071545, -8.024999999999991473 ) ) ;
#27934 = EDGE_CURVE ( 'NONE', #42659, #67453, #23275, .T. ) ;
#27935 = FACE_OUTER_BOUND ( 'NONE', #67522, .T. ) ;
#27936 = PRESENTATION_STYLE_ASSIGNMENT (( #17781 ) ) ;
#27937 = DIRECTION ( 'NONE',  ( 0.8660254037844387076, -0.000000000000000000, 0.4999999999999998890 ) ) ;
#27938 = DIRECTION ( 'NONE',  ( 0.000000000000000000, 0.000000000000000000, 1.000000000000000000 ) ) ;
#27939 = SURFACE_STYLE_FILL_AREA ( #39258 ) ;
#27940 = CARTESIAN_POINT ( 'NONE',  ( -98.09292637653378222, 3.094860106618433360, 9.524999999999991473 ) ) ;
#27941 = APPLICATION_PROTOCOL_DEFINITION ( 'draft international standard', 'automotive_design', 1998, #21711 ) ;
#27942 = CARTESIAN_POINT ( 'NONE',  ( -52.82340657583479526, -10.67641508236616943, 2.169052831005622295 ) ) ;
#27943 = SPHERICAL_SURFACE ( 'NONE', #27043, 1.000000000000000000 ) ;
#27944 = DIRECTION ( 'NONE',  ( -0.000000000000000000, 1.000000000000000000, -0.000000000000000000 ) ) ;
#27945 = FACE_OUTER_BOUND ( 'NONE', #4433, .T. ) ;
#27946 = FILL_AREA_STYLE_COLOUR ( '', #48392 ) ;
#27947 = AXIS2_PLACEMENT_3D ( 'NONE', #21726, #64644, #549 ) ;
#27948 = EDGE_CURVE ( 'NONE', #5309, #29847, #62292, .T. ) ;
#27949 = ORIENTED_EDGE ( 'NONE', *, *, #10323, .F. ) ;
#27950 = DIRECTION ( 'NONE',  ( 0.000000000000000000, 0.000000000000000000, -1.000000000000000000 ) ) ;
#27951 = DIRECTION ( 'NONE',  ( 1.000000000000000000, 2.168404344971008868E-16, -0.000000000000000000 ) ) ;
#27952 = ORIENTED_EDGE ( 'NONE', *, *, #62802, .T. ) ;
#27953 = CARTESIAN_POINT ( 'NONE',  ( 72.00000000000000000, 14.49137674618942562, 10.00000000000000000 ) ) ;
#27954 = ADVANCED_FACE ( 'NONE', ( #9189 ), #57463, .T. ) ;
#27955 = CARTESIAN_POINT ( 'NONE',  ( -6.826472737025120807, 127.5070736234661695, -4.959722759717907437 ) ) ;
#27956 = CYLINDRICAL_SURFACE ( 'NONE', #19241, 0.5000000000000004441 ) ;
#27957 = CARTESIAN_POINT ( 'NONE',  ( 75.00000000000000000, 19.84496280275719471, -6.370902851337238992 ) ) ;
#27958 = B_SPLINE_CURVE_WITH_KNOTS ( 'NONE', 3,
 ( #9957, #9269, #63415, #4281, #51465, #8904, #63744, #62368, #26107, #3577, #14190, #3221, #31376, #9624, #36728, #24710, #57082, #42008, #47641, #25083, #51830, #19803, #68701, #41293, #62689, #14517, #31042, #30685, #52536, #25762, #25424, #46939, #20129, #41638, #63057, #36380, #69048, #47278, #20499, #15260, #16636, #53554, #701, #26781 ),
 .UNSPECIFIED., .F., .F.,
 ( 4, 2, 2, 2, 2, 2, 2, 2, 2, 2, 2, 2, 2, 2, 2, 2, 2, 2, 2, 2, 2, 4 ),
 ( 0.008690707667102838888, 0.01030713786529197443, 0.01192356806348110823, 0.01353999826167024204, 0.01515642845985937757, 0.01596464355895394621, 0.01677285865804851311, 0.01838928885623765386, 0.01919750395533222423, 0.02000571905442679460, 0.02162214925261593881, 0.02323857945080508303, 0.02404679454989964993, 0.02485500964899422377, 0.02647143984718336451, 0.02727965494627793142, 0.02808787004537250526, 0.02970430024356164600, 0.03051251534265621984, 0.03132073044175079368, 0.03293716063993993443, 0.03455359083812908211 ),
 .UNSPECIFIED. ) ;
#27959 = FILL_AREA_STYLE_COLOUR ( '', #34211 ) ;
#27960 = ORIENTED_EDGE ( 'NONE', *, *, #42468, .F. ) ;
#27962 = EDGE_LOOP ( 'NONE', ( #46157, #228, #53106, #17218, #48289 ) ) ;
#27961 = CIRCLE ( 'NONE', #54937, 1.000000000000000888 ) ;
#27963 = CARTESIAN_POINT ( 'NONE',  ( -116.3070736234661666, -10.01517768586948698, 6.132527647946031529E-16 ) ) ;
#27964 = ORIENTED_EDGE ( 'NONE', *, *, #5096, .F. ) ;
#27965 = FILL_AREA_STYLE ('',( #16784 ) ) ;
#27966 = DIRECTION ( 'NONE',  ( 0.000000000000000000, 0.000000000000000000, -1.000000000000000000 ) ) ;
#27967 = VECTOR ( 'NONE', #22696, 999.9999999999998863 ) ;
#27968 = AXIS2_PLACEMENT_3D ( 'NONE', #27640, #6532, #1215 ) ;
#27969 = CARTESIAN_POINT ( 'NONE',  ( 4.716976649647096842, 148.7429263765338021, 6.492361379858953896 ) ) ;
#27970 = CARTESIAN_POINT ( 'NONE',  ( -94.64499999999999602, 4.716976649647091513, -6.492361379858946790 ) ) ;
#27972 = ORIENTED_EDGE ( 'NONE', *, *, #44376, .T. ) ;
#27971 = CIRCLE ( 'NONE', #6649, 22.50000000000000000 ) ;
#27973 = AXIS2_PLACEMENT_3D ( 'NONE', #33900, #7525, #49759 ) ;
#27974 = AXIS2_PLACEMENT_3D ( 'NONE', #4337, #16005, #4716 ) ;
#27975 = CARTESIAN_POINT ( 'NONE',  ( -4.716976649647097730, 123.2429263765338163, -6.492361379858953896 ) ) ;
#27976 = DIRECTION ( 'NONE',  ( -1.000000000000000000, 0.000000000000000000, 0.000000000000000000 ) ) ;
#27977 = ORIENTED_EDGE ( 'NONE', *, *, #8371, .F. ) ;
#27978 = CARTESIAN_POINT ( 'NONE',  ( 10.39230484541327115, -4.119968255444916849E-15, 7.500000000000000000 ) ) ;
#27979 = SURFACE_STYLE_USAGE ( .BOTH. , #27290 ) ;
#27980 = CIRCLE ( 'NONE', #10059, 5.500000000000005329 ) ;
#27981 = PRESENTATION_STYLE_ASSIGNMENT (( #50182 ) ) ;
#27982 = ORIENTED_EDGE ( 'NONE', *, *, #38361, .T. ) ;
#27983 = ADVANCED_FACE ( 'NONE', ( #47562 ), #68272, .F. ) ;
#27984 = PRESENTATION_STYLE_ASSIGNMENT (( #49492 ) ) ;
#27985 = ORIENTED_EDGE ( 'NONE', *, *, #56285, .T. ) ;
#27986 = CARTESIAN_POINT ( 'NONE',  ( 27.00000000000001776, 14.00000000000000000, -34.49999999999999289 ) ) ;
#27987 = DIRECTION ( 'NONE',  ( -0.000000000000000000, 0.000000000000000000, 1.000000000000000000 ) ) ;
#27988 = DIRECTION ( 'NONE',  ( 1.000000000000000000, 0.000000000000000000, 0.000000000000000000 ) ) ;
#27989 = CARTESIAN_POINT ( 'NONE',  ( -178.5570736234661808, -1.166476076187852838E-15, -9.524999999999991473 ) ) ;
#27990 = CARTESIAN_POINT ( 'NONE',  ( -13.23915246117191025, 52.65078610323165265, -2.000000000000000000 ) ) ;
#27991 = MECHANICAL_DESIGN_GEOMETRIC_PRESENTATION_REPRESENTATION (  '', ( #56091 ), #61692 ) ;
#27992 = CARTESIAN_POINT ( 'NONE',  ( 16.75000000000000711, 27.74999999999998224, -4.000000000000000000 ) ) ;
#27993 = ADVANCED_FACE ( 'NONE', ( #15186 ), #6594, .T. ) ;
#27994 = CARTESIAN_POINT ( 'NONE',  ( -68.24292637653380211, 5.598654528085804216, 7.705886871421366635 ) ) ;
#27995 = CARTESIAN_POINT ( 'NONE',  ( -7.968833018235937260, 153.7102887258889723, 3.588351662842281353 ) ) ;
#27996 = EDGE_LOOP ( 'NONE', ( #63595, #16083, #26924, #26874 ) ) ;
#27997 = DIRECTION ( 'NONE',  ( -0.9704308468600219006, 0.2413793103448194921, -0.000000000000000000 ) ) ;
#27998 = CARTESIAN_POINT ( 'NONE',  ( 1.999798566743339334, 49.09558629977726696, -2.000000000000000000 ) ) ;
#27999 = VERTEX_POINT ( 'NONE', #57716 ) ;
#28000 = EDGE_CURVE ( 'NONE', #22460, #51117, #6883, .T. ) ;
#28001 = CARTESIAN_POINT ( 'NONE',  ( -162.9549999999999841, -7.632228543268599452, 2.479861379858951054 ) ) ;
#28002 = DIRECTION ( 'NONE',  ( 0.000000000000000000, 0.000000000000000000, 1.000000000000000000 ) ) ;
#28003 = SURFACE_STYLE_FILL_AREA ( #39319 ) ;
#28004 = CARTESIAN_POINT ( 'NONE',  ( -178.3449999999999989, 7.632228543268599452, -2.479861379858951942 ) ) ;
#28005 = CARTESIAN_POINT ( 'NONE',  ( -157.1949999999999932, 8.437984349512086979, -1.550032578732815448E-15 ) ) ;
#28006 = STYLED_ITEM ( 'NONE', ( #47018 ), #58937 ) ;
#28007 = EDGE_LOOP ( 'NONE', ( #3732, #36176, #35900, #39350 ) ) ;
#28008 = FACE_OUTER_BOUND ( 'NONE', #68275, .T. ) ;
#28009 =( LENGTH_UNIT ( ) NAMED_UNIT ( * ) SI_UNIT ( .MILLI., .METRE. ) );
#28010 = AXIS2_PLACEMENT_3D ( 'NONE', #20804, #38045, #5987 ) ;
#28011 = FACE_OUTER_BOUND ( 'NONE', #10706, .T. ) ;
#28012 = CARTESIAN_POINT ( 'NONE',  ( -71.45499999999998408, 7.632228543268599452, -2.479861379858951942 ) ) ;
#28013 = CARTESIAN_POINT ( 'NONE',  ( 0.4142135623730951455, 42.99999999999999289, 35.50000000000000000 ) ) ;
#28014 = FACE_OUTER_BOUND ( 'NONE', #20942, .T. ) ;
#28015 = AXIS2_PLACEMENT_3D ( 'NONE', #29321, #44862, #1146 ) ;
#28016 = EDGE_CURVE ( 'NONE', #33323, #18360, #11132, .T. ) ;
#28017 = CARTESIAN_POINT ( 'NONE',  ( -75.59499999999998465, 2.607480562269072433, 8.024999999999991473 ) ) ;
#28018 = CARTESIAN_POINT ( 'NONE',  ( 3.094860106618435136, 137.4050000000000296, -9.525000000000000355 ) ) ;
#28019 = LINE ( 'NONE', #6574, #3886 ) ;
#28020 = AXIS2_PLACEMENT_3D ( 'NONE', #24583, #13009, #2395 ) ;
#28021 = CARTESIAN_POINT ( 'NONE',  ( -176.6929263765337907, 10.01517768586948698, -1.839758294383808966E-15 ) ) ;
#28022 = AXIS2_PLACEMENT_3D ( 'NONE', #59458, #53519, #53185 ) ;
#28023 = PRESENTATION_STYLE_ASSIGNMENT (( #48872 ) ) ;
#28024 = SURFACE_STYLE_FILL_AREA ( #39339 ) ;
#28025 = VERTEX_POINT ( 'NONE', #30252 ) ;
#28026 = AXIS2_PLACEMENT_3D ( 'NONE', #43809, #65219, #37154 ) ;
#28027 = DIRECTION ( 'NONE',  ( 0.000000000000000000, 0.000000000000000000, 1.000000000000000000 ) ) ;
#28028 = PRESENTATION_LAYER_ASSIGNMENT (  '', '', ( #3311 ) ) ;
#28029 = DIRECTION ( 'NONE',  ( 1.156482317317870344E-15, -1.000000000000000000, 0.000000000000000000 ) ) ;
#28030 = CARTESIAN_POINT ( 'NONE',  ( -119.3929263765337936, 8.102448949553176405, 5.886773742842740909 ) ) ;
#28031 = CARTESIAN_POINT ( 'NONE',  ( 0.000000000000000000, 42.00000000000000000, 79.00402776293826435 ) ) ;
#28032 = ORIENTED_EDGE ( 'NONE', *, *, #67061, .T. ) ;
#28033 = CIRCLE ( 'NONE', #59495, 0.9999999999999991118 ) ;
#28034 = EDGE_LOOP ( 'NONE', ( #59089, #26172, #47612, #35823 ) ) ;
#28035 = CYLINDRICAL_SURFACE ( 'NONE', #23775, 0.2500000000000002220 ) ;
#28036 = FILL_AREA_STYLE_COLOUR ( '', #34887 ) ;
#28037 = STYLED_ITEM ( 'NONE', ( #48947 ), #69042 ) ;
#28038 = CARTESIAN_POINT ( 'NONE',  ( -91.94292637653380496, 0.000000000000000000, 9.524999999999991473 ) ) ;
#28039 = CARTESIAN_POINT ( 'NONE',  ( -69.05707362346618083, 0.000000000000000000, 9.524999999999991473 ) ) ;
#28040 = VERTEX_POINT ( 'NONE', #35914 ) ;
#28041 = CARTESIAN_POINT ( 'NONE',  ( -110.6049999999999756, 6.826472737025113702, -4.959722759717902107 ) ) ;
#28042 = EDGE_LOOP ( 'NONE', ( #28759, #6307, #22374, #40389 ) ) ;
#28043 = FILL_AREA_STYLE_COLOUR ( '', #47842 ) ;
#28044 = DIRECTION ( 'NONE',  ( 1.000000000000000000, 0.000000000000000000, 0.000000000000000000 ) ) ;
#28045 = ORIENTED_EDGE ( 'NONE', *, *, #436, .F. ) ;
#28046 = CARTESIAN_POINT ( 'NONE',  ( 44.99999999999977973, 149.4999999999999716, 9.500000000000000000 ) ) ;
#28047 = DIRECTION ( 'NONE',  ( 0.000000000000000000, 0.000000000000000000, 1.000000000000000000 ) ) ;
#28048 = EDGE_LOOP ( 'NONE', ( #4932, #9599, #49566, #37304 ) ) ;
#28049 = MECHANICAL_DESIGN_GEOMETRIC_PRESENTATION_REPRESENTATION (  '', ( #19083 ), #21350 ) ;
#28050 = CARTESIAN_POINT ( 'NONE',  ( 0.000000000000000000, 160.4449999999999932, -9.525000000000000355 ) ) ;
#28051 = DIRECTION ( 'NONE',  ( -0.000000000000000000, 0.000000000000000000, -1.000000000000000000 ) ) ;
#28052 = ORIENTED_EDGE ( 'NONE', *, *, #37863, .F. ) ;
#28053 = VERTEX_POINT ( 'NONE', #30964 ) ;
#28054 = CARTESIAN_POINT ( 'NONE',  ( -15.98999599679679839, 146.4999999999999716, 7.000000000000000000 ) ) ;
#28055 = ORIENTED_EDGE ( 'NONE', *, *, #21403, .T. ) ;
#28056 = CARTESIAN_POINT ( 'NONE',  ( 4.716976649647099507, 137.6429263765338078, -6.492361379858953008 ) ) ;
#28057 = DIRECTION ( 'NONE',  ( -1.000000000000000000, -0.000000000000000000, -0.000000000000000000 ) ) ;
#28058 = CYLINDRICAL_SURFACE ( 'NONE', #2875, 5.000000000000004441 ) ;
#28059 = DIRECTION ( 'NONE',  ( 0.000000000000000000, 0.000000000000000000, 1.000000000000000000 ) ) ;
#28060 = DIRECTION ( 'NONE',  ( -1.000000000000000000, 0.000000000000000000, -0.000000000000000000 ) ) ;
#28061 = ORIENTED_EDGE ( 'NONE', *, *, #27364, .T. ) ;
#28062 = EDGE_CURVE ( 'NONE', #2941, #23178, #4205, .T. ) ;
#28063 = STYLED_ITEM ( 'NONE', ( #66302 ), #21057 ) ;
#28064 = DIRECTION ( 'NONE',  ( 1.000000000000000000, 0.000000000000000000, 0.000000000000000000 ) ) ;
#28065 = ORIENTED_EDGE ( 'NONE', *, *, #28247, .F. ) ;
#28066 = CARTESIAN_POINT ( 'NONE',  ( -49.79292637653379217, -3.094860106618429807, 9.524999999999991473 ) ) ;
#28067 = CARTESIAN_POINT ( 'NONE',  ( -74.50000000000000000, 119.9999999999997726, 10.00000000000000000 ) ) ;
#28068 = FACE_OUTER_BOUND ( 'NONE', #61484, .T. ) ;
#28069 = FACE_OUTER_BOUND ( 'NONE', #18230, .T. ) ;
#28070 = CARTESIAN_POINT ( 'NONE',  ( -144.3549999999999898, -4.716976649647093289, -6.492361379858945902 ) ) ;
#28071 = DIRECTION ( 'NONE',  ( -1.000000000000000000, 1.156482317317866302E-16, 0.000000000000000000 ) ) ;
#28072 = CYLINDRICAL_SURFACE ( 'NONE', #29364, 0.5000000000000004441 ) ;
#28073 = VERTEX_POINT ( 'NONE', #25678 ) ;
#28074 = AXIS2_PLACEMENT_3D ( 'NONE', #35950, #56711, #57755 ) ;
#28075 = CARTESIAN_POINT ( 'NONE',  ( -2.376974287405969816E-15, 13.58578643762690419, 35.91421356237309226 ) ) ;
#28076 = CARTESIAN_POINT ( 'NONE',  ( -45.00000000000000711, 8.164352767049518178, -6.987111781054301751 ) ) ;
#28077 = ORIENTED_EDGE ( 'NONE', *, *, #50693, .F. ) ;
#28078 = VECTOR ( 'NONE', #65958, 1000.000000000000000 ) ;
#28079 = ORIENTED_EDGE ( 'NONE', *, *, #61684, .F. ) ;
#28080 = LINE ( 'NONE', #5604, #50822 ) ;
#28081 = CARTESIAN_POINT ( 'NONE',  ( 22.99999999999996092, 5.000000000000000000, -77.00402776293825013 ) ) ;
#28082 = CARTESIAN_POINT ( 'NONE',  ( -56.75499999999997414, 4.716976649647091513, -6.492361379858946790 ) ) ;
#28083 = VERTEX_POINT ( 'NONE', #63331 ) ;
#28084 = SURFACE_STYLE_FILL_AREA ( #1329 ) ;
#28085 = ADVANCED_FACE ( 'NONE', ( #42606 ), #22149, .T. ) ;
#28086 =( LENGTH_UNIT ( ) NAMED_UNIT ( * ) SI_UNIT ( .MILLI., .METRE. ) );
#28087 =( LENGTH_UNIT ( ) NAMED_UNIT ( * ) SI_UNIT ( .MILLI., .METRE. ) );
#28088 = EDGE_CURVE ( 'NONE', #42340, #58089, #4927, .T. ) ;
#28089 = COLOUR_RGB ( '', 0.31764706, 0.68627451, 0.89019608) ;
#28090 = STYLED_ITEM ( 'NONE', ( #13689 ), #15583 ) ;
#28091 = EDGE_CURVE ( 'NONE', #53965, #38934, #85, .T. ) ;
#28092 = DIRECTION ( 'NONE',  ( -1.000000000000000000, 0.000000000000000000, 0.000000000000000000 ) ) ;
#28093 = CARTESIAN_POINT ( 'NONE',  ( -147.0570736234661808, 0.000000000000000000, 9.524999999999991473 ) ) ;
#28094 = ORIENTED_EDGE ( 'NONE', *, *, #47236, .F. ) ;
#28095 = STYLED_ITEM ( 'NONE', ( #58103 ), #57167 ) ;
#28096 = EDGE_CURVE ( 'NONE', #64569, #16390, #31659, .T. ) ;
#28097 =( LENGTH_UNIT ( ) NAMED_UNIT ( * ) SI_UNIT ( .MILLI., .METRE. ) );
#28098 = DIRECTION ( 'NONE',  ( -1.000000000000000000, 0.000000000000000000, 0.000000000000000000 ) ) ;
#28099 = B_SPLINE_CURVE_WITH_KNOTS ( 'NONE', 3,
 ( #46936, #35644, #40945, #62365, #30682, #20496 ),
 .UNSPECIFIED., .F., .F.,
 ( 4, 2, 4 ),
 ( 0.004189585287972440175, 0.006269578072783811573, 0.008349570857595182971 ),
 .UNSPECIFIED. ) ;
#28100 = FACE_OUTER_BOUND ( 'NONE', #56225, .T. ) ;
#28101 = COLOUR_RGB ( '', 0.66274510, 0.83137255, 0.94901961) ;
#28102 = FACE_OUTER_BOUND ( 'NONE', #41212, .T. ) ;
#28103 = ADVANCED_FACE ( 'NONE', ( #27735 ), #26706, .T. ) ;
#28104 = CARTESIAN_POINT ( 'NONE',  ( -108.4449999999999790, 0.000000000000000000, 8.024999999999991473 ) ) ;
#28105 = CARTESIAN_POINT ( 'NONE',  ( -1.166476076187854022E-15, 158.9449999999999932, 9.525000000000000355 ) ) ;
#28106 = CARTESIAN_POINT ( 'NONE',  ( -75.14499999999999602, -4.716976649647092401, 6.492361379858946790 ) ) ;
#28107 = CARTESIAN_POINT ( 'NONE',  ( 52.99999999999999289, 27.74999999999998579, 3.750000000000000000 ) ) ;
#28108 =( NAMED_UNIT ( * ) PLANE_ANGLE_UNIT ( ) SI_UNIT ( $, .RADIAN. ) );
#28109 = CYLINDRICAL_SURFACE ( 'NONE', #23819, 0.2500000000000002220 ) ;
#28110 = CARTESIAN_POINT ( 'NONE',  ( 40.96656732556692049, 108.0254117342834377, -3.574171091744781759 ) ) ;
#28111 = ORIENTED_EDGE ( 'NONE', *, *, #35925, .T. ) ;
#28112 = CARTESIAN_POINT ( 'NONE',  ( -121.1929263765337907, -10.01517768586948698, 6.132527647946031529E-16 ) ) ;
#28113 = COLOUR_RGB ( '', 0.72549020, 0.75294118, 0.79215686) ;
#28114 = CARTESIAN_POINT ( 'NONE',  ( -136.4949999999999477, 6.826472737025113702, -4.959722759717902107 ) ) ;
#28116 = MANIFOLD_SOLID_BREP ( 'Cut-Sweep1', #28366 ) ;
#28115 = AXIS2_PLACEMENT_3D ( 'NONE', #8870, #51795, #63019 ) ;
#28117 = DIRECTION ( 'NONE',  ( 0.000000000000000000, 0.000000000000000000, 1.000000000000000000 ) ) ;
#28118 = FACE_OUTER_BOUND ( 'NONE', #23998, .T. ) ;
#28119 = ORIENTED_EDGE ( 'NONE', *, *, #30962, .F. ) ;
#28120 = ORIENTED_EDGE ( 'NONE', *, *, #18413, .T. ) ;
#28121 = TOROIDAL_SURFACE ( 'NONE', #18070, 2.000000000000000000, 1.000000000000000000 ) ;
#28122 = DIRECTION ( 'NONE',  ( 0.000000000000000000, 0.000000000000000000, -1.000000000000000000 ) ) ;
#28123 = DIRECTION ( 'NONE',  ( 1.000000000000000000, 0.000000000000000000, 0.000000000000000000 ) ) ;
#28124 = CARTESIAN_POINT ( 'NONE',  ( -45.50000000000000000, -2.024042244987997205E-14, 6.500000000000000000 ) ) ;
#28125 = CARTESIAN_POINT ( 'NONE',  ( -117.4429263765338050, -1.166476076187852838E-15, -9.524999999999991473 ) ) ;
#28126 = DIRECTION ( 'NONE',  ( 0.000000000000000000, 1.000000000000000000, 0.000000000000000000 ) ) ;
#28127 = VERTEX_POINT ( 'NONE', #23516 ) ;
#28128 = CARTESIAN_POINT ( 'NONE',  ( -144.3549999999999898, -4.716976649647093289, -6.492361379858945902 ) ) ;
#28129 = ORIENTED_EDGE ( 'NONE', *, *, #40438, .T. ) ;
#28130 = VERTEX_POINT ( 'NONE', #59408 ) ;
#28131 = CARTESIAN_POINT ( 'NONE',  ( 4.041451884327379673, -7.000000000000002665, 7.500000000000000000 ) ) ;
#28132 = CARTESIAN_POINT ( 'NONE',  ( 0.000000000000000000, 109.9999999999999858, 0.000000000000000000 ) ) ;
#28133 = ORIENTED_EDGE ( 'NONE', *, *, #34159, .F. ) ;
#28134 = STYLED_ITEM ( 'NONE', ( #40100 ), #17696 ) ;
#28135 = CARTESIAN_POINT ( 'NONE',  ( -15.98999599679679839, 118.4999999999999716, -9.500000000000000000 ) ) ;
#28136 = CARTESIAN_POINT ( 'NONE',  ( 0.000000000000000000, 127.4449999999999790, -9.525000000000000355 ) ) ;
#28137 = COLOUR_RGB ( '', 0.40784314, 0.44705882, 0.49803922) ;
#28138 = PRODUCT_DEFINITION_FORMATION_WITH_SPECIFIED_SOURCE ( 'ANY', '', #25974, .NOT_KNOWN. ) ;
#28139 = ORIENTED_EDGE ( 'NONE', *, *, #60466, .T. ) ;
#28140 = CARTESIAN_POINT ( 'NONE',  ( 5.598654528085809545, 128.2549999999999670, -7.705886871421373741 ) ) ;
#28141 = CARTESIAN_POINT ( 'NONE',  ( -50.15499999999997982, 7.632228543268600340, 2.479861379858949277 ) ) ;
#28142 =( NAMED_UNIT ( * ) SI_UNIT ( $, .STERADIAN. ) SOLID_ANGLE_UNIT ( ) );
#28143 = EDGE_LOOP ( 'NONE', ( #17490, #3396, #34460, #30792 ) ) ;
#28144 = CARTESIAN_POINT ( 'NONE',  ( -8.102448949553181734, 153.0050000000000239, -5.886773742842749790 ) ) ;
#28145 = DIRECTION ( 'NONE',  ( -0.000000000000000000, 1.000000000000000000, -0.000000000000000000 ) ) ;
#28146 = DIRECTION ( 'NONE',  ( 0.000000000000000000, 0.000000000000000000, -1.000000000000000000 ) ) ;
#28147 = ORIENTED_EDGE ( 'NONE', *, *, #49026, .F. ) ;
#28148 = EDGE_CURVE ( 'NONE', #6192, #3199, #13820, .T. ) ;
#28149 = FACE_OUTER_BOUND ( 'NONE', #27274, .T. ) ;
#28150 = ORIENTED_EDGE ( 'NONE', *, *, #50513, .T. ) ;
#28151 = CARTESIAN_POINT ( 'NONE',  ( -34.07444628652228857, -9.981032396169499776, -3.023059613375652876 ) ) ;
#28152 = FILL_AREA_STYLE ('',( #1410 ) ) ;
#28154 = CARTESIAN_POINT ( 'NONE',  ( -173.1550000000000011, 7.632228543268600340, 2.479861379858949277 ) ) ;
#28153 = AXIS2_PLACEMENT_3D ( 'NONE', #65692, #23462, #60400 ) ;
#28155 = ORIENTED_EDGE ( 'NONE', *, *, #42939, .F. ) ;
#28156 = FILL_AREA_STYLE_COLOUR ( '', #11545 ) ;
#28157 = EDGE_CURVE ( 'NONE', #17912, #65192, #11941, .T. ) ;
#28158 = AXIS2_PLACEMENT_3D ( 'NONE', #25908, #47432, #5472 ) ;
#28159 = STYLED_ITEM ( 'NONE', ( #21734 ), #12491 ) ;
#28160 = DIRECTION ( 'NONE',  ( 1.000000000000000000, 0.000000000000000000, 0.000000000000000000 ) ) ;
#28161 = FILL_AREA_STYLE ('',( #50705 ) ) ;
#28162 = FACE_OUTER_BOUND ( 'NONE', #44691, .T. ) ;
#28163 =( BOUNDED_CURVE ( )  B_SPLINE_CURVE ( 2, ( #59117, #49625, #58786, #38055, #32050, #10937, #5998, #54864, #43364, #27773, #48262 ),
 .UNSPECIFIED., .F., .F. ) 
 B_SPLINE_CURVE_WITH_KNOTS ( ( 3, 2, 2, 2, 2, 3 ),
 ( 0.8369565217391304879, 0.8391304347826087362, 0.8413043478260869845, 0.8434782608695652328, 0.8456521739130434812, 0.8478260869565217295 ),
 .UNSPECIFIED. ) 
 CURVE ( )  GEOMETRIC_REPRESENTATION_ITEM ( )  RATIONAL_B_SPLINE_CURVE ( ( 1.000000000000000000, 0.9510565162951535312, 1.000000000000000000, 0.9510565162951535312, 1.000000000000000000, 0.9510565162951535312, 1.000000000000000000, 0.9510565162951535312, 1.000000000000000000, 0.9510565162951535312, 1.000000000000000000 ) ) 
 REPRESENTATION_ITEM ( '' )  );
#28164 = ORIENTED_EDGE ( 'NONE', *, *, #24059, .T. ) ;
#28165 = EDGE_CURVE ( 'NONE', #23235, #36781, #26011, .T. ) ;
#28166 = ORIENTED_EDGE ( 'NONE', *, *, #64031, .F. ) ;
#28167 = DIRECTION ( 'NONE',  ( -1.000000000000000000, -0.000000000000000000, -0.000000000000000000 ) ) ;
#28168 = CARTESIAN_POINT ( 'NONE',  ( -90.20499999999999829, -2.607480562269071545, -8.024999999999991473 ) ) ;
#28169 = ORIENTED_EDGE ( 'NONE', *, *, #5159, .T. ) ;
#28170 = CARTESIAN_POINT ( 'NONE',  ( 57.00000000000000000, 16.00000000000000000, 60.00402776293825724 ) ) ;
#28171 = AXIS2_PLACEMENT_3D ( 'NONE', #13713, #35170, #56631 ) ;
#28172 = ADVANCED_FACE ( 'NONE', ( #49589 ), #6971, .F. ) ;
#28173 = COLOUR_RGB ( '', 0.08235294, 0.09019608, 0.10196078) ;
#28174 = CYLINDRICAL_SURFACE ( 'NONE', #40742, 4.999999999999997335 ) ;
#28175 = DIRECTION ( 'NONE',  ( 1.000000000000000000, 0.000000000000000000, 0.000000000000000000 ) ) ;
#28176 = AXIS2_PLACEMENT_3D ( 'NONE', #35955, #57402, #30647 ) ;
#28177 = EDGE_CURVE ( 'NONE', #16622, #41269, #25517, .T. ) ;
#28178 = CARTESIAN_POINT ( 'NONE',  ( -74.33437949985298587, 8.455502173247598563, -6.462386104487723770 ) ) ;
#28179 = VERTEX_POINT ( 'NONE', #1995 ) ;
#28180 = CARTESIAN_POINT ( 'NONE',  ( 2.755511676787084419, 7.000000000000007105, 0.5168645644872258416 ) ) ;
#28181 = MECHANICAL_DESIGN_GEOMETRIC_PRESENTATION_REPRESENTATION (  '', ( #55159 ), #49570 ) ;
#28182 = CARTESIAN_POINT ( 'NONE',  ( 8.000000000000000000, 5.000000000000000000, 72.00402776293825013 ) ) ;
#28183 = CARTESIAN_POINT ( 'NONE',  ( -10.01517768586949231, 125.1950000000000074, -6.132527647946036459E-16 ) ) ;
#28184 = CARTESIAN_POINT ( 'NONE',  ( -103.6449999999999818, 4.716976649647091513, -6.492361379858946790 ) ) ;
#28185 = SURFACE_STYLE_FILL_AREA ( #60240 ) ;
#28186 = AXIS2_PLACEMENT_3D ( 'NONE', #50482, #14234, #2210 ) ;
#28187 = CARTESIAN_POINT ( 'NONE',  ( 10.01517768586949231, 145.8050000000000068, 1.839758294383810543E-15 ) ) ;
#28189 = CARTESIAN_POINT ( 'NONE',  ( -20.00017592768050179, 12.00007330319154697, -0.3280245013256660735 ) ) ;
#28188 = CARTESIAN_POINT ( 'NONE',  ( 1.709458476932651091E-14, 14.00000000000000533, -35.50000000000000000 ) ) ;
#28190 = CARTESIAN_POINT ( 'NONE',  ( -154.7929263765337851, -3.094860106618429807, 9.524999999999991473 ) ) ;
#28191 =( GEOMETRIC_REPRESENTATION_CONTEXT ( 3 ) GLOBAL_UNCERTAINTY_ASSIGNED_CONTEXT ( ( #50905 ) ) GLOBAL_UNIT_ASSIGNED_CONTEXT ( ( #36036, #57476, #46268 ) ) REPRESENTATION_CONTEXT ( 'NONE', 'WORKASPACE' ) );
#28192 = CARTESIAN_POINT ( 'NONE',  ( -176.9950000000000045, -6.826472737025115478, 4.959722759717900331 ) ) ;
#28193 = AXIS2_PLACEMENT_3D ( 'NONE', #1764, #7099, #66534 ) ;
#28194 = DIRECTION ( 'NONE',  ( -1.000000000000000000, 0.000000000000000000, 0.000000000000000000 ) ) ;
#28195 = DIRECTION ( 'NONE',  ( 1.000000000000000000, 0.000000000000000000, 0.000000000000000000 ) ) ;
#28196 = EDGE_LOOP ( 'NONE', ( #27310, #35917, #29967, #54306 ) ) ;
#28197 = FILL_AREA_STYLE ('',( #43766 ) ) ;
#28198 = ORIENTED_EDGE ( 'NONE', *, *, #34252, .F. ) ;
#28199 = COLOUR_RGB ( '', 0.08235294, 0.09019608, 0.10196078) ;
#28200 = CARTESIAN_POINT ( 'NONE',  ( -68.84292637653379643, 9.058813317711329915, -2.943386871421373119 ) ) ;
#28201 = FACE_OUTER_BOUND ( 'NONE', #1420, .T. ) ;
#28202 = FILL_AREA_STYLE ('',( #27175 ) ) ;
#28203 = EDGE_CURVE ( 'NONE', #31124, #5580, #6634, .T. ) ;
#28204 = COLOUR_RGB ( '', 0.40784314, 0.44705882, 0.49803922) ;
#28205 = CARTESIAN_POINT ( 'NONE',  ( -174.0570736234661808, 0.000000000000000000, 9.524999999999991473 ) ) ;
#28206 =( NAMED_UNIT ( * ) SI_UNIT ( $, .STERADIAN. ) SOLID_ANGLE_UNIT ( ) );
#28207 = CARTESIAN_POINT ( 'NONE',  ( 44.37550316447022425, 9.999999999999982236, -3.428884149106774970 ) ) ;
#28209 = CIRCLE ( 'NONE', #14821, 3.100000000000001865 ) ;
#28208 = DIRECTION ( 'NONE',  ( 1.000000000000000000, 0.000000000000000000, -0.000000000000000000 ) ) ;
#28210 = ORIENTED_EDGE ( 'NONE', *, *, #10742, .F. ) ;
#28211 = CARTESIAN_POINT ( 'NONE',  ( -166.5550000000000068, 0.000000000000000000, 8.024999999999991473 ) ) ;
#28212 = VERTEX_POINT ( 'NONE', #54823 ) ;
#28213 = DIRECTION ( 'NONE',  ( -6.938893903907221278E-15, 0.000000000000000000, -1.000000000000000000 ) ) ;
#28214 =( NAMED_UNIT ( * ) SI_UNIT ( $, .STERADIAN. ) SOLID_ANGLE_UNIT ( ) );
#28215 = CIRCLE ( 'NONE', #6863, 9.500000000000005329 ) ;
#28216 = CYLINDRICAL_SURFACE ( 'NONE', #38799, 0.5000000000000004441 ) ;
#28217 = CARTESIAN_POINT ( 'NONE',  ( -8.437984349512095861, 154.8070736234661524, -5.166775262442723748E-16 ) ) ;
#28218 = CIRCLE ( 'NONE', #32725, 9.499999999999994671 ) ;
#28219 = ORIENTED_EDGE ( 'NONE', *, *, #50135, .T. ) ;
#28220 = DIRECTION ( 'NONE',  ( 0.000000000000000000, 1.000000000000000000, 0.000000000000000000 ) ) ;
#28221 = CARTESIAN_POINT ( 'NONE',  ( -79.55499999999999261, 0.000000000000000000, 8.024999999999991473 ) ) ;
#28222 = AXIS2_PLACEMENT_3D ( 'NONE', #1171, #60657, #28988 ) ;
#28223 = SURFACE_STYLE_FILL_AREA ( #1107 ) ;
#28224 = EDGE_CURVE ( 'NONE', #44696, #51304, #47992, .T. ) ;
#28225 = CARTESIAN_POINT ( 'NONE',  ( -72.20707362346617231, 3.094860106618433360, 9.524999999999991473 ) ) ;
#28226 = EDGE_CURVE ( 'NONE', #37986, #66051, #17001, .T. ) ;
#28227 = CARTESIAN_POINT ( 'NONE',  ( -113.9929263765338021, 8.102448949553172852, -5.886773742842744461 ) ) ;
#28228 = DIRECTION ( 'NONE',  ( -0.000000000000000000, -0.000000000000000000, -1.000000000000000000 ) ) ;
#28229 = AXIS2_PLACEMENT_3D ( 'NONE', #40175, #50362, #7456 ) ;
#28230 = EDGE_LOOP ( 'NONE', ( #10373, #56114, #54203, #11515 ) ) ;
#28231 = CARTESIAN_POINT ( 'NONE',  ( 36.00000000000002132, 5.000000000000000000, -77.00402776293825013 ) ) ;
#28232 = CARTESIAN_POINT ( 'NONE',  ( -58.19500000000000028, 8.437984349512085203, -1.550032578732815448E-15 ) ) ;
#28233 = ORIENTED_EDGE ( 'NONE', *, *, #7948, .F. ) ;
#28234 = ADVANCED_FACE ( 'NONE', ( #55173 ), #52014, .F. ) ;
#28235 = CIRCLE ( 'NONE', #60848, 1.000000000000000888 ) ;
#28236 = CARTESIAN_POINT ( 'NONE',  ( -45.00000000000000000, 9.708372641349546583, -6.050536800209449062 ) ) ;
#28237 = ORIENTED_EDGE ( 'NONE', *, *, #15052, .F. ) ;
#28238 = DIRECTION ( 'NONE',  ( 0.000000000000000000, 1.000000000000000000, 0.000000000000000000 ) ) ;
#28239 = CARTESIAN_POINT ( 'NONE',  ( -56.84499999999997755, -7.632228543268599452, 2.479861379858951054 ) ) ;
#28240 = ORIENTED_EDGE ( 'NONE', *, *, #34867, .T. ) ;
#28241 = AXIS2_PLACEMENT_3D ( 'NONE', #36077, #9345, #14260 ) ;
#28242 = CARTESIAN_POINT ( 'NONE',  ( -75.00000000000000000, 8.681424763010927137, 5.653729937179129195 ) ) ;
#28243 = CARTESIAN_POINT ( 'NONE',  ( -118.1049999999999898, -6.826472737025115478, 4.959722759717900331 ) ) ;
#28244 = VERTEX_POINT ( 'NONE', #19267 ) ;
#28245 = DIRECTION ( 'NONE',  ( 0.000000000000000000, -0.000000000000000000, -1.000000000000000000 ) ) ;
#28246 =( NAMED_UNIT ( * ) PLANE_ANGLE_UNIT ( ) SI_UNIT ( $, .RADIAN. ) );
#28247 = EDGE_CURVE ( 'NONE', #58978, #19151, #15957, .T. ) ;
#28248 = CARTESIAN_POINT ( 'NONE',  ( -22.50000000000000711, 33.74999999999999289, -3.750000000000000000 ) ) ;
#28249 = DIRECTION ( 'NONE',  ( 1.000000000000000000, 0.000000000000000000, 0.000000000000000000 ) ) ;
#28250 = CARTESIAN_POINT ( 'NONE',  ( -147.5070736234661695, 8.102448949553176405, 5.886773742842740909 ) ) ;
#28251 = VECTOR ( 'NONE', #48263, 1000.000000000000000 ) ;
#28252 = CARTESIAN_POINT ( 'NONE',  ( 29.00000000000000000, 38.93969262078592664, -89.65797985667437331 ) ) ;
#28253 = CARTESIAN_POINT ( 'NONE',  ( 10.01517768586949408, 132.6949999999999648, 1.839758294383810543E-15 ) ) ;
#28254 = CARTESIAN_POINT ( 'NONE',  ( -81.35707362346616378, 5.598654528085804216, 7.705886871421366635 ) ) ;
#28255 = AXIS2_PLACEMENT_3D ( 'NONE', #69452, #21239, #25834 ) ;
#28256 = STYLED_ITEM ( 'NONE', ( #34977 ), #13010 ) ;
#28257 = EDGE_CURVE ( 'NONE', #13670, #22419, #58112, .T. ) ;
#28258 = CARTESIAN_POINT ( 'NONE',  ( 179.4361977533490347, 0.9999999999999991118, 103.7004518695263044 ) ) ;
#28259 = ORIENTED_EDGE ( 'NONE', *, *, #4913, .F. ) ;
#28260 = LINE ( 'NONE', #29324, #52698 ) ;
#28263 =( GEOMETRIC_REPRESENTATION_CONTEXT ( 3 ) GLOBAL_UNCERTAINTY_ASSIGNED_CONTEXT ( ( #18694 ) ) GLOBAL_UNIT_ASSIGNED_CONTEXT ( ( #60906, #43748, #54599 ) ) REPRESENTATION_CONTEXT ( 'NONE', 'WORKASPACE' ) );
#28262 = DIRECTION ( 'NONE',  ( 1.000000000000000000, 0.000000000000000000, 0.000000000000000000 ) ) ;
#28261 = LINE ( 'NONE', #49770, #12180 ) ;
#28264 =( LENGTH_UNIT ( ) NAMED_UNIT ( * ) SI_UNIT ( .MILLI., .METRE. ) );
#28265 = CARTESIAN_POINT ( 'NONE',  ( -131.4549999999999841, 7.632228543268599452, -2.479861379858951942 ) ) ;
#28266 = CARTESIAN_POINT ( 'NONE',  ( -16.75000000000000000, -4.000000000000000000, 24.00000000000000000 ) ) ;
#28267 = DIRECTION ( 'NONE',  ( -1.000000000000000000, 0.000000000000000000, 0.000000000000000000 ) ) ;
#28268 = DIRECTION ( 'NONE',  ( 0.000000000000000000, -0.7431448254773944662, -0.6691306063588580155 ) ) ;
#28269 = AXIS2_PLACEMENT_3D ( 'NONE', #2226, #29733, #40302 ) ;
#28270 = CARTESIAN_POINT ( 'NONE',  ( -143.8449999999999989, -7.632228543268599452, 2.479861379858951054 ) ) ;
#28271 = CARTESIAN_POINT ( 'NONE',  ( -132.2949999999999875, -2.607480562269069768, 8.024999999999991473 ) ) ;
#28272 = PRESENTATION_LAYER_ASSIGNMENT (  '', '', ( #6960 ) ) ;
#28273 = ORIENTED_EDGE ( 'NONE', *, *, #65277, .T. ) ;
#28274 = PRESENTATION_LAYER_ASSIGNMENT (  '', '', ( #20438 ) ) ;
#28275 = CARTESIAN_POINT ( 'NONE',  ( -146.6070736234661638, -8.102448949553174629, 5.886773742842742685 ) ) ;
#28276 = PRESENTATION_STYLE_ASSIGNMENT (( #1160 ) ) ;
#28277 =( LENGTH_UNIT ( ) NAMED_UNIT ( * ) SI_UNIT ( .MILLI., .METRE. ) );
#28278 = UNCERTAINTY_MEASURE_WITH_UNIT (LENGTH_MEASURE( 1.000000000000000082E-05 ), #61316, 'distance_accuracy_value', 'NONE');
#28279 = CARTESIAN_POINT ( 'NONE',  ( -178.7929263765338135, -3.094860106618429807, 9.524999999999991473 ) ) ;
#28280 = COLOUR_RGB ( '', 0.72549020, 0.75294118, 0.79215686) ;
#28281 = CARTESIAN_POINT ( 'NONE',  ( -63.14499999999998181, -4.716976649647092401, 6.492361379858946790 ) ) ;
#28282 = AXIS2_PLACEMENT_3D ( 'NONE', #60628, #18089, #39576 ) ;
#28283 = DIRECTION ( 'NONE',  ( 0.000000000000000000, -1.000000000000000000, 0.000000000000000000 ) ) ;
#28284 = DIRECTION ( 'NONE',  ( -1.000000000000000000, 0.000000000000000000, 0.000000000000000000 ) ) ;
#28285 = CARTESIAN_POINT ( 'NONE',  ( -72.49999999999998579, 119.9999999999997868, 9.500000000000000000 ) ) ;
#28286 = AXIS2_PLACEMENT_3D ( 'NONE', #52803, #53482, #14442 ) ;
#28287 = DIRECTION ( 'NONE',  ( 0.000000000000000000, -1.000000000000000000, 0.000000000000000000 ) ) ;
#28288 = CARTESIAN_POINT ( 'NONE',  ( 9.827790563157511022E-16, 87.30187232391182306, -8.025000000000000355 ) ) ;
#28289 = CARTESIAN_POINT ( 'NONE',  ( -90.89292637653380780, -8.102448949553172852, -5.886773742842741797 ) ) ;
#28290 = FILL_AREA_STYLE_COLOUR ( '', #24451 ) ;
#28291 =( BOUNDED_CURVE ( )  B_SPLINE_CURVE ( 2, ( #8664, #4049, #3325, #9724, #20600, #24814, #14278, #52630, #14637, #35744, #36479 ),
 .UNSPECIFIED., .F., .F. ) 
 B_SPLINE_CURVE_WITH_KNOTS ( ( 3, 2, 2, 2, 2, 3 ),
 ( 0.8478260869565217295, 0.8499999999999999778, 0.8521739130434782261, 0.8543478260869564744, 0.8565217391304348338, 0.8586956521739130821 ),
 .UNSPECIFIED. ) 
 CURVE ( )  GEOMETRIC_REPRESENTATION_ITEM ( )  RATIONAL_B_SPLINE_CURVE ( ( 1.000000000000000000, 0.9510565162951535312, 1.000000000000000000, 0.9510565162951535312, 1.000000000000000000, 0.9510565162951535312, 1.000000000000000000, 0.9510565162951535312, 1.000000000000000000, 0.9510565162951535312, 1.000000000000000000 ) ) 
 REPRESENTATION_ITEM ( '' )  );
#28292 = EDGE_CURVE ( 'NONE', #10009, #45103, #60840, .T. ) ;
#28293 = PRESENTATION_LAYER_ASSIGNMENT (  '', '', ( #30563 ) ) ;
#28294 = DIRECTION ( 'NONE',  ( 0.000000000000000000, 0.000000000000000000, 1.000000000000000000 ) ) ;
#28295 = CONICAL_SURFACE ( 'NONE', #65444, 3.499999999999997780, 0.7853981633974452814 ) ;
#28296 = VERTEX_POINT ( 'NONE', #57981 ) ;
#28297 =( LENGTH_UNIT ( ) NAMED_UNIT ( * ) SI_UNIT ( .MILLI., .METRE. ) );
#28298 = CARTESIAN_POINT ( 'NONE',  ( -54.93556801395976663, -8.762778093175660032, -2.499999999999992895 ) ) ;
#28299 = ORIENTED_EDGE ( 'NONE', *, *, #44181, .F. ) ;
#28300 =( NAMED_UNIT ( * ) PLANE_ANGLE_UNIT ( ) SI_UNIT ( $, .RADIAN. ) );
#28301 = COLOUR_RGB ( '', 0.31764706, 0.68627451, 0.89019608) ;
#28302 = CARTESIAN_POINT ( 'NONE',  ( -4.716976649647098618, 119.2570736234661553, 6.492361379858953008 ) ) ;
#28303 = PRODUCT_RELATED_PRODUCT_CATEGORY ( 'part', '', ( #4050 ) ) ;
#28304 =( GEOMETRIC_REPRESENTATION_CONTEXT ( 3 ) GLOBAL_UNCERTAINTY_ASSIGNED_CONTEXT ( ( #46714 ) ) GLOBAL_UNIT_ASSIGNED_CONTEXT ( ( #14101, #61555, #51041 ) ) REPRESENTATION_CONTEXT ( 'NONE', 'WORKASPACE' ) );
#28305 = EDGE_CURVE ( 'NONE', #28053, #43827, #42933, .T. ) ;
#28306 = DIRECTION ( 'NONE',  ( 0.000000000000000000, 0.000000000000000000, -1.000000000000000000 ) ) ;
#28307 = EDGE_CURVE ( 'NONE', #27455, #35469, #14837, .T. ) ;
#28308 = CARTESIAN_POINT ( 'NONE',  ( 0.000000000000000000, 139.0570736234661808, -8.025000000000000355 ) ) ;
#28309 = AXIS2_PLACEMENT_3D ( 'NONE', #63489, #10031, #47350 ) ;
#28310 = DIRECTION ( 'NONE',  ( -0.000000000000000000, 0.000000000000000000, -1.000000000000000000 ) ) ;
#28311 = EDGE_LOOP ( 'NONE', ( #40566, #55934, #27126, #15236 ) ) ;
#28312 = EDGE_CURVE ( 'NONE', #17287, #15954, #14351, .T. ) ;
#28313 = DIRECTION ( 'NONE',  ( 1.000000000000000000, 0.000000000000000000, 0.000000000000000000 ) ) ;
#28314 = ORIENTED_EDGE ( 'NONE', *, *, #9390, .T. ) ;
#28315 = ADVANCED_FACE ( 'NONE', ( #68526 ), #4120, .T. ) ;
#28316 = FACE_OUTER_BOUND ( 'NONE', #58630, .T. ) ;
#28317 = CARTESIAN_POINT ( 'NONE',  ( -93.95707362346617231, 9.058813317711329915, -2.943386871421373119 ) ) ;
#28318 = AXIS2_PLACEMENT_3D ( 'NONE', #46225, #23682, #13123 ) ;
#28319 = CARTESIAN_POINT ( 'NONE',  ( 0.000000000000000000, 134.9429263765338192, -8.025000000000000355 ) ) ;
#28320 = CARTESIAN_POINT ( 'NONE',  ( -92.09499999999998465, -2.607480562269071545, -8.024999999999991473 ) ) ;
#28321 = ORIENTED_EDGE ( 'NONE', *, *, #8457, .F. ) ;
#28322 = AXIS2_PLACEMENT_3D ( 'NONE', #59387, #55519, #48909 ) ;
#28323 = SURFACE_STYLE_USAGE ( .BOTH. , #65644 ) ;
#28324 =( NAMED_UNIT ( * ) SI_UNIT ( $, .STERADIAN. ) SOLID_ANGLE_UNIT ( ) );
#28325 = EDGE_CURVE ( 'NONE', #7688, #10952, #41828, .T. ) ;
#28326 = SURFACE_STYLE_FILL_AREA ( #59663 ) ;
#28327 = EDGE_LOOP ( 'NONE', ( #64958, #11469, #13039, #22229, #23403 ) ) ;
#28328 = FACE_OUTER_BOUND ( 'NONE', #10780, .T. ) ;
#28329 = EDGE_CURVE ( 'NONE', #60166, #7942, #8738, .T. ) ;
#28330 = CIRCLE ( 'NONE', #25007, 0.5000000000000000000 ) ;
#28331 = CARTESIAN_POINT ( 'NONE',  ( 5.603096392576905949, 1.514639124457112240, -8.295152368350905192 ) ) ;
#28332 = ORIENTED_EDGE ( 'NONE', *, *, #57598, .T. ) ;
#28333 = AXIS2_PLACEMENT_3D ( 'NONE', #26291, #53399, #4473 ) ;
#28334 = CARTESIAN_POINT ( 'NONE',  ( 31.00000000000001066, 42.00000000000000000, -4.033029030585349936E-15 ) ) ;
#28335 = ORIENTED_EDGE ( 'NONE', *, *, #24313, .F. ) ;
#28336 = DIRECTION ( 'NONE',  ( 0.000000000000000000, 0.000000000000000000, -1.000000000000000000 ) ) ;
#28337 = DIRECTION ( 'NONE',  ( 0.000000000000000000, 0.000000000000000000, 1.000000000000000000 ) ) ;
#28338 = LINE ( 'NONE', #1580, #36444 ) ;
#28339 = LINE ( 'NONE', #182, #41225 ) ;
#28340 = CARTESIAN_POINT ( 'NONE',  ( -179.6070736234661922, -8.102448949553172852, 5.886773742842742685 ) ) ;
#28341 = SURFACE_STYLE_USAGE ( .BOTH. , #66001 ) ;
#28342 = CARTESIAN_POINT ( 'NONE',  ( -22.75000000000000711, 36.75000000000000000, 4.000000000000000000 ) ) ;
#28343 = CARTESIAN_POINT ( 'NONE',  ( -114.0570736234661808, 0.000000000000000000, 9.524999999999991473 ) ) ;
#28344 = CARTESIAN_POINT ( 'NONE',  ( -4.792168507806671585, 9.000000000000008882, 1.190312887963165922 ) ) ;
#28345 = COLOUR_RGB ( '', 0.08235294, 0.09019608, 0.10196078) ;
#28346 = CARTESIAN_POINT ( 'NONE',  ( 51.49999999999998579, 2.837994680254535968E-15, 10.50000000000000000 ) ) ;
#28347 = VERTEX_POINT ( 'NONE', #57264 ) ;
#28348 = CARTESIAN_POINT ( 'NONE',  ( 6.826472737025121695, 122.4929263765338021, -4.959722759717905660 ) ) ;
#28349 = CARTESIAN_POINT ( 'NONE',  ( -149.9070736234666015, -3.094860106611606820, 9.525000000004951062 ) ) ;
#28350 = EDGE_LOOP ( 'NONE', ( #63120, #6258, #19808, #31028 ) ) ;
#28351 = CARTESIAN_POINT ( 'NONE',  ( -160.1049999999999613, -6.826472737025115478, 4.959722759717900331 ) ) ;
#28352 = CARTESIAN_POINT ( 'NONE',  ( -75.00000000000000000, 7.768687147774684831, 6.999999999999999112 ) ) ;
#28353 = CARTESIAN_POINT ( 'NONE',  ( 15.98999599679679839, 118.4999999999999716, -7.500000000000000000 ) ) ;
#28354 = CARTESIAN_POINT ( 'NONE',  ( -175.3449999999999989, 7.632228543268599452, -2.479861379858951942 ) ) ;
#28355 = AXIS2_PLACEMENT_3D ( 'NONE', #60792, #49588, #65037 ) ;
#28356 = CARTESIAN_POINT ( 'NONE',  ( -159.4449999999999932, 0.000000000000000000, 8.024999999999991473 ) ) ;
#28357 = ADVANCED_FACE ( 'NONE', ( #47103 ), #55220, .F. ) ;
#28358 = VERTEX_POINT ( 'NONE', #52369 ) ;
#28359 = CARTESIAN_POINT ( 'NONE',  ( 44.75458990717699947, 9.918196635725768928, 3.527112199763593914 ) ) ;
#28360 = CARTESIAN_POINT ( 'NONE',  ( -76.85499999999998977, 4.716976649647094177, 6.492361379858945902 ) ) ;
#28361 = B_SPLINE_CURVE_WITH_KNOTS ( 'NONE', 3,
 ( #52211, #36405, #68727, #67317, #9979, #46617, #52894, #62392, #20523, #14210, #13856, #25787, #14920, #47300, #35668, #30350, #14544, #57105, #67670, #42032, #20155, #19470, #36748, #36020, #56775, #57462, #31399, #19823, #8927, #40612, #3974, #8590, #25444, #57819, #41311, #9645 ),
 .UNSPECIFIED., .F., .F.,
 ( 4, 2, 2, 2, 2, 2, 2, 2, 2, 2, 2, 2, 2, 2, 2, 2, 2, 4 ),
 ( 0.02371714007185215731, 0.02470529243674880401, 0.02569344480164545072, 0.02668159716654209743, 0.02766974953143874066, 0.02865790189633538737, 0.02964605426123203408, 0.03063420662612868078, 0.03162235899102532749, 0.03261051135592197420, 0.03359866372081862090, 0.03458681608571526761, 0.03557496845061191432, 0.03656312081550856102, 0.03755127318040520773, 0.03804534936285353108, 0.03853942554530184750, 0.03952757791019850808 ),
 .UNSPECIFIED. ) ;
#28362 = CARTESIAN_POINT ( 'NONE',  ( -39.71230376710084187, -11.68673171624858931, 3.338102362379923083 ) ) ;
#28363 = VECTOR ( 'NONE', #25759, 1000.000000000000000 ) ;
#28364 = CARTESIAN_POINT ( 'NONE',  ( 27.99999999999999645, 5.000000000000000000, -24.00402776293821816 ) ) ;
#28365 = CARTESIAN_POINT ( 'NONE',  ( -66.59499999999998465, 2.607480562269072433, 8.024999999999991473 ) ) ;
#28366 = CLOSED_SHELL ( 'NONE', ( #64427, #48541, #30465, #26728, #55830, #18130, #12772, #7725, #30554, #20131, #30904, #27578, #48535, #18619, #65841, #67186, #64664, #66256, #36708, #15671, #27232, #32019, #25544, #38822, #51009, #794, #6670, #62575, #21448, #64861, #54940, #64502, #27533, #51320, #29721, #17357, #37288, #20004, #15461, #55910, #37809, #68146, #47576, #33759, #50388, #50198, #13107, #47071, #44520, #41236, #45046, #64494, #55689, #31206, #2300, #29942, #19393, #20831, #34424, #33519, #5942, #18510, #23173, #68096, #60147, #41984, #13646, #16959, #36342, #18025, #29374, #13416, #24372, #41999, #46682, #30823, #860, #64335, #49900, #17505, #49927, #4244, #23349, #1361, #2979, #18736, #36833, #5913, #29292, #26811, #64847, #62418, #49406, #18146, #26588, #31123, #34285, #66208, #4098, #15915, #1193, #57934, #5543, #4514, #25713, #29051, #48820, #2068, #3743, #65300, #10747, #55078, #27954, #18668, #8169, #16171, #17748, #3134, #8018 ) ) ;
#28367 = CARTESIAN_POINT ( 'NONE',  ( 9.058813317711338797, 142.9550000000000125, -2.943386871421372675 ) ) ;
#28368 = CARTESIAN_POINT ( 'NONE',  ( 15.98999599679679839, 146.4999999999999716, -7.500000000000000000 ) ) ;
#28369 = PRODUCT_DEFINITION_SHAPE ( 'NONE', 'NONE',  #69715 ) ;
#28370 = MECHANICAL_DESIGN_GEOMETRIC_PRESENTATION_REPRESENTATION (  '', ( #50854 ), #3608 ) ;
#28371 = CARTESIAN_POINT ( 'NONE',  ( 4.886038412224959160, 154.3548647706442409, 8.015157697667703474 ) ) ;
#28372 = UNCERTAINTY_MEASURE_WITH_UNIT (LENGTH_MEASURE( 1.000000000000000082E-05 ), #52259, 'distance_accuracy_value', 'NONE');
#28373 = MECHANICAL_DESIGN_GEOMETRIC_PRESENTATION_REPRESENTATION (  '', ( #32893 ), #67730 ) ;
#28374 = LINE ( 'NONE', #2288, #59613 ) ;
#28375 = VERTEX_POINT ( 'NONE', #15092 ) ;
#28376 = CIRCLE ( 'NONE', #23894, 0.4999999999999994449 ) ;
#28377 = DIRECTION ( 'NONE',  ( -0.000000000000000000, 1.000000000000000000, -0.000000000000000000 ) ) ;
#28378 = STYLED_ITEM ( 'NONE', ( #48414 ), #19538 ) ;
#28379 = DIRECTION ( 'NONE',  ( 1.000000000000000000, -0.000000000000000000, -0.000000000000000000 ) ) ;
#28380 =( NAMED_UNIT ( * ) SI_UNIT ( $, .STERADIAN. ) SOLID_ANGLE_UNIT ( ) );
#28381 = ORIENTED_EDGE ( 'NONE', *, *, #10289, .T. ) ;
#28382 = VERTEX_POINT ( 'NONE', #2721 ) ;
#28383 = DIRECTION ( 'NONE',  ( -0.000000000000000000, -0.000000000000000000, 1.000000000000000000 ) ) ;
#28384 = FILL_AREA_STYLE_COLOUR ( '', #3457 ) ;
#28385 = CIRCLE ( 'NONE', #4817, 0.2500000000000002220 ) ;
#28386 = EDGE_CURVE ( 'NONE', #20026, #47636, #14018, .T. ) ;
#28387 = SURFACE_SIDE_STYLE ('',( #49545 ) ) ;
#28388 = CARTESIAN_POINT ( 'NONE',  ( 4.793834890952475725, 1.308853920463818987, 9.000000000000005329 ) ) ;
#28389 = SURFACE_STYLE_USAGE ( .BOTH. , #28752 ) ;
#28390 = EDGE_LOOP ( 'NONE', ( #23165, #35007, #5560, #45073 ) ) ;
#28391 = CARTESIAN_POINT ( 'NONE',  ( -111.5049999999999955, -6.826472737025113702, -4.959722759717900331 ) ) ;
#28392 = ORIENTED_EDGE ( 'NONE', *, *, #18753, .T. ) ;
#28393 = DIRECTION ( 'NONE',  ( 0.000000000000000000, 1.000000000000000000, 0.000000000000000000 ) ) ;
#28394 = EDGE_CURVE ( 'NONE', #54981, #18574, #29494, .T. ) ;
#28395 = ORIENTED_EDGE ( 'NONE', *, *, #51536, .F. ) ;
#28396 = FACE_OUTER_BOUND ( 'NONE', #58984, .T. ) ;
#28397 = CARTESIAN_POINT ( 'NONE',  ( -68.45707362346617231, -9.058813317711329915, 2.943386871421371787 ) ) ;
#28398 = EDGE_LOOP ( 'NONE', ( #6614, #15942, #57142, #23803 ) ) ;
#28399 = CIRCLE ( 'NONE', #4881, 1.000000000000000000 ) ;
#28400 = PRESENTATION_LAYER_ASSIGNMENT (  '', '', ( #52065 ) ) ;
#28401 = SURFACE_SIDE_STYLE ('',( #33370 ) ) ;
#28402 = CARTESIAN_POINT ( 'NONE',  ( 24.00000000000000355, 36.75000000000000000, -3.750000000000000000 ) ) ;
#28403 = ORIENTED_EDGE ( 'NONE', *, *, #2130, .T. ) ;
#28404 = ORIENTED_EDGE ( 'NONE', *, *, #50250, .F. ) ;
#28405 = AXIS2_PLACEMENT_3D ( 'NONE', #30861, #14705, #9082 ) ;
#28406 = CARTESIAN_POINT ( 'NONE',  ( -9.159675819040165479, 110.5000000000000000, -2.649765445813976328 ) ) ;
#28407 = CYLINDRICAL_SURFACE ( 'NONE', #158, 1.000000000000000888 ) ;
#28408 = DIRECTION ( 'NONE',  ( 0.000000000000000000, -1.000000000000000000, 0.000000000000000000 ) ) ;
#28409 = ORIENTED_EDGE ( 'NONE', *, *, #15906, .T. ) ;
#28410 = CARTESIAN_POINT ( 'NONE',  ( 6.826472737025119919, 133.8929263765338078, 4.959722759717908325 ) ) ;
#28411 = DIRECTION ( 'NONE',  ( 0.000000000000000000, 0.000000000000000000, 1.000000000000000000 ) ) ;
#28412 = LINE ( 'NONE', #34067, #5167 ) ;
#28413 = ADVANCED_FACE ( 'NONE', ( #36195 ), #57625, .T. ) ;
#28414 = CARTESIAN_POINT ( 'NONE',  ( -103.9429263765338050, 0.000000000000000000, 9.524999999999991473 ) ) ;
#28415 = CARTESIAN_POINT ( 'NONE',  ( -34.99999999999999289, 99.99999999999998579, 9.500000000000000000 ) ) ;
#28416 = EDGE_LOOP ( 'NONE', ( #62960, #57114, #7015, #32192 ) ) ;
#28417 = ORIENTED_EDGE ( 'NONE', *, *, #15295, .F. ) ;
#28418 = CARTESIAN_POINT ( 'NONE',  ( 51.99999999999998579, 1.797044900979284448E-15, -11.50000000000000000 ) ) ;
#28419 = FACE_OUTER_BOUND ( 'NONE', #69010, .T. ) ;
#28420 =( LENGTH_UNIT ( ) NAMED_UNIT ( * ) SI_UNIT ( .MILLI., .METRE. ) );
#28421 = CARTESIAN_POINT ( 'NONE',  ( -136.1049999999999898, -6.826472737025115478, 4.959722759717900331 ) ) ;
#28422 = MECHANICAL_DESIGN_GEOMETRIC_PRESENTATION_REPRESENTATION (  '', ( #10494 ), #54303 ) ;
#28423 = DIRECTION ( 'NONE',  ( -1.000000000000000000, 0.000000000000000000, 0.000000000000000000 ) ) ;
#28424 = CARTESIAN_POINT ( 'NONE',  ( 31.00000000000002132, 42.00000000000000000, 79.00402776293823592 ) ) ;
#28425 = ORIENTED_EDGE ( 'NONE', *, *, #69346, .T. ) ;
#28426 = STYLED_ITEM ( 'NONE', ( #49576 ), #55468 ) ;
#28428 = CARTESIAN_POINT ( 'NONE',  ( -156.8929263765338078, -8.102448949553174629, -5.886773742842741797 ) ) ;
#28427 = COLOUR_RGB ( '', 0.72549020, 0.75294118, 0.79215686) ;
#28429 = CARTESIAN_POINT ( 'NONE',  ( -0.3558155366086588334, -2.493171897977409568, 7.000000000000000000 ) ) ;
#28430 = EDGE_LOOP ( 'NONE', ( #23374, #49998, #23335, #68035 ) ) ;
#28431 = EDGE_LOOP ( 'NONE', ( #18895, #3289, #35546, #53188 ) ) ;
#28432 = DIRECTION ( 'NONE',  ( -1.000000000000000000, -0.000000000000000000, -0.000000000000000000 ) ) ;
#28433 = CARTESIAN_POINT ( 'NONE',  ( -108.4429263765338050, -1.166476076187852838E-15, -9.524999999999991473 ) ) ;
#28434 = VECTOR ( 'NONE', #6683, 1000.000000000000000 ) ;
#28435 = FILL_AREA_STYLE_COLOUR ( '', #10662 ) ;
#28436 = VERTEX_POINT ( 'NONE', #53710 ) ;
#28437 = CARTESIAN_POINT ( 'NONE',  ( -49.55707362346617373, -1.166476076187852838E-15, -9.524999999999991473 ) ) ;
#28438 = FILL_AREA_STYLE ('',( #39754 ) ) ;
#28439 = EDGE_CURVE ( 'NONE', #17595, #62740, #46286, .T. ) ;
#28440 = DIRECTION ( 'NONE',  ( 0.000000000000000000, 1.000000000000000000, 0.000000000000000000 ) ) ;
#28441 = EDGE_CURVE ( 'NONE', #8059, #9217, #47825, .T. ) ;
#28442 = FILL_AREA_STYLE_COLOUR ( '', #6180 ) ;
#28443 = ORIENTED_EDGE ( 'NONE', *, *, #39007, .F. ) ;
#28444 = AXIS2_PLACEMENT_3D ( 'NONE', #4851, #69562, #548 ) ;
#28445 = CARTESIAN_POINT ( 'NONE',  ( 10.00000000000002309, 60.69879356856722552, 69.02971849933236115 ) ) ;
#28446 = STYLED_ITEM ( 'NONE', ( #23918 ), #8906 ) ;
#28447 = CARTESIAN_POINT ( 'NONE',  ( 0.000000000000000000, 43.00000000000000000, 0.000000000000000000 ) ) ;
#28448 = PRESENTATION_STYLE_ASSIGNMENT (( #33746 ) ) ;
#28449 = CARTESIAN_POINT ( 'NONE',  ( -195.0000000000000000, 0.000000000000000000, 0.000000000000000000 ) ) ;
#28450 = DIRECTION ( 'NONE',  ( 1.000000000000000000, 0.000000000000000000, 0.000000000000000000 ) ) ;
#28451 = CYLINDRICAL_SURFACE ( 'NONE', #34849, 9.524999999999991473 ) ;
#28452 = PRESENTATION_LAYER_ASSIGNMENT (  '', '', ( #14033 ) ) ;
#28453 = CARTESIAN_POINT ( 'NONE',  ( -98.54499999999998749, -7.632228543268600340, -2.479861379858950166 ) ) ;
#28454 = CARTESIAN_POINT ( 'NONE',  ( -3.094860106618434248, 117.9049999999999727, 9.525000000000000355 ) ) ;
#28455 = CARTESIAN_POINT ( 'NONE',  ( -81.74499999999999034, 4.716976649647094177, 6.492361379858945902 ) ) ;
#28456 = SURFACE_STYLE_USAGE ( .BOTH. , #1704 ) ;
#28458 = DIRECTION ( 'NONE',  ( 0.000000000000000000, 0.000000000000000000, 1.000000000000000000 ) ) ;
#28457 = VECTOR ( 'NONE', #58267, 1000.000000000000114 ) ;
#28459 = CIRCLE ( 'NONE', #35227, 26.49999999999999645 ) ;
#28460 = FILL_AREA_STYLE ('',( #22881 ) ) ;
#28461 = FACE_OUTER_BOUND ( 'NONE', #40764, .T. ) ;
#28462 = UNCERTAINTY_MEASURE_WITH_UNIT (LENGTH_MEASURE( 1.000000000000000082E-05 ), #2439, 'distance_accuracy_value', 'NONE');
#28464 = CARTESIAN_POINT ( 'NONE',  ( -3.692675730757587168E-15, 42.00000000000000000, -28.38386403503541899 ) ) ;
#28463 =( REPRESENTATION_RELATIONSHIP ('NONE','NONE', #5102, #21315 ) REPRESENTATION_RELATIONSHIP_WITH_TRANSFORMATION ( #19493 )SHAPE_REPRESENTATION_RELATIONSHIP( ) );
#28465 = PRESENTATION_LAYER_ASSIGNMENT (  '', '', ( #9383 ) ) ;
#28466 = FILL_AREA_STYLE ('',( #65788 ) ) ;
#28467 = ORIENTED_EDGE ( 'NONE', *, *, #8606, .F. ) ;
#28468 = STYLED_ITEM ( 'NONE', ( #7828 ), #2312 ) ;
#28469 = CARTESIAN_POINT ( 'NONE',  ( -119.5429263765338135, 9.058813317711329915, 2.943386871421369566 ) ) ;
#28470 =( NAMED_UNIT ( * ) PLANE_ANGLE_UNIT ( ) SI_UNIT ( $, .RADIAN. ) );
#28471 = CARTESIAN_POINT ( 'NONE',  ( -141.7450000000000045, 4.716976649647094177, 6.492361379858945902 ) ) ;
#28472 = FILL_AREA_STYLE ('',( #39095 ) ) ;
#28473 = CONICAL_SURFACE ( 'NONE', #62235, 8.025000000000000355, 0.7853981633974421728 ) ;
#28474 = EDGE_CURVE ( 'NONE', #45120, #21141, #63917, .T. ) ;
#28475 = CARTESIAN_POINT ( 'NONE',  ( -173.9929263765338021, 8.102448949553172852, -5.886773742842744461 ) ) ;
#28476 = ORIENTED_EDGE ( 'NONE', *, *, #69259, .F. ) ;
#28477 = ORIENTED_EDGE ( 'NONE', *, *, #20988, .T. ) ;
#28478 = DIRECTION ( 'NONE',  ( 0.000000000000000000, 0.000000000000000000, -1.000000000000000000 ) ) ;
#28479 = PRESENTATION_STYLE_ASSIGNMENT (( #6004 ) ) ;
#28480 = MECHANICAL_DESIGN_GEOMETRIC_PRESENTATION_REPRESENTATION (  '', ( #43180 ), #37561 ) ;
#28481 = DIRECTION ( 'NONE',  ( 0.000000000000000000, 0.000000000000000000, -1.000000000000000000 ) ) ;
#28482 = CARTESIAN_POINT ( 'NONE',  ( -131.7570736234661695, -5.598654528085801552, 7.705886871421367523 ) ) ;
#28483 = CARTESIAN_POINT ( 'NONE',  ( -69.74999999999998579, -3.000000000000000000, 20.00000000000000000 ) ) ;
#28484 = CIRCLE ( 'NONE', #37564, 0.5000000000000004441 ) ;
#28485 = ORIENTED_EDGE ( 'NONE', *, *, #20745, .T. ) ;
#28486 = CARTESIAN_POINT ( 'NONE',  ( -141.3550000000000182, -4.716976649647093289, -6.492361379858945902 ) ) ;
#28487 = ORIENTED_EDGE ( 'NONE', *, *, #26195, .F. ) ;
#28488 = AXIS2_PLACEMENT_3D ( 'NONE', #14314, #67424, #62141 ) ;
#28489 = EDGE_CURVE ( 'NONE', #38619, #54121, #44524, .T. ) ;
#28490 = ORIENTED_EDGE ( 'NONE', *, *, #55524, .F. ) ;
#28491 = DIRECTION ( 'NONE',  ( -0.000000000000000000, -0.000000000000000000, 1.000000000000000000 ) ) ;
#28492 = CARTESIAN_POINT ( 'NONE',  ( 10.00000000000001776, 42.74314482547740113, -27.71473342867655987 ) ) ;
#28493 = ORIENTED_EDGE ( 'NONE', *, *, #19194, .T. ) ;
#28494 = FACE_OUTER_BOUND ( 'NONE', #37349, .T. ) ;
#28495 = EDGE_CURVE ( 'NONE', #26861, #65035, #12102, .T. ) ;
#28496 = DIRECTION ( 'NONE',  ( 0.000000000000000000, 0.000000000000000000, 1.000000000000000000 ) ) ;
#28497 = CARTESIAN_POINT ( 'NONE',  ( 8.102448949553183510, 129.9950000000000045, -5.886773742842746238 ) ) ;
#28498 = CARTESIAN_POINT ( 'NONE',  ( 25.00000000000001421, 43.00000000000000000, 29.68999999999999417 ) ) ;
#28499 =( BOUNDED_CURVE ( )  B_SPLINE_CURVE ( 2, ( #51225, #29033, #18840, #61066, #25176, #29400, #61741, #3322, #45964, #30089, #45288, #40010, #13567, #51924, #19183, #35036, #46693, #23784, #56487, #50535, #2257, #51562, #68109, #34347, #67391, #2971, #9008, #55796, #66705, #12883, #18522, #61403, #8322, #24460, #62103, #13218, #67747, #14276, #50875, #13930, #8660, #2634, #35398, #56849, #24808, #24131, #46328, #34675, #45639, #19547, #41044, #62459, #30422, #35740, #20595, #69142, #42111, #10404, #57537, #68440, #25860, #20948, #16045, #42445, #15682, #58230, #31479, #10052, #53317, #15358, #63506, #47369, #48070, #52287, #4046, #63835, #9718, #36812, #68804, #42800, #57897, #26869, #26549, #37164, #58573, #4751, #58929, #52627, #47748, #5101, #31130, #52963, #37522, #10739, #32187, #69473, #20237, #31827, #21263, #64188, #53638, #5423, #26206, #14633, #48407, #97, #30788, #41385, #62791, #36095, #9363, #25512, #4381, #36475, #47026, #41739, #63164, #15000, #39230, #64553, #59240, #6148, #11063, #27579, #38195, #12103, #6473, #33569, #33232, #32510, #33906, #27222, #1142, #50120, #49419, #55002, #55373, #16394, #27907, #11769, #60629, #5775, #21628, #48760, #43144, #49096, #17078, #22676, #12444, #28253, #44525, #59598, #43821, #38894, #1502, #37869, #65578, #60300, #17428, #23030, #21992, #64878, #781, #16731, #65229, #7195, #6830, #22325, #44179, #38557, #49764, #53974, #463, #59950, #43495, #65929, #54326, #11416, #32890, #54672, #17758, #28623, #45563, #24056, #56053, #8584, #12801, #34268, #51152, #39930, #2547, #29318, #66265, #13487, #34959, #18776, #23708, #61333, #62022, #2899, #24727, #13851, #13143, #66983, #46245, #67665, #40968, #35316, #28956, #24387, #45884, #67313, #19102, #35661, #62387, #30343, #56772, #7869, #1847, #50798, #18091, #40254, #40608, #51481, #34598, #66628, #18445, #23358, #3239, #30018, #14203, #19465, #57099, #8920, #61656, #39577, #56405, #8241, #44859, #29683, #60982, #55723, #7529, #50447, #2176, #45207, #68032, #15611, #31057, #25780, #46611, #36744, #52551, #58159, #58845, #15965, #42025, #19818, #69066, #63431, #63075, #42713, #58496, #5023, #20147, #4297, #20872, #31747, #41305, #26125, #42374, #47661, #53235, #52206, #52889, #41657, #63760, #62706, #51847, #37085, #47292, #9975, #68720, #10321, #14536, #9280, #36398, #36013, #26476, #14914, #30698, #3594, #57813, #15278, #4672, #48001, #20517 ),
 .UNSPECIFIED., .F., .F. ) 
 B_SPLINE_CURVE_WITH_KNOTS ( ( 3, 2, 2, 2, 2, 2, 2, 2, 2, 2, 2, 2, 2, 2, 2, 2, 2, 2, 2, 2, 2, 2, 2, 2, 2, 2, 2, 2, 2, 2, 2, 2, 2, 2, 2, 2, 2, 2, 2, 2, 2, 2, 2, 2, 2, 2, 2, 2, 2, 2, 2, 2, 2, 2, 2, 2, 2, 2, 2, 2, 2, 2, 2, 2, 2, 2, 2, 2, 2, 2, 2, 2, 2, 2, 2, 2, 2, 2, 2, 2, 2, 2, 2, 2, 2, 2, 2, 2, 2, 2, 2, 2, 2, 2, 2, 2, 2, 2, 2, 2, 2, 2, 2, 2, 2, 2, 2, 2, 2, 2, 2, 2, 2, 2, 2, 2, 2, 2, 2, 2, 2, 2, 2, 2, 2, 2, 2, 2, 2, 2, 2, 2, 2, 2, 2, 2, 2, 2, 2, 2, 2, 2, 2, 2, 2, 2, 2, 2, 3 ),
 ( 0.02068387785645816809, 0.02352941176470588203, 0.02941176470588235253, 0.03529411764705882304, 0.04117647058823529355, 0.04705882352941176405, 0.05294117647058824150, 0.05882352941176470507, 0.06470588235294118251, 0.07058823529411764608, 0.07647058823529412352, 0.08235294117647057321, 0.08823529411764706454, 0.09411764705882352811, 0.1000000000000000056, 0.1058823529411764691, 0.1117647058823529466, 0.1176470588235294101, 0.1235294117647058876, 0.1294117647058823650, 0.1352941176470588147, 0.1411764705882352922, 0.1470588235294117696, 0.1529411764705882470, 0.1588235294117646967, 0.1647058823529411742, 0.1705882352941176516, 0.1764705882352941568, 0.1823529411764705788, 0.1882352941176470562, 0.1941176470588235337, 0.2000000000000000111, 0.2058823529411764608, 0.2117647058823529382, 0.2176470588235294157, 0.2235294117647058931, 0.2294117647058823428, 0.2352941176470588203, 0.2411764705882352977, 0.2470588235294117752, 0.2529411764705882248, 0.2588235294117647300, 0.2647058823529411797, 0.2705882352941176294, 0.2764705882352941346, 0.2823529411764705843, 0.2882352941176470340, 0.2941176470588235392, 0.2999999999999999889, 0.3058823529411764941, 0.3117647058823529438, 0.3176470588235293935, 0.3235294117647059542, 0.3294117647058822929, 0.3352941176470587981, 0.3411764705882353033, 0.3470588235294117530, 0.3529411764705882582, 0.3588235294117647078, 0.3647058823529412130, 0.3705882352941176627, 0.3764705882352941124, 0.3823529411764705621, 0.3882352941176470673, 0.3941176470588235170, 0.4000000000000000222, 0.4058823529411764719, 0.4117647058823529216, 0.4176470588235294268, 0.4235294117647058765, 0.4294117647058823262, 0.4352941176470587759, 0.4411764705882352811, 0.4470588235294117863, 0.4529411764705882359, 0.4588235294117646856, 0.4647058823529411908, 0.4705882352941176960, 0.4764705882352940902, 0.4823529411764705954, 0.4882352941176470451, 0.4941176470588235503, 0.5000000000000000000, 0.5058823529411765607, 0.5117647058823528994, 0.5176470588235294601, 0.5235294117647059098, 0.5294117647058823595, 0.5352941176470588092, 0.5411764705882352589, 0.5470588235294118196, 0.5529411764705882693, 0.5588235294117647189, 0.5647058823529411686, 0.5705882352941176183, 0.5764705882352940680, 0.5823529411764706287, 0.5882352941176470784, 0.5941176470588235281, 0.5999999999999999778, 0.6058823529411764275, 0.6117647058823529882, 0.6176470588235294379, 0.6235294117647058876, 0.6294117647058823373, 0.6352941176470587870, 0.6411764705882353477, 0.6470588235294117974, 0.6529411764705882470, 0.6588235294117646967, 0.6647058823529411464, 0.6705882352941175961, 0.6764705882352941568, 0.6823529411764706065, 0.6882352941176470562, 0.6941176470588235059, 0.6999999999999999556, 0.7058823529411765163, 0.7117647058823529660, 0.7176470588235294157, 0.7235294117647058654, 0.7294117647058823151, 0.7352941176470588758, 0.7411764705882352144, 0.7470588235294117752, 0.7529411764705882248, 0.7588235294117646745, 0.7647058823529411242, 0.7705882352941177960, 0.7764705882352941346, 0.7823529411764704733, 0.7882352941176470340, 0.7941176470588234837, 0.8000000000000000444, 0.8058823529411764941, 0.8117647058823530548, 0.8176470588235293935, 0.8235294117647058432, 0.8294117647058824039, 0.8352941176470588536, 0.8411764705882353033, 0.8470588235294117530, 0.8529411764705883137, 0.8588235294117646523, 0.8647058823529412130, 0.8705882352941176627, 0.8764705882352941124, 0.8823529411764705621, 0.8834592151850780839 ),
 .UNSPECIFIED. ) 
 CURVE ( )  GEOMETRIC_REPRESENTATION_ITEM ( )  RATIONAL_B_SPLINE_CURVE ( ( 0.9755541358147095110, 0.9763240417801153370, 1.000000000000000000, 0.9510565162951535312, 1.000000000000000000, 0.9510565162951535312, 1.000000000000000000, 0.9510565162951535312, 1.000000000000000000, 0.9510565162951535312, 1.000000000000000000, 0.9510565162951535312, 1.000000000000000000, 0.9510565162951535312, 1.000000000000000000, 0.9510565162951535312, 1.000000000000000000, 0.9510565162951535312, 1.000000000000000000, 0.9510565162951535312, 1.000000000000000000, 0.9510565162951535312, 1.000000000000000000, 0.9510565162951535312, 1.000000000000000000, 0.9510565162951535312, 1.000000000000000000, 0.9510565162951535312, 1.000000000000000000, 0.9510565162951535312, 1.000000000000000000, 0.9510565162951535312, 1.000000000000000000, 0.9510565162951535312, 1.000000000000000000, 0.9510565162951535312, 1.000000000000000000, 0.9510565162951535312, 1.000000000000000000, 0.9510565162951535312, 1.000000000000000000, 0.9510565162951535312, 1.000000000000000000, 0.9510565162951535312, 1.000000000000000000, 0.9510565162951535312, 1.000000000000000000, 0.9510565162951535312, 1.000000000000000000, 0.9510565162951535312, 1.000000000000000000, 0.9510565162951535312, 1.000000000000000000, 0.9510565162951535312, 1.000000000000000000, 0.9510565162951535312, 1.000000000000000000, 0.9510565162951535312, 1.000000000000000000, 0.9510565162951535312, 1.000000000000000000, 0.9510565162951535312, 1.000000000000000000, 0.9510565162951535312, 1.000000000000000000, 0.9510565162951535312, 1.000000000000000000, 0.9510565162951535312, 1.000000000000000000, 0.9510565162951535312, 1.000000000000000000, 0.9510565162951535312, 1.000000000000000000, 0.9510565162951535312, 1.000000000000000000, 0.9510565162951535312, 1.000000000000000000, 0.9510565162951535312, 1.000000000000000000, 0.9510565162951535312, 1.000000000000000000, 0.9510565162951535312, 1.000000000000000000, 0.9510565162951535312, 1.000000000000000000, 0.9510565162951535312, 1.000000000000000000, 0.9510565162951535312, 1.000000000000000000, 0.9510565162951535312, 1.000000000000000000, 0.9510565162951535312, 1.000000000000000000, 0.9510565162951535312, 1.000000000000000000, 0.9510565162951535312, 1.000000000000000000, 0.9510565162951535312, 1.000000000000000000, 0.9510565162951535312, 1.000000000000000000, 0.9510565162951535312, 1.000000000000000000, 0.9510565162951535312, 1.000000000000000000, 0.9510565162951535312, 1.000000000000000000, 0.9510565162951535312, 1.000000000000000000, 0.9510565162951535312, 1.000000000000000000, 0.9510565162951535312, 1.000000000000000000, 0.9510565162951535312, 1.000000000000000000, 0.9510565162951535312, 1.000000000000000000, 0.9510565162951535312, 1.000000000000000000, 0.9510565162951535312, 1.000000000000000000, 0.9510565162951535312, 1.000000000000000000, 0.9510565162951535312, 1.000000000000000000, 0.9510565162951535312, 1.000000000000000000, 0.9510565162951535312, 1.000000000000000000, 0.9510565162951535312, 1.000000000000000000, 0.9510565162951535312, 1.000000000000000000, 0.9510565162951535312, 1.000000000000000000, 0.9510565162951535312, 1.000000000000000000, 0.9510565162951535312, 1.000000000000000000, 0.9510565162951535312, 1.000000000000000000, 0.9510565162951535312, 1.000000000000000000, 0.9510565162951535312, 1.000000000000000000, 0.9510565162951535312, 1.000000000000000000, 0.9510565162951535312, 1.000000000000000000, 0.9510565162951535312, 1.000000000000000000, 0.9510565162951535312, 1.000000000000000000, 0.9510565162951535312, 1.000000000000000000, 0.9510565162951535312, 1.000000000000000000, 0.9510565162951535312, 1.000000000000000000, 0.9510565162951535312, 1.000000000000000000, 0.9510565162951535312, 1.000000000000000000, 0.9510565162951535312, 1.000000000000000000, 0.9510565162951535312, 1.000000000000000000, 0.9510565162951535312, 1.000000000000000000, 0.9510565162951535312, 1.000000000000000000, 0.9510565162951535312, 1.000000000000000000, 0.9510565162951535312, 1.000000000000000000, 0.9510565162951535312, 1.000000000000000000, 0.9510565162951535312, 1.000000000000000000, 0.9510565162951535312, 1.000000000000000000, 0.9510565162951535312, 1.000000000000000000, 0.9510565162951535312, 1.000000000000000000, 0.9510565162951535312, 1.000000000000000000, 0.9510565162951535312, 1.000000000000000000, 0.9510565162951535312, 1.000000000000000000, 0.9510565162951535312, 1.000000000000000000, 0.9510565162951535312, 1.000000000000000000, 0.9510565162951535312, 1.000000000000000000, 0.9510565162951535312, 1.000000000000000000, 0.9510565162951535312, 1.000000000000000000, 0.9510565162951535312, 1.000000000000000000, 0.9510565162951535312, 1.000000000000000000, 0.9510565162951535312, 1.000000000000000000, 0.9510565162951535312, 1.000000000000000000, 0.9510565162951535312, 1.000000000000000000, 0.9510565162951535312, 1.000000000000000000, 0.9510565162951535312, 1.000000000000000000, 0.9510565162951535312, 1.000000000000000000, 0.9510565162951535312, 1.000000000000000000, 0.9510565162951535312, 1.000000000000000000, 0.9510565162951535312, 1.000000000000000000, 0.9510565162951535312, 1.000000000000000000, 0.9510565162951535312, 1.000000000000000000, 0.9510565162951535312, 1.000000000000000000, 0.9510565162951535312, 1.000000000000000000, 0.9510565162951535312, 1.000000000000000000, 0.9510565162951535312, 1.000000000000000000, 0.9510565162951535312, 1.000000000000000000, 0.9510565162951535312, 1.000000000000000000, 0.9510565162951535312, 1.000000000000000000, 0.9510565162951535312, 1.000000000000000000, 0.9510565162951535312, 1.000000000000000000, 0.9510565162951535312, 1.000000000000000000, 0.9510565162951535312, 1.000000000000000000, 0.9510565162951535312, 1.000000000000000000, 0.9510565162951535312, 1.000000000000000000, 0.9510565162951535312, 1.000000000000000000, 0.9510565162951535312, 1.000000000000000000, 0.9510565162951535312, 1.000000000000000000, 0.9510565162951535312, 1.000000000000000000, 0.9510565162951535312, 1.000000000000000000, 0.9510565162951535312, 1.000000000000000000, 0.9510565162951535312, 1.000000000000000000, 0.9510565162951535312, 1.000000000000000000, 0.9510565162951535312, 1.000000000000000000, 0.9510565162951535312, 1.000000000000000000, 0.9510565162951535312, 1.000000000000000000, 0.9510565162951535312, 1.000000000000000000, 0.9510565162951535312, 1.000000000000000000, 0.9510565162951535312, 1.000000000000000000, 0.9510565162951535312, 1.000000000000000000, 0.9510565162951535312, 1.000000000000000000, 0.9510565162951535312, 1.000000000000000000, 0.9510565162951535312, 1.000000000000000000, 0.9510565162951535312, 1.000000000000000000, 0.9510565162951535312, 1.000000000000000000, 0.9510565162951535312, 1.000000000000000000, 0.9907953663347257578, 0.9850529006435514434 ) ) 
 REPRESENTATION_ITEM ( '' )  );
#28500 = COLOUR_RGB ( '', 0.66274510, 0.83137255, 0.94901961) ;
#28501 = ORIENTED_EDGE ( 'NONE', *, *, #20500, .T. ) ;
#28502 = CIRCLE ( 'NONE', #47728, 1.999999999999998224 ) ;
#28503 = SURFACE_SIDE_STYLE ('',( #66510 ) ) ;
#28505 = EDGE_CURVE ( 'NONE', #60023, #50403, #53394, .T. ) ;
#28504 = CARTESIAN_POINT ( 'NONE',  ( -1.166476076187854022E-15, 127.0549999999999784, 9.525000000000000355 ) ) ;
#28506 = CARTESIAN_POINT ( 'NONE',  ( -53.90499999999997272, 2.607480562269069324, -8.024999999999993250 ) ) ;
#28507 = CARTESIAN_POINT ( 'NONE',  ( 40.99999999999998579, 108.0041655821620026, -3.000000000000000888 ) ) ;
#28508 = ORIENTED_EDGE ( 'NONE', *, *, #18883, .T. ) ;
#28509 = CARTESIAN_POINT ( 'NONE',  ( 5.598654528085805993, 157.3549999999999898, 7.705886871421374629 ) ) ;
#28510 = DIRECTION ( 'NONE',  ( -0.000000000000000000, -0.000000000000000000, -1.000000000000000000 ) ) ;
#28511 = UNCERTAINTY_MEASURE_WITH_UNIT (LENGTH_MEASURE( 1.000000000000000082E-05 ), #38764, 'distance_accuracy_value', 'NONE');
#28512 = CARTESIAN_POINT ( 'NONE',  ( -4.041451884327381450, 7.000000000000006217, 1.082903768654761345 ) ) ;
#28513 = EDGE_CURVE ( 'NONE', #19343, #24476, #42515, .T. ) ;
#28514 = STYLED_ITEM ( 'NONE', ( #65315 ), #62816 ) ;
#28515 = SURFACE_SIDE_STYLE ('',( #53875 ) ) ;
#28516 = CARTESIAN_POINT ( 'NONE',  ( 18.25000000000000711, 33.74999999999999289, -4.000000000000000000 ) ) ;
#28517 = VERTEX_POINT ( 'NONE', #9797 ) ;
#28518 =( NAMED_UNIT ( * ) PLANE_ANGLE_UNIT ( ) SI_UNIT ( $, .RADIAN. ) );
#28519 = EDGE_LOOP ( 'NONE', ( #52294, #50573, #12700, #7650 ) ) ;
#28520 = MECHANICAL_DESIGN_GEOMETRIC_PRESENTATION_REPRESENTATION (  '', ( #10580 ), #9538 ) ;
#28521 = STYLED_ITEM ( 'NONE', ( #16090 ), #61952 ) ;
#28522 = CARTESIAN_POINT ( 'NONE',  ( 6.062177826491068622, 2.500000000000000000, -3.500000000000001332 ) ) ;
#28523 = CARTESIAN_POINT ( 'NONE',  ( -195.0000000000000000, 0.000000000000000000, 9.524999999999991473 ) ) ;
#28524 = CARTESIAN_POINT ( 'NONE',  ( -164.6049999999999898, 6.826472737025113702, -4.959722759717902107 ) ) ;
#28525 = ORIENTED_EDGE ( 'NONE', *, *, #58427, .T. ) ;
#28526 = UNCERTAINTY_MEASURE_WITH_UNIT (LENGTH_MEASURE( 1.000000000000000082E-05 ), #3058, 'distance_accuracy_value', 'NONE');
#28527 =( NAMED_UNIT ( * ) PLANE_ANGLE_UNIT ( ) SI_UNIT ( $, .RADIAN. ) );
#28528 = CARTESIAN_POINT ( 'NONE',  ( 0.000000000000000000, 27.74999999999998934, 4.000000000000000000 ) ) ;
#28529 = DIRECTION ( 'NONE',  ( 0.000000000000000000, -0.000000000000000000, -1.000000000000000000 ) ) ;
#28530 = EDGE_LOOP ( 'NONE', ( #12660, #60207, #56641, #282 ) ) ;
#28531 = VERTEX_POINT ( 'NONE', #4468 ) ;
#28532 = LINE ( 'NONE', #49012, #34997 ) ;
#28533 = DIRECTION ( 'NONE',  ( 1.000000000000000000, 0.000000000000000000, 0.000000000000000000 ) ) ;
#28534 = CARTESIAN_POINT ( 'NONE',  ( -88.10499999999998977, -6.826472737025115478, 4.959722759717900331 ) ) ;
#28536 = ORIENTED_EDGE ( 'NONE', *, *, #57118, .T. ) ;
#28535 = COLOUR_RGB ( '', 0.66274510, 0.83137255, 0.94901961) ;
#28537 = FILL_AREA_STYLE ('',( #2095 ) ) ;
#28538 = CIRCLE ( 'NONE', #6062, 1.000000000000001554 ) ;
#28539 = CARTESIAN_POINT ( 'NONE',  ( -74.99999999999998579, 50.00000000000000000, -9.500000000000001776 ) ) ;
#28540 = MECHANICAL_DESIGN_GEOMETRIC_PRESENTATION_REPRESENTATION (  '', ( #1536 ), #60034 ) ;
#28541 = PRESENTATION_LAYER_ASSIGNMENT (  '', '', ( #3820 ) ) ;
#28542 = CYLINDRICAL_SURFACE ( 'NONE', #63839, 4.999999999999997335 ) ;
#28543 = CIRCLE ( 'NONE', #56690, 0.5000000000000004441 ) ;
#28544 = ORIENTED_EDGE ( 'NONE', *, *, #19773, .F. ) ;
#28545 = FILL_AREA_STYLE_COLOUR ( '', #11197 ) ;
#28546 = CARTESIAN_POINT ( 'NONE',  ( 3.094860106618431583, 129.0949999999999704, 9.525000000000000355 ) ) ;
#28547 = CARTESIAN_POINT ( 'NONE',  ( -108.1449999999999960, -4.716976649647092401, 6.492361379858946790 ) ) ;
#28548 = PRESENTATION_LAYER_ASSIGNMENT (  '', '', ( #20753 ) ) ;
#28549 =( LENGTH_UNIT ( ) NAMED_UNIT ( * ) SI_UNIT ( .MILLI., .METRE. ) );
#28550 = MECHANICAL_DESIGN_GEOMETRIC_PRESENTATION_REPRESENTATION (  '', ( #49938 ), #48857 ) ;
#28551 = CARTESIAN_POINT ( 'NONE',  ( -154.4929263765338305, -8.102448949553172852, 5.886773742842742685 ) ) ;
#28552 = PRESENTATION_STYLE_ASSIGNMENT (( #6416 ) ) ;
#28553 = CARTESIAN_POINT ( 'NONE',  ( -163.3449999999999989, 7.632228543268599452, -2.479861379858951942 ) ) ;
#28554 = PRESENTATION_LAYER_ASSIGNMENT (  '', '', ( #51040 ) ) ;
#28555 = DIRECTION ( 'NONE',  ( 0.000000000000000000, 1.000000000000000000, 0.000000000000000000 ) ) ;
#28556 = ADVANCED_FACE ( 'NONE', ( #48141 ), #125, .T. ) ;
#28557 = CONICAL_SURFACE ( 'NONE', #52220, 9.000000000000000000, 0.7853981633974500554 ) ;
#28558 =( LENGTH_UNIT ( ) NAMED_UNIT ( * ) SI_UNIT ( .MILLI., .METRE. ) );
#28559 = VERTEX_POINT ( 'NONE', #47463 ) ;
#28560 = SURFACE_STYLE_USAGE ( .BOTH. , #7131 ) ;
#28561 = ORIENTED_EDGE ( 'NONE', *, *, #55032, .T. ) ;
#28562 = CARTESIAN_POINT ( 'NONE',  ( -66.74292637653380211, -5.598654528085803328, -7.705886871421366635 ) ) ;
#28564 = ADVANCED_FACE ( 'NONE', ( #20686 ), #42195, .T. ) ;
#28563 = DIRECTION ( 'NONE',  ( 0.000000000000000000, 0.000000000000000000, 1.000000000000000000 ) ) ;
#28565 = ADVANCED_FACE ( 'NONE', ( #63587 ), #15430, .T. ) ;
#28566 = CARTESIAN_POINT ( 'NONE',  ( 31.00000000000000711, 15.00000000000000000, -34.49999999999999289 ) ) ;
#28567 =( NAMED_UNIT ( * ) PLANE_ANGLE_UNIT ( ) SI_UNIT ( $, .RADIAN. ) );
#28568 = CARTESIAN_POINT ( 'NONE',  ( 44.81371295029482837, 9.999999999999978684, -3.255911637198365405 ) ) ;
#28569 = EDGE_CURVE ( 'NONE', #6428, #45911, #15769, .T. ) ;
#28570 = LINE ( 'NONE', #60580, #47717 ) ;
#28571 = ORIENTED_EDGE ( 'NONE', *, *, #27852, .T. ) ;
#28572 = CARTESIAN_POINT ( 'NONE',  ( -167.0049999999999670, 6.826472737025115478, 4.959722759717899443 ) ) ;
#28573 = CIRCLE ( 'NONE', #32016, 0.2500000000000002220 ) ;
#28574 = ADVANCED_FACE ( 'NONE', ( #53044 ), #27143, .T. ) ;
#28575 = ORIENTED_EDGE ( 'NONE', *, *, #8766, .F. ) ;
#28576 = FACE_OUTER_BOUND ( 'NONE', #16984, .T. ) ;
#28577 = SURFACE_SIDE_STYLE ('',( #17035 ) ) ;
#28578 = EDGE_CURVE ( 'NONE', #68565, #65809, #55092, .T. ) ;
#28579 = CIRCLE ( 'NONE', #5002, 0.5000000000000000000 ) ;
#28580 = EDGE_CURVE ( 'NONE', #44927, #12184, #56052, .T. ) ;
#28581 = CARTESIAN_POINT ( 'NONE',  ( 2.607480562269076430, 153.9070736234662036, -8.025000000000000355 ) ) ;
#28582 = ORIENTED_EDGE ( 'NONE', *, *, #61769, .T. ) ;
#28583 = DIRECTION ( 'NONE',  ( 0.000000000000000000, 0.000000000000000000, 1.000000000000000000 ) ) ;
#28585 = EDGE_CURVE ( 'NONE', #24967, #10181, #23796, .T. ) ;
#28584 = SURFACE_SIDE_STYLE ('',( #38859 ) ) ;
#28586 = CARTESIAN_POINT ( 'NONE',  ( -85.70499999999998408, 2.607480562269072433, 8.024999999999991473 ) ) ;
#28587 = PRESENTATION_LAYER_ASSIGNMENT (  '', '', ( #31964 ) ) ;
#28588 = CARTESIAN_POINT ( 'NONE',  ( 0.000000000000000000, 0.000000000000000000, 0.2500000000000011102 ) ) ;
#28589 =( BOUNDED_CURVE ( )  B_SPLINE_CURVE ( 2, ( #28125, #22197, #32382, #16268, #44046, #37742, #59459, #64765, #11290, #16603, #54197 ),
 .UNSPECIFIED., .F., .F. ) 
 B_SPLINE_CURVE_WITH_KNOTS ( ( 3, 2, 2, 2, 2, 3 ),
 ( 0.4891304347825970456, 0.4913043478260752384, 0.4934782608695534312, 0.4956521739130317350, 0.4978260869565099278, 0.4999999999999881206 ),
 .UNSPECIFIED. ) 
 CURVE ( )  GEOMETRIC_REPRESENTATION_ITEM ( )  RATIONAL_B_SPLINE_CURVE ( ( 1.000000000000262457, 0.9510565162948910745, 1.000000000000000000, 0.9510565162951535312, 1.000000000000000000, 0.9510565162951535312, 1.000000000000000000, 0.9510565162951535312, 1.000000000000000000, 0.9510565162954209839, 0.9999999999997325473 ) ) 
 REPRESENTATION_ITEM ( '' )  );
#28590 = CARTESIAN_POINT ( 'NONE',  ( 5.598654528085809545, 128.2549999999999670, -7.705886871421373741 ) ) ;
#28591 = UNCERTAINTY_MEASURE_WITH_UNIT (LENGTH_MEASURE( 1.000000000000000082E-05 ), #22298, 'distance_accuracy_value', 'NONE');
#28592 = SURFACE_STYLE_FILL_AREA ( #7162 ) ;
#28593 = CARTESIAN_POINT ( 'NONE',  ( -169.1929263765338476, -10.01517768586948698, 6.132527647946031529E-16 ) ) ;
#28594 = DIRECTION ( 'NONE',  ( 0.000000000000000000, 0.000000000000000000, -1.000000000000000000 ) ) ;
#28595 = CARTESIAN_POINT ( 'NONE',  ( 44.99999999999977973, 146.4999999999999716, -7.000000000000000000 ) ) ;
#28596 = ORIENTED_EDGE ( 'NONE', *, *, #1046, .T. ) ;
#28597 = LINE ( 'NONE', #44160, #24935 ) ;
#28598 =( NAMED_UNIT ( * ) SI_UNIT ( $, .STERADIAN. ) SOLID_ANGLE_UNIT ( ) );
#28599 = CARTESIAN_POINT ( 'NONE',  ( -61.64499999999998892, 4.716976649647091513, -6.492361379858946790 ) ) ;
#28600 = ORIENTED_EDGE ( 'NONE', *, *, #65212, .F. ) ;
#28601 = DIRECTION ( 'NONE',  ( 9.376883653928687363E-17, -1.000000000000000000, 0.000000000000000000 ) ) ;
#28602 =( GEOMETRIC_REPRESENTATION_CONTEXT ( 3 ) GLOBAL_UNCERTAINTY_ASSIGNED_CONTEXT ( ( #3206 ) ) GLOBAL_UNIT_ASSIGNED_CONTEXT ( ( #54167, #65059, #6324 ) ) REPRESENTATION_CONTEXT ( 'NONE', 'WORKASPACE' ) );
#28603 = PRESENTATION_LAYER_ASSIGNMENT (  '', '', ( #6178 ) ) ;
#28604 = CARTESIAN_POINT ( 'NONE',  ( -48.59292637653380353, -3.094860106618431139, -9.524999999999991473 ) ) ;
#28605 = CARTESIAN_POINT ( 'NONE',  ( -139.5570736234661808, -1.166476076187852838E-15, -9.524999999999991473 ) ) ;
#28606 = FILL_AREA_STYLE_COLOUR ( '', #10477 ) ;
#28607 = ORIENTED_EDGE ( 'NONE', *, *, #55188, .T. ) ;
#28608 = CARTESIAN_POINT ( 'NONE',  ( -48.30000751666425174, -13.25410963537987286, 0.9681788673137204926 ) ) ;
#28609 = CARTESIAN_POINT ( 'NONE',  ( -50.24499999999998323, -4.716976649647093289, -6.492361379858945902 ) ) ;
#28610 = ORIENTED_EDGE ( 'NONE', *, *, #35017, .F. ) ;
#28611 = DIRECTION ( 'NONE',  ( 0.5000000000000001110, 0.8660254037844385966, 0.000000000000000000 ) ) ;
#28612 = CARTESIAN_POINT ( 'NONE',  ( -114.8049999999999926, -8.437984349512085203, 5.166775262442717831E-16 ) ) ;
#28613 = ORIENTED_EDGE ( 'NONE', *, *, #46520, .T. ) ;
#28614 = PRESENTATION_STYLE_ASSIGNMENT (( #12795 ) ) ;
#28615 = FILL_AREA_STYLE_COLOUR ( '', #2696 ) ;
#28616 = SURFACE_STYLE_FILL_AREA ( #12797 ) ;
#28617 = DIRECTION ( 'NONE',  ( -0.000000000000000000, -0.000000000000000000, -1.000000000000000000 ) ) ;
#28618 = AXIS2_PLACEMENT_3D ( 'NONE', #3017, #35084, #67100 ) ;
#28619 = CARTESIAN_POINT ( 'NONE',  ( -154.4070736234661467, 3.094860106618428031, -9.524999999999993250 ) ) ;
#28620 = STYLED_ITEM ( 'NONE', ( #13623 ), #5852 ) ;
#28621 =( BOUNDED_CURVE ( )  B_SPLINE_CURVE ( 2, ( #4902, #606, #65019, #38351, #53455, #16876, #59754, #17233, #11564, #27716, #60099 ),
 .UNSPECIFIED., .F., .F. ) 
 B_SPLINE_CURVE_WITH_KNOTS ( ( 3, 2, 2, 2, 2, 3 ),
 ( 0.4673913043478151175, 0.4695652173912933103, 0.4717391304347715031, 0.4739130434782496959, 0.4760869565217279442, 0.4782608695652061370 ),
 .UNSPECIFIED. ) 
 CURVE ( )  GEOMETRIC_REPRESENTATION_ITEM ( )  RATIONAL_B_SPLINE_CURVE ( ( 1.000000000000247358, 0.9510565162949060625, 1.000000000000000000, 0.9510565162951535312, 1.000000000000000000, 0.9510565162951535312, 1.000000000000000000, 0.9510565162951535312, 1.000000000000000000, 0.9510565162954072171, 0.9999999999997463140 ) ) 
 REPRESENTATION_ITEM ( '' )  );
#28622 = CARTESIAN_POINT ( 'NONE',  ( -59.60707362346616378, -8.102448949553174629, 5.886773742842742685 ) ) ;
#28623 = CARTESIAN_POINT ( 'NONE',  ( -8.102448949553179958, 137.4950000000000045, 5.886773742842747126 ) ) ;
#28624 = CARTESIAN_POINT ( 'NONE',  ( -87.80707362346616662, 10.01517768586948698, -1.839758294383808571E-15 ) ) ;
#28625 = EDGE_CURVE ( 'NONE', #5088, #44431, #50772, .T. ) ;
#28626 = CARTESIAN_POINT ( 'NONE',  ( -54.93556801395976663, -8.762778093175661809, -2.499999999999995559 ) ) ;
#28627 = VERTEX_POINT ( 'NONE', #46244 ) ;
#28628 = DIRECTION ( 'NONE',  ( -0.3420201433256663814, 0.9396926207859092051, -0.000000000000000000 ) ) ;
#28629 = VECTOR ( 'NONE', #60710, 1000.000000000000000 ) ;
#28631 = SPHERICAL_SURFACE ( 'NONE', #17842, 0.5000000000000000000 ) ;
#28630 = FILL_AREA_STYLE_COLOUR ( '', #16702 ) ;
#28632 = SURFACE_STYLE_FILL_AREA ( #12451 ) ;
#28633 = COLOUR_RGB ( '', 0.66274510, 0.83137255, 0.94901961) ;
#28634 = CARTESIAN_POINT ( 'NONE',  ( -127.7049999999999699, 2.607480562269073321, 8.024999999999991473 ) ) ;
#28635 = CARTESIAN_POINT ( 'NONE',  ( -164.5429263765338135, 9.058813317711329915, 2.943386871421369566 ) ) ;
#28636 = SURFACE_SIDE_STYLE ('',( #50128 ) ) ;
#28637 = CARTESIAN_POINT ( 'NONE',  ( -134.3949999999999250, -6.826472737025115478, -4.959722759717899443 ) ) ;
#28638 = CARTESIAN_POINT ( 'NONE',  ( -124.7949999999999733, 2.607480562269069324, -8.024999999999993250 ) ) ;
#28639 = DIRECTION ( 'NONE',  ( 1.000000000000000000, 0.000000000000000000, 0.000000000000000000 ) ) ;
#28640 = EDGE_LOOP ( 'NONE', ( #4536, #1649, #48968, #4882 ) ) ;
#28641 = AXIS2_PLACEMENT_3D ( 'NONE', #44489, #23323, #18739 ) ;
#28642 = DIRECTION ( 'NONE',  ( 0.000000000000000000, -1.000000000000000000, 0.000000000000000000 ) ) ;
#28643 = LINE ( 'NONE', #8603, #17081 ) ;
#28644 =( GEOMETRIC_REPRESENTATION_CONTEXT ( 3 ) GLOBAL_UNCERTAINTY_ASSIGNED_CONTEXT ( ( #3941 ) ) GLOBAL_UNIT_ASSIGNED_CONTEXT ( ( #17192, #38663, #18553 ) ) REPRESENTATION_CONTEXT ( 'NONE', 'WORKASPACE' ) );
#28645 = CARTESIAN_POINT ( 'NONE',  ( -180.2929263765338419, 3.094860106618428031, -9.524999999999993250 ) ) ;
#28646 = SURFACE_SIDE_STYLE ('',( #38577 ) ) ;
#28647 = CARTESIAN_POINT ( 'NONE',  ( -47.09499999999999886, -2.607480562269071545, -8.024999999999991473 ) ) ;
#28648 = EDGE_CURVE ( 'NONE', #17121, #51653, #29412, .T. ) ;
#28649 = CARTESIAN_POINT ( 'NONE',  ( 5.196152422706631135, 2.500000000000000000, 9.000000000000001776 ) ) ;
#28650 = LINE ( 'NONE', #44885, #21182 ) ;
#28651 = DIRECTION ( 'NONE',  ( -0.000000000000000000, 1.000000000000000000, -0.000000000000000000 ) ) ;
#28652 = CARTESIAN_POINT ( 'NONE',  ( -93.14292637653380780, 5.598654528085800663, -7.705886871421367523 ) ) ;
#28653 = APPLICATION_PROTOCOL_DEFINITION ( 'draft international standard', 'automotive_design', 1998, #39716 ) ;
#28655 = EDGE_CURVE ( 'NONE', #12255, #11851, #67639, .T. ) ;
#28654 =( LENGTH_UNIT ( ) NAMED_UNIT ( * ) SI_UNIT ( .MILLI., .METRE. ) );
#28656 = TOROIDAL_SURFACE ( 'NONE', #23063, 7.500000000000011546, 0.5000000000000000000 ) ;
#28657 = SURFACE_STYLE_FILL_AREA ( #12133 ) ;
#28658 = FILL_AREA_STYLE ('',( #17462 ) ) ;
#28659 = CARTESIAN_POINT ( 'NONE',  ( -41.61090298506120888, 107.5097581389847647, 4.000000003093457046 ) ) ;
#28660 = MECHANICAL_DESIGN_GEOMETRIC_PRESENTATION_REPRESENTATION (  '', ( #42203 ), #12953 ) ;
#28661 = FILL_AREA_STYLE_COLOUR ( '', #55151 ) ;
#28662 = ORIENTED_EDGE ( 'NONE', *, *, #52618, .F. ) ;
#28663 = ADVANCED_FACE ( 'NONE', ( #51151, #24386, #40253 ), #2898, .T. ) ;
#28664 = CARTESIAN_POINT ( 'NONE',  ( -57.33772693497696338, -7.785970543056433435, -0.9053205669554239554 ) ) ;
#28666 = ORIENTED_EDGE ( 'NONE', *, *, #47146, .F. ) ;
#28665 = VECTOR ( 'NONE', #48895, 1000.000000000000000 ) ;
#28667 = CARTESIAN_POINT ( 'NONE',  ( -195.0000000000000000, 0.000000000000000000, 0.000000000000000000 ) ) ;
#28668 = AXIS2_PLACEMENT_3D ( 'NONE', #48148, #32975, #43571 ) ;
#28669 = CARTESIAN_POINT ( 'NONE',  ( 7.632228543268607446, 120.1570736234661609, 2.479861379858954606 ) ) ;
#28671 = EDGE_CURVE ( 'NONE', #28083, #2689, #26052, .T. ) ;
#28670 =( NAMED_UNIT ( * ) SI_UNIT ( $, .STERADIAN. ) SOLID_ANGLE_UNIT ( ) );
#28672 = DIRECTION ( 'NONE',  ( -0.000000000000000000, -0.000000000000000000, 1.000000000000000000 ) ) ;
#28673 = VERTEX_POINT ( 'NONE', #13850 ) ;
#28674 = SURFACE_STYLE_FILL_AREA ( #17475 ) ;
#28675 = DIRECTION ( 'NONE',  ( 0.000000000000000000, 0.000000000000000000, -1.000000000000000000 ) ) ;
#28676 = ORIENTED_EDGE ( 'NONE', *, *, #42939, .T. ) ;
#28677 = DIRECTION ( 'NONE',  ( -1.000000000000000000, 0.000000000000000000, 0.000000000000000000 ) ) ;
#28678 = CARTESIAN_POINT ( 'NONE',  ( -45.00000000000000000, 9.708372675170618749, 6.000000000000000888 ) ) ;
#28679 = COLOUR_RGB ( '', 0.09019608, 0.27058824, 0.51372549) ;
#28680 = CARTESIAN_POINT ( 'NONE',  ( -58.75000000000000000, -13.99999999999999822, 18.10000000000000497 ) ) ;
#28681 = CARTESIAN_POINT ( 'NONE',  ( -91.49499999999997613, 6.826472737025113702, -4.959722759717902107 ) ) ;
#28682 = ORIENTED_EDGE ( 'NONE', *, *, #39344, .F. ) ;
#28683 = CIRCLE ( 'NONE', #37756, 0.5000000000000004441 ) ;
#28684 =( NAMED_UNIT ( * ) PLANE_ANGLE_UNIT ( ) SI_UNIT ( $, .RADIAN. ) );
#28685 = CARTESIAN_POINT ( 'NONE',  ( 45.54151037965569770, 9.791825115387426948, 6.500000000000000888 ) ) ;
#28686 = FILL_AREA_STYLE ('',( #44243 ) ) ;
#28687 = STYLED_ITEM ( 'NONE', ( #43847 ), #32306 ) ;
#28688 = ORIENTED_EDGE ( 'NONE', *, *, #60809, .T. ) ;
#28689 = FILL_AREA_STYLE ('',( #51547 ) ) ;
#28690 = FACE_OUTER_BOUND ( 'NONE', #48176, .T. ) ;
#28691 = CARTESIAN_POINT ( 'NONE',  ( 13.74999999999998757, -7.950815931560351124E-15, 3.750000000000000000 ) ) ;
#28692 = ORIENTED_EDGE ( 'NONE', *, *, #4425, .T. ) ;
#28693 = DIRECTION ( 'NONE',  ( 1.300977106640434891E-16, -0.000000000000000000, 1.000000000000000000 ) ) ;
#28694 = ORIENTED_EDGE ( 'NONE', *, *, #32371, .F. ) ;
#28695 =( NAMED_UNIT ( * ) PLANE_ANGLE_UNIT ( ) SI_UNIT ( $, .RADIAN. ) );
#28696 = DIRECTION ( 'NONE',  ( 1.000000000000000000, 0.000000000000000000, 0.000000000000000000 ) ) ;
#28697 = CARTESIAN_POINT ( 'NONE',  ( -23.21231517720797655, 117.9999999999999716, 7.500000000000000000 ) ) ;
#28698 = CARTESIAN_POINT ( 'NONE',  ( -178.4070736234662036, 3.094860106618428031, -9.524999999999993250 ) ) ;
#28699 = LINE ( 'NONE', #33645, #28629 ) ;
#28700 = CARTESIAN_POINT ( 'NONE',  ( 1.804495846578303864, 51.08602766979955589, -2.000000000000000000 ) ) ;
#28701 = CARTESIAN_POINT ( 'NONE',  ( -109.2570736234661837, 5.598654528085800663, -7.705886871421367523 ) ) ;
#28702 = EDGE_CURVE ( 'NONE', #13649, #64044, #35047, .T. ) ;
#28703 = TOROIDAL_SURFACE ( 'NONE', #32140, 18.50000000000000355, 0.5000000000000000000 ) ;
#28704 = DIRECTION ( 'NONE',  ( -1.000000000000000000, -0.000000000000000000, -0.000000000000000000 ) ) ;
#28705 = CARTESIAN_POINT ( 'NONE',  ( -85.55707362346618083, -1.166476076187852838E-15, -9.524999999999991473 ) ) ;
#28706 = EDGE_LOOP ( 'NONE', ( #5193, #63478, #45032, #42707 ) ) ;
#28707 = EDGE_CURVE ( 'NONE', #20368, #12157, #28330, .T. ) ;
#28708 = CARTESIAN_POINT ( 'NONE',  ( 6.898093598910793212, -2.361802048420730049, -6.052151411320861207 ) ) ;
#28709 =( LENGTH_UNIT ( ) NAMED_UNIT ( * ) SI_UNIT ( .MILLI., .METRE. ) );
#28711 = LINE ( 'NONE', #66352, #45597 ) ;
#28710 = AXIS2_PLACEMENT_3D ( 'NONE', #62872, #23868, #35478 ) ;
#28712 = ORIENTED_EDGE ( 'NONE', *, *, #65025, .F. ) ;
#28713 = CARTESIAN_POINT ( 'NONE',  ( -159.2050000000000125, -2.607480562269071545, -8.024999999999991473 ) ) ;
#28714 = LINE ( 'NONE', #50546, #29685 ) ;
#28715 = CARTESIAN_POINT ( 'NONE',  ( -183.5367403587429180, -4.194181754694801256, -7.955897757997197672 ) ) ;
#28716 = CARTESIAN_POINT ( 'NONE',  ( -161.3950000000000102, -6.826472737025115478, -4.959722759717899443 ) ) ;
#28717 = CIRCLE ( 'NONE', #17519, 1.000000000000000000 ) ;
#28718 = AXIS2_PLACEMENT_3D ( 'NONE', #44655, #61122, #22818 ) ;
#28719 = CARTESIAN_POINT ( 'NONE',  ( -155.3950000000000102, -6.826472737025113702, -4.959722759717900331 ) ) ;
#28720 = VERTEX_POINT ( 'NONE', #24055 ) ;
#28721 = FACE_OUTER_BOUND ( 'NONE', #27996, .T. ) ;
#28722 = LINE ( 'NONE', #6243, #13236 ) ;
#28723 = CARTESIAN_POINT ( 'NONE',  ( -71.15499999999998693, 7.632228543268600340, 2.479861379858949277 ) ) ;
#28724 = LINE ( 'NONE', #39329, #19126 ) ;
#28725 = DIRECTION ( 'NONE',  ( 0.000000000000000000, 0.000000000000000000, 1.000000000000000000 ) ) ;
#28726 = EDGE_CURVE ( 'NONE', #23486, #18241, #7194, .T. ) ;
#28727 = AXIS2_PLACEMENT_3D ( 'NONE', #22913, #22206, #43703 ) ;
#28728 = CARTESIAN_POINT ( 'NONE',  ( -74.84499999999998465, -7.632228543268599452, 2.479861379858951054 ) ) ;
#28729 = EDGE_CURVE ( 'NONE', #35530, #57014, #45883, .T. ) ;
#28730 = CARTESIAN_POINT ( 'NONE',  ( -9.058813317711338797, 150.4550000000000125, 2.943386871421373563 ) ) ;
#28731 = CARTESIAN_POINT ( 'NONE',  ( -75.00000000000000000, 7.768687147774684831, 6.999999999999999112 ) ) ;
#28732 = MECHANICAL_DESIGN_GEOMETRIC_PRESENTATION_REPRESENTATION (  '', ( #23141 ), #68087 ) ;
#28733 = AXIS2_PLACEMENT_3D ( 'NONE', #23276, #44773, #13398 ) ;
#28734 = FILL_AREA_STYLE_COLOUR ( '', #3443 ) ;
#28735 = STYLED_ITEM ( 'NONE', ( #55147 ), #57156 ) ;
#28736 = DIRECTION ( 'NONE',  ( -0.000000000000000000, -1.000000000000000000, 0.000000000000000000 ) ) ;
#28737 = EDGE_CURVE ( 'NONE', #40140, #67406, #34267, .T. ) ;
#28738 = DIRECTION ( 'NONE',  ( -0.000000000000000000, -1.000000000000000000, -0.000000000000000000 ) ) ;
#28739 = EDGE_CURVE ( 'NONE', #56203, #1355, #61655, .T. ) ;
#28740 = CARTESIAN_POINT ( 'NONE',  ( -20.12916642283592950, 110.4999999999999858, 10.05319148936170137 ) ) ;
#28741 = DIRECTION ( 'NONE',  ( -1.000000000000000000, 0.000000000000000000, 0.000000000000000000 ) ) ;
#28742 = ADVANCED_FACE ( 'NONE', ( #66627 ), #34957, .T. ) ;
#28743 = FILL_AREA_STYLE_COLOUR ( '', #28301 ) ;
#28744 = ORIENTED_EDGE ( 'NONE', *, *, #17429, .F. ) ;
#28745 = ORIENTED_EDGE ( 'NONE', *, *, #19213, .T. ) ;
#28746 = CARTESIAN_POINT ( 'NONE',  ( 12.50000000000000533, 27.99999999999998224, 3.750000000000000000 ) ) ;
#28747 = AXIS2_PLACEMENT_3D ( 'NONE', #44186, #23365, #65585 ) ;
#28748 = ADVANCED_FACE ( 'NONE', ( #40967 ), #15277, .T. ) ;
#28749 = LINE ( 'NONE', #35783, #61942 ) ;
#28750 =( NAMED_UNIT ( * ) PLANE_ANGLE_UNIT ( ) SI_UNIT ( $, .RADIAN. ) );
#28751 = FACE_OUTER_BOUND ( 'NONE', #47605, .T. ) ;
#28752 = SURFACE_SIDE_STYLE ('',( #24177 ) ) ;
#28753 = ORIENTED_EDGE ( 'NONE', *, *, #38726, .T. ) ;
#28754 = CARTESIAN_POINT ( 'NONE',  ( -102.6549999999999869, -7.632228543268600340, -2.479861379858950166 ) ) ;
#28755 = ORIENTED_EDGE ( 'NONE', *, *, #61840, .T. ) ;
#28756 = VECTOR ( 'NONE', #18912, 1000.000000000000000 ) ;
#28757 = CARTESIAN_POINT ( 'NONE',  ( 68.99999999999998579, 1.000000000000008438, -3.000000000000000000 ) ) ;
#28758 = FACE_OUTER_BOUND ( 'NONE', #22552, .T. ) ;
#28759 = ORIENTED_EDGE ( 'NONE', *, *, #25278, .T. ) ;
#28760 = DIRECTION ( 'NONE',  ( -0.000000000000000000, 1.000000000000000000, -0.000000000000000000 ) ) ;
#28761 = ORIENTED_EDGE ( 'NONE', *, *, #27930, .T. ) ;
#28762 = ADVANCED_BREP_SHAPE_REPRESENTATION ( '', ( #50950, #42840 ), #7944 ) ;
#28763 = MECHANICAL_DESIGN_GEOMETRIC_PRESENTATION_REPRESENTATION (  '', ( #7404 ), #50145 ) ;
#28764 = CARTESIAN_POINT ( 'NONE',  ( 29.00000000000000000, 34.36176364315826248, -80.00402776293826435 ) ) ;
#28765 = SURFACE_STYLE_FILL_AREA ( #45000 ) ;
#28766 = ORIENTED_EDGE ( 'NONE', *, *, #45899, .F. ) ;
#28767 = ORIENTED_EDGE ( 'NONE', *, *, #39932, .F. ) ;
#28768 = CARTESIAN_POINT ( 'NONE',  ( -74.50000000000000000, 7.768687147774688384, -6.500000000000000000 ) ) ;
#28769 = DIRECTION ( 'NONE',  ( -1.000000000000000000, 0.000000000000000000, 0.000000000000000000 ) ) ;
#28770 = DIRECTION ( 'NONE',  ( 0.000000000000000000, 1.000000000000000000, 0.000000000000000000 ) ) ;
#28771 = ORIENTED_EDGE ( 'NONE', *, *, #3809, .F. ) ;
#28772 = CARTESIAN_POINT ( 'NONE',  ( 0.000000000000000000, 137.9429263765338192, -8.025000000000000355 ) ) ;
#28773 = CARTESIAN_POINT ( 'NONE',  ( 62.60000000000000142, 11.99999999999999822, 4.000000000000000000 ) ) ;
#28774 = CARTESIAN_POINT ( 'NONE',  ( 57.74999999999998579, 30.99999999999999289, -3.750000000000000000 ) ) ;
#28775 = CARTESIAN_POINT ( 'NONE',  ( -74.99999999999998579, 50.00000000000000000, 12.00000000000000000 ) ) ;
#28776 = VECTOR ( 'NONE', #6974, 1000.000000000000000 ) ;
#28777 = CARTESIAN_POINT ( 'NONE',  ( -2.607480562269048896, 115.2929263765338135, 8.025000000000019895 ) ) ;
#28778 = EDGE_LOOP ( 'NONE', ( #16467, #57576, #11053, #26084 ) ) ;
#28779 = FACE_OUTER_BOUND ( 'NONE', #62603, .T. ) ;
#28780 = ORIENTED_EDGE ( 'NONE', *, *, #11029, .T. ) ;
#28781 = DIRECTION ( 'NONE',  ( -1.000000000000000000, 0.000000000000000000, 0.000000000000000000 ) ) ;
#28782 =( GEOMETRIC_REPRESENTATION_CONTEXT ( 3 ) GLOBAL_UNCERTAINTY_ASSIGNED_CONTEXT ( ( #7941 ) ) GLOBAL_UNIT_ASSIGNED_CONTEXT ( ( #36733, #47991, #68018 ) ) REPRESENTATION_CONTEXT ( 'NONE', 'WORKASPACE' ) );
#28783 = DIRECTION ( 'NONE',  ( -1.000000000000000000, -5.782411586589351722E-16, 0.000000000000000000 ) ) ;
#28784 = CARTESIAN_POINT ( 'NONE',  ( 7.750000000000000000, 33.74999999999998579, -3.750000000000000000 ) ) ;
#28785 = CARTESIAN_POINT ( 'NONE',  ( -44.99999999999977973, 149.4999999999999716, -10.00000000000000000 ) ) ;
#28786 = CARTESIAN_POINT ( 'NONE',  ( -134.4549999999999841, 7.632228543268599452, -2.479861379858951942 ) ) ;
#28787 = FILL_AREA_STYLE_COLOUR ( '', #12850 ) ;
#28788 = FACE_OUTER_BOUND ( 'NONE', #17383, .T. ) ;
#28789 = ORIENTED_EDGE ( 'NONE', *, *, #871, .T. ) ;
#28790 = ADVANCED_FACE ( 'NONE', ( #42024 ), #25779, .F. ) ;
#28791 = CARTESIAN_POINT ( 'NONE',  ( -23.21231517720797655, 117.4999999999999716, -7.000000000000000000 ) ) ;
#28792 = PRESENTATION_STYLE_ASSIGNMENT (( #49941 ) ) ;
#28793 = VERTEX_POINT ( 'NONE', #52205 ) ;
#28794 = ORIENTED_EDGE ( 'NONE', *, *, #30441, .T. ) ;
#28795 = CARTESIAN_POINT ( 'NONE',  ( 66.49999999999998579, 34.24999999999999289, 4.000000000000000000 ) ) ;
#28796 = CARTESIAN_POINT ( 'NONE',  ( 45.00000000000000000, 99.99999999999992895, -4.000000000000000000 ) ) ;
#28797 = CARTESIAN_POINT ( 'NONE',  ( 1.000000000000000000, 0.9999999999999991118, -79.00402776293826435 ) ) ;
#28798 = CARTESIAN_POINT ( 'NONE',  ( -51.65499999999997982, -7.632228543268600340, -2.479861379858950166 ) ) ;
#28799 = VERTEX_POINT ( 'NONE', #46952 ) ;
#28800 = CARTESIAN_POINT ( 'NONE',  ( -124.2570736234661837, 5.598654528085800663, -7.705886871421367523 ) ) ;
#28801 = CARTESIAN_POINT ( 'NONE',  ( -52.24999999999999289, 4.336808689942018722E-16, -5.099999999999999645 ) ) ;
#28802 = CARTESIAN_POINT ( 'NONE',  ( -195.0000000000000000, 0.000000000000000000, 0.000000000000000000 ) ) ;
#28803 =( NAMED_UNIT ( * ) SI_UNIT ( $, .STERADIAN. ) SOLID_ANGLE_UNIT ( ) );
#28804 = SURFACE_STYLE_USAGE ( .BOTH. , #13318 ) ;
#28805 = EDGE_LOOP ( 'NONE', ( #25136, #10337, #25897, #12894, #66697, #48738 ) ) ;
#28806 = CARTESIAN_POINT ( 'NONE',  ( 0.000000000000000000, 137.9429263765338192, -8.025000000000000355 ) ) ;
#28807 = ADVANCED_FACE ( 'NONE', ( #68362 ), #37419, .T. ) ;
#28808 = CARTESIAN_POINT ( 'NONE',  ( -144.2070736234666697, 3.094860106626365237, 9.524999999994228972 ) ) ;
#28809 = DIRECTION ( 'NONE',  ( -0.000000000000000000, -0.000000000000000000, 1.000000000000000000 ) ) ;
#28810 = CARTESIAN_POINT ( 'NONE',  ( -29.83276705773152315, -8.499999999999996447, 0.3716419282406659419 ) ) ;
#28811 = CARTESIAN_POINT ( 'NONE',  ( 0.000000000000000000, 0.000000000000000000, 1.000000000000000000 ) ) ;
#28812 = EDGE_CURVE ( 'NONE', #30560, #16813, #21010, .T. ) ;
#28813 = PRESENTATION_LAYER_ASSIGNMENT (  '', '', ( #36762 ) ) ;
#28814 = EDGE_CURVE ( 'NONE', #9058, #65770, #46381, .T. ) ;
#28815 = CARTESIAN_POINT ( 'NONE',  ( -102.2949999999999733, -2.607480562269069768, 8.024999999999991473 ) ) ;
#28816 = ADVANCED_FACE ( 'NONE', ( #16312 ), #1342, .F. ) ;
#28817 = CARTESIAN_POINT ( 'NONE',  ( -5.598654528085806881, 116.8549999999999898, -7.705886871421374629 ) ) ;
#28818 = MECHANICAL_DESIGN_GEOMETRIC_PRESENTATION_REPRESENTATION (  '', ( #35584 ), #56900 ) ;
#28819 = CARTESIAN_POINT ( 'NONE',  ( -75.44499999999997897, 0.000000000000000000, 8.024999999999991473 ) ) ;
#28820 = CIRCLE ( 'NONE', #29943, 0.2500000000000002220 ) ;
#28821 = CARTESIAN_POINT ( 'NONE',  ( 3.249999999999998668, 36.74999999999999289, 3.750000000000000000 ) ) ;
#28822 =( NAMED_UNIT ( * ) PLANE_ANGLE_UNIT ( ) SI_UNIT ( $, .RADIAN. ) );
#28823 = CARTESIAN_POINT ( 'NONE',  ( 48.74999999999999289, 24.99999999999998579, -3.750000000000000000 ) ) ;
#28824 = FACE_OUTER_BOUND ( 'NONE', #66688, .T. ) ;
#28825 =( NAMED_UNIT ( * ) SI_UNIT ( $, .STERADIAN. ) SOLID_ANGLE_UNIT ( ) );
#28826 = ORIENTED_EDGE ( 'NONE', *, *, #56619, .F. ) ;
#28827 = CARTESIAN_POINT ( 'NONE',  ( -116.2429263765338021, 5.598654528085804216, 7.705886871421366635 ) ) ;
#28828 = CARTESIAN_POINT ( 'NONE',  ( -137.6949999999999932, -8.437984349512085203, 5.166775262442717831E-16 ) ) ;
#28829 = ADVANCED_FACE ( 'NONE', ( #37791 ), #28174, .F. ) ;
#28830 = AXIS2_PLACEMENT_3D ( 'NONE', #56462, #28677, #34325 ) ;
#28831 = SURFACE_SIDE_STYLE ('',( #7730 ) ) ;
#28832 = DIRECTION ( 'NONE',  ( -1.000000000000000000, 0.000000000000000000, 0.000000000000000000 ) ) ;
#28833 = ORIENTED_EDGE ( 'NONE', *, *, #39354, .F. ) ;
#28834 = ORIENTED_EDGE ( 'NONE', *, *, #42401, .F. ) ;
#28835 = CARTESIAN_POINT ( 'NONE',  ( -29.91370621994235890, -7.761720733523295834, -0.7755720678495816589 ) ) ;
#28836 = DIRECTION ( 'NONE',  ( -0.000000000000000000, -0.000000000000000000, 1.000000000000000000 ) ) ;
#28837 = DIRECTION ( 'NONE',  ( 0.000000000000000000, 0.000000000000000000, -1.000000000000000000 ) ) ;
#28838 = DIRECTION ( 'NONE',  ( -1.000000000000000000, 0.000000000000000000, 0.000000000000000000 ) ) ;
#28839 = DIRECTION ( 'NONE',  ( 0.000000000000000000, -0.000000000000000000, -1.000000000000000000 ) ) ;
#28840 = PRESENTATION_STYLE_ASSIGNMENT (( #60853 ) ) ;
#28841 = ORIENTED_EDGE ( 'NONE', *, *, #4618, .T. ) ;
#28842 = CARTESIAN_POINT ( 'NONE',  ( -132.5049999999999955, -6.826472737025113702, -4.959722759717900331 ) ) ;
#28843 = ORIENTED_EDGE ( 'NONE', *, *, #42284, .F. ) ;
#28844 = ADVANCED_FACE ( 'NONE', ( #48325 ), #38478, .T. ) ;
#28845 = VERTEX_POINT ( 'NONE', #27499 ) ;
#28846 = SURFACE_STYLE_USAGE ( .BOTH. , #48983 ) ;
#28847 = ORIENTED_EDGE ( 'NONE', *, *, #15594, .F. ) ;
#28848 = DIRECTION ( 'NONE',  ( 1.000000000000000000, 0.000000000000000000, 0.000000000000000000 ) ) ;
#28849 = ADVANCED_FACE ( 'NONE', ( #64468 ), #32432, .F. ) ;
#28850 = CARTESIAN_POINT ( 'NONE',  ( -23.21231517720797655, 117.4999999999999716, 7.500000000000000000 ) ) ;
#28851 = CARTESIAN_POINT ( 'NONE',  ( 5.598654528085805993, 138.2449999999999761, 7.705886871421374629 ) ) ;
#28852 = ORIENTED_EDGE ( 'NONE', *, *, #43574, .F. ) ;
#28853 = CARTESIAN_POINT ( 'NONE',  ( -44.99999999999977973, 149.9999999999999716, 9.500000000000000000 ) ) ;
#28854 = CARTESIAN_POINT ( 'NONE',  ( 9.058813317711338797, 142.9550000000000125, -2.943386871421372675 ) ) ;
#28855 = CARTESIAN_POINT ( 'NONE',  ( -59.00499999999998124, 6.826472737025115478, 4.959722759717899443 ) ) ;
#28856 = CARTESIAN_POINT ( 'NONE',  ( 41.49999999999997868, 106.9282032302754999, -3.500000000000000888 ) ) ;
#28857 = PRODUCT_DEFINITION_SHAPE ( 'NONE', 'NONE',  #69697 ) ;
#28858 = ORIENTED_EDGE ( 'NONE', *, *, #20834, .T. ) ;
#28859 = CARTESIAN_POINT ( 'NONE',  ( 5.598654528085805993, 154.3549999999999898, 7.705886871421374629 ) ) ;
#28860 = LINE ( 'NONE', #38452, #4105 ) ;
#28861 = SURFACE_STYLE_USAGE ( .BOTH. , #7440 ) ;
#28862 = FACE_OUTER_BOUND ( 'NONE', #9354, .T. ) ;
#28863 = AXIS2_PLACEMENT_3D ( 'NONE', #23093, #23411, #33630 ) ;
#28864 = ORIENTED_EDGE ( 'NONE', *, *, #31773, .T. ) ;
#28865 = AXIS2_PLACEMENT_3D ( 'NONE', #38265, #22386, #17144 ) ;
#28866 = EDGE_LOOP ( 'NONE', ( #62712, #22152, #24612 ) ) ;
#28867 = CARTESIAN_POINT ( 'NONE',  ( -28.74999999999999645, -8.499999999999996447, 18.10000000000000497 ) ) ;
#28868 = CARTESIAN_POINT ( 'NONE',  ( 60.00000000000000000, 1.797044900979284448E-15, -6.500000000000000000 ) ) ;
#28869 = CARTESIAN_POINT ( 'NONE',  ( -50.39495521537276090, -10.76536571987046820, 3.807206309028079882 ) ) ;
#28870 = CARTESIAN_POINT ( 'NONE',  ( -165.9549999999999841, -7.632228543268599452, 2.479861379858951054 ) ) ;
#28871 = ORIENTED_EDGE ( 'NONE', *, *, #44225, .T. ) ;
#28872 = SURFACE_STYLE_USAGE ( .BOTH. , #56305 ) ;
#28873 = FILL_AREA_STYLE ('',( #54232 ) ) ;
#28874 = ORIENTED_EDGE ( 'NONE', *, *, #30441, .F. ) ;
#28875 = ORIENTED_EDGE ( 'NONE', *, *, #41104, .F. ) ;
#28876 = DIRECTION ( 'NONE',  ( 0.000000000000000000, -1.000000000000000000, 0.000000000000000000 ) ) ;
#28877 =( GEOMETRIC_REPRESENTATION_CONTEXT ( 3 ) GLOBAL_UNCERTAINTY_ASSIGNED_CONTEXT ( ( #20037 ) ) GLOBAL_UNIT_ASSIGNED_CONTEXT ( ( #52264, #25152, #46666 ) ) REPRESENTATION_CONTEXT ( 'NONE', 'WORKASPACE' ) );
#28878 = LINE ( 'NONE', #55279, #48181 ) ;
#28879 = CARTESIAN_POINT ( 'NONE',  ( -72.95499999999999829, -7.632228543268599452, 2.479861379858951054 ) ) ;
#28880 = ORIENTED_EDGE ( 'NONE', *, *, #578, .T. ) ;
#28881 = CARTESIAN_POINT ( 'NONE',  ( -75.75000000000000000, -0.9999999999999995559, 19.00000000000000000 ) ) ;
#28882 = ADVANCED_FACE ( 'NONE', ( #56319 ), #18284, .T. ) ;
#28883 = DIRECTION ( 'NONE',  ( 0.000000000000000000, 0.000000000000000000, 1.000000000000000000 ) ) ;
#28884 = SURFACE_STYLE_USAGE ( .BOTH. , #45129 ) ;
#28885 = APPLICATION_CONTEXT ( 'automotive_design' ) ;
#28886 = EDGE_CURVE ( 'NONE', #48195, #35826, #29519, .T. ) ;
#28887 = FILL_AREA_STYLE ('',( #18008 ) ) ;
#28888 = ORIENTED_EDGE ( 'NONE', *, *, #22578, .T. ) ;
#28889 = CARTESIAN_POINT ( 'NONE',  ( 3.409623619629272184, 7.000000000000006217, 0.7804846576204730324 ) ) ;
#28890 = CARTESIAN_POINT ( 'NONE',  ( -87.50000000000000000, -8.499999999999989342, 24.00000000000000000 ) ) ;
#28891 = EDGE_CURVE ( 'NONE', #62580, #5418, #62310, .T. ) ;
#28892 = CARTESIAN_POINT ( 'NONE',  ( 8.102448949553181734, 141.3949999999999818, 5.886773742842750679 ) ) ;
#28893 = CARTESIAN_POINT ( 'NONE',  ( -110.2449999999999903, -4.716976649647093289, -6.492361379858945902 ) ) ;
#28894 = CARTESIAN_POINT ( 'NONE',  ( -52.24999999999999289, 4.336808689942018722E-16, -5.099999999999999645 ) ) ;
#28896 = CARTESIAN_POINT ( 'NONE',  ( -17.22936139948035361, 11.13022047738569675, 4.487408569146854376 ) ) ;
#28895 = DIRECTION ( 'NONE',  ( -0.000000000000000000, -0.000000000000000000, 1.000000000000000000 ) ) ;
#28897 = CARTESIAN_POINT ( 'NONE',  ( -156.1429263765338078, 5.598654528085800663, -7.705886871421367523 ) ) ;
#28898 = CARTESIAN_POINT ( 'NONE',  ( -168.5949999999999989, 2.607480562269073321, 8.024999999999991473 ) ) ;
#28899 = AXIS2_PLACEMENT_3D ( 'NONE', #61147, #12955, #28060 ) ;
#28900 = AXIS2_PLACEMENT_3D ( 'NONE', #51658, #2726, #30519 ) ;
#28901 = EDGE_CURVE ( 'NONE', #19491, #29473, #45128, .T. ) ;
#28902 = COLOUR_RGB ( '', 0.72549020, 0.75294118, 0.79215686) ;
#28903 = DIRECTION ( 'NONE',  ( 0.000000000000000000, 0.000000000000000000, -1.000000000000000000 ) ) ;
#28904 = SURFACE_STYLE_USAGE ( .BOTH. , #56713 ) ;
#28905 = ORIENTED_EDGE ( 'NONE', *, *, #53850, .F. ) ;
#28906 = EDGE_LOOP ( 'NONE', ( #39967, #18319, #61852, #53223 ) ) ;
#28907 = CARTESIAN_POINT ( 'NONE',  ( -64.34292637653379643, -9.058813317711329915, 2.943386871421371787 ) ) ;
#28908 = CARTESIAN_POINT ( 'NONE',  ( 0.000000000000000000, 0.000000000000000000, 0.000000000000000000 ) ) ;
#28909 =( BOUNDED_SURFACE ( )  B_SPLINE_SURFACE ( 3, 2, ( 
 ( #53909, #17363, #60243 ),
 ( #65867, #1787, #37807 ),
 ( #17003, #5713, #43081 ),
 ( #38493, #48694, #33500 ) ),
 .UNSPECIFIED., .F., .F., .F. ) 
 B_SPLINE_SURFACE_WITH_KNOTS ( ( 4, 4 ),
 ( 3, 3 ),
 ( 1.868947704930512543E-15, 0.002371732043463299026 ),
 ( 0.000000000000000000, 1.000000000000000000 ),
 .UNSPECIFIED. ) 
 GEOMETRIC_REPRESENTATION_ITEM ( )  RATIONAL_B_SPLINE_SURFACE ( (
 ( 1.000000000000000000, 0.9473232638934960814, 1.000000000000000000),
 ( 1.000000000000000000, 0.9785952379402158563, 1.000000000000000000),
 ( 1.000000000000000000, 1.000279878396717725, 1.000000000000000000),
 ( 1.000000000000000000, 1.000000000000000000, 1.000000000000000000) ) ) 
 REPRESENTATION_ITEM ( '' )  SURFACE ( )  );
#28910 = FILL_AREA_STYLE ('',( #66934 ) ) ;
#28911 = CARTESIAN_POINT ( 'NONE',  ( -4.167402100491157668E-16, 42.24290439781417916, 74.85424052902104108 ) ) ;
#28912 = DIRECTION ( 'NONE',  ( -1.000000000000000000, 0.000000000000000000, 0.000000000000000000 ) ) ;
#28913 = COLOUR_RGB ( '', 0.31764706, 0.68627451, 0.89019608) ;
#28914 = CARTESIAN_POINT ( 'NONE',  ( 4.000000000000030198, 38.70020753820971748, 89.00000000000000000 ) ) ;
#28915 =( GEOMETRIC_REPRESENTATION_CONTEXT ( 3 ) GLOBAL_UNCERTAINTY_ASSIGNED_CONTEXT ( ( #20763 ) ) GLOBAL_UNIT_ASSIGNED_CONTEXT ( ( #3119, #41204, #64706 ) ) REPRESENTATION_CONTEXT ( 'NONE', 'WORKASPACE' ) );
#28916 = ORIENTED_EDGE ( 'NONE', *, *, #26488, .T. ) ;
#28917 = CARTESIAN_POINT ( 'NONE',  ( -168.3550000000000182, -4.716976649647093289, -6.492361379858945902 ) ) ;
#28918 = ORIENTED_EDGE ( 'NONE', *, *, #30975, .T. ) ;
#28919 = CARTESIAN_POINT ( 'NONE',  ( -111.5929263765347059, -3.094860106633758434, -9.524999999988855492 ) ) ;
#28920 =( NAMED_UNIT ( * ) SI_UNIT ( $, .STERADIAN. ) SOLID_ANGLE_UNIT ( ) );
#28921 = SURFACE_STYLE_FILL_AREA ( #13103 ) ;
#28922 = SURFACE_STYLE_FILL_AREA ( #61296 ) ;
#28923 = CARTESIAN_POINT ( 'NONE',  ( -7.632228543268607446, 151.6570736234661751, -2.479861379858953718 ) ) ;
#28924 = ORIENTED_EDGE ( 'NONE', *, *, #48042, .F. ) ;
#28925 = FACE_OUTER_BOUND ( 'NONE', #15474, .T. ) ;
#28926 = CARTESIAN_POINT ( 'NONE',  ( 3.094860106618435136, 113.4049999999999869, -9.525000000000000355 ) ) ;
#28927 = CARTESIAN_POINT ( 'NONE',  ( -85.55499999999999261, 0.000000000000000000, 8.024999999999991473 ) ) ;
#28928 = SPHERICAL_SURFACE ( 'NONE', #50001, 0.2500000000000000000 ) ;
#28929 = CARTESIAN_POINT ( 'NONE',  ( -1.166476076187854022E-15, 133.0549999999999784, 9.525000000000000355 ) ) ;
#28930 = FILL_AREA_STYLE ('',( #2143 ) ) ;
#28931 = SURFACE_STYLE_FILL_AREA ( #7505 ) ;
#28932 = CARTESIAN_POINT ( 'NONE',  ( 0.000000000000000000, 2.299999999999999822, -5.000000000000000000 ) ) ;
#28933 = CARTESIAN_POINT ( 'NONE',  ( -45.50000000000000000, 99.99999999999992895, 10.00000000000000000 ) ) ;
#28934 = EDGE_LOOP ( 'NONE', ( #44327, #31769, #46662, #3731 ) ) ;
#28935 = CARTESIAN_POINT ( 'NONE',  ( -51.59499999999997755, 2.607480562269073321, 8.024999999999991473 ) ) ;
#28936 = VERTEX_POINT ( 'NONE', #45485 ) ;
#28937 = CARTESIAN_POINT ( 'NONE',  ( 6.330869393641158638, 43.00000000000000000, 28.38386403503541899 ) ) ;
#28938 = DIRECTION ( 'NONE',  ( -0.000000000000000000, 1.000000000000000000, -0.000000000000000000 ) ) ;
#28939 = AXIS2_PLACEMENT_3D ( 'NONE', #36313, #4222, #36670 ) ;
#28940 = CARTESIAN_POINT ( 'NONE',  ( -15.98999599679679839, 118.4999999999999716, -7.500000000000000000 ) ) ;
#28941 = ORIENTED_EDGE ( 'NONE', *, *, #24134, .T. ) ;
#28942 = CARTESIAN_POINT ( 'NONE',  ( -50.11702274195462792, -10.88632520110945734, 3.736191679969255386 ) ) ;
#28943 = CARTESIAN_POINT ( 'NONE',  ( -56.99499999999999034, -6.826472737025113702, 4.959722759717902107 ) ) ;
#28944 = SURFACE_STYLE_FILL_AREA ( #14195 ) ;
#28945 = VERTEX_POINT ( 'NONE', #2097 ) ;
#28946 = CIRCLE ( 'NONE', #7626, 1.000000000000000888 ) ;
#28947 = AXIS2_PLACEMENT_3D ( 'NONE', #4053, #32195, #47032 ) ;
#28948 = CARTESIAN_POINT ( 'NONE',  ( -74.41756005331312451, 8.116436936526460144, 6.493641663363979077 ) ) ;
#28949 = CARTESIAN_POINT ( 'NONE',  ( -102.6549999999999869, -7.632228543268600340, -2.479861379858950166 ) ) ;
#28950 = ORIENTED_EDGE ( 'NONE', *, *, #6042, .T. ) ;
#28951 = CYLINDRICAL_SURFACE ( 'NONE', #38481, 9.524999999999991473 ) ;
#28952 = ADVANCED_FACE ( 'NONE', ( #29944 ), #65477, .F. ) ;
#28953 = CARTESIAN_POINT ( 'NONE',  ( 34.99999999999999289, 99.99999999999998579, 10.00000000000000000 ) ) ;
#28954 = CARTESIAN_POINT ( 'NONE',  ( -152.3070736234661240, -10.01517768586948698, 6.132527647946031529E-16 ) ) ;
#28955 = DIRECTION ( 'NONE',  ( 0.000000000000000000, 0.000000000000000000, 1.000000000000000000 ) ) ;
#28956 = CARTESIAN_POINT ( 'NONE',  ( 9.058813317711337021, 141.5449999999999875, 2.943386871421375783 ) ) ;
#28957 = CARTESIAN_POINT ( 'NONE',  ( -85.25707362346616947, 5.598654528085800663, -7.705886871421367523 ) ) ;
#28958 = PRESENTATION_STYLE_ASSIGNMENT (( #60631 ) ) ;
#28959 = CARTESIAN_POINT ( 'NONE',  ( 15.98999599679679839, 146.4999999999999716, 7.500000000000000000 ) ) ;
#28960 = VERTEX_POINT ( 'NONE', #18004 ) ;
#28961 = FILL_AREA_STYLE_COLOUR ( '', #68457 ) ;
#28962 = VECTOR ( 'NONE', #61272, 1000.000000000000000 ) ;
#28963 = EDGE_CURVE ( 'NONE', #32796, #31059, #11544, .T. ) ;
#28965 = FILL_AREA_STYLE_COLOUR ( '', #56087 ) ;
#28964 = DIRECTION ( 'NONE',  ( -0.000000000000000000, 1.000000000000000000, -0.000000000000000000 ) ) ;
#28966 = CARTESIAN_POINT ( 'NONE',  ( -134.6050000000000182, 6.826472737025113702, -4.959722759717902107 ) ) ;
#28967 = EDGE_CURVE ( 'NONE', #64020, #31165, #23671, .T. ) ;
#28968 = DIRECTION ( 'NONE',  ( 0.000000000000000000, 0.000000000000000000, -1.000000000000000000 ) ) ;
#28969 = CARTESIAN_POINT ( 'NONE',  ( -146.3929263765337794, 8.102448949553176405, 5.886773742842740909 ) ) ;
#28970 = CARTESIAN_POINT ( 'NONE',  ( 44.99999999999977973, 149.4999999999999716, 10.00000000000000000 ) ) ;
#28971 = CARTESIAN_POINT ( 'NONE',  ( -138.2949999999999591, -2.607480562269069768, 8.024999999999991473 ) ) ;
#28972 = EDGE_CURVE ( 'NONE', #33857, #51702, #50863, .T. ) ;
#28973 = CARTESIAN_POINT ( 'NONE',  ( -127.4949999999999903, 6.826472737025113702, -4.959722759717902107 ) ) ;
#28974 = EDGE_CURVE ( 'NONE', #40596, #44849, #4217, .T. ) ;
#28975 = FACE_OUTER_BOUND ( 'NONE', #62665, .T. ) ;
#28977 = ORIENTED_EDGE ( 'NONE', *, *, #27065, .T. ) ;
#28976 = B_SPLINE_CURVE_WITH_KNOTS ( 'NONE', 3,
 ( #69382, #69038, #42349, #63736, #64086, #15939 ),
 .UNSPECIFIED., .F., .F.,
 ( 4, 2, 4 ),
 ( 0.004189585287972440175, 0.006269578072783815043, 0.008349570857595189910 ),
 .UNSPECIFIED. ) ;
#28978 = CARTESIAN_POINT ( 'NONE',  ( -146.0070736234661410, -8.102448949553174629, -5.886773742842741797 ) ) ;
#28979 =( NAMED_UNIT ( * ) PLANE_ANGLE_UNIT ( ) SI_UNIT ( $, .RADIAN. ) );
#28980 = EDGE_CURVE ( 'NONE', #21181, #34757, #57592, .T. ) ;
#28981 = CARTESIAN_POINT ( 'NONE',  ( 9.827790563157511022E-16, 87.30187232391182306, -8.025000000000000355 ) ) ;
#28982 = CARTESIAN_POINT ( 'NONE',  ( -177.8929263765338078, -8.102448949553172852, -5.886773742842741797 ) ) ;
#28983 = SURFACE_STYLE_USAGE ( .BOTH. , #28646 ) ;
#28984 = CARTESIAN_POINT ( 'NONE',  ( -50.99499999999999034, -6.826472737025115478, 4.959722759717900331 ) ) ;
#28985 =( NAMED_UNIT ( * ) SI_UNIT ( $, .STERADIAN. ) SOLID_ANGLE_UNIT ( ) );
#28986 =( GEOMETRIC_REPRESENTATION_CONTEXT ( 3 ) GLOBAL_UNCERTAINTY_ASSIGNED_CONTEXT ( ( #15184 ) ) GLOBAL_UNIT_ASSIGNED_CONTEXT ( ( #8547, #3188, #3552 ) ) REPRESENTATION_CONTEXT ( 'NONE', 'WORKASPACE' ) );
#28987 = CYLINDRICAL_SURFACE ( 'NONE', #50380, 4.000000000000000000 ) ;
#28988 = DIRECTION ( 'NONE',  ( 1.000000000000000000, 0.000000000000000000, 0.000000000000000000 ) ) ;
#28989 = CARTESIAN_POINT ( 'NONE',  ( -96.74292637653380211, -5.598654528085803328, -7.705886871421366635 ) ) ;
#28990 = PRODUCT_CONTEXT ( 'NONE', #21711, 'mechanical' ) ;
#28991 = CIRCLE ( 'NONE', #36939, 0.5000000000000004441 ) ;
#28992 = DIRECTION ( 'NONE',  ( -0.000000000000000000, -0.000000000000000000, -1.000000000000000000 ) ) ;
#28993 = DIRECTION ( 'NONE',  ( -0.000000000000000000, -1.000000000000000000, 0.000000000000000000 ) ) ;
#28994 = CARTESIAN_POINT ( 'NONE',  ( 48.50000000000000000, 14.49137674618942562, 7.500000000000000000 ) ) ;
#28995 = CARTESIAN_POINT ( 'NONE',  ( -13.25000000000000355, 27.99999999999998934, -3.750000000000000000 ) ) ;
#28996 = STYLED_ITEM ( 'NONE', ( #49323 ), #50993 ) ;
#28997 = VECTOR ( 'NONE', #28964, 1000.000000000000000 ) ;
#28998 = SURFACE_STYLE_FILL_AREA ( #50158 ) ;
#28999 = VERTEX_POINT ( 'NONE', #37000 ) ;
#29000 = LINE ( 'NONE', #38324, #62340 ) ;
#29001 = CARTESIAN_POINT ( 'NONE',  ( 2.755455298081543989E-15, 154.9999999999999716, 22.49999999999999645 ) ) ;
#29002 = VERTEX_POINT ( 'NONE', #52810 ) ;
#29003 = CARTESIAN_POINT ( 'NONE',  ( 0.000000000000000000, 133.0570736234661524, -8.025000000000000355 ) ) ;
#29004 = STYLED_ITEM ( 'NONE', ( #15632 ), #14500 ) ;
#29005 = CARTESIAN_POINT ( 'NONE',  ( 6.826472737025119919, 126.0070736234661695, 4.959722759717908325 ) ) ;
#29006 = PRESENTATION_LAYER_ASSIGNMENT (  '', '', ( #59337 ) ) ;
#29007 = DIRECTION ( 'NONE',  ( 0.000000000000000000, -0.000000000000000000, -1.000000000000000000 ) ) ;
#29008 =( NAMED_UNIT ( * ) PLANE_ANGLE_UNIT ( ) SI_UNIT ( $, .RADIAN. ) );
#29009 = ORIENTED_EDGE ( 'NONE', *, *, #7782, .T. ) ;
#29010 = DIRECTION ( 'NONE',  ( -0.000000000000000000, -0.000000000000000000, 1.000000000000000000 ) ) ;
#29011 = CARTESIAN_POINT ( 'NONE',  ( 3.000000000000030198, 38.93969262078591242, 89.65797985667433068 ) ) ;
#29012 = FACE_OUTER_BOUND ( 'NONE', #66136, .T. ) ;
#29013 = B_SPLINE_CURVE_WITH_KNOTS ( 'NONE', 3,
 ( #35224, #51401, #10572, #64374, #26713, #43329 ),
 .UNSPECIFIED., .F., .F.,
 ( 4, 2, 4 ),
 ( 0.004189585287972438440, 0.006269578072783812440, 0.008349570857595186441 ),
 .UNSPECIFIED. ) ;
#29014 = DIRECTION ( 'NONE',  ( 1.000000000000000000, 0.000000000000000000, 0.000000000000000000 ) ) ;
#29015 = CARTESIAN_POINT ( 'NONE',  ( -81.29499999999998749, -2.607480562269069768, 8.024999999999991473 ) ) ;
#29016 = VERTEX_POINT ( 'NONE', #62304 ) ;
#29017 = CARTESIAN_POINT ( 'NONE',  ( -20.54889675933014814, 114.6603872790887095, -10.28544290717500509 ) ) ;
#29018 = FILL_AREA_STYLE ('',( #14613 ) ) ;
#29019 = AXIS2_PLACEMENT_3D ( 'NONE', #43666, #45048, #17607 ) ;
#29020 = ORIENTED_EDGE ( 'NONE', *, *, #38697, .T. ) ;
#29021 = SURFACE_STYLE_FILL_AREA ( #28689 ) ;
#29022 = CIRCLE ( 'NONE', #9994, 5.000000000000000888 ) ;
#29023 = EDGE_LOOP ( 'NONE', ( #41247, #24504, #66007 ) ) ;
#29024 = DIRECTION ( 'NONE',  ( 0.000000000000000000, -1.000000000000000000, 0.000000000000000000 ) ) ;
#29026 = EDGE_LOOP ( 'NONE', ( #27012, #13624, #44228, #9606 ) ) ;
#29025 = EDGE_CURVE ( 'NONE', #7949, #11857, #14125, .T. ) ;
#29028 = PRESENTATION_STYLE_ASSIGNMENT (( #45282 ) ) ;
#29027 = PRESENTATION_LAYER_ASSIGNMENT (  '', '', ( #36997 ) ) ;
#29029 = LINE ( 'NONE', #23105, #11127 ) ;
#29030 = SURFACE_STYLE_FILL_AREA ( #34343 ) ;
#29031 = DIRECTION ( 'NONE',  ( 0.000000000000000000, 0.000000000000000000, 1.000000000000000000 ) ) ;
#29032 = CARTESIAN_POINT ( 'NONE',  ( -180.3570736234661638, 5.598654528085804216, 7.705886871421366635 ) ) ;
#29033 = CARTESIAN_POINT ( 'NONE',  ( -6.778496103155775110, 110.5743167862572278, 6.848681790824214133 ) ) ;
#29034 = PRESENTATION_LAYER_ASSIGNMENT (  '', '', ( #37002 ) ) ;
#29035 = EDGE_CURVE ( 'NONE', #54235, #57448, #66842, .T. ) ;
#29036 = CARTESIAN_POINT ( 'NONE',  ( -114.2070736234661581, 3.094860106618433360, 9.524999999999991473 ) ) ;
#29037 = DIRECTION ( 'NONE',  ( 1.000000000000000000, 0.000000000000000000, 0.000000000000000000 ) ) ;
#29038 = CARTESIAN_POINT ( 'NONE',  ( -71.74137931034481142, 36.89918356738973415, -10.00000000000000000 ) ) ;
#29039 = VERTEX_POINT ( 'NONE', #62630 ) ;
#29040 = AXIS2_PLACEMENT_3D ( 'NONE', #9916, #63010, #47234 ) ;
#29041 = CARTESIAN_POINT ( 'NONE',  ( 0.3542424171060651328, 42.77450929379338618, 45.47201693779177134 ) ) ;
#29042 = CIRCLE ( 'NONE', #2032, 0.5000000000000004441 ) ;
#29043 = DIRECTION ( 'NONE',  ( -0.000000000000000000, -0.000000000000000000, 1.000000000000000000 ) ) ;
#29044 = DIRECTION ( 'NONE',  ( 0.000000000000000000, 0.000000000000000000, -1.000000000000000000 ) ) ;
#29045 = PRESENTATION_STYLE_ASSIGNMENT (( #56495 ) ) ;
#29046 = ORIENTED_EDGE ( 'NONE', *, *, #51088, .T. ) ;
#29047 = CARTESIAN_POINT ( 'NONE',  ( -159.5049999999999955, -6.826472737025115478, -4.959722759717899443 ) ) ;
#29048 = PRESENTATION_STYLE_ASSIGNMENT (( #26630 ) ) ;
#29049 = LINE ( 'NONE', #49860, #12246 ) ;
#29050 = CARTESIAN_POINT ( 'NONE',  ( -167.3949999999999534, -6.826472737025115478, -4.959722759717899443 ) ) ;
#29051 = ADVANCED_FACE ( 'NONE', ( #41936 ), #9202, .T. ) ;
#29052 = CARTESIAN_POINT ( 'NONE',  ( -154.9449999999999932, -9.827790563157499189E-16, -8.024999999999991473 ) ) ;
#29053 = EDGE_LOOP ( 'NONE', ( #57984, #13542, #63664, #13479 ) ) ;
#29054 =( GEOMETRIC_REPRESENTATION_CONTEXT ( 3 ) GLOBAL_UNCERTAINTY_ASSIGNED_CONTEXT ( ( #12881 ) ) GLOBAL_UNIT_ASSIGNED_CONTEXT ( ( #51486, #51853, #15283 ) ) REPRESENTATION_CONTEXT ( 'NONE', 'WORKASPACE' ) );
#29055 = CARTESIAN_POINT ( 'NONE',  ( 44.97648960591795486, 10.67803934730671322, 3.825005713026917942 ) ) ;
#29056 = EDGE_CURVE ( 'NONE', #20549, #30521, #19423, .T. ) ;
#29057 = PLANE ( 'NONE',  #13617 ) ;
#29058 = CARTESIAN_POINT ( 'NONE',  ( -74.90499999999997272, 2.607480562269068880, -8.024999999999993250 ) ) ;
#29059 = CARTESIAN_POINT ( 'NONE',  ( 25.75000000000001066, 21.74999999999998224, -3.750000000000000000 ) ) ;
#29060 =( GEOMETRIC_REPRESENTATION_CONTEXT ( 3 ) GLOBAL_UNCERTAINTY_ASSIGNED_CONTEXT ( ( #34704 ) ) GLOBAL_UNIT_ASSIGNED_CONTEXT ( ( #46340, #15011, #19900 ) ) REPRESENTATION_CONTEXT ( 'NONE', 'WORKASPACE' ) );
#29061 = CARTESIAN_POINT ( 'NONE',  ( -70.19499999999997897, 8.437984349512086979, -1.550032578732815448E-15 ) ) ;
#29062 = CARTESIAN_POINT ( 'NONE',  ( -8.102448949553181734, 144.0050000000000239, -5.886773742842749790 ) ) ;
#29063 = DIRECTION ( 'NONE',  ( -1.000000000000000000, -0.000000000000000000, -0.000000000000000000 ) ) ;
#29064 = CARTESIAN_POINT ( 'NONE',  ( -37.50000000000000000, 58.31681314173471975, -6.349999999999996092 ) ) ;
#29065 = UNCERTAINTY_MEASURE_WITH_UNIT (LENGTH_MEASURE( 1.000000000000000082E-05 ), #28549, 'distance_accuracy_value', 'NONE');
#29066 = CARTESIAN_POINT ( 'NONE',  ( 0.000000000000000000, -2.500000000000000000, 0.000000000000000000 ) ) ;
#29067 = AXIS2_PLACEMENT_3D ( 'NONE', #39595, #56074, #55389 ) ;
#29068 = CARTESIAN_POINT ( 'NONE',  ( 8.920833891111493941, 2.231456886122029193, -2.548662454712524728 ) ) ;
#29069 = CONICAL_SURFACE ( 'NONE', #22373, 7.000000000000000888, 0.7853981633974500554 ) ;
#29070 = DIRECTION ( 'NONE',  ( 0.2413793103448194644, 0.9704308468600220117, 0.000000000000000000 ) ) ;
#29071 = COLOUR_RGB ( '', 0.09019608, 0.27058824, 0.51372549) ;
#29072 =( NAMED_UNIT ( * ) SI_UNIT ( $, .STERADIAN. ) SOLID_ANGLE_UNIT ( ) );
#29073 =( LENGTH_UNIT ( ) NAMED_UNIT ( * ) SI_UNIT ( .MILLI., .METRE. ) );
#29074 = ORIENTED_EDGE ( 'NONE', *, *, #39600, .T. ) ;
#29075 = MECHANICAL_DESIGN_GEOMETRIC_PRESENTATION_REPRESENTATION (  '', ( #37041 ), #21260 ) ;
#29076 = ORIENTED_EDGE ( 'NONE', *, *, #41261, .T. ) ;
#29077 = STYLED_ITEM ( 'NONE', ( #40645 ), #33588 ) ;
#29078 = ADVANCED_FACE ( 'NONE', ( #31312 ), #30265, .T. ) ;
#29079 = FILL_AREA_STYLE_COLOUR ( '', #53952 ) ;
#29080 = CIRCLE ( 'NONE', #32464, 0.9999999999999991118 ) ;
#29081 = CARTESIAN_POINT ( 'NONE',  ( -23.71231517720798010, 117.9999999999999716, 9.500000000000000000 ) ) ;
#29082 = ORIENTED_EDGE ( 'NONE', *, *, #56199, .T. ) ;
#29083 = VERTEX_POINT ( 'NONE', #5973 ) ;
#29084 = LINE ( 'NONE', #40741, #58967 ) ;
#29085 = SURFACE_SIDE_STYLE ('',( #2311 ) ) ;
#29086 = VERTEX_POINT ( 'NONE', #17268 ) ;
#29087 = CARTESIAN_POINT ( 'NONE',  ( 9.058813317711337021, 112.6549999999999869, 2.943386871421375783 ) ) ;
#29088 = DIRECTION ( 'NONE',  ( -1.000000000000000000, -7.709882115452469292E-16, 0.000000000000000000 ) ) ;
#29089 = EDGE_LOOP ( 'NONE', ( #58347, #15822, #1966, #64459 ) ) ;
#29090 = CARTESIAN_POINT ( 'NONE',  ( 3.749999999999999556, 34.24999999999998579, 4.000000000000000000 ) ) ;
#29091 = CARTESIAN_POINT ( 'NONE',  ( -111.4449999999999932, 0.000000000000000000, 8.024999999999991473 ) ) ;
#29092 = ORIENTED_EDGE ( 'NONE', *, *, #8371, .T. ) ;
#29093 = ORIENTED_EDGE ( 'NONE', *, *, #55202, .T. ) ;
#29094 = CARTESIAN_POINT ( 'NONE',  ( -74.24150567752717222, 8.825695369645321975, -6.400617768950437991 ) ) ;
#29095 = FILL_AREA_STYLE_COLOUR ( '', #17095 ) ;
#29096 = CARTESIAN_POINT ( 'NONE',  ( -11.02951865299722556, -11.60758465034584930, 3.056320357840781377 ) ) ;
#29097 = ORIENTED_EDGE ( 'NONE', *, *, #6646, .F. ) ;
#29098 = B_SPLINE_CURVE_WITH_KNOTS ( 'NONE', 3,
 ( #39787, #66483, #55578, #50312, #61519, #56966 ),
 .UNSPECIFIED., .F., .F.,
 ( 4, 2, 4 ),
 ( 0.004189585287972434971, 0.006269578072783811573, 0.008349570857595188175 ),
 .UNSPECIFIED. ) ;
#29099 = CARTESIAN_POINT ( 'NONE',  ( -7.632228543268608334, 144.8429263765338249, 2.479861379858952830 ) ) ;
#29100 = CARTESIAN_POINT ( 'NONE',  ( 0.000000000000000000, 114.4999999999999574, -23.00000000000000000 ) ) ;
#29101 =( LENGTH_UNIT ( ) NAMED_UNIT ( * ) SI_UNIT ( .MILLI., .METRE. ) );
#29102 = AXIS2_PLACEMENT_3D ( 'NONE', #24068, #19827, #13861 ) ;
#29103 = ADVANCED_FACE ( 'NONE', ( #59100 ), #47570, .F. ) ;
#29104 = CARTESIAN_POINT ( 'NONE',  ( -7.632228543268608334, 114.8429263765338106, 2.479861379858952830 ) ) ;
#29105 = ADVANCED_FACE ( 'NONE', ( #27414 ), #640, .T. ) ;
#29106 = VERTEX_POINT ( 'NONE', #53149 ) ;
#29107 = SURFACE_STYLE_USAGE ( .BOTH. , #56205 ) ;
#29108 = ORIENTED_EDGE ( 'NONE', *, *, #23731, .F. ) ;
#29109 = FILL_AREA_STYLE ('',( #44678 ) ) ;
#29110 = SURFACE_STYLE_FILL_AREA ( #37683 ) ;
#29111 = DIRECTION ( 'NONE',  ( 0.000000000000000000, 0.000000000000000000, -1.000000000000000000 ) ) ;
#29112 = CARTESIAN_POINT ( 'NONE',  ( 41.25908726609139165, 107.3516760703038102, -3.442203282073897253 ) ) ;
#29113 = CARTESIAN_POINT ( 'NONE',  ( -131.7549999999999955, 4.716976649647091513, -6.492361379858946790 ) ) ;
#29114 = AXIS2_PLACEMENT_3D ( 'NONE', #61728, #51548, #29386 ) ;
#29115 = COLOUR_RGB ( '', 0.09019608, 0.27058824, 0.51372549) ;
#29116 = SURFACE_STYLE_USAGE ( .BOTH. , #7680 ) ;
#29117 = ORIENTED_EDGE ( 'NONE', *, *, #65982, .T. ) ;
#29118 = EDGE_CURVE ( 'NONE', #52602, #21193, #26719, .T. ) ;
#29119 = TOROIDAL_SURFACE ( 'NONE', #33612, 1.000000000000000000, 0.5000000000000000000 ) ;
#29120 = CARTESIAN_POINT ( 'NONE',  ( 10.00000000000000178, 60.69879356856722552, -69.02971849933236115 ) ) ;
#29121 = DIRECTION ( 'NONE',  ( -1.000000000000000000, -0.000000000000000000, -0.000000000000000000 ) ) ;
#29122 = CARTESIAN_POINT ( 'NONE',  ( 22.00000000000000711, 50.00000000000000000, -60.00000000000000711 ) ) ;
#29123 = VERTEX_POINT ( 'NONE', #37706 ) ;
#29124 = ORIENTED_EDGE ( 'NONE', *, *, #42284, .T. ) ;
#29125 = FACE_OUTER_BOUND ( 'NONE', #13752, .T. ) ;
#29126 = AXIS2_PLACEMENT_3D ( 'NONE', #68034, #41308, #14916 ) ;
#29127 = CARTESIAN_POINT ( 'NONE',  ( -31.24124550007784507, -8.558011161593890748, -0.5650761621075199859 ) ) ;
#29128 = SURFACE_STYLE_USAGE ( .BOTH. , #38725 ) ;
#29129 = DIRECTION ( 'NONE',  ( 0.000000000000000000, 1.000000000000000000, 0.000000000000000000 ) ) ;
#29130 = ORIENTED_EDGE ( 'NONE', *, *, #65861, .T. ) ;
#29131 = DIRECTION ( 'NONE',  ( 0.000000000000000000, 0.000000000000000000, 1.000000000000000000 ) ) ;
#29132 = SURFACE_STYLE_FILL_AREA ( #61845 ) ;
#29133 = CYLINDRICAL_SURFACE ( 'NONE', #53735, 9.524999999999991473 ) ;
#29134 = VECTOR ( 'NONE', #2441, 1000.000000000000000 ) ;
#29135 = CARTESIAN_POINT ( 'NONE',  ( -51.80707362346617373, 10.01517768586948698, -1.839758294383808571E-15 ) ) ;
#29136 = EDGE_CURVE ( 'NONE', #58906, #14945, #51979, .T. ) ;
#29137 = PRESENTATION_LAYER_ASSIGNMENT (  '', '', ( #5591 ) ) ;
#29138 = SURFACE_STYLE_FILL_AREA ( #7699 ) ;
#29139 = CIRCLE ( 'NONE', #41549, 7.500000000000000000 ) ;
#29140 = CARTESIAN_POINT ( 'NONE',  ( -177.2070736234662434, 3.094860106619617746, 9.524999999999131717 ) ) ;
#29141 = ORIENTED_EDGE ( 'NONE', *, *, #50584, .F. ) ;
#29142 = STYLED_ITEM ( 'NONE', ( #5735 ), #9473 ) ;
#29143 = CARTESIAN_POINT ( 'NONE',  ( -145.4070736234666015, 3.094860106610764827, -9.525000000005562129 ) ) ;
#29145 = EDGE_CURVE ( 'NONE', #17716, #40317, #43662, .T. ) ;
#29144 = AXIS2_PLACEMENT_3D ( 'NONE', #46238, #62376, #27141 ) ;
#29146 = LINE ( 'NONE', #45737, #48433 ) ;
#29147 = CARTESIAN_POINT ( 'NONE',  ( -98.75499999999999545, 4.716976649647091513, -6.492361379858946790 ) ) ;
#29148 = CARTESIAN_POINT ( 'NONE',  ( 7.616319612703724040, 154.5000000000000568, -5.787195445650213266 ) ) ;
#29149 = FACE_OUTER_BOUND ( 'NONE', #32955, .T. ) ;
#29150 = CARTESIAN_POINT ( 'NONE',  ( 0.000000000000000000, 42.00000000000000000, -79.00402776293826435 ) ) ;
#29151 = CARTESIAN_POINT ( 'NONE',  ( -96.59499999999998465, 2.607480562269072433, 8.024999999999991473 ) ) ;
#29152 = CARTESIAN_POINT ( 'NONE',  ( 3.094860106618431583, 118.2049999999999699, 9.525000000000000355 ) ) ;
#29153 = CARTESIAN_POINT ( 'NONE',  ( -73.34499999999999886, 7.632228543268599452, -2.479861379858951942 ) ) ;
#29154 = PRESENTATION_STYLE_ASSIGNMENT (( #39774 ) ) ;
#29155 = AXIS2_PLACEMENT_3D ( 'NONE', #67594, #67239, #46887 ) ;
#29156 = CYLINDRICAL_SURFACE ( 'NONE', #47481, 9.524999999999991473 ) ;
#29157 = UNCERTAINTY_MEASURE_WITH_UNIT (LENGTH_MEASURE( 1.000000000000000082E-05 ), #64529, 'distance_accuracy_value', 'NONE');
#29158 = STYLED_ITEM ( 'NONE', ( #13422 ), #16001 ) ;
#29159 = CARTESIAN_POINT ( 'NONE',  ( 41.72783051798698040, 107.4000574072429259, -4.000000000000000888 ) ) ;
#29160 = ORIENTED_EDGE ( 'NONE', *, *, #1980, .F. ) ;
#29161 = CARTESIAN_POINT ( 'NONE',  ( -119.0929263765337964, 3.094860106618433360, 9.524999999999991473 ) ) ;
#29162 = CARTESIAN_POINT ( 'NONE',  ( -139.4949999999999761, 6.826472737025113702, -4.959722759717902107 ) ) ;
#29163 = DIRECTION ( 'NONE',  ( 0.000000000000000000, 0.000000000000000000, 1.000000000000000000 ) ) ;
#29164 =( GEOMETRIC_REPRESENTATION_CONTEXT ( 3 ) GLOBAL_UNCERTAINTY_ASSIGNED_CONTEXT ( ( #35431 ) ) GLOBAL_UNIT_ASSIGNED_CONTEXT ( ( #35504, #68908, #62217 ) ) REPRESENTATION_CONTEXT ( 'NONE', 'WORKASPACE' ) );
#29165 = CARTESIAN_POINT ( 'NONE',  ( 57.00000000000000000, 13.00000000000000178, 80.00402776293826435 ) ) ;
#29166 = CARTESIAN_POINT ( 'NONE',  ( 0.000000000000000000, 0.000000000000000000, 0.2499999999999941436 ) ) ;
#29167 =( NAMED_UNIT ( * ) SI_UNIT ( $, .STERADIAN. ) SOLID_ANGLE_UNIT ( ) );
#29168 = VERTEX_POINT ( 'NONE', #21119 ) ;
#29169 = ORIENTED_EDGE ( 'NONE', *, *, #218, .F. ) ;
#29170 = PRESENTATION_LAYER_ASSIGNMENT (  '', '', ( #20196 ) ) ;
#29171 =( GEOMETRIC_REPRESENTATION_CONTEXT ( 3 ) GLOBAL_UNCERTAINTY_ASSIGNED_CONTEXT ( ( #29875 ) ) GLOBAL_UNIT_ASSIGNED_CONTEXT ( ( #10568, #5259, #60794 ) ) REPRESENTATION_CONTEXT ( 'NONE', 'WORKASPACE' ) );
#29172 = CARTESIAN_POINT ( 'NONE',  ( -15.48999599679679662, 146.4999999999999716, 7.000000000000000000 ) ) ;
#29173 = EDGE_CURVE ( 'NONE', #19777, #2072, #27233, .T. ) ;
#29174 = AXIS2_PLACEMENT_3D ( 'NONE', #32039, #47939, #26404 ) ;
#29175 = DIRECTION ( 'NONE',  ( 1.000000000000000000, 0.000000000000000000, 0.000000000000000000 ) ) ;
#29176 = CARTESIAN_POINT ( 'NONE',  ( 48.25000000000000000, 21.74999999999998579, 4.000000000000000000 ) ) ;
#29177 = CARTESIAN_POINT ( 'NONE',  ( 71.49999999999998579, 119.9999999999997868, -7.000000000000000000 ) ) ;
#29178 = DIRECTION ( 'NONE',  ( 0.000000000000000000, 0.000000000000000000, -1.000000000000000000 ) ) ;
#29179 = ORIENTED_EDGE ( 'NONE', *, *, #35664, .T. ) ;
#29180 = CARTESIAN_POINT ( 'NONE',  ( -136.1049999999999898, -6.826472737025113702, 4.959722759717902107 ) ) ;
#29181 = VERTEX_POINT ( 'NONE', #53812 ) ;
#29182 = EDGE_LOOP ( 'NONE', ( #58550, #37735, #10717 ) ) ;
#29183 = FACE_OUTER_BOUND ( 'NONE', #27295, .T. ) ;
#29184 = DIRECTION ( 'NONE',  ( 0.000000000000000000, 0.000000000000000000, 1.000000000000000000 ) ) ;
#29185 = ORIENTED_EDGE ( 'NONE', *, *, #42457, .T. ) ;
#29186 = CIRCLE ( 'NONE', #6755, 10.00000000000000178 ) ;
#29187 = VECTOR ( 'NONE', #1686, 1000.000000000000000 ) ;
#29188 =( NAMED_UNIT ( * ) SI_UNIT ( $, .STERADIAN. ) SOLID_ANGLE_UNIT ( ) );
#29189 = MECHANICAL_DESIGN_GEOMETRIC_PRESENTATION_REPRESENTATION (  '', ( #53908 ), #44967 ) ;
#29190 = CARTESIAN_POINT ( 'NONE',  ( 0.000000000000000000, 136.4449999999999932, -9.525000000000000355 ) ) ;
#29191 = CARTESIAN_POINT ( 'NONE',  ( 35.99999999999999289, 5.000000000000000000, 72.00402776293825013 ) ) ;
#29192 = ORIENTED_EDGE ( 'NONE', *, *, #46439, .T. ) ;
#29193 = ADVANCED_FACE ( 'NONE', ( #5610 ), #12641, .F. ) ;
#29194 = CARTESIAN_POINT ( 'NONE',  ( 3.094860106618435136, 137.4049999999999727, -9.525000000000000355 ) ) ;
#29195 = CARTESIAN_POINT ( 'NONE',  ( -48.80499999999997129, -8.437984349512086979, 5.166775262442717831E-16 ) ) ;
#29196 = STYLED_ITEM ( 'NONE', ( #12916 ), #33173 ) ;
#29197 = FILL_AREA_STYLE_COLOUR ( '', #55420 ) ;
#29198 = ORIENTED_EDGE ( 'NONE', *, *, #56873, .T. ) ;
#29199 = CARTESIAN_POINT ( 'NONE',  ( -9.827790563157511022E-16, 112.4429263765338192, 8.025000000000000355 ) ) ;
#29200 = DIRECTION ( 'NONE',  ( -0.000000000000000000, -1.000000000000000000, -0.000000000000000000 ) ) ;
#29201 = UNCERTAINTY_MEASURE_WITH_UNIT (LENGTH_MEASURE( 1.000000000000000082E-05 ), #10176, 'distance_accuracy_value', 'NONE');
#29202 = STYLED_ITEM ( 'NONE', ( #36137 ), #51812 ) ;
#29203 = EDGE_CURVE ( 'NONE', #61204, #32928, #43040, .T. ) ;
#29204 = SURFACE_STYLE_USAGE ( .BOTH. , #3483 ) ;
#29205 = CARTESIAN_POINT ( 'NONE',  ( 4.041451884327379673, -7.000000000000002665, 7.500000000000000000 ) ) ;
#29206 = ADVANCED_FACE ( 'NONE', ( #37354 ), #38032, .F. ) ;
#29207 = VERTEX_POINT ( 'NONE', #34441 ) ;
#29208 = COLOUR_RGB ( '', 0.66274510, 0.83137255, 0.94901961) ;
#29209 =( NAMED_UNIT ( * ) SI_UNIT ( $, .STERADIAN. ) SOLID_ANGLE_UNIT ( ) );
#29210 = ORIENTED_EDGE ( 'NONE', *, *, #44874, .F. ) ;
#29211 = FACE_OUTER_BOUND ( 'NONE', #23907, .T. ) ;
#29212 = VECTOR ( 'NONE', #46080, 1000.000000000000000 ) ;
#29213 = CARTESIAN_POINT ( 'NONE',  ( -122.7570736234661695, -5.598654528085801552, 7.705886871421367523 ) ) ;
#29214 = DIRECTION ( 'NONE',  ( 0.000000000000000000, 0.000000000000000000, 1.000000000000000000 ) ) ;
#29215 = CARTESIAN_POINT ( 'NONE',  ( -163.8549999999999898, 4.716976649647094177, 6.492361379858945902 ) ) ;
#29216 = VERTEX_POINT ( 'NONE', #17921 ) ;
#29217 = CARTESIAN_POINT ( 'NONE',  ( -45.50000000000000000, 1.797044900979284448E-15, 9.500000000000000000 ) ) ;
#29218 = UNCERTAINTY_MEASURE_WITH_UNIT (LENGTH_MEASURE( 1.000000000000000082E-05 ), #64266, 'distance_accuracy_value', 'NONE');
#29219 = MECHANICAL_DESIGN_GEOMETRIC_PRESENTATION_REPRESENTATION (  '', ( #6732 ), #20236 ) ;
#29220 = MECHANICAL_DESIGN_GEOMETRIC_PRESENTATION_REPRESENTATION (  '', ( #28095 ), #37119 ) ;
#29221 = EDGE_CURVE ( 'NONE', #35999, #62163, #8057, .T. ) ;
#29222 = DIRECTION ( 'NONE',  ( 0.000000000000000000, 1.000000000000000000, 0.000000000000000000 ) ) ;
#29223 = DIRECTION ( 'NONE',  ( -1.000000000000000000, 0.000000000000000000, 0.000000000000000000 ) ) ;
#29224 = SURFACE_STYLE_USAGE ( .BOTH. , #61253 ) ;
#29225 = ORIENTED_EDGE ( 'NONE', *, *, #60826, .F. ) ;
#29226 = CIRCLE ( 'NONE', #37169, 0.2500000000000002220 ) ;
#29228 = EDGE_CURVE ( 'NONE', #29216, #14021, #61494, .T. ) ;
#29227 = VERTEX_POINT ( 'NONE', #13317 ) ;
#29229 = DIRECTION ( 'NONE',  ( 1.000000000000000000, 0.000000000000000000, 0.000000000000000000 ) ) ;
#29230 = CARTESIAN_POINT ( 'NONE',  ( 8.000000000000000000, 33.74999999999998579, -3.750000000000000000 ) ) ;
#29231 = CARTESIAN_POINT ( 'NONE',  ( -76.70499999999999829, 2.607480562269073321, 8.024999999999991473 ) ) ;
#29232 = ORIENTED_EDGE ( 'NONE', *, *, #59974, .F. ) ;
#29233 = CARTESIAN_POINT ( 'NONE',  ( -24.21231517720798010, 113.4999999999999858, -7.000000000000000000 ) ) ;
#29234 = PRESENTATION_LAYER_ASSIGNMENT (  '', '', ( #9069 ) ) ;
#29235 =( BOUNDED_CURVE ( )  B_SPLINE_CURVE ( 2, ( #7293, #29420, #13948, #40031, #61089, #62122, #24148, #17845, #45656, #45983, #13234 ),
 .UNSPECIFIED., .F., .F. ) 
 B_SPLINE_CURVE_WITH_KNOTS ( ( 3, 2, 2, 2, 2, 3 ),
 ( 0.8478260869565217295, 0.8499999999999999778, 0.8521739130434782261, 0.8543478260869564744, 0.8565217391304348338, 0.8586956521739130821 ),
 .UNSPECIFIED. ) 
 CURVE ( )  GEOMETRIC_REPRESENTATION_ITEM ( )  RATIONAL_B_SPLINE_CURVE ( ( 1.000000000000000000, 0.9510565162951535312, 1.000000000000000000, 0.9510565162951535312, 1.000000000000000000, 0.9510565162951535312, 1.000000000000000000, 0.9510565162951535312, 1.000000000000000000, 0.9510565162951535312, 1.000000000000000000 ) ) 
 REPRESENTATION_ITEM ( '' )  );
#29236 = CARTESIAN_POINT ( 'NONE',  ( -63.65707362346617515, 9.058813317711329915, 2.943386871421369566 ) ) ;
#29237 = CARTESIAN_POINT ( 'NONE',  ( 8.750000000000001776, 24.74999999999998579, -4.000000000000000000 ) ) ;
#29238 = CIRCLE ( 'NONE', #55044, 0.5000000000000004441 ) ;
#29239 = CARTESIAN_POINT ( 'NONE',  ( -74.41717294046213738, 8.118038230903733776, -6.493553718642556483 ) ) ;
#29240 = EDGE_LOOP ( 'NONE', ( #38080, #56897, #39555, #41637 ) ) ;
#29241 = SURFACE_STYLE_FILL_AREA ( #19024 ) ;
#29242 = DIRECTION ( 'NONE',  ( -1.000000000000000000, -0.000000000000000000, -0.000000000000000000 ) ) ;
#29243 = CARTESIAN_POINT ( 'NONE',  ( -8.102448949553181734, 140.4949999999999761, 5.886773742842747126 ) ) ;
#29244 = CARTESIAN_POINT ( 'NONE',  ( -105.2949999999999875, -2.607480562269069768, 8.024999999999991473 ) ) ;
#29245 = STYLED_ITEM ( 'NONE', ( #45918 ), #21212 ) ;
#29246 = CARTESIAN_POINT ( 'NONE',  ( 68.99999999999998579, 36.75000000000000000, 3.000000000000000000 ) ) ;
#29247 = LINE ( 'NONE', #2836, #43856 ) ;
#29248 = EDGE_CURVE ( 'NONE', #38790, #15297, #28376, .T. ) ;
#29249 =( GEOMETRIC_REPRESENTATION_CONTEXT ( 3 ) GLOBAL_UNCERTAINTY_ASSIGNED_CONTEXT ( ( #13738 ) ) GLOBAL_UNIT_ASSIGNED_CONTEXT ( ( #66394, #28750, #54454 ) ) REPRESENTATION_CONTEXT ( 'NONE', 'WORKASPACE' ) );
#29251 = CARTESIAN_POINT ( 'NONE',  ( -19.96716105561538512, 11.98620757464661146, 0.6605852583158889901 ) ) ;
#29250 = DIRECTION ( 'NONE',  ( -0.000000000000000000, 0.000000000000000000, -1.000000000000000000 ) ) ;
#29252 = COLOUR_RGB ( '', 0.31764706, 0.68627451, 0.89019608) ;
#29253 = CARTESIAN_POINT ( 'NONE',  ( -140.8429263765338249, 9.058813317711329915, -2.943386871421373119 ) ) ;
#29254 = CARTESIAN_POINT ( 'NONE',  ( -170.0949999999999704, -2.607480562269071545, -8.024999999999991473 ) ) ;
#29255 =( GEOMETRIC_REPRESENTATION_CONTEXT ( 3 ) GLOBAL_UNCERTAINTY_ASSIGNED_CONTEXT ( ( #41951 ) ) GLOBAL_UNIT_ASSIGNED_CONTEXT ( ( #48360, #5380, #31788 ) ) REPRESENTATION_CONTEXT ( 'NONE', 'WORKASPACE' ) );
#29256 = FACE_OUTER_BOUND ( 'NONE', #25873, .T. ) ;
#29257 =( GEOMETRIC_REPRESENTATION_CONTEXT ( 3 ) GLOBAL_UNCERTAINTY_ASSIGNED_CONTEXT ( ( #5298 ) ) GLOBAL_UNIT_ASSIGNED_CONTEXT ( ( #1309, #10896, #48220 ) ) REPRESENTATION_CONTEXT ( 'NONE', 'WORKASPACE' ) );
#29258 = CARTESIAN_POINT ( 'NONE',  ( 44.99999999999998579, 119.9999999999999716, 9.500000000000000000 ) ) ;
#29259 = ORIENTED_EDGE ( 'NONE', *, *, #32621, .T. ) ;
#29260 = DIRECTION ( 'NONE',  ( -1.000000000000000000, 0.000000000000000000, 0.000000000000000000 ) ) ;
#29261 = VERTEX_POINT ( 'NONE', #33407 ) ;
#29262 = AXIS2_PLACEMENT_3D ( 'NONE', #14053, #46088, #30197 ) ;
#29263 = FILL_AREA_STYLE ('',( #19048 ) ) ;
#29264 = AXIS2_PLACEMENT_3D ( 'NONE', #41074, #14305, #30458 ) ;
#29265 = CYLINDRICAL_SURFACE ( 'NONE', #5702, 0.5000000000000004441 ) ;
#29266 = CARTESIAN_POINT ( 'NONE',  ( -48.00000000000000000, 99.99999999999992895, -7.000000000000000000 ) ) ;
#29267 = FILL_AREA_STYLE ('',( #44480 ) ) ;
#29268 = PRESENTATION_LAYER_ASSIGNMENT (  '', '', ( #18095 ) ) ;
#29269 = FACE_OUTER_BOUND ( 'NONE', #8215, .T. ) ;
#29270 = ORIENTED_EDGE ( 'NONE', *, *, #45705, .F. ) ;
#29271 = CARTESIAN_POINT ( 'NONE',  ( -161.0049999999999955, 6.826472737025115478, 4.959722759717899443 ) ) ;
#29272 = ORIENTED_EDGE ( 'NONE', *, *, #28474, .T. ) ;
#29273 = SURFACE_SIDE_STYLE ('',( #56730 ) ) ;
#29275 = EDGE_CURVE ( 'NONE', #36711, #52251, #44361, .T. ) ;
#29274 = CARTESIAN_POINT ( 'NONE',  ( 53.24999999999999289, 27.74999999999998579, 3.750000000000000000 ) ) ;
#29276 = TOROIDAL_SURFACE ( 'NONE', #16971, 14.49999999999999822, 0.5000000000000000000 ) ;
#29277 = CARTESIAN_POINT ( 'NONE',  ( 5.590169943749474513, -4.999999999999999112, -6.123233995736765296E-16 ) ) ;
#29278 = PRESENTATION_STYLE_ASSIGNMENT (( #7831 ) ) ;
#29279 = CARTESIAN_POINT ( 'NONE',  ( -8.437984349512095861, 157.8070736234661240, -5.166775262442723748E-16 ) ) ;
#29280 = ORIENTED_EDGE ( 'NONE', *, *, #13559, .T. ) ;
#29281 = ADVANCED_FACE ( 'NONE', ( #11950 ), #66449, .T. ) ;
#29282 = DIRECTION ( 'NONE',  ( 0.000000000000000000, -1.000000000000000000, 0.000000000000000000 ) ) ;
#29283 = DIRECTION ( 'NONE',  ( 1.000000000000000000, 0.000000000000000000, 0.000000000000000000 ) ) ;
#29284 = VECTOR ( 'NONE', #5979, 1000.000000000000000 ) ;
#29285 = CARTESIAN_POINT ( 'NONE',  ( -87.80499999999999261, -8.437984349512086979, 5.166775262442717831E-16 ) ) ;
#29286 = CARTESIAN_POINT ( 'NONE',  ( -79.99999999999998579, 50.00000000000000000, 11.50000000000003730 ) ) ;
#29287 = CARTESIAN_POINT ( 'NONE',  ( 8.102448949553183510, 125.1049999999999756, -5.886773742842746238 ) ) ;
#29288 = UNCERTAINTY_MEASURE_WITH_UNIT (LENGTH_MEASURE( 1.000000000000000082E-05 ), #66486, 'distance_accuracy_value', 'NONE');
#29289 = CARTESIAN_POINT ( 'NONE',  ( 0.000000000000000000, 133.0570736234661524, -8.025000000000000355 ) ) ;
#29290 = PRESENTATION_STYLE_ASSIGNMENT (( #1818 ) ) ;
#29291 = AXIS2_PLACEMENT_3D ( 'NONE', #20354, #25618, #59035 ) ;
#29292 = ADVANCED_FACE ( 'NONE', ( #12269 ), #55189, .T. ) ;
#29293 = SURFACE_STYLE_USAGE ( .BOTH. , #12773 ) ;
#29294 = STYLED_ITEM ( 'NONE', ( #11020 ), #21278 ) ;
#29295 = ORIENTED_EDGE ( 'NONE', *, *, #33508, .T. ) ;
#29296 = DIRECTION ( 'NONE',  ( -1.000000000000000000, 0.000000000000000000, 0.000000000000000000 ) ) ;
#29297 =( NAMED_UNIT ( * ) SI_UNIT ( $, .STERADIAN. ) SOLID_ANGLE_UNIT ( ) );
#29298 = CARTESIAN_POINT ( 'NONE',  ( -57.74499999999999034, 4.716976649647094177, 6.492361379858945902 ) ) ;
#29299 = ORIENTED_EDGE ( 'NONE', *, *, #37055, .T. ) ;
#29300 = CARTESIAN_POINT ( 'NONE',  ( -65.99999999999998579, 50.00000000000000000, 11.50000000000000000 ) ) ;
#29301 = DIRECTION ( 'NONE',  ( 0.000000000000000000, 0.000000000000000000, 1.000000000000000000 ) ) ;
#29302 = CARTESIAN_POINT ( 'NONE',  ( -87.44292637653380496, -1.166476076187852838E-15, -9.524999999999991473 ) ) ;
#29303 =( LENGTH_UNIT ( ) NAMED_UNIT ( * ) SI_UNIT ( .MILLI., .METRE. ) );
#29304 = ORIENTED_EDGE ( 'NONE', *, *, #16502, .T. ) ;
#29305 = CARTESIAN_POINT ( 'NONE',  ( 0.000000000000000000, 87.30187232391182306, 0.000000000000000000 ) ) ;
#29306 = CARTESIAN_POINT ( 'NONE',  ( -49.79499999999998039, 2.607480562269069324, -8.024999999999993250 ) ) ;
#29307 = FACE_OUTER_BOUND ( 'NONE', #3053, .T. ) ;
#29308 = ORIENTED_EDGE ( 'NONE', *, *, #9946, .F. ) ;
#29309 = ADVANCED_FACE ( 'NONE', ( #2364 ), #18935, .F. ) ;
#29310 = CARTESIAN_POINT ( 'NONE',  ( -75.00000000000000000, 8.421502636539848652, 6.236752812775003818 ) ) ;
#29311 = CARTESIAN_POINT ( 'NONE',  ( -107.9050000000000011, 2.607480562269068880, -8.024999999999993250 ) ) ;
#29312 = ORIENTED_EDGE ( 'NONE', *, *, #36666, .T. ) ;
#29313 = CIRCLE ( 'NONE', #55163, 17.00000000000000000 ) ;
#29314 = DIRECTION ( 'NONE',  ( 0.000000000000000000, -1.000000000000000000, 0.000000000000000000 ) ) ;
#29315 = CARTESIAN_POINT ( 'NONE',  ( -144.3570736234661638, 5.598654528085804216, 7.705886871421366635 ) ) ;
#29316 = CARTESIAN_POINT ( 'NONE',  ( -74.99999999999998579, 50.00000000000000000, -9.500000000000000000 ) ) ;
#29317 = PRESENTATION_LAYER_ASSIGNMENT (  '', '', ( #11348 ) ) ;
#29318 = CARTESIAN_POINT ( 'NONE',  ( 8.102448949553181734, 138.9949999999999761, -5.886773742842746238 ) ) ;
#29319 = CARTESIAN_POINT ( 'NONE',  ( -80.90707362346614673, -3.094860106618429807, 9.524999999999991473 ) ) ;
#29320 = ORIENTED_EDGE ( 'NONE', *, *, #6946, .F. ) ;
#29321 = CARTESIAN_POINT ( 'NONE',  ( 34.99999999999999289, 99.99999999999998579, -7.500000000000000000 ) ) ;
#29322 = DIRECTION ( 'NONE',  ( -1.000000000000000000, 0.000000000000000000, 0.000000000000000000 ) ) ;
#29323 =( GEOMETRIC_REPRESENTATION_CONTEXT ( 3 ) GLOBAL_UNCERTAINTY_ASSIGNED_CONTEXT ( ( #24844 ) ) GLOBAL_UNIT_ASSIGNED_CONTEXT ( ( #65869, #46180, #34537 ) ) REPRESENTATION_CONTEXT ( 'NONE', 'WORKASPACE' ) );
#29324 = CARTESIAN_POINT ( 'NONE',  ( 6.000000000000017764, 43.00000000000000000, -35.50000000000000000 ) ) ;
#29326 = FACE_OUTER_BOUND ( 'NONE', #20485, .T. ) ;
#29325 = FACE_OUTER_BOUND ( 'NONE', #16935, .T. ) ;
#29327 = CARTESIAN_POINT ( 'NONE',  ( -121.5549999999999926, 0.000000000000000000, 8.024999999999991473 ) ) ;
#29328 = CARTESIAN_POINT ( 'NONE',  ( 5.000000000000000000, 6.123233995736766282E-16, 0.2500000000000011102 ) ) ;
#29329 = CARTESIAN_POINT ( 'NONE',  ( 24.58168140846667526, 25.30925735143623356, -27.43541942659303956 ) ) ;
#29330 = CARTESIAN_POINT ( 'NONE',  ( -10.01517768586949231, 113.1949999999999790, -6.132527647946036459E-16 ) ) ;
#29331 = CARTESIAN_POINT ( 'NONE',  ( -132.1449999999999818, -4.716976649647092401, 6.492361379858946790 ) ) ;
#29332 = CARTESIAN_POINT ( 'NONE',  ( -118.7950000000000017, 2.607480562269069324, -8.024999999999993250 ) ) ;
#29333 = CIRCLE ( 'NONE', #3491, 0.5000000000000004441 ) ;
#29334 = CARTESIAN_POINT ( 'NONE',  ( 72.49999999999998579, 119.9999999999997868, -9.500000000000000000 ) ) ;
#29335 = EDGE_CURVE ( 'NONE', #51718, #34770, #38110, .T. ) ;
#29336 = ORIENTED_EDGE ( 'NONE', *, *, #4864, .T. ) ;
#29337 =( BOUNDED_SURFACE ( )  B_SPLINE_SURFACE ( 3, 2, ( 
 ( #44281, #29424, #40034 ),
 ( #6937, #55475, #55818 ),
 ( #6568, #12905, #34697 ),
 ( #56155, #49524, #1252 ),
 ( #1936, #17528, #38998 ),
 ( #60391, #61094, #44960 ),
 ( #12195, #33668, #23136 ),
 ( #7980, #55110, #34370 ),
 ( #1608, #50896, #45659 ),
 ( #28362, #44626, #66022 ),
 ( #9030, #30813, #47397 ),
 ( #56506, #52313, #46716 ) ),
 .UNSPECIFIED., .F., .F., .F. ) 
 B_SPLINE_SURFACE_WITH_KNOTS ( ( 4, 2, 2, 2, 2, 4 ),
 ( 3, 3 ),
 ( -8.673617379884035472E-18, 0.001550269635854629969, 0.002325404453781949182, 0.003100539271709268612, 0.004650808907563907038, 0.006201078543418545898 ),
 ( 0.000000000000000000, 1.000000000000000000 ),
 .UNSPECIFIED. ) 
 GEOMETRIC_REPRESENTATION_ITEM ( )  RATIONAL_B_SPLINE_SURFACE ( (
 ( 1.000000000000000000, 0.8674236696762899212, 1.000000000000000000),
 ( 1.000000000000000000, 0.8645660010316111865, 1.000000000000000000),
 ( 1.000000000000000000, 0.8607579482992175901, 1.000000000000000000),
 ( 1.000000000000000000, 0.8539431028568349458, 1.000000000000000000),
 ( 1.000000000000000000, 0.8514892559288537166, 1.000000000000000000),
 ( 1.000000000000000000, 0.8463012804488235785, 1.000000000000000000),
 ( 1.000000000000000000, 0.8435608369020011210, 1.000000000000000000),
 ( 1.000000000000000000, 0.8352445106661940954, 1.000000000000000000),
 ( 1.000000000000000000, 0.8295255392545153317, 1.000000000000000000),
 ( 1.000000000000000000, 0.8186818959322059719, 1.000000000000000000),
 ( 1.000000000000000000, 0.8135412794198538800, 1.000000000000000000),
 ( 1.000000000000000000, 0.8093049424017615401, 1.000000000000000000) ) ) 
 REPRESENTATION_ITEM ( '' )  SURFACE ( )  );
#29338 = CARTESIAN_POINT ( 'NONE',  ( 20.71231517720798010, 146.9999999999999716, -7.000000000000000000 ) ) ;
#29339 = CARTESIAN_POINT ( 'NONE',  ( -121.9429263765338050, 0.000000000000000000, 9.524999999999991473 ) ) ;
#29340 = CARTESIAN_POINT ( 'NONE',  ( -171.5929263765338249, -3.094860106618431139, -9.524999999999991473 ) ) ;
#29341 = CARTESIAN_POINT ( 'NONE',  ( -51.14499999999999602, -4.716976649647092401, 6.492361379858946790 ) ) ;
#29342 = STYLED_ITEM ( 'NONE', ( #11507 ), #11509 ) ;
#29343 = DIRECTION ( 'NONE',  ( -1.000000000000000000, 0.000000000000000000, 0.000000000000000000 ) ) ;
#29344 = DIRECTION ( 'NONE',  ( 0.000000000000000000, 1.000000000000000000, 0.000000000000000000 ) ) ;
#29345 = LINE ( 'NONE', #23383, #49281 ) ;
#29346 = CARTESIAN_POINT ( 'NONE',  ( -3.414918479307654575, -7.000000000000001776, 0.7696370661448970196 ) ) ;
#29347 = CARTESIAN_POINT ( 'NONE',  ( -98.39292637653380780, 8.102448949553176405, 5.886773742842740909 ) ) ;
#29348 = APPLICATION_PROTOCOL_DEFINITION ( 'draft international standard', 'automotive_design', 1998, #50483 ) ;
#29349 =( NAMED_UNIT ( * ) PLANE_ANGLE_UNIT ( ) SI_UNIT ( $, .RADIAN. ) );
#29350 = SURFACE_SIDE_STYLE ('',( #24089 ) ) ;
#29351 = DIRECTION ( 'NONE',  ( 0.000000000000000000, -1.000000000000000000, -0.000000000000000000 ) ) ;
#29352 =( LENGTH_UNIT ( ) NAMED_UNIT ( * ) SI_UNIT ( .MILLI., .METRE. ) );
#29353 = CARTESIAN_POINT ( 'NONE',  ( -40.99999999999998579, 107.7459666864129417, 3.076101031310321421 ) ) ;
#29354 = AXIS2_PLACEMENT_3D ( 'NONE', #67696, #14572, #3993 ) ;
#29355 = CARTESIAN_POINT ( 'NONE',  ( -16.75000000000000000, -3.000000000000000000, 20.00000000000000000 ) ) ;
#29356 = UNCERTAINTY_MEASURE_WITH_UNIT (LENGTH_MEASURE( 1.000000000000000082E-05 ), #60467, 'distance_accuracy_value', 'NONE');
#29357 = VERTEX_POINT ( 'NONE', #59448 ) ;
#29358 = CARTESIAN_POINT ( 'NONE',  ( -65.49999999999997158, -1.956686671034893189E-14, 12.00000000000000000 ) ) ;
#29359 = EDGE_CURVE ( 'NONE', #30684, #1198, #15899, .T. ) ;
#29360 = ORIENTED_EDGE ( 'NONE', *, *, #37502, .F. ) ;
#29361 = CARTESIAN_POINT ( 'NONE',  ( -63.44292637653379785, -1.166476076187852838E-15, -9.524999999999991473 ) ) ;
#29362 = COLOUR_RGB ( '', 0.72549020, 0.75294118, 0.79215686) ;
#29363 = CARTESIAN_POINT ( 'NONE',  ( 6.826472737025121695, 132.6070736234661638, -4.959722759717905660 ) ) ;
#29364 = AXIS2_PLACEMENT_3D ( 'NONE', #66433, #61156, #17588 ) ;
#29365 = CARTESIAN_POINT ( 'NONE',  ( -25.21060798583054563, 4.336808689942018722E-16, 0.000000000000000000 ) ) ;
#29366 = AXIS2_PLACEMENT_3D ( 'NONE', #34859, #17676, #39145 ) ;
#29367 = FACE_OUTER_BOUND ( 'NONE', #58383, .T. ) ;
#29368 = ORIENTED_EDGE ( 'NONE', *, *, #17277, .F. ) ;
#29369 = CARTESIAN_POINT ( 'NONE',  ( -93.74292637653380211, -5.598654528085803328, -7.705886871421366635 ) ) ;
#29370 = EDGE_CURVE ( 'NONE', #57245, #2500, #28163, .T. ) ;
#29371 = CARTESIAN_POINT ( 'NONE',  ( -104.9070736234671273, -3.094860106602564720, 9.525000000011518253 ) ) ;
#29372 = LINE ( 'NONE', #56109, #21648 ) ;
#29373 = AXIS2_PLACEMENT_3D ( 'NONE', #46825, #36613, #4519 ) ;
#29374 = ADVANCED_FACE ( 'NONE', ( #317 ), #5293, .T. ) ;
#29375 = DIRECTION ( 'NONE',  ( 0.000000000000000000, 0.000000000000000000, -1.000000000000000000 ) ) ;
#29376 = CARTESIAN_POINT ( 'NONE',  ( -78.44499999999999318, 0.000000000000000000, 8.024999999999991473 ) ) ;
#29377 = ORIENTED_EDGE ( 'NONE', *, *, #19280, .T. ) ;
#29378 =( LENGTH_UNIT ( ) NAMED_UNIT ( * ) SI_UNIT ( .MILLI., .METRE. ) );
#29379 = CIRCLE ( 'NONE', #53006, 9.499999999999994671 ) ;
#29380 = DIRECTION ( 'NONE',  ( 0.000000000000000000, 0.000000000000000000, 1.000000000000000000 ) ) ;
#29381 = ADVANCED_FACE ( 'NONE', ( #64408 ), #64756, .T. ) ;
#29382 = AXIS2_PLACEMENT_3D ( 'NONE', #27244, #48432, #11788 ) ;
#29383 = DIRECTION ( 'NONE',  ( -0.000000000000000000, -1.000000000000000000, -0.000000000000000000 ) ) ;
#29384 = ORIENTED_EDGE ( 'NONE', *, *, #18364, .F. ) ;
#29385 = CARTESIAN_POINT ( 'NONE',  ( -75.89292637653379359, -8.102448949553174629, -5.886773742842741797 ) ) ;
#29386 = DIRECTION ( 'NONE',  ( 0.000000000000000000, 0.000000000000000000, -1.000000000000000000 ) ) ;
#29387 = CIRCLE ( 'NONE', #68744, 0.2500000000000002220 ) ;
#29388 = AXIS2_PLACEMENT_3D ( 'NONE', #27662, #16489, #65325 ) ;
#29389 = ADVANCED_FACE ( 'NONE', ( #27088 ), #44037, .F. ) ;
#29390 = CARTESIAN_POINT ( 'NONE',  ( -8.082903768654762899, 3.463586619550771876E-15, 1.082903768654759125 ) ) ;
#29391 = EDGE_LOOP ( 'NONE', ( #30415, #36263, #55599, #3741 ) ) ;
#29392 = AXIS2_PLACEMENT_3D ( 'NONE', #17870, #11201, #39015 ) ;
#29393 = VERTEX_POINT ( 'NONE', #33096 ) ;
#29394 = CARTESIAN_POINT ( 'NONE',  ( -195.0000000000000000, 0.000000000000000000, 9.524999999999991473 ) ) ;
#29395 =( NAMED_UNIT ( * ) PLANE_ANGLE_UNIT ( ) SI_UNIT ( $, .RADIAN. ) );
#29396 = CARTESIAN_POINT ( 'NONE',  ( -9.250000000000003553, 27.74999999999998934, 3.750000000000000000 ) ) ;
#29397 = CARTESIAN_POINT ( 'NONE',  ( -172.1070736234661069, 8.102448949553171076, -5.886773742842744461 ) ) ;
#29398 = PRESENTATION_LAYER_ASSIGNMENT (  '', '', ( #64204 ) ) ;
#29399 = CARTESIAN_POINT ( 'NONE',  ( -177.4429263765338192, -1.166476076187852838E-15, -9.524999999999991473 ) ) ;
#29400 = CARTESIAN_POINT ( 'NONE',  ( 3.094860106618431583, 111.0949999999999704, 9.525000000000000355 ) ) ;
#29401 = CARTESIAN_POINT ( 'NONE',  ( -110.1570736234661751, -9.058813317711329915, -2.943386871421370898 ) ) ;
#29402 = AXIS2_PLACEMENT_3D ( 'NONE', #56288, #66871, #8120 ) ;
#29403 =( REPRESENTATION_RELATIONSHIP ('NONE','NONE', #5102, #60355 ) REPRESENTATION_RELATIONSHIP_WITH_TRANSFORMATION ( #20896 )SHAPE_REPRESENTATION_RELATIONSHIP( ) );
#29404 = CARTESIAN_POINT ( 'NONE',  ( -1.233556390955557802, 2.406758536254373748, 6.999999999999999112 ) ) ;
#29405 = CARTESIAN_POINT ( 'NONE',  ( -84.50707362346616947, 8.102448949553176405, 5.886773742842740909 ) ) ;
#29406 = ORIENTED_EDGE ( 'NONE', *, *, #54395, .F. ) ;
#29407 = CIRCLE ( 'NONE', #61995, 0.5000000000000004441 ) ;
#29408 = CARTESIAN_POINT ( 'NONE',  ( 5.603096392576905949, -1.514639124457112240, -8.295152368350905192 ) ) ;
#29409 = SURFACE_SIDE_STYLE ('',( #23439 ) ) ;
#29410 = LINE ( 'NONE', #51232, #18861 ) ;
#29411 = FILL_AREA_STYLE ('',( #43912 ) ) ;
#29412 = CIRCLE ( 'NONE', #68758, 5.000000000000000000 ) ;
#29413 = CARTESIAN_POINT ( 'NONE',  ( -146.1549999999999727, 7.632228543268600340, 2.479861379858949277 ) ) ;
#29414 = CYLINDRICAL_SURFACE ( 'NONE', #69012, 9.524999999999991473 ) ;
#29415 = SURFACE_STYLE_FILL_AREA ( #3333 ) ;
#29416 = VECTOR ( 'NONE', #33065, 1000.000000000000000 ) ;
#29417 = CARTESIAN_POINT ( 'NONE',  ( -161.6950000000000216, -8.437984349512085203, 5.166775262442717831E-16 ) ) ;
#29418 = CARTESIAN_POINT ( 'NONE',  ( -157.6449999999999818, 4.716976649647091513, -6.492361379858946790 ) ) ;
#29419 = ORIENTED_EDGE ( 'NONE', *, *, #36591, .F. ) ;
#29420 = CARTESIAN_POINT ( 'NONE',  ( -67.79292637653381348, -3.094860106618429807, 9.524999999999991473 ) ) ;
#29421 = DIRECTION ( 'NONE',  ( 0.000000000000000000, 1.000000000000000000, 0.000000000000000000 ) ) ;
#29422 = CARTESIAN_POINT ( 'NONE',  ( -123.1429263765338078, 5.598654528085800663, -7.705886871421367523 ) ) ;
#29423 = CARTESIAN_POINT ( 'NONE',  ( -75.80499999999997840, -8.437984349512085203, 5.166775262442717831E-16 ) ) ;
#29424 = CARTESIAN_POINT ( 'NONE',  ( -34.48878133304234694, -10.53184416402257106, 3.891476709836707126 ) ) ;
#29425 = CIRCLE ( 'NONE', #37326, 0.2500000000000002220 ) ;
#29426 = SURFACE_SIDE_STYLE ('',( #62128 ) ) ;
#29427 = CARTESIAN_POINT ( 'NONE',  ( -68.39499999999996760, -6.826472737025113702, -4.959722759717900331 ) ) ;
#29428 = CARTESIAN_POINT ( 'NONE',  ( -8.102448949553181734, 147.0049999999999955, -5.886773742842749790 ) ) ;
#29429 = CARTESIAN_POINT ( 'NONE',  ( 17.75000000000000711, 30.99999999999999289, -4.000000000000000000 ) ) ;
#29430 = AXIS2_PLACEMENT_3D ( 'NONE', #67090, #50917, #6586 ) ;
#29431 = CARTESIAN_POINT ( 'NONE',  ( 0.000000000000000000, 2.000000000000000444, 0.000000000000000000 ) ) ;
#29432 = FILL_AREA_STYLE ('',( #7989 ) ) ;
#29433 = CARTESIAN_POINT ( 'NONE',  ( 55.40000000000000568, 11.99999999999999822, -4.000000000000000000 ) ) ;
#29434 = MECHANICAL_DESIGN_GEOMETRIC_PRESENTATION_REPRESENTATION (  '', ( #22724 ), #1318 ) ;
#29435 = CIRCLE ( 'NONE', #41847, 0.5000000000000004441 ) ;
#29436 = CYLINDRICAL_SURFACE ( 'NONE', #23596, 0.5000000000000004441 ) ;
#29437 = CARTESIAN_POINT ( 'NONE',  ( 7.794228634059946259, 2.500000000000000000, -4.500000000000001776 ) ) ;
#29438 = CIRCLE ( 'NONE', #28309, 0.5000000000000004441 ) ;
#29439 = DIRECTION ( 'NONE',  ( -0.4468085106382997385, -0.000000000000000000, -0.8946296187927071930 ) ) ;
#29440 = EDGE_CURVE ( 'NONE', #41529, #49536, #11974, .T. ) ;
#29441 = LINE ( 'NONE', #55124, #57701 ) ;
#29442 = DIRECTION ( 'NONE',  ( 0.000000000000000000, 0.000000000000000000, 1.000000000000000000 ) ) ;
#29443 = ORIENTED_EDGE ( 'NONE', *, *, #40846, .F. ) ;
#29444 = VERTEX_POINT ( 'NONE', #48966 ) ;
#29445 = CARTESIAN_POINT ( 'NONE',  ( -60.50707362346616236, 8.102448949553176405, 5.886773742842740909 ) ) ;
#29446 = VECTOR ( 'NONE', #1658, 1000.000000000000000 ) ;
#29447 = EDGE_CURVE ( 'NONE', #20404, #41337, #21489, .T. ) ;
#29448 =( GEOMETRIC_REPRESENTATION_CONTEXT ( 3 ) GLOBAL_UNCERTAINTY_ASSIGNED_CONTEXT ( ( #44029 ) ) GLOBAL_UNIT_ASSIGNED_CONTEXT ( ( #14697, #16708, #36171 ) ) REPRESENTATION_CONTEXT ( 'NONE', 'WORKASPACE' ) );
#29449 = ADVANCED_FACE ( 'NONE', ( #32372 ), #43686, .T. ) ;
#29450 = DIRECTION ( 'NONE',  ( 0.000000000000000000, 1.000000000000000000, 0.000000000000000000 ) ) ;
#29451 = EDGE_CURVE ( 'NONE', #40838, #5687, #68911, .T. ) ;
#29452 = FILL_AREA_STYLE_COLOUR ( '', #27352 ) ;
#29453 = ORIENTED_EDGE ( 'NONE', *, *, #24064, .T. ) ;
#29454 = VERTEX_POINT ( 'NONE', #61520 ) ;
#29455 = FILL_AREA_STYLE ('',( #7648 ) ) ;
#29456 = FACE_OUTER_BOUND ( 'NONE', #12509, .T. ) ;
#29457 = AXIS2_PLACEMENT_3D ( 'NONE', #47291, #31394, #5022 ) ;
#29458 = EDGE_CURVE ( 'NONE', #69192, #10939, #30660, .T. ) ;
#29459 = ORIENTED_EDGE ( 'NONE', *, *, #32623, .T. ) ;
#29460 = CARTESIAN_POINT ( 'NONE',  ( 24.75000000000000355, 36.75000000000000000, -3.000000000000000000 ) ) ;
#29461 = ORIENTED_EDGE ( 'NONE', *, *, #13741, .F. ) ;
#29462 = CIRCLE ( 'NONE', #40747, 0.2500000000000002220 ) ;
#29463 = EDGE_CURVE ( 'NONE', #12490, #11857, #12689, .T. ) ;
#29464 = CARTESIAN_POINT ( 'NONE',  ( -34.99999999999999289, 99.99999999999998579, 7.500000000000000000 ) ) ;
#29465 = PRESENTATION_STYLE_ASSIGNMENT (( #45692 ) ) ;
#29466 = CARTESIAN_POINT ( 'NONE',  ( -106.9449999999999790, -9.827790563157499189E-16, -8.024999999999991473 ) ) ;
#29467 = VERTEX_POINT ( 'NONE', #7043 ) ;
#29468 = AXIS2_PLACEMENT_3D ( 'NONE', #28170, #27829, #59510 ) ;
#29469 = CARTESIAN_POINT ( 'NONE',  ( -4.251564707942288912, 110.4999999999999858, -8.568970148020829569 ) ) ;
#29470 = SURFACE_SIDE_STYLE ('',( #40397 ) ) ;
#29471 = CARTESIAN_POINT ( 'NONE',  ( -12.48379447375185336, -11.19212576109403656, -4.332794091909712542 ) ) ;
#29472 = EDGE_CURVE ( 'NONE', #8712, #45556, #56519, .T. ) ;
#29473 = VERTEX_POINT ( 'NONE', #18305 ) ;
#29474 = CARTESIAN_POINT ( 'NONE',  ( -4.716976649647097730, 147.2429263765338305, -6.492361379858953896 ) ) ;
#29475 = DIRECTION ( 'NONE',  ( 0.000000000000000000, 0.000000000000000000, -1.000000000000000000 ) ) ;
#29476 = VECTOR ( 'NONE', #28601, 1000.000000000000000 ) ;
#29477 = DIRECTION ( 'NONE',  ( -1.239088197126290817E-16, 0.000000000000000000, -1.000000000000000000 ) ) ;
#29478 = FACE_BOUND ( 'NONE', #33701, .T. ) ;
#29479 = ORIENTED_EDGE ( 'NONE', *, *, #37400, .F. ) ;
#29480 = DIRECTION ( 'NONE',  ( 0.000000000000000000, 0.000000000000000000, -1.000000000000000000 ) ) ;
#29481 = VERTEX_POINT ( 'NONE', #44391 ) ;
#29482 =( NAMED_UNIT ( * ) PLANE_ANGLE_UNIT ( ) SI_UNIT ( $, .RADIAN. ) );
#29483 = PRESENTATION_STYLE_ASSIGNMENT (( #39731 ) ) ;
#29484 = DIRECTION ( 'NONE',  ( 0.000000000000000000, 0.000000000000000000, 1.000000000000000000 ) ) ;
#29485 = DIRECTION ( 'NONE',  ( 1.000000000000000000, 1.009293658750142399E-15, 0.000000000000000000 ) ) ;
#29486 = AXIS2_PLACEMENT_3D ( 'NONE', #13396, #30608, #2450 ) ;
#29488 = CARTESIAN_POINT ( 'NONE',  ( -136.7050000000000125, 2.607480562269073321, 8.024999999999991473 ) ) ;
#29487 = AXIS2_PLACEMENT_3D ( 'NONE', #63544, #36143, #41783 ) ;
#29489 = FILL_AREA_STYLE ('',( #28787 ) ) ;
#29490 = DIRECTION ( 'NONE',  ( -1.000000000000000000, 0.000000000000000000, 0.000000000000000000 ) ) ;
#29491 = EDGE_LOOP ( 'NONE', ( #30931, #56206, #35863, #5136, #13205 ) ) ;
#29492 = SURFACE_STYLE_FILL_AREA ( #25254 ) ;
#29493 = CIRCLE ( 'NONE', #68832, 0.5000000000000004441 ) ;
#29494 = LINE ( 'NONE', #14720, #24887 ) ;
#29495 = CARTESIAN_POINT ( 'NONE',  ( -3.414270897520784942, -1.730686724748536465, 7.000000000000000000 ) ) ;
#29496 = ORIENTED_EDGE ( 'NONE', *, *, #50915, .T. ) ;
#29497 =( GEOMETRIC_REPRESENTATION_CONTEXT ( 3 ) GLOBAL_UNCERTAINTY_ASSIGNED_CONTEXT ( ( #33538 ) ) GLOBAL_UNIT_ASSIGNED_CONTEXT ( ( #49740, #3218, #28598 ) ) REPRESENTATION_CONTEXT ( 'NONE', 'WORKASPACE' ) );
#29498 = ORIENTED_EDGE ( 'NONE', *, *, #67674, .T. ) ;
#29499 =( NAMED_UNIT ( * ) SI_UNIT ( $, .STERADIAN. ) SOLID_ANGLE_UNIT ( ) );
#29500 = CARTESIAN_POINT ( 'NONE',  ( -13.50000000000000355, 28.24999999999998934, -3.750000000000000000 ) ) ;
#29501 = CARTESIAN_POINT ( 'NONE',  ( 6.413663052920311358, -2.499999999999998668, 2.891209729714698806 ) ) ;
#29502 = CARTESIAN_POINT ( 'NONE',  ( -50.75499999999999545, 4.716976649647091513, -6.492361379858946790 ) ) ;
#29503 = EDGE_LOOP ( 'NONE', ( #3839, #38595, #32082, #39140 ) ) ;
#29504 = AXIS2_PLACEMENT_3D ( 'NONE', #4813, #52344, #47800 ) ;
#29505 = CYLINDRICAL_SURFACE ( 'NONE', #6823, 0.5000000000000004441 ) ;
#29506 =( NAMED_UNIT ( * ) SI_UNIT ( $, .STERADIAN. ) SOLID_ANGLE_UNIT ( ) );
#29507 = CARTESIAN_POINT ( 'NONE',  ( -56.75707362346615525, -5.598654528085801552, 7.705886871421367523 ) ) ;
#29508 = MECHANICAL_DESIGN_GEOMETRIC_PRESENTATION_REPRESENTATION (  '', ( #53134 ), #24994 ) ;
#29509 = FILL_AREA_STYLE_COLOUR ( '', #55423 ) ;
#29510 = CARTESIAN_POINT ( 'NONE',  ( -177.0570736234661808, 0.000000000000000000, 9.524999999999991473 ) ) ;
#29511 = EDGE_LOOP ( 'NONE', ( #53368, #12081, #50018, #43569 ) ) ;
#29512 = ADVANCED_FACE ( 'NONE', ( #45755 ), #29532, .T. ) ;
#29513 = VECTOR ( 'NONE', #33139, 1000.000000000000000 ) ;
#29514 = CYLINDRICAL_SURFACE ( 'NONE', #23468, 1.000000000000000888 ) ;
#29515 = SURFACE_STYLE_FILL_AREA ( #45736 ) ;
#29516 = CARTESIAN_POINT ( 'NONE',  ( -102.2049999999999983, -2.607480562269071545, -8.024999999999991473 ) ) ;
#29517 = CARTESIAN_POINT ( 'NONE',  ( -30.38025804287905629, -8.499999999999996447, 0.06931351858119244591 ) ) ;
#29518 = LINE ( 'NONE', #2374, #21329 ) ;
#29519 = CIRCLE ( 'NONE', #46441, 0.5000000000000004441 ) ;
#29520 = CARTESIAN_POINT ( 'NONE',  ( -98.69499999999999318, -8.437984349512086979, 5.166775262442717831E-16 ) ) ;
#29521 = CARTESIAN_POINT ( 'NONE',  ( -10.01517768586949231, 117.3049999999999784, -6.132527647946036459E-16 ) ) ;
#29522 = CARTESIAN_POINT ( 'NONE',  ( -82.34499999999998465, 7.632228543268599452, -2.479861379858951942 ) ) ;
#29523 = CIRCLE ( 'NONE', #50866, 0.2500000000000002220 ) ;
#29524 = DIRECTION ( 'NONE',  ( 0.000000000000000000, 0.000000000000000000, 1.000000000000000000 ) ) ;
#29525 = DIRECTION ( 'NONE',  ( -0.000000000000000000, -0.000000000000000000, -1.000000000000000000 ) ) ;
#29526 = ORIENTED_EDGE ( 'NONE', *, *, #25869, .F. ) ;
#29527 = CARTESIAN_POINT ( 'NONE',  ( -112.7929263765337851, -3.094860106618429807, 9.524999999999991473 ) ) ;
#29528 = CARTESIAN_POINT ( 'NONE',  ( -133.9449999999999932, -9.827790563157499189E-16, -8.024999999999991473 ) ) ;
#29529 = DIRECTION ( 'NONE',  ( 1.000000000000000000, 0.000000000000000000, 0.000000000000000000 ) ) ;
#29530 =( GEOMETRIC_REPRESENTATION_CONTEXT ( 3 ) GLOBAL_UNCERTAINTY_ASSIGNED_CONTEXT ( ( #39198 ) ) GLOBAL_UNIT_ASSIGNED_CONTEXT ( ( #5256, #58393, #26704 ) ) REPRESENTATION_CONTEXT ( 'NONE', 'WORKASPACE' ) );
#29531 = ADVANCED_FACE ( 'NONE', ( #34468 ), #17950, .T. ) ;
#29532 = PLANE ( 'NONE',  #19474 ) ;
#29533 = CARTESIAN_POINT ( 'NONE',  ( -60.00000000000000000, -2.024042244987997205E-14, -6.500000000000000000 ) ) ;
#29534 = VERTEX_POINT ( 'NONE', #47149 ) ;
#29536 = ORIENTED_EDGE ( 'NONE', *, *, #17635, .F. ) ;
#29535 = CIRCLE ( 'NONE', #23915, 1.000000000000000888 ) ;
#29537 = AXIS2_PLACEMENT_3D ( 'NONE', #67022, #51520, #41005 ) ;
#29538 = CARTESIAN_POINT ( 'NONE',  ( -80.49999999999998579, 50.00000000000000000, 6.500000000000000000 ) ) ;
#29539 = LINE ( 'NONE', #29172, #45479 ) ;
#29540 = ADVANCED_FACE ( 'NONE', ( #24949 ), #3814, .T. ) ;
#29541 = MECHANICAL_DESIGN_GEOMETRIC_PRESENTATION_REPRESENTATION (  '', ( #54245 ), #65501 ) ;
#29542 = CARTESIAN_POINT ( 'NONE',  ( 22.75000000000000711, 37.00000000000000000, -3.750000000000000000 ) ) ;
#29543 = CARTESIAN_POINT ( 'NONE',  ( 2.418047948263831071, 2.101261491288920702, 7.000000000000001776 ) ) ;
#29544 = DIRECTION ( 'NONE',  ( 1.000000000000000000, 0.000000000000000000, 0.000000000000000000 ) ) ;
#29545 = DIRECTION ( 'NONE',  ( -1.000000000000000000, 0.000000000000000000, 0.000000000000000000 ) ) ;
#29546 = ORIENTED_EDGE ( 'NONE', *, *, #46520, .F. ) ;
#29547 = CARTESIAN_POINT ( 'NONE',  ( -135.5049999999999670, -6.826472737025113702, -4.959722759717900331 ) ) ;
#29548 = EDGE_LOOP ( 'NONE', ( #21186, #39817, #11942, #62591 ) ) ;
#29549 = CARTESIAN_POINT ( 'NONE',  ( -125.7570736234661695, -5.598654528085801552, 7.705886871421367523 ) ) ;
#29550 = ORIENTED_EDGE ( 'NONE', *, *, #32971, .T. ) ;
#29551 = CARTESIAN_POINT ( 'NONE',  ( -172.3429263765338249, -9.058813317711329915, 2.943386871421371787 ) ) ;
#29552 = DIRECTION ( 'NONE',  ( -0.000000000000000000, -0.000000000000000000, 1.000000000000000000 ) ) ;
#29553 =( GEOMETRIC_REPRESENTATION_CONTEXT ( 3 ) GLOBAL_UNCERTAINTY_ASSIGNED_CONTEXT ( ( #44829 ) ) GLOBAL_UNIT_ASSIGNED_CONTEXT ( ( #25654, #9854, #5236 ) ) REPRESENTATION_CONTEXT ( 'NONE', 'WORKASPACE' ) );
#29554 = EDGE_LOOP ( 'NONE', ( #50616, #1805, #10202, #45839 ) ) ;
#29555 = EDGE_CURVE ( 'NONE', #42883, #33741, #9494, .T. ) ;
#29556 = DIRECTION ( 'NONE',  ( 0.07854820085872887825, 0.9914125719358882760, 0.1045528208578022367 ) ) ;
#29557 = FACE_OUTER_BOUND ( 'NONE', #18066, .T. ) ;
#29558 = CARTESIAN_POINT ( 'NONE',  ( 10.01517768586949231, 135.6949999999999932, 1.839758294383810543E-15 ) ) ;
#29559 = VERTEX_POINT ( 'NONE', #46822 ) ;
#29560 = DIRECTION ( 'NONE',  ( 0.000000000000000000, -1.000000000000000000, 0.000000000000000000 ) ) ;
#29561 = CARTESIAN_POINT ( 'NONE',  ( -8.102448949553179958, 144.0049999999999955, -5.886773742842749790 ) ) ;
#29562 = FACE_OUTER_BOUND ( 'NONE', #24506, .T. ) ;
#29563 = EDGE_CURVE ( 'NONE', #61539, #4364, #44231, .T. ) ;
#29564 = CARTESIAN_POINT ( 'NONE',  ( 41.61090298506073992, 107.5097581389851911, -4.000000003092934797 ) ) ;
#29565 = ORIENTED_EDGE ( 'NONE', *, *, #17680, .T. ) ;
#29566 = CARTESIAN_POINT ( 'NONE',  ( 7.632228543268608334, 119.3429263765338249, -2.479861379858951942 ) ) ;
#29567 = DIRECTION ( 'NONE',  ( 0.000000000000000000, 0.000000000000000000, 1.000000000000000000 ) ) ;
#29568 =( NAMED_UNIT ( * ) PLANE_ANGLE_UNIT ( ) SI_UNIT ( $, .RADIAN. ) );
#29569 = AXIS2_PLACEMENT_3D ( 'NONE', #1747, #3476, #67199 ) ;
#29570 = AXIS2_PLACEMENT_3D ( 'NONE', #68922, #58026, #41172 ) ;
#29571 = DIRECTION ( 'NONE',  ( 0.000000000000000000, 0.000000000000000000, 1.000000000000000000 ) ) ;
#29572 = DIRECTION ( 'NONE',  ( 1.000000000000000000, 0.000000000000000000, 0.000000000000000000 ) ) ;
#29573 = VERTEX_POINT ( 'NONE', #40819 ) ;
#29574 = CARTESIAN_POINT ( 'NONE',  ( -1.805736402306165722, -9.000000000000007105, 0.1687517039304795019 ) ) ;
#29575 = ORIENTED_EDGE ( 'NONE', *, *, #651, .T. ) ;
#29576 = DIRECTION ( 'NONE',  ( -0.000000000000000000, 1.000000000000000000, -0.000000000000000000 ) ) ;
#29577 = CYLINDRICAL_SURFACE ( 'NONE', #43505, 8.025000000000000355 ) ;
#29578 = CARTESIAN_POINT ( 'NONE',  ( -4.750000000000002665, 24.74999999999998579, 3.750000000000000000 ) ) ;
#29579 = CARTESIAN_POINT ( 'NONE',  ( -163.5550000000000068, 0.000000000000000000, 8.024999999999991473 ) ) ;
#29580 = VERTEX_POINT ( 'NONE', #30206 ) ;
#29581 =( NAMED_UNIT ( * ) PLANE_ANGLE_UNIT ( ) SI_UNIT ( $, .RADIAN. ) );
#29582 = VECTOR ( 'NONE', #67485, 1000.000000000000000 ) ;
#29583 = FILL_AREA_STYLE_COLOUR ( '', #50995 ) ;
#29584 = DIRECTION ( 'NONE',  ( -0.000000000000000000, -1.000000000000000000, -0.000000000000000000 ) ) ;
#29585 = CARTESIAN_POINT ( 'NONE',  ( 44.99999999999999289, 9.801220280675213559, -6.455927277197755387 ) ) ;
#29586 = ORIENTED_EDGE ( 'NONE', *, *, #31239, .F. ) ;
#29587 = VERTEX_POINT ( 'NONE', #53089 ) ;
#29588 = CARTESIAN_POINT ( 'NONE',  ( -195.0000000000000000, 0.000000000000000000, 0.000000000000000000 ) ) ;
#29589 = FILL_AREA_STYLE_COLOUR ( '', #12042 ) ;
#29590 = CARTESIAN_POINT ( 'NONE',  ( 60.99999999999998579, 50.00000000000000000, -7.500000000000000000 ) ) ;
#29591 = CARTESIAN_POINT ( 'NONE',  ( -77.15499999999998693, 7.632228543268600340, 2.479861379858949277 ) ) ;
#29592 = ORIENTED_EDGE ( 'NONE', *, *, #18557, .T. ) ;
#29593 = CARTESIAN_POINT ( 'NONE',  ( -54.44292637653380496, -1.166476076187852838E-15, -9.524999999999991473 ) ) ;
#29594 = VECTOR ( 'NONE', #30091, 1000.000000000000000 ) ;
#29596 = PRESENTATION_LAYER_ASSIGNMENT (  '', '', ( #42003 ) ) ;
#29595 = STYLED_ITEM ( 'NONE', ( #27702 ), #61678 ) ;
#29597 = DIRECTION ( 'NONE',  ( -1.000000000000000000, 0.000000000000000000, 0.000000000000000000 ) ) ;
#29598 = EDGE_CURVE ( 'NONE', #8720, #30297, #53190, .T. ) ;
#29599 =( GEOMETRIC_REPRESENTATION_CONTEXT ( 3 ) GLOBAL_UNCERTAINTY_ASSIGNED_CONTEXT ( ( #53656 ) ) GLOBAL_UNIT_ASSIGNED_CONTEXT ( ( #15595, #5010, #26465 ) ) REPRESENTATION_CONTEXT ( 'NONE', 'WORKASPACE' ) );
#29600 = CARTESIAN_POINT ( 'NONE',  ( -75.00000000000000000, 9.518682052516130199, -6.447728916822595302 ) ) ;
#29601 = ORIENTED_EDGE ( 'NONE', *, *, #37804, .T. ) ;
#29602 = DIRECTION ( 'NONE',  ( 1.000000000000000000, 0.000000000000000000, 0.000000000000000000 ) ) ;
#29603 = CARTESIAN_POINT ( 'NONE',  ( -54.05707362346618083, 0.000000000000000000, 9.524999999999991473 ) ) ;
#29604 = CIRCLE ( 'NONE', #48884, 0.4999999999999994449 ) ;
#29605 = CARTESIAN_POINT ( 'NONE',  ( -10.01517768586949231, 143.1949999999999932, -6.132527647946036459E-16 ) ) ;
#29606 = CARTESIAN_POINT ( 'NONE',  ( -102.8949999999999960, 6.826472737025116366, 4.959722759717898555 ) ) ;
#29607 = LINE ( 'NONE', #35239, #55473 ) ;
#29608 = DIRECTION ( 'NONE',  ( -1.000000000000000000, 0.000000000000000000, 0.000000000000000000 ) ) ;
#29609 = AXIS2_PLACEMENT_3D ( 'NONE', #34417, #3395, #51296 ) ;
#29610 = PRODUCT_DEFINITION ( 'UNKNOWN', '', #28138, #62047 ) ;
#29612 = CARTESIAN_POINT ( 'NONE',  ( 0.000000000000000000, 0.000000000000000000, 32.50000000000000000 ) ) ;
#29611 = CARTESIAN_POINT ( 'NONE',  ( -5.196152422706636465, -1.107695154586737063, 9.000000000000001776 ) ) ;
#29613 = EDGE_CURVE ( 'NONE', #49361, #15159, #42239, .T. ) ;
#29614 = CARTESIAN_POINT ( 'NONE',  ( -142.9429263765337907, 0.000000000000000000, 9.524999999999991473 ) ) ;
#29615 = CIRCLE ( 'NONE', #68950, 9.000000000000007105 ) ;
#29616 = SHAPE_REPRESENTATION_RELATIONSHIP ( 'NONE' , 'NONE' ,  #38844, #12828 ) ;
#29617 = CARTESIAN_POINT ( 'NONE',  ( -165.2949999999999591, -2.607480562269069768, 8.024999999999991473 ) ) ;
#29618 = VECTOR ( 'NONE', #10201, 1000.000000000000000 ) ;
#29619 = EDGE_CURVE ( 'NONE', #45200, #59828, #56582, .T. ) ;
#29620 = AXIS2_PLACEMENT_3D ( 'NONE', #11193, #53753, #5549 ) ;
#29621 = EDGE_CURVE ( 'NONE', #12107, #60087, #20005, .T. ) ;
#29622 =( NAMED_UNIT ( * ) SI_UNIT ( $, .STERADIAN. ) SOLID_ANGLE_UNIT ( ) );
#29623 = CARTESIAN_POINT ( 'NONE',  ( -20.94636006565341191, 149.9999999999999716, -9.500000000000000000 ) ) ;
#29624 = ORIENTED_EDGE ( 'NONE', *, *, #37497, .F. ) ;
#29625 = CARTESIAN_POINT ( 'NONE',  ( -12.74999999999999822, -0.9999999999999995559, 6.000000000000001776 ) ) ;
#29627 = EDGE_LOOP ( 'NONE', ( #24013, #13096, #64089, #29906 ) ) ;
#29626 = AXIS2_PLACEMENT_3D ( 'NONE', #21878, #16957, #37759 ) ;
#29628 = EDGE_CURVE ( 'NONE', #45809, #53118, #21406, .T. ) ;
#29629 =( NAMED_UNIT ( * ) PLANE_ANGLE_UNIT ( ) SI_UNIT ( $, .RADIAN. ) );
#29630 = VECTOR ( 'NONE', #63598, 1000.000000000000000 ) ;
#29631 = PRESENTATION_LAYER_ASSIGNMENT (  '', '', ( #21750 ) ) ;
#29632 = EDGE_CURVE ( 'NONE', #44394, #67626, #30859, .T. ) ;
#29633 =( LENGTH_UNIT ( ) NAMED_UNIT ( * ) SI_UNIT ( .MILLI., .METRE. ) );
#29634 = DIRECTION ( 'NONE',  ( 0.000000000000000000, -1.000000000000000000, 0.000000000000000000 ) ) ;
#29635 = CARTESIAN_POINT ( 'NONE',  ( -110.7570736234661837, -5.598654528085801552, 7.705886871421367523 ) ) ;
#29636 = EDGE_CURVE ( 'NONE', #4102, #13223, #3775, .T. ) ;
#29637 = CARTESIAN_POINT ( 'NONE',  ( -2.607480562269158586, 143.4070736234661751, 8.024999999999939959 ) ) ;
#29638 = ORIENTED_EDGE ( 'NONE', *, *, #32399, .F. ) ;
#29639 = CARTESIAN_POINT ( 'NONE',  ( -156.8050000000000068, -8.437984349512086979, 5.166775262442717831E-16 ) ) ;
#29640 = MECHANICAL_DESIGN_GEOMETRIC_PRESENTATION_REPRESENTATION (  '', ( #28514 ), #36421 ) ;
#29641 = ORIENTED_EDGE ( 'NONE', *, *, #13369, .T. ) ;
#29642 = CARTESIAN_POINT ( 'NONE',  ( -20.44220712062818635, 115.3857587453612865, -10.00000000000000000 ) ) ;
#29643 = ORIENTED_EDGE ( 'NONE', *, *, #53915, .F. ) ;
#29644 = EDGE_CURVE ( 'NONE', #7407, #49325, #66395, .T. ) ;
#29645 = COLOUR_RGB ( '', 0.31764706, 0.68627451, 0.89019608) ;
#29646 = MECHANICAL_DESIGN_GEOMETRIC_PRESENTATION_REPRESENTATION (  '', ( #28521 ), #26266 ) ;
#29647 = DIRECTION ( 'NONE',  ( 0.000000000000000000, 0.000000000000000000, 1.000000000000000000 ) ) ;
#29648 = CARTESIAN_POINT ( 'NONE',  ( 7.632228543268607446, 159.1570736234661467, 2.479861379858954606 ) ) ;
#29649 = TOROIDAL_SURFACE ( 'NONE', #38679, 17.50000000000000000, 0.5000000000000000000 ) ;
#29650 = ORIENTED_EDGE ( 'NONE', *, *, #43099, .T. ) ;
#29651 = CARTESIAN_POINT ( 'NONE',  ( 61.74999999999998579, 30.74999999999999289, -3.750000000000000000 ) ) ;
#29652 = CARTESIAN_POINT ( 'NONE',  ( 15.98999599679679839, 118.4999999999999716, -9.500000000000000000 ) ) ;
#29653 = CARTESIAN_POINT ( 'NONE',  ( -71.75499999999998124, 4.716976649647091513, -6.492361379858946790 ) ) ;
#29654 = EDGE_CURVE ( 'NONE', #30209, #28559, #26247, .T. ) ;
#29655 = DIRECTION ( 'NONE',  ( 0.000000000000000000, 0.000000000000000000, 1.000000000000000000 ) ) ;
#29656 = CARTESIAN_POINT ( 'NONE',  ( 5.598654528085809545, 137.2549999999999955, -7.705886871421373741 ) ) ;
#29657 = DIRECTION ( 'NONE',  ( 1.000000000000000000, 0.000000000000000000, 0.000000000000000000 ) ) ;
#29658 = CARTESIAN_POINT ( 'NONE',  ( 20.06812647026248086, 114.9888238951376991, 10.44321692355803144 ) ) ;
#29659 = DIRECTION ( 'NONE',  ( -1.000000000000000000, 0.000000000000000000, 0.000000000000000000 ) ) ;
#29660 = SURFACE_SIDE_STYLE ('',( #67643 ) ) ;
#29661 = VERTEX_POINT ( 'NONE', #26659 ) ;
#29663 = CARTESIAN_POINT ( 'NONE',  ( -34.99999999999992895, 109.9999999999999858, 10.00000000000000000 ) ) ;
#29662 = AXIS2_PLACEMENT_3D ( 'NONE', #67743, #14273, #63503 ) ;
#29664 = CARTESIAN_POINT ( 'NONE',  ( 74.50000000000000000, -2.220952357103124925E-14, -9.500000000000000000 ) ) ;
#29665 = CARTESIAN_POINT ( 'NONE',  ( -57.59499999999998465, 2.607480562269073321, 8.024999999999991473 ) ) ;
#29666 = EDGE_LOOP ( 'NONE', ( #18995, #28169, #29384, #68486 ) ) ;
#29667 =( BOUNDED_CURVE ( )  B_SPLINE_CURVE ( 2, ( #42601, #32685, #17252, #38018, #47909, #32003, #57445, #59084, #53473, #16556, #27041 ),
 .UNSPECIFIED., .F., .F. ) 
 B_SPLINE_CURVE_WITH_KNOTS ( ( 3, 2, 2, 2, 2, 3 ),
 ( 0.04347826086956423780, 0.04565217391304245143, 0.04782608695652066505, 0.04999999999999887174, 0.05217391304347707842, 0.05434782608695529205 ),
 .UNSPECIFIED. ) 
 CURVE ( )  GEOMETRIC_REPRESENTATION_ITEM ( )  RATIONAL_B_SPLINE_CURVE ( ( 1.000000000000021982, 0.9510565162951315488, 1.000000000000000000, 0.9510565162951535312, 1.000000000000000000, 0.9510565162951535312, 1.000000000000000000, 0.9510565162951535312, 1.000000000000000000, 0.9510565162951811757, 0.9999999999999723554 ) ) 
 REPRESENTATION_ITEM ( '' )  );
#29668 = CARTESIAN_POINT ( 'NONE',  ( -44.99999999999977263, 147.4999999999999716, -9.500000000000000000 ) ) ;
#29669 = MECHANICAL_DESIGN_GEOMETRIC_PRESENTATION_REPRESENTATION (  '', ( #63358 ), #11690 ) ;
#29670 = SURFACE_SIDE_STYLE ('',( #34250 ) ) ;
#29671 = CARTESIAN_POINT ( 'NONE',  ( -87.29292637653379927, 3.094860106618428031, -9.524999999999993250 ) ) ;
#29672 = VERTEX_POINT ( 'NONE', #63960 ) ;
#29673 = CARTESIAN_POINT ( 'NONE',  ( -49.34499999999997044, 7.632228543268599452, -2.479861379858951942 ) ) ;
#29674 =( LENGTH_UNIT ( ) NAMED_UNIT ( * ) SI_UNIT ( .MILLI., .METRE. ) );
#29675 = ORIENTED_EDGE ( 'NONE', *, *, #33462, .T. ) ;
#29676 = CARTESIAN_POINT ( 'NONE',  ( -107.6049999999999756, 6.826472737025113702, -4.959722759717902107 ) ) ;
#29677 = VERTEX_POINT ( 'NONE', #49197 ) ;
#29678 = DIRECTION ( 'NONE',  ( 0.000000000000000000, 1.350863103983176297E-16, -1.000000000000000000 ) ) ;
#29679 = FILL_AREA_STYLE ('',( #46949 ) ) ;
#29680 = CARTESIAN_POINT ( 'NONE',  ( -139.8570736234661638, -5.598654528085803328, -7.705886871421366635 ) ) ;
#29681 = CIRCLE ( 'NONE', #8350, 5.000000000000004441 ) ;
#29682 = CARTESIAN_POINT ( 'NONE',  ( -59.30707362346615952, -10.01517768586948698, 6.132527647946031529E-16 ) ) ;
#29683 = CARTESIAN_POINT ( 'NONE',  ( -10.01517768586949408, 146.1949999999999648, -6.132527647946036459E-16 ) ) ;
#29684 = CARTESIAN_POINT ( 'NONE',  ( -86.45707362346617231, -9.058813317711329915, 2.943386871421371787 ) ) ;
#29685 = VECTOR ( 'NONE', #6555, 1000.000000000000000 ) ;
#29686 = AXIS2_PLACEMENT_3D ( 'NONE', #43126, #37508, #5412 ) ;
#29687 = CARTESIAN_POINT ( 'NONE',  ( -96.14292637653380780, 5.598654528085800663, -7.705886871421367523 ) ) ;
#29688 = DIRECTION ( 'NONE',  ( 0.000000000000000000, 0.000000000000000000, -1.000000000000000000 ) ) ;
#29689 = DIRECTION ( 'NONE',  ( 1.000000000000000000, -0.000000000000000000, -1.300977106640434891E-16 ) ) ;
#29691 = CARTESIAN_POINT ( 'NONE',  ( 30.25000000000000711, 18.74999999999997868, 3.750000000000000000 ) ) ;
#29690 = DIRECTION ( 'NONE',  ( 0.000000000000000000, 0.000000000000000000, -1.000000000000000000 ) ) ;
#29692 = CARTESIAN_POINT ( 'NONE',  ( -125.6050000000000040, 6.826472737025113702, -4.959722759717902107 ) ) ;
#29693 = CARTESIAN_POINT ( 'NONE',  ( -158.2429263765338021, 5.598654528085804216, 7.705886871421366635 ) ) ;
#29694 = CARTESIAN_POINT ( 'NONE',  ( -9.058813317711337021, 110.0449999999999875, -2.943386871421374895 ) ) ;
#29695 = CARTESIAN_POINT ( 'NONE',  ( -138.7450000000000045, 4.716976649647094177, 6.492361379858945902 ) ) ;
#29696 = CIRCLE ( 'NONE', #8365, 7.500000000000000000 ) ;
#29697 = CARTESIAN_POINT ( 'NONE',  ( -116.0949999999999704, -2.607480562269071545, -8.024999999999991473 ) ) ;
#29698 = CARTESIAN_POINT ( 'NONE',  ( 74.65811388300841145, 19.88603796100278487, -6.500000000000000000 ) ) ;
#29699 = EDGE_LOOP ( 'NONE', ( #50277, #56467, #55686, #29536 ) ) ;
#29700 = CARTESIAN_POINT ( 'NONE',  ( -71.75000000000000000, -3.000000000000000000, 20.00000000000000000 ) ) ;
#29701 = SURFACE_STYLE_FILL_AREA ( #34614 ) ;
#29702 = EDGE_CURVE ( 'NONE', #16496, #62518, #67845, .T. ) ;
#29703 = CARTESIAN_POINT ( 'NONE',  ( -174.2929263765338419, 3.094860106618428031, -9.524999999999993250 ) ) ;
#29704 = DIRECTION ( 'NONE',  ( 0.000000000000000000, -1.000000000000000000, 0.000000000000000000 ) ) ;
#29705 = ADVANCED_FACE ( 'NONE', ( #580 ), #6262, .T. ) ;
#29706 = EDGE_CURVE ( 'NONE', #4654, #3912, #34137, .T. ) ;
#29707 = VECTOR ( 'NONE', #58350, 1000.000000000000000 ) ;
#29708 = FILL_AREA_STYLE_COLOUR ( '', #64618 ) ;
#29709 = AXIS2_PLACEMENT_3D ( 'NONE', #38889, #29314, #33901 ) ;
#29710 = SURFACE_STYLE_USAGE ( .BOTH. , #45588 ) ;
#29711 = CARTESIAN_POINT ( 'NONE',  ( 65.00000000000000000, 1.797044900979284448E-15, -12.00000000000000000 ) ) ;
#29712 = ORIENTED_EDGE ( 'NONE', *, *, #42180, .T. ) ;
#29713 = PRODUCT_DEFINITION_CONTEXT ( 'detailed design', #67111, 'design' ) ;
#29714 = CARTESIAN_POINT ( 'NONE',  ( -85.34292637653381064, -9.058813317711329915, 2.943386871421371787 ) ) ;
#29715 = APPLICATION_PROTOCOL_DEFINITION ( 'draft international standard', 'automotive_design', 1998, #45596 ) ;
#29716 = AXIS2_PLACEMENT_3D ( 'NONE', #11027, #32151, #64512 ) ;
#29717 = FACE_OUTER_BOUND ( 'NONE', #17567, .T. ) ;
#29718 = AXIS2_PLACEMENT_3D ( 'NONE', #63616, #4498, #4868 ) ;
#29719 = CARTESIAN_POINT ( 'NONE',  ( -9.827790563157511022E-16, 122.5570736234661524, 8.025000000000000355 ) ) ;
#29720 = CARTESIAN_POINT ( 'NONE',  ( -41.08002123031664610, 107.6301924976384470, 3.280722492564424719 ) ) ;
#29721 = ADVANCED_FACE ( 'NONE', ( #37289 ), #60075, .T. ) ;
#29722 = STYLED_ITEM ( 'NONE', ( #25989 ), #30729 ) ;
#29723 = CARTESIAN_POINT ( 'NONE',  ( -41.49999999999997868, 9.999999999999978684, 3.000000000000000000 ) ) ;
#29724 = ORIENTED_EDGE ( 'NONE', *, *, #67498, .T. ) ;
#29725 = DIRECTION ( 'NONE',  ( -0.03448275862069643399, 0.9994052928406507164, -3.469446951953618922E-15 ) ) ;
#29726 =( NAMED_UNIT ( * ) PLANE_ANGLE_UNIT ( ) SI_UNIT ( $, .RADIAN. ) );
#29727 = VERTEX_POINT ( 'NONE', #11889 ) ;
#29728 = SURFACE_STYLE_FILL_AREA ( #45248 ) ;
#29729 = CARTESIAN_POINT ( 'NONE',  ( 4.716976649647096842, 131.8570736234661638, 6.492361379858953896 ) ) ;
#29730 = TOROIDAL_SURFACE ( 'NONE', #58911, 24.00000000000001421, 1.000000000000000000 ) ;
#29731 = VECTOR ( 'NONE', #25253, 1000.000000000000000 ) ;
#29732 = DIRECTION ( 'NONE',  ( 0.000000000000000000, 0.000000000000000000, 1.000000000000000000 ) ) ;
#29733 = DIRECTION ( 'NONE',  ( -0.000000000000000000, -0.000000000000000000, -1.000000000000000000 ) ) ;
#29734 = DIRECTION ( 'NONE',  ( 1.776356839400250465E-15, 0.000000000000000000, 1.000000000000000000 ) ) ;
#29735 = ORIENTED_EDGE ( 'NONE', *, *, #62754, .T. ) ;
#29736 = CARTESIAN_POINT ( 'NONE',  ( -93.89292637653377938, -8.102448949553174629, -5.886773742842741797 ) ) ;
#29737 = SURFACE_STYLE_FILL_AREA ( #41360 ) ;
#29738 = CARTESIAN_POINT ( 'NONE',  ( 6.826472737025119919, 150.0070736234661695, 4.959722759717908325 ) ) ;
#29739 = EDGE_CURVE ( 'NONE', #62495, #69341, #26322, .T. ) ;
#29740 = CYLINDRICAL_SURFACE ( 'NONE', #51992, 16.00000000000000000 ) ;
#29741 = VECTOR ( 'NONE', #7159, 1000.000000000000000 ) ;
#29742 = CARTESIAN_POINT ( 'NONE',  ( -71.00707362346615525, -8.102448949553174629, -5.886773742842741797 ) ) ;
#29743 = EDGE_CURVE ( 'NONE', #54047, #1442, #58696, .T. ) ;
#29744 = CARTESIAN_POINT ( 'NONE',  ( -82.49499999999997613, 6.826472737025113702, -4.959722759717902107 ) ) ;
#29745 = VERTEX_POINT ( 'NONE', #64675 ) ;
#29746 = CARTESIAN_POINT ( 'NONE',  ( 68.99999999999998579, 8.450062914116736267E-15, 4.000000000000000000 ) ) ;
#29747 =( LENGTH_UNIT ( ) NAMED_UNIT ( * ) SI_UNIT ( .MILLI., .METRE. ) );
#29748 = UNCERTAINTY_MEASURE_WITH_UNIT (LENGTH_MEASURE( 1.000000000000000082E-05 ), #19720, 'distance_accuracy_value', 'NONE');
#29749 = EDGE_LOOP ( 'NONE', ( #15164, #5262, #20749, #40077 ) ) ;
#29750 = PRESENTATION_LAYER_ASSIGNMENT (  '', '', ( #44426 ) ) ;
#29751 = CARTESIAN_POINT ( 'NONE',  ( 71.50000000000000000, 35.92875272052971525, 7.500000000000000000 ) ) ;
#29752 =( GEOMETRIC_REPRESENTATION_CONTEXT ( 3 ) GLOBAL_UNCERTAINTY_ASSIGNED_CONTEXT ( ( #46132 ) ) GLOBAL_UNIT_ASSIGNED_CONTEXT ( ( #54284, #31432, #64842 ) ) REPRESENTATION_CONTEXT ( 'NONE', 'WORKASPACE' ) );
#29753 =( NAMED_UNIT ( * ) SI_UNIT ( $, .STERADIAN. ) SOLID_ANGLE_UNIT ( ) );
#29754 = ORIENTED_EDGE ( 'NONE', *, *, #4689, .F. ) ;
#29755 = PRESENTATION_STYLE_ASSIGNMENT (( #14270 ) ) ;
#29756 = AXIS2_PLACEMENT_3D ( 'NONE', #53615, #26528, #43116 ) ;
#29757 = ORIENTED_EDGE ( 'NONE', *, *, #7322, .F. ) ;
#29758 = PLANE ( 'NONE',  #68390 ) ;
#29759 = DIRECTION ( 'NONE',  ( 0.000000000000000000, -1.000000000000000000, 0.000000000000000000 ) ) ;
#29760 = CARTESIAN_POINT ( 'NONE',  ( 3.409440450227775532, -1.719598803868653603, 7.000000000000000888 ) ) ;
#29761 = CARTESIAN_POINT ( 'NONE',  ( -172.5570736234661808, -1.166476076187852838E-15, -9.524999999999991473 ) ) ;
#29762 = CARTESIAN_POINT ( 'NONE',  ( 22.50000000000000711, 33.99999999999999289, 4.000000000000000000 ) ) ;
#29763 =( GEOMETRIC_REPRESENTATION_CONTEXT ( 3 ) GLOBAL_UNCERTAINTY_ASSIGNED_CONTEXT ( ( #977 ) ) GLOBAL_UNIT_ASSIGNED_CONTEXT ( ( #63393, #67275, #61987 ) ) REPRESENTATION_CONTEXT ( 'NONE', 'WORKASPACE' ) );
#29764 =( BOUNDED_CURVE ( )  B_SPLINE_CURVE ( 2, ( #52097, #67555, #10207, #62954, #31644, #35894, #41904, #53124, #24984, #20039, #19353 ),
 .UNSPECIFIED., .F., .F. ) 
 B_SPLINE_CURVE_WITH_KNOTS ( ( 3, 2, 2, 2, 2, 3 ),
 ( 0.6195652173912895577, 0.6217391304347678060, 0.6239130434782459433, 0.6260869565217243027, 0.6282608695652024400, 0.6304347826086806883 ),
 .UNSPECIFIED. ) 
 CURVE ( )  GEOMETRIC_REPRESENTATION_ITEM ( )  RATIONAL_B_SPLINE_CURVE ( ( 1.000000000000332401, 0.9510565162948211304, 1.000000000000000000, 0.9510565162951535312, 1.000000000000000000, 0.9510565162951535312, 1.000000000000000000, 0.9510565162951535312, 1.000000000000000000, 0.9510565162954909280, 0.9999999999996626032 ) ) 
 REPRESENTATION_ITEM ( '' )  );
#29765 = CARTESIAN_POINT ( 'NONE',  ( -112.1070736234661496, 8.102448949553171076, -5.886773742842744461 ) ) ;
#29766 = CARTESIAN_POINT ( 'NONE',  ( -183.0000000000000000, 7.623482428031956637, -5.710353812986356026 ) ) ;
#29767 = VECTOR ( 'NONE', #35063, 1000.000000000000000 ) ;
#29768 = PLANE ( 'NONE',  #13380 ) ;
#29769 = EDGE_LOOP ( 'NONE', ( #451, #3582, #24047, #58202 ) ) ;
#29770 = CARTESIAN_POINT ( 'NONE',  ( 27.00000000000001776, 42.00000000000000000, -34.49999999999999289 ) ) ;
#29771 = SURFACE_STYLE_USAGE ( .BOTH. , #12532 ) ;
#29772 = CARTESIAN_POINT ( 'NONE',  ( 71.49999999999998579, 64.07124727947029896, -7.500000000000000000 ) ) ;
#29773 = FILL_AREA_STYLE ('',( #56140 ) ) ;
#29774 = CARTESIAN_POINT ( 'NONE',  ( -146.7549999999999955, 4.716976649647091513, -6.492361379858946790 ) ) ;
#29775 =( LENGTH_UNIT ( ) NAMED_UNIT ( * ) SI_UNIT ( .MILLI., .METRE. ) );
#29776 = CARTESIAN_POINT ( 'NONE',  ( -6.962908620255356063, 111.9337395095162719, 4.200728263596600343 ) ) ;
#29777 = EDGE_CURVE ( 'NONE', #61721, #38442, #8297, .T. ) ;
#29778 = CARTESIAN_POINT ( 'NONE',  ( -166.6449999999999818, 4.716976649647091513, -6.492361379858946790 ) ) ;
#29779 = CARTESIAN_POINT ( 'NONE',  ( -146.0949999999999989, -2.607480562269071545, -8.024999999999991473 ) ) ;
#29780 = ORIENTED_EDGE ( 'NONE', *, *, #37585, .T. ) ;
#29781 = STYLED_ITEM ( 'NONE', ( #46438 ), #27529 ) ;
#29782 = CYLINDRICAL_SURFACE ( 'NONE', #68434, 9.524999999999991473 ) ;
#29783 = MECHANICAL_DESIGN_GEOMETRIC_PRESENTATION_REPRESENTATION (  '', ( #6178 ), #45544 ) ;
#29784 = FACE_OUTER_BOUND ( 'NONE', #54225, .T. ) ;
#29785 = FACE_OUTER_BOUND ( 'NONE', #29904, .T. ) ;
#29786 = CARTESIAN_POINT ( 'NONE',  ( -64.85499999999997556, 4.716976649647094177, 6.492361379858945902 ) ) ;
#29787 = CARTESIAN_POINT ( 'NONE',  ( 13.50000000000000533, 30.74999999999999289, 4.000000000000000000 ) ) ;
#29788 = CARTESIAN_POINT ( 'NONE',  ( 26.00000000000001066, 18.99999999999997868, 3.750000000000000000 ) ) ;
#29789 = VECTOR ( 'NONE', #57043, 1000.000000000000000 ) ;
#29790 = EDGE_CURVE ( 'NONE', #52838, #26396, #31958, .T. ) ;
#29791 = CARTESIAN_POINT ( 'NONE',  ( -62.39499999999998181, -6.826472737025113702, -4.959722759717900331 ) ) ;
#29792 = CARTESIAN_POINT ( 'NONE',  ( -5.598654528085808657, 150.7549999999999955, 7.705886871421373741 ) ) ;
#29793 = CARTESIAN_POINT ( 'NONE',  ( 13.75000000000000533, 30.74999999999999289, -3.750000000000000000 ) ) ;
#29794 =( NAMED_UNIT ( * ) SI_UNIT ( $, .STERADIAN. ) SOLID_ANGLE_UNIT ( ) );
#29795 = UNCERTAINTY_MEASURE_WITH_UNIT (LENGTH_MEASURE( 1.000000000000000082E-05 ), #31771, 'distance_accuracy_value', 'NONE');
#29796 = CARTESIAN_POINT ( 'NONE',  ( 0.08961394468541557246, 42.48853604202995626, -45.29557250688775127 ) ) ;
#29797 = DIRECTION ( 'NONE',  ( 0.000000000000000000, -1.000000000000000000, 0.000000000000000000 ) ) ;
#29798 = LINE ( 'NONE', #24490, #30345 ) ;
#29799 = ADVANCED_FACE ( 'NONE', ( #37983 ), #69593, .T. ) ;
#29800 = VECTOR ( 'NONE', #18344, 1000.000000000000000 ) ;
#29801 = CARTESIAN_POINT ( 'NONE',  ( 68.99999999999998579, 36.75000000000000000, -4.000000000000000000 ) ) ;
#29802 = CARTESIAN_POINT ( 'NONE',  ( 15.00000000000000000, 8.000000000000000000, 4.000000000000000000 ) ) ;
#29803 = EDGE_LOOP ( 'NONE', ( #59958, #48344, #33764, #36859 ) ) ;
#29804 = EDGE_LOOP ( 'NONE', ( #5226, #16725, #11714, #64935 ) ) ;
#29805 = CARTESIAN_POINT ( 'NONE',  ( 23.50000000000001776, 27.44010416289936316, -27.18999999999999417 ) ) ;
#29806 = AXIS2_PLACEMENT_3D ( 'NONE', #23730, #17455, #39254 ) ;
#29807 = ORIENTED_EDGE ( 'NONE', *, *, #41330, .F. ) ;
#29808 = ORIENTED_EDGE ( 'NONE', *, *, #44298, .F. ) ;
#29809 =( NAMED_UNIT ( * ) SI_UNIT ( $, .STERADIAN. ) SOLID_ANGLE_UNIT ( ) );
#29810 = ORIENTED_EDGE ( 'NONE', *, *, #57066, .T. ) ;
#29811 = CARTESIAN_POINT ( 'NONE',  ( -10.01517768586949231, 114.3049999999999926, -6.132527647946036459E-16 ) ) ;
#29812 = CARTESIAN_POINT ( 'NONE',  ( -145.1929263765337907, -10.01517768586948698, 6.132527647946031529E-16 ) ) ;
#29813 = ORIENTED_EDGE ( 'NONE', *, *, #12382, .F. ) ;
#29814 = CARTESIAN_POINT ( 'NONE',  ( 3.000000000000000000, 0.000000000000000000, -72.00402776293822171 ) ) ;
#29815 = DIRECTION ( 'NONE',  ( 2.312964634635740689E-15, -1.000000000000000000, 0.000000000000000000 ) ) ;
#29816 = CARTESIAN_POINT ( 'NONE',  ( -112.3449999999999847, 7.632228543268599452, -2.479861379858951942 ) ) ;
#29817 = VERTEX_POINT ( 'NONE', #60407 ) ;
#29818 = APPLICATION_CONTEXT ( 'automotive_design' ) ;
#29819 = CARTESIAN_POINT ( 'NONE',  ( -53.69292637653380496, 10.01517768586948698, -1.839758294383808966E-15 ) ) ;
#29820 = CARTESIAN_POINT ( 'NONE',  ( -10.75962301985815017, -11.70357532857513938, -2.654319096146382062 ) ) ;
#29821 = ORIENTED_EDGE ( 'NONE', *, *, #48672, .T. ) ;
#29822 = CARTESIAN_POINT ( 'NONE',  ( -6.826472737025120807, 141.9929263765338305, 4.959722759717906548 ) ) ;
#29823 = FILL_AREA_STYLE ('',( #18901 ) ) ;
#29824 = CARTESIAN_POINT ( 'NONE',  ( -11.74999999999999645, -3.585786437626905077, 19.00000000000000000 ) ) ;
#29825 = CIRCLE ( 'NONE', #47881, 0.4999999999999993339 ) ;
#29826 = CARTESIAN_POINT ( 'NONE',  ( 73.01088739851488185, 0.000000000000000000, -65.71817553072278884 ) ) ;
#29827 = ORIENTED_EDGE ( 'NONE', *, *, #24059, .F. ) ;
#29828 = ORIENTED_EDGE ( 'NONE', *, *, #55313, .T. ) ;
#29829 = CYLINDRICAL_SURFACE ( 'NONE', #39457, 23.00000000000000000 ) ;
#29830 = STYLED_ITEM ( 'NONE', ( #55421 ), #49411 ) ;
#29831 = DIRECTION ( 'NONE',  ( -0.8946296187927070820, 0.000000000000000000, -0.4468085106382997385 ) ) ;
#29832 = CARTESIAN_POINT ( 'NONE',  ( -60.00000000000000000, -2.024042244987997205E-14, 11.50000000000003020 ) ) ;
#29833 = STYLED_ITEM ( 'NONE', ( #16529 ), #5619 ) ;
#29834 = CARTESIAN_POINT ( 'NONE',  ( -131.6049999999999898, 6.826472737025113702, -4.959722759717902107 ) ) ;
#29835 = PLANE ( 'NONE',  #39869 ) ;
#29836 = EDGE_LOOP ( 'NONE', ( #934, #54212, #37646, #66969 ) ) ;
#29837 = SURFACE_STYLE_USAGE ( .BOTH. , #56215 ) ;
#29838 = CARTESIAN_POINT ( 'NONE',  ( 75.00000000000000000, 19.99999999999997868, -6.500000000000000000 ) ) ;
#29839 = CYLINDRICAL_SURFACE ( 'NONE', #9022, 1.000000000000000888 ) ;
#29840 = EDGE_LOOP ( 'NONE', ( #13156, #1049, #43375, #22288 ) ) ;
#29841 = ORIENTED_EDGE ( 'NONE', *, *, #1851, .F. ) ;
#29842 = DIRECTION ( 'NONE',  ( -7.080503983578803083E-17, 1.000000000000000000, 0.000000000000000000 ) ) ;
#29843 = FACE_OUTER_BOUND ( 'NONE', #64053, .T. ) ;
#29844 = DIRECTION ( 'NONE',  ( 0.000000000000000000, 0.000000000000000000, -1.000000000000000000 ) ) ;
#29845 = CARTESIAN_POINT ( 'NONE',  ( -3.000000000000000444, 0.000000000000000000, 7.500000000000000000 ) ) ;
#29847 = VERTEX_POINT ( 'NONE', #23826 ) ;
#29846 = VECTOR ( 'NONE', #35183, 1000.000000000000000 ) ;
#29848 = CARTESIAN_POINT ( 'NONE',  ( -179.0050000000000239, 6.826472737025116366, 4.959722759717898555 ) ) ;
#29849 = SURFACE_SIDE_STYLE ('',( #62545 ) ) ;
#29850 = PRESENTATION_STYLE_ASSIGNMENT (( #52026 ) ) ;
#29851 = AXIS2_PLACEMENT_3D ( 'NONE', #11227, #4558, #26013 ) ;
#29852 = EDGE_CURVE ( 'NONE', #54470, #21703, #23994, .T. ) ;
#29853 = CARTESIAN_POINT ( 'NONE',  ( -52.85707362346617089, -5.598654528085803328, -7.705886871421366635 ) ) ;
#29854 = VECTOR ( 'NONE', #51058, 1000.000000000000000 ) ;
#29855 = CARTESIAN_POINT ( 'NONE',  ( -173.2449999999999761, -4.716976649647093289, -6.492361379858945902 ) ) ;
#29856 = DIRECTION ( 'NONE',  ( -1.000000000000000000, 0.000000000000000000, 0.000000000000000000 ) ) ;
#29857 = AXIS2_PLACEMENT_3D ( 'NONE', #43964, #33028, #1288 ) ;
#29859 = EDGE_CURVE ( 'NONE', #3684, #62473, #9317, .T. ) ;
#29858 = VERTEX_POINT ( 'NONE', #34711 ) ;
#29860 = DIRECTION ( 'NONE',  ( -1.000000000000000000, 0.000000000000000000, 0.000000000000000000 ) ) ;
#29861 = CIRCLE ( 'NONE', #34334, 1.000000000000000888 ) ;
#29862 = CARTESIAN_POINT ( 'NONE',  ( -95.75499999999999545, 4.716976649647091513, -6.492361379858946790 ) ) ;
#29863 = CARTESIAN_POINT ( 'NONE',  ( 61.99999999999998579, 31.24999999999999289, -3.750000000000000000 ) ) ;
#29864 = FILL_AREA_STYLE ('',( #63610 ) ) ;
#29865 = CARTESIAN_POINT ( 'NONE',  ( 57.49999999999998579, 30.99999999999999289, 4.000000000000000000 ) ) ;
#29866 = EDGE_CURVE ( 'NONE', #66133, #7763, #12739, .T. ) ;
#29867 = CARTESIAN_POINT ( 'NONE',  ( -99.29499999999998749, -2.607480562269069768, 8.024999999999991473 ) ) ;
#29868 = CARTESIAN_POINT ( 'NONE',  ( 5.598654528085809545, 119.2549999999999812, -7.705886871421373741 ) ) ;
#29869 = CARTESIAN_POINT ( 'NONE',  ( -68.54499999999998749, -7.632228543268600340, -2.479861379858950166 ) ) ;
#29870 = EDGE_CURVE ( 'NONE', #26003, #58118, #333, .T. ) ;
#29871 = DIRECTION ( 'NONE',  ( 1.084202172485504434E-16, 0.000000000000000000, 1.000000000000000000 ) ) ;
#29872 = CYLINDRICAL_SURFACE ( 'NONE', #24713, 1.000000000000000888 ) ;
#29873 = EDGE_CURVE ( 'NONE', #37046, #20411, #29441, .T. ) ;
#29874 = FILL_AREA_STYLE_COLOUR ( '', #48474 ) ;
#29875 = UNCERTAINTY_MEASURE_WITH_UNIT (LENGTH_MEASURE( 1.000000000000000082E-05 ), #10568, 'distance_accuracy_value', 'NONE');
#29876 = PRESENTATION_LAYER_ASSIGNMENT (  '', '', ( #40012 ) ) ;
#29877 = SURFACE_STYLE_USAGE ( .BOTH. , #46815 ) ;
#29878 = ORIENTED_EDGE ( 'NONE', *, *, #57066, .F. ) ;
#29879 = EDGE_CURVE ( 'NONE', #13443, #9871, #12919, .T. ) ;
#29880 = CARTESIAN_POINT ( 'NONE',  ( -110.9929263765338163, 8.102448949553171076, -5.886773742842744461 ) ) ;
#29881 = CARTESIAN_POINT ( 'NONE',  ( -130.0449999999999875, 7.632228543268600340, 2.479861379858949277 ) ) ;
#29882 = CARTESIAN_POINT ( 'NONE',  ( 24.21231517720798010, 113.4999999999999858, 7.000000000000000000 ) ) ;
#29883 = PRESENTATION_LAYER_ASSIGNMENT (  '', '', ( #61355 ) ) ;
#29884 = CARTESIAN_POINT ( 'NONE',  ( 0.000000000000000000, 21.74999999999998224, 4.000000000000000000 ) ) ;
#29886 = PLANE ( 'NONE',  #18027 ) ;
#29885 = FILL_AREA_STYLE_COLOUR ( '', #52040 ) ;
#29887 = AXIS2_PLACEMENT_3D ( 'NONE', #41627, #68005, #9945 ) ;
#29889 = AXIS2_PLACEMENT_3D ( 'NONE', #612, #12951, #66421 ) ;
#29888 = DIRECTION ( 'NONE',  ( 0.000000000000000000, 0.000000000000000000, 1.000000000000000000 ) ) ;
#29890 = EDGE_LOOP ( 'NONE', ( #24337, #13300, #22045, #6140, #20894, #65378 ) ) ;
#29891 = VERTEX_POINT ( 'NONE', #2674 ) ;
#29892 = STYLED_ITEM ( 'NONE', ( #49551 ), #5776 ) ;
#29893 = CARTESIAN_POINT ( 'NONE',  ( 11.00000000000001776, 26.00000000000000355, 23.99999999999999645 ) ) ;
#29894 = CARTESIAN_POINT ( 'NONE',  ( 3.999798566743338668, 49.09558629977726696, 7.322456175549363344 ) ) ;
#29895 = SURFACE_STYLE_USAGE ( .BOTH. , #24955 ) ;
#29896 = DIRECTION ( 'NONE',  ( 0.000000000000000000, 0.000000000000000000, 1.000000000000000000 ) ) ;
#29897 = CARTESIAN_POINT ( 'NONE',  ( 3.249999999999999112, 34.24999999999998579, 4.000000000000000000 ) ) ;
#29898 = ORIENTED_EDGE ( 'NONE', *, *, #44133, .F. ) ;
#29899 = CARTESIAN_POINT ( 'NONE',  ( -132.3549999999999898, -4.716976649647093289, -6.492361379858945902 ) ) ;
#29900 = VERTEX_POINT ( 'NONE', #34385 ) ;
#29901 = DIRECTION ( 'NONE',  ( 1.000000000000000000, 0.000000000000000000, 0.000000000000000000 ) ) ;
#29902 = CIRCLE ( 'NONE', #61324, 0.2500000000000002220 ) ;
#29903 = CARTESIAN_POINT ( 'NONE',  ( -120.2070736234661865, 3.094860106618433360, 9.524999999999991473 ) ) ;
#29904 = EDGE_LOOP ( 'NONE', ( #41006, #68283, #44295, #5975 ) ) ;
#29905 = CARTESIAN_POINT ( 'NONE',  ( 44.28021770739999852, 9.999999999999980460, -3.500000000000000000 ) ) ;
#29906 = ORIENTED_EDGE ( 'NONE', *, *, #48477, .F. ) ;
#29907 = PRESENTATION_LAYER_ASSIGNMENT (  '', '', ( #60239 ) ) ;
#29908 = CARTESIAN_POINT ( 'NONE',  ( 8.102448949553181734, 138.3950000000000102, 5.886773742842750679 ) ) ;
#29909 = DIRECTION ( 'NONE',  ( -0.000000000000000000, -1.000000000000000000, -0.000000000000000000 ) ) ;
#29910 = VECTOR ( 'NONE', #17051, 1000.000000000000000 ) ;
#29911 = ORIENTED_EDGE ( 'NONE', *, *, #14381, .F. ) ;
#29912 = CARTESIAN_POINT ( 'NONE',  ( 18.00000000000000711, 31.24999999999999289, -3.750000000000000000 ) ) ;
#29913 = CARTESIAN_POINT ( 'NONE',  ( -9.058813317711338797, 138.4549999999999841, 2.943386871421373563 ) ) ;
#29914 = DIRECTION ( 'NONE',  ( 0.7713892158398705234, 0.000000000000000000, -0.6363636363636357984 ) ) ;
#29915 = ORIENTED_EDGE ( 'NONE', *, *, #36687, .F. ) ;
#29916 = CARTESIAN_POINT ( 'NONE',  ( -7.632228543268608334, 114.8429263765338106, 2.479861379858952830 ) ) ;
#29917 = LINE ( 'NONE', #67917, #16627 ) ;
#29918 = UNCERTAINTY_MEASURE_WITH_UNIT (LENGTH_MEASURE( 1.000000000000000082E-05 ), #25578, 'distance_accuracy_value', 'NONE');
#29919 = CARTESIAN_POINT ( 'NONE',  ( 1.000000000000000000, 14.00000000000000000, -80.00402776293826435 ) ) ;
#29920 = LINE ( 'NONE', #51378, #26487 ) ;
#29921 = ORIENTED_EDGE ( 'NONE', *, *, #54271, .T. ) ;
#29922 = DIRECTION ( 'NONE',  ( 0.000000000000000000, 1.000000000000000000, 0.000000000000000000 ) ) ;
#29923 = ORIENTED_EDGE ( 'NONE', *, *, #53993, .F. ) ;
#29924 = LINE ( 'NONE', #2805, #21309 ) ;
#29925 = CARTESIAN_POINT ( 'NONE',  ( 20.20444455447386645, 114.9652390998742533, 10.39771284005833252 ) ) ;
#29926 = DIRECTION ( 'NONE',  ( -0.000000000000000000, -0.000000000000000000, 1.000000000000000000 ) ) ;
#29927 = CARTESIAN_POINT ( 'NONE',  ( -159.9549999999999841, -7.632228543268599452, 2.479861379858951054 ) ) ;
#29928 = ORIENTED_EDGE ( 'NONE', *, *, #55047, .T. ) ;
#29929 = UNCERTAINTY_MEASURE_WITH_UNIT (LENGTH_MEASURE( 1.000000000000000082E-05 ), #47582, 'distance_accuracy_value', 'NONE');
#29930 =( NAMED_UNIT ( * ) SI_UNIT ( $, .STERADIAN. ) SOLID_ANGLE_UNIT ( ) );
#29931 = CARTESIAN_POINT ( 'NONE',  ( -56.30661091817325570, -8.499999999999996447, 7.186868961046329218 ) ) ;
#29932 = CARTESIAN_POINT ( 'NONE',  ( 74.52070078832272770, 19.38218994716120847, 6.500000000000000888 ) ) ;
#29933 = ORIENTED_EDGE ( 'NONE', *, *, #5769, .T. ) ;
#29934 =( NAMED_UNIT ( * ) SI_UNIT ( $, .STERADIAN. ) SOLID_ANGLE_UNIT ( ) );
#29935 = ORIENTED_EDGE ( 'NONE', *, *, #14294, .F. ) ;
#29936 = CARTESIAN_POINT ( 'NONE',  ( 52.75000000000000000, 25.24999999999998579, 4.000000000000000000 ) ) ;
#29937 = CIRCLE ( 'NONE', #54677, 0.2500000000000002220 ) ;
#29938 = CARTESIAN_POINT ( 'NONE',  ( -73.55499999999997840, 0.000000000000000000, 8.024999999999991473 ) ) ;
#29939 = ORIENTED_EDGE ( 'NONE', *, *, #12094, .T. ) ;
#29941 = CIRCLE ( 'NONE', #43459, 4.750000000000000000 ) ;
#29940 = DIRECTION ( 'NONE',  ( 0.000000000000000000, 0.000000000000000000, 1.000000000000000000 ) ) ;
#29942 = ADVANCED_FACE ( 'NONE', ( #55833 ), #49538, .T. ) ;
#29943 = AXIS2_PLACEMENT_3D ( 'NONE', #1399, #16626, #65114 ) ;
#29944 = FACE_OUTER_BOUND ( 'NONE', #59563, .T. ) ;
#29945 =( LENGTH_UNIT ( ) NAMED_UNIT ( * ) SI_UNIT ( .MILLI., .METRE. ) );
#29946 = EDGE_CURVE ( 'NONE', #60879, #53365, #45331, .T. ) ;
#29947 =( NAMED_UNIT ( * ) PLANE_ANGLE_UNIT ( ) SI_UNIT ( $, .RADIAN. ) );
#29948 = ORIENTED_EDGE ( 'NONE', *, *, #58004, .F. ) ;
#29949 = CARTESIAN_POINT ( 'NONE',  ( 23.32387453076606221, 27.44010416289935606, -27.18999999999999773 ) ) ;
#29950 = FACE_OUTER_BOUND ( 'NONE', #63491, .T. ) ;
#29951 = AXIS2_PLACEMENT_3D ( 'NONE', #6889, #44234, #37919 ) ;
#29952 = CARTESIAN_POINT ( 'NONE',  ( -9.058813317711337021, 137.0449999999999875, -2.943386871421374895 ) ) ;
#29953 = CARTESIAN_POINT ( 'NONE',  ( -99.44499999999999318, 0.000000000000000000, 8.024999999999991473 ) ) ;
#29954 = EDGE_CURVE ( 'NONE', #18076, #32404, #13256, .T. ) ;
#29955 = CARTESIAN_POINT ( 'NONE',  ( -83.99999999999997158, 50.00000000000000000, 10.50000000000000000 ) ) ;
#29956 = UNCERTAINTY_MEASURE_WITH_UNIT (LENGTH_MEASURE( 1.000000000000000082E-05 ), #44897, 'distance_accuracy_value', 'NONE');
#29958 = CARTESIAN_POINT ( 'NONE',  ( -41.49999999999998579, 106.9282032302754999, -3.500000000000000000 ) ) ;
#29957 = DIRECTION ( 'NONE',  ( -1.000000000000000000, 0.000000000000000000, -0.000000000000000000 ) ) ;
#29959 = COLOUR_RGB ( '', 0.31764706, 0.68627451, 0.89019608) ;
#29960 = EDGE_CURVE ( 'NONE', #60536, #54396, #39749, .T. ) ;
#29961 = CARTESIAN_POINT ( 'NONE',  ( -140.0929263765337964, 3.094860106618433360, 9.524999999999991473 ) ) ;
#29962 = FILL_AREA_STYLE_COLOUR ( '', #68668 ) ;
#29963 = SURFACE_STYLE_FILL_AREA ( #8528 ) ;
#29964 = CARTESIAN_POINT ( 'NONE',  ( -170.8449999999999989, -7.632228543268599452, 2.479861379858951054 ) ) ;
#29965 = AXIS2_PLACEMENT_3D ( 'NONE', #48736, #60279, #6122 ) ;
#29966 = CARTESIAN_POINT ( 'NONE',  ( 6.000000000000017764, 26.00000000000000355, -24.00000000000000355 ) ) ;
#29967 = ORIENTED_EDGE ( 'NONE', *, *, #7692, .F. ) ;
#29968 = CARTESIAN_POINT ( 'NONE',  ( -43.75000000000000000, 0.000000000000000000, -6.999999999999999112 ) ) ;
#29969 = ORIENTED_EDGE ( 'NONE', *, *, #30038, .F. ) ;
#29970 = CARTESIAN_POINT ( 'NONE',  ( 34.99999999999992895, 112.4999999999999858, -10.00000000000000000 ) ) ;
#29971 = FILL_AREA_STYLE ('',( #2494 ) ) ;
#29972 = CARTESIAN_POINT ( 'NONE',  ( -45.58282705953852343, 8.118038230903730224, 6.493553718642735006 ) ) ;
#29973 = DIRECTION ( 'NONE',  ( -0.2413793103448194644, 0.9704308468600220117, 0.000000000000000000 ) ) ;
#29974 = ORIENTED_EDGE ( 'NONE', *, *, #1609, .F. ) ;
#29975 = CARTESIAN_POINT ( 'NONE',  ( -164.4549999999999841, 7.632228543268599452, -2.479861379858951942 ) ) ;
#29976 = CIRCLE ( 'NONE', #69323, 0.5000000000000006661 ) ;
#29977 = VERTEX_POINT ( 'NONE', #14673 ) ;
#29978 = DIRECTION ( 'NONE',  ( 0.000000000000000000, 0.000000000000000000, 1.000000000000000000 ) ) ;
#29979 =( NAMED_UNIT ( * ) SI_UNIT ( $, .STERADIAN. ) SOLID_ANGLE_UNIT ( ) );
#29980 = ORIENTED_EDGE ( 'NONE', *, *, #47319, .T. ) ;
#29981 = CIRCLE ( 'NONE', #17906, 3.000000000000000444 ) ;
#29982 = SURFACE_STYLE_USAGE ( .BOTH. , #67992 ) ;
#29983 = CARTESIAN_POINT ( 'NONE',  ( -5.598654528085806881, 112.7449999999999903, -7.705886871421374629 ) ) ;
#29984 = EDGE_CURVE ( 'NONE', #13573, #13184, #9406, .T. ) ;
#29985 = EDGE_LOOP ( 'NONE', ( #14441, #17838, #48650, #68103 ) ) ;
#29986 = DIRECTION ( 'NONE',  ( -1.000000000000000000, 0.000000000000000000, 0.000000000000000000 ) ) ;
#29987 = CARTESIAN_POINT ( 'NONE',  ( -3.094860106618434248, 111.9049999999999869, 9.525000000000000355 ) ) ;
#29988 = CARTESIAN_POINT ( 'NONE',  ( -75.50499999999998124, -6.826472737025113702, -4.959722759717900331 ) ) ;
#29989 = CARTESIAN_POINT ( 'NONE',  ( -74.50000000000000000, -2.220952357103124925E-14, -6.500000000000000000 ) ) ;
#29990 = EDGE_LOOP ( 'NONE', ( #42020, #33020, #55717, #37960 ) ) ;
#29991 = CARTESIAN_POINT ( 'NONE',  ( 9.058813317711338797, 136.9549999999999841, -2.943386871421372675 ) ) ;
#29992 = UNCERTAINTY_MEASURE_WITH_UNIT (LENGTH_MEASURE( 1.000000000000000082E-05 ), #37368, 'distance_accuracy_value', 'NONE');
#29993 =( LENGTH_UNIT ( ) NAMED_UNIT ( * ) SI_UNIT ( .MILLI., .METRE. ) );
#29994 = AXIS2_PLACEMENT_3D ( 'NONE', #22926, #12686, #7438 ) ;
#29995 =( NAMED_UNIT ( * ) SI_UNIT ( $, .STERADIAN. ) SOLID_ANGLE_UNIT ( ) );
#29996 = SURFACE_STYLE_FILL_AREA ( #42350 ) ;
#29997 = FILL_AREA_STYLE ('',( #35987 ) ) ;
#29998 = ORIENTED_EDGE ( 'NONE', *, *, #61239, .F. ) ;
#29999 =( LENGTH_UNIT ( ) NAMED_UNIT ( * ) SI_UNIT ( .MILLI., .METRE. ) );
#30000 = CARTESIAN_POINT ( 'NONE',  ( -53.39499999999998892, -6.826472737025115478, -4.959722759717899443 ) ) ;
#30001 = ORIENTED_EDGE ( 'NONE', *, *, #14220, .F. ) ;
#30002 = CARTESIAN_POINT ( 'NONE',  ( 68.99999999999998579, 37.00000000000000000, -3.750000000000000000 ) ) ;
#30003 = CARTESIAN_POINT ( 'NONE',  ( 3.046771365092978190, 72.00000000000001421, -6.349999999999997868 ) ) ;
#30004 = CARTESIAN_POINT ( 'NONE',  ( -86.69292637653380496, 10.01517768586948698, -1.839758294383808966E-15 ) ) ;
#30005 = DIRECTION ( 'NONE',  ( 0.000000000000000000, 0.000000000000000000, -1.000000000000000000 ) ) ;
#30006 = VERTEX_POINT ( 'NONE', #30468 ) ;
#30007 = DIRECTION ( 'NONE',  ( 0.000000000000000000, -0.000000000000000000, -1.000000000000000000 ) ) ;
#30008 = VERTEX_POINT ( 'NONE', #56522 ) ;
#30009 = ADVANCED_FACE ( 'NONE', ( #36514 ), #40730, .T. ) ;
#30010 = DIRECTION ( 'NONE',  ( 0.000000000000000000, 0.000000000000000000, 1.000000000000000000 ) ) ;
#30011 = CARTESIAN_POINT ( 'NONE',  ( -103.2549999999999812, -4.716976649647092401, 6.492361379858946790 ) ) ;
#30012 = EDGE_LOOP ( 'NONE', ( #60018, #37590, #7524, #8812 ) ) ;
#30013 = ADVANCED_FACE ( 'NONE', ( #8362 ), #54313, .T. ) ;
#30014 = CARTESIAN_POINT ( 'NONE',  ( -8.437984349512095861, 118.8070736234661524, -5.166775262442723748E-16 ) ) ;
#30015 = CYLINDRICAL_SURFACE ( 'NONE', #962, 23.00000000000000000 ) ;
#30016 = CARTESIAN_POINT ( 'NONE',  ( -145.5570736234661808, -1.166476076187852838E-15, -9.524999999999991473 ) ) ;
#30017 = CARTESIAN_POINT ( 'NONE',  ( -44.50000000000000000, 10.49999999999998224, -4.000000000000000000 ) ) ;
#30018 = CARTESIAN_POINT ( 'NONE',  ( 10.01517768586949408, 144.6949999999999932, 1.839758294383810543E-15 ) ) ;
#30019 = CARTESIAN_POINT ( 'NONE',  ( -71.45707362346617231, -9.058813317711329915, 2.943386871421371787 ) ) ;
#30020 = EDGE_CURVE ( 'NONE', #39120, #57229, #62201, .T. ) ;
#30021 = SURFACE_SIDE_STYLE ('',( #30701 ) ) ;
#30022 =( NAMED_UNIT ( * ) PLANE_ANGLE_UNIT ( ) SI_UNIT ( $, .RADIAN. ) );
#30023 =( GEOMETRIC_REPRESENTATION_CONTEXT ( 3 ) GLOBAL_UNCERTAINTY_ASSIGNED_CONTEXT ( ( #66471 ) ) GLOBAL_UNIT_ASSIGNED_CONTEXT ( ( #53700, #43216, #59307 ) ) REPRESENTATION_CONTEXT ( 'NONE', 'WORKASPACE' ) );
#30025 = SURFACE_STYLE_FILL_AREA ( #14546 ) ;
#30024 = CARTESIAN_POINT ( 'NONE',  ( 31.00000000000000000, 42.00000000000000000, -79.00402776293826435 ) ) ;
#30026 = AXIS2_PLACEMENT_3D ( 'NONE', #6310, #1682, #66089 ) ;
#30027 = CARTESIAN_POINT ( 'NONE',  ( -123.6549999999999869, -7.632228543268600340, -2.479861379858950166 ) ) ;
#30028 = VECTOR ( 'NONE', #63325, 1000.000000000000000 ) ;
#30029 = SURFACE_STYLE_FILL_AREA ( #34968 ) ;
#30030 = CARTESIAN_POINT ( 'NONE',  ( -1.166476076187854022E-15, 113.9449999999999932, 9.525000000000000355 ) ) ;
#30031 = CARTESIAN_POINT ( 'NONE',  ( -127.4950000000000045, 6.826472737025113702, -4.959722759717902107 ) ) ;
#30032 = EDGE_CURVE ( 'NONE', #37399, #39381, #1491, .T. ) ;
#30033 = CARTESIAN_POINT ( 'NONE',  ( -117.7449999999999903, 4.716976649647094177, 6.492361379858945902 ) ) ;
#30034 = SURFACE_SIDE_STYLE ('',( #25452 ) ) ;
#30035 = ORIENTED_EDGE ( 'NONE', *, *, #42320, .T. ) ;
#30036 = CARTESIAN_POINT ( 'NONE',  ( -71.18918918918917882, 14.09971791521133255, -9.500000000000000000 ) ) ;
#30037 = CARTESIAN_POINT ( 'NONE',  ( 71.50000000000000000, 35.92875272052971525, 7.000000000000000000 ) ) ;
#30038 = EDGE_CURVE ( 'NONE', #60303, #2848, #49872, .T. ) ;
#30039 = CARTESIAN_POINT ( 'NONE',  ( -174.1429263765338078, 5.598654528085800663, -7.705886871421367523 ) ) ;
#30040 = SURFACE_SIDE_STYLE ('',( #56429 ) ) ;
#30041 = CARTESIAN_POINT ( 'NONE',  ( -50.54499999999998039, -7.632228543268600340, -2.479861379858950166 ) ) ;
#30042 = VECTOR ( 'NONE', #31989, 1000.000000000000000 ) ;
#30043 = CARTESIAN_POINT ( 'NONE',  ( 0.000000000000000000, 87.30187232391182306, 8.025000000000000355 ) ) ;
#30044 = FACE_OUTER_BOUND ( 'NONE', #65819, .T. ) ;
#30045 = CARTESIAN_POINT ( 'NONE',  ( 6.062177826491070398, 3.500000000000002665, 0.000000000000000000 ) ) ;
#30046 = ORIENTED_EDGE ( 'NONE', *, *, #40080, .F. ) ;
#30047 = CARTESIAN_POINT ( 'NONE',  ( -86.24292637653380211, 5.598654528085804216, 7.705886871421366635 ) ) ;
#30048 = CARTESIAN_POINT ( 'NONE',  ( 45.50000000000000000, -1.469576158976824618E-14, 6.999999999999999112 ) ) ;
#30049 = CARTESIAN_POINT ( 'NONE',  ( 7.632228543268608334, 123.4570736234661581, -2.479861379858951942 ) ) ;
#30050 = SURFACE_STYLE_USAGE ( .BOTH. , #30742 ) ;
#30051 = DIRECTION ( 'NONE',  ( -0.000000000000000000, 1.000000000000000000, 0.000000000000000000 ) ) ;
#30052 = ORIENTED_EDGE ( 'NONE', *, *, #53298, .F. ) ;
#30053 = CARTESIAN_POINT ( 'NONE',  ( 4.682380833558962507, 5.889878495889167453, 0.4967607073414696539 ) ) ;
#30054 =( NAMED_UNIT ( * ) SI_UNIT ( $, .STERADIAN. ) SOLID_ANGLE_UNIT ( ) );
#30055 = DIRECTION ( 'NONE',  ( 0.000000000000000000, 0.000000000000000000, 1.000000000000000000 ) ) ;
#30056 = ORIENTED_EDGE ( 'NONE', *, *, #40850, .F. ) ;
#30057 =( BOUNDED_CURVE ( )  B_SPLINE_CURVE ( 3, ( #17572, #66417, #49565, #55155 ),
 .UNSPECIFIED., .F., .F. ) 
 B_SPLINE_CURVE_WITH_KNOTS ( ( 4, 4 ),
 ( 1.570796326794883901, 3.141592653589793116 ),
 .UNSPECIFIED. ) 
 CURVE ( )  GEOMETRIC_REPRESENTATION_ITEM ( )  RATIONAL_B_SPLINE_CURVE ( ( 1.000000000000000000, 0.8047378541243619399, 0.8047378541243619399, 1.000000000000000000 ) ) 
 REPRESENTATION_ITEM ( '' )  );
#30058 = CARTESIAN_POINT ( 'NONE',  ( -4.716976649647098618, 131.2570736234661695, 6.492361379858953008 ) ) ;
#30059 = EDGE_CURVE ( 'NONE', #61571, #18083, #63542, .T. ) ;
#30060 = EDGE_LOOP ( 'NONE', ( #4628, #25125, #12089, #642, #66353 ) ) ;
#30061 = SURFACE_STYLE_USAGE ( .BOTH. , #62432 ) ;
#30062 = CARTESIAN_POINT ( 'NONE',  ( -105.2049999999999841, -2.607480562269071545, -8.024999999999991473 ) ) ;
#30063 = CARTESIAN_POINT ( 'NONE',  ( 75.00000000000000000, 19.58219357181276266, -6.973972669042648675 ) ) ;
#30064 = DIRECTION ( 'NONE',  ( -0.000000000000000000, -0.000000000000000000, -1.000000000000000000 ) ) ;
#30065 = AXIS2_PLACEMENT_3D ( 'NONE', #55783, #8644, #62773 ) ;
#30066 = EDGE_LOOP ( 'NONE', ( #60342, #61148, #25632, #27875 ) ) ;
#30067 = CARTESIAN_POINT ( 'NONE',  ( 19.49999999999997513, 8.000000000000000000, -4.000000000000000000 ) ) ;
#30068 = DIRECTION ( 'NONE',  ( 1.000000000000000000, 0.000000000000000000, 0.000000000000000000 ) ) ;
#30069 = LINE ( 'NONE', #51538, #66564 ) ;
#30070 = CARTESIAN_POINT ( 'NONE',  ( -86.39499999999999602, -6.826472737025115478, -4.959722759717899443 ) ) ;
#30071 = EDGE_LOOP ( 'NONE', ( #46833, #29280, #40657, #40030, #2784, #24828 ) ) ;
#30072 = EDGE_CURVE ( 'NONE', #19085, #41992, #67788, .T. ) ;
#30073 = DIRECTION ( 'NONE',  ( -1.000000000000000000, 0.000000000000000000, -0.000000000000000000 ) ) ;
#30074 = FILL_AREA_STYLE_COLOUR ( '', #49881 ) ;
#30075 = ORIENTED_EDGE ( 'NONE', *, *, #59164, .T. ) ;
#30076 = FILL_AREA_STYLE ('',( #67378 ) ) ;
#30077 = DIRECTION ( 'NONE',  ( -0.000000000000000000, -0.000000000000000000, -1.000000000000000000 ) ) ;
#30078 = PRESENTATION_LAYER_ASSIGNMENT (  '', '', ( #33507 ) ) ;
#30079 = ADVANCED_FACE ( 'NONE', ( #68482 ), #31163, .F. ) ;
#30080 = FACE_OUTER_BOUND ( 'NONE', #57217, .T. ) ;
#30081 =( NAMED_UNIT ( * ) PLANE_ANGLE_UNIT ( ) SI_UNIT ( $, .RADIAN. ) );
#30082 = ORIENTED_EDGE ( 'NONE', *, *, #48887, .T. ) ;
#30083 = EDGE_CURVE ( 'NONE', #42973, #57523, #25213, .T. ) ;
#30084 = DIRECTION ( 'NONE',  ( -1.000000000000000000, 0.000000000000000000, 0.000000000000000000 ) ) ;
#30085 = ORIENTED_EDGE ( 'NONE', *, *, #35012, .F. ) ;
#30086 = DIRECTION ( 'NONE',  ( -1.000000000000000000, -0.000000000000000000, -0.000000000000000000 ) ) ;
#30087 =( NAMED_UNIT ( * ) SI_UNIT ( $, .STERADIAN. ) SOLID_ANGLE_UNIT ( ) );
#30088 = CARTESIAN_POINT ( 'NONE',  ( -167.3070736234662093, -10.01517768586948698, 6.132527647946031529E-16 ) ) ;
#30089 = CARTESIAN_POINT ( 'NONE',  ( 10.01517768586949408, 111.6949999999999932, 1.839758294383810543E-15 ) ) ;
#30090 = CARTESIAN_POINT ( 'NONE',  ( -106.4070736234661609, 3.094860106618428031, -9.524999999999993250 ) ) ;
#30091 = DIRECTION ( 'NONE',  ( -0.000000000000000000, -0.000000000000000000, 1.000000000000000000 ) ) ;
#30092 = EDGE_CURVE ( 'NONE', #35716, #14824, #68141, .T. ) ;
#30093 = SURFACE_STYLE_FILL_AREA ( #4755 ) ;
#30094 = ORIENTED_EDGE ( 'NONE', *, *, #22975, .T. ) ;
#30095 = CARTESIAN_POINT ( 'NONE',  ( -107.5429263765337993, 9.058813317711329915, 2.943386871421369566 ) ) ;
#30096 = CARTESIAN_POINT ( 'NONE',  ( -106.5570736234661666, -1.166476076187852838E-15, -9.524999999999991473 ) ) ;
#30097 = EDGE_CURVE ( 'NONE', #41190, #37694, #31923, .T. ) ;
#30099 = DIRECTION ( 'NONE',  ( -0.000000000000000000, 0.000000000000000000, -1.000000000000000000 ) ) ;
#30098 = DIRECTION ( 'NONE',  ( -1.000000000000000000, 0.000000000000000000, 0.000000000000000000 ) ) ;
#30100 = CARTESIAN_POINT ( 'NONE',  ( -147.9550000000000125, -7.632228543268599452, 2.479861379858951054 ) ) ;
#30101 = SURFACE_STYLE_USAGE ( .BOTH. , #8332 ) ;
#30102 = CARTESIAN_POINT ( 'NONE',  ( -147.8929263765338078, -8.102448949553174629, -5.886773742842741797 ) ) ;
#30103 = CARTESIAN_POINT ( 'NONE',  ( -160.7949999999999591, 2.607480562269068880, -8.024999999999993250 ) ) ;
#30104 = CARTESIAN_POINT ( 'NONE',  ( -145.4949999999999477, 6.826472737025113702, -4.959722759717902107 ) ) ;
#30105 = EDGE_LOOP ( 'NONE', ( #23839, #29928, #53486, #57802, #40486, #65723, #51017, #1633, #17980, #67752, #14626, #59468, #2937 ) ) ;
#30106 = DIRECTION ( 'NONE',  ( -1.000000000000000000, 0.000000000000000000, 0.000000000000000000 ) ) ;
#30107 = LINE ( 'NONE', #9028, #15929 ) ;
#30108 = CARTESIAN_POINT ( 'NONE',  ( -61.40499999999999403, -2.607480562269069768, 8.024999999999991473 ) ) ;
#30109 = DIRECTION ( 'NONE',  ( 1.000000000000000000, -1.734723475976805517E-15, 0.000000000000000000 ) ) ;
#30110 = CYLINDRICAL_SURFACE ( 'NONE', #31377, 0.2500000000000002220 ) ;
#30111 = CIRCLE ( 'NONE', #28947, 0.5000000000000004441 ) ;
#30112 = CARTESIAN_POINT ( 'NONE',  ( -58.49499999999998323, 6.826472737025113702, -4.959722759717902107 ) ) ;
#30113 = CARTESIAN_POINT ( 'NONE',  ( 8.102448949553183510, 155.1049999999999898, -5.886773742842746238 ) ) ;
#30114 = EDGE_CURVE ( 'NONE', #38290, #21071, #21797, .T. ) ;
#30115 = FACE_OUTER_BOUND ( 'NONE', #1520, .T. ) ;
#30116 = PRESENTATION_LAYER_ASSIGNMENT (  '', '', ( #29004 ) ) ;
#30117 = EDGE_CURVE ( 'NONE', #14523, #31107, #28570, .T. ) ;
#30118 = DIRECTION ( 'NONE',  ( 1.000000000000000000, -1.776356839400250465E-15, 0.000000000000000000 ) ) ;
#30119 = DIRECTION ( 'NONE',  ( 0.000000000000000000, 0.000000000000000000, 1.000000000000000000 ) ) ;
#30120 = DIRECTION ( 'NONE',  ( 0.000000000000000000, 1.000000000000000000, 0.000000000000000000 ) ) ;
#30121 = STYLED_ITEM ( 'NONE', ( #23987 ), #67921 ) ;
#30122 = CARTESIAN_POINT ( 'NONE',  ( -74.99999999999998579, 50.00000000000000000, 7.000000000000000000 ) ) ;
#30123 = ORIENTED_EDGE ( 'NONE', *, *, #33620, .T. ) ;
#30124 = ORIENTED_EDGE ( 'NONE', *, *, #34801, .T. ) ;
#30125 =( NAMED_UNIT ( * ) SI_UNIT ( $, .STERADIAN. ) SOLID_ANGLE_UNIT ( ) );
#30126 = PRESENTATION_LAYER_ASSIGNMENT (  '', '', ( #9941 ) ) ;
#30127 = DIRECTION ( 'NONE',  ( 0.000000000000000000, -1.000000000000000000, 0.000000000000000000 ) ) ;
#30128 = VERTEX_POINT ( 'NONE', #7141 ) ;
#30130 = ORIENTED_EDGE ( 'NONE', *, *, #65607, .T. ) ;
#30129 = CIRCLE ( 'NONE', #8833, 0.5000000000000004441 ) ;
#30131 = SURFACE_SIDE_STYLE ('',( #62150 ) ) ;
#30132 = FILL_AREA_STYLE_COLOUR ( '', #8421 ) ;
#30133 = ORIENTED_EDGE ( 'NONE', *, *, #58358, .F. ) ;
#30134 = CARTESIAN_POINT ( 'NONE',  ( -8.102448949553181734, 111.0049999999999955, -5.886773742842749790 ) ) ;
#30135 = LINE ( 'NONE', #3737, #614 ) ;
#30136 = ORIENTED_EDGE ( 'NONE', *, *, #19290, .F. ) ;
#30137 = ADVANCED_FACE ( 'NONE', ( #49058 ), #18436, .T. ) ;
#30138 = AXIS2_PLACEMENT_3D ( 'NONE', #60502, #27456, #11990 ) ;
#30139 = SURFACE_SIDE_STYLE ('',( #13629 ) ) ;
#30140 = CARTESIAN_POINT ( 'NONE',  ( -24.00000000000000355, 36.75000000000000000, -4.000000000000000000 ) ) ;
#30141 = CARTESIAN_POINT ( 'NONE',  ( -115.0449999999999875, 7.632228543268600340, 2.479861379858949277 ) ) ;
#30142 = VERTEX_POINT ( 'NONE', #23315 ) ;
#30143 = AXIS2_PLACEMENT_3D ( 'NONE', #42872, #11140, #32587 ) ;
#30144 =( BOUNDED_CURVE ( )  B_SPLINE_CURVE ( 2, ( #31095, #41350, #62753, #52252, #15322, #58193, #20914, #47336, #25822, #42070, #31435 ),
 .UNSPECIFIED., .F., .F. ) 
 B_SPLINE_CURVE_WITH_KNOTS ( ( 3, 2, 2, 2, 2, 3 ),
 ( 0.5326086956521612903, 0.5347826086956395386, 0.5369565217391176759, 0.5391304347825959242, 0.5413043478260740615, 0.5434782608695523098 ),
 .UNSPECIFIED. ) 
 CURVE ( )  GEOMETRIC_REPRESENTATION_ITEM ( )  RATIONAL_B_SPLINE_CURVE ( ( 1.000000000000284883, 0.9510565162948685369, 1.000000000000000000, 0.9510565162951535312, 1.000000000000000000, 0.9510565162951535312, 1.000000000000000000, 0.9510565162951535312, 1.000000000000000000, 0.9510565162954435214, 0.9999999999997100097 ) ) 
 REPRESENTATION_ITEM ( '' )  );
#30145 = CARTESIAN_POINT ( 'NONE',  ( -9.271665717542465046, 110.5000000000000142, -2.225342505666574322 ) ) ;
#30146 = FACE_OUTER_BOUND ( 'NONE', #49478, .T. ) ;
#30147 = EDGE_CURVE ( 'NONE', #26396, #38068, #391, .T. ) ;
#30148 = SURFACE_STYLE_USAGE ( .BOTH. , #46757 ) ;
#30149 = VERTEX_POINT ( 'NONE', #745 ) ;
#30150 = CARTESIAN_POINT ( 'NONE',  ( 2.607480562269076430, 140.7929263765337851, -8.025000000000000355 ) ) ;
#30151 = CARTESIAN_POINT ( 'NONE',  ( -53.32003218646550380, -10.00128081186071327, -3.271960291195576076 ) ) ;
#30152 = COLOUR_RGB ( '', 0.40784314, 0.44705882, 0.49803922) ;
#30153 = AXIS2_PLACEMENT_3D ( 'NONE', #6839, #48767, #44185 ) ;
#30154 = EDGE_CURVE ( 'NONE', #31521, #21181, #55319, .T. ) ;
#30155 = ORIENTED_EDGE ( 'NONE', *, *, #18407, .T. ) ;
#30156 = FILL_AREA_STYLE_COLOUR ( '', #39683 ) ;
#30157 = ORIENTED_EDGE ( 'NONE', *, *, #47574, .T. ) ;
#30158 = DIRECTION ( 'NONE',  ( 0.000000000000000000, 0.000000000000000000, -1.000000000000000000 ) ) ;
#30159 = DIRECTION ( 'NONE',  ( 0.000000000000000000, 0.000000000000000000, -1.000000000000000000 ) ) ;
#30160 = CARTESIAN_POINT ( 'NONE',  ( -20.57648123223228254, 114.4999999999999574, 10.27659574468085069 ) ) ;
#30162 = AXIS2_PLACEMENT_3D ( 'NONE', #26817, #59186, #48352 ) ;
#30161 = DIRECTION ( 'NONE',  ( 1.000000000000000000, 0.000000000000000000, 0.000000000000000000 ) ) ;
#30163 = CARTESIAN_POINT ( 'NONE',  ( -125.0049999999999812, 6.826472737025116366, 4.959722759717898555 ) ) ;
#30164 = LINE ( 'NONE', #53389, #15160 ) ;
#30165 = CARTESIAN_POINT ( 'NONE',  ( 39.24999999999999289, 15.74999999999997513, -3.750000000000000000 ) ) ;
#30166 = LINE ( 'NONE', #8041, #63527 ) ;
#30167 = CARTESIAN_POINT ( 'NONE',  ( -114.0570736234661808, 0.000000000000000000, 9.524999999999991473 ) ) ;
#30168 = ORIENTED_EDGE ( 'NONE', *, *, #60350, .F. ) ;
#30169 = AXIS2_PLACEMENT_3D ( 'NONE', #28353, #23798, #61082 ) ;
#30170 = ORIENTED_EDGE ( 'NONE', *, *, #64312, .T. ) ;
#30171 = SURFACE_STYLE_FILL_AREA ( #56221 ) ;
#30172 = EDGE_CURVE ( 'NONE', #17985, #44158, #54688, .T. ) ;
#30173 =( NAMED_UNIT ( * ) SI_UNIT ( $, .STERADIAN. ) SOLID_ANGLE_UNIT ( ) );
#30174 = DIRECTION ( 'NONE',  ( 1.000000000000000000, 0.000000000000000000, 0.000000000000000000 ) ) ;
#30175 = EDGE_LOOP ( 'NONE', ( #48461, #42553, #8624, #25490 ) ) ;
#30176 = CARTESIAN_POINT ( 'NONE',  ( -179.9049999999999727, 2.607480562269068880, -8.024999999999993250 ) ) ;
#30177 = DIRECTION ( 'NONE',  ( 0.000000000000000000, 0.000000000000000000, 1.000000000000000000 ) ) ;
#30178 = SURFACE_STYLE_USAGE ( .BOTH. , #30524 ) ;
#30179 = CARTESIAN_POINT ( 'NONE',  ( -55.70707362346616520, -3.094860106618431139, -9.524999999999991473 ) ) ;
#30180 = CARTESIAN_POINT ( 'NONE',  ( -177.5949999999999989, 2.607480562269072433, 8.024999999999991473 ) ) ;
#30181 = ORIENTED_EDGE ( 'NONE', *, *, #61518, .F. ) ;
#30182 = SURFACE_STYLE_USAGE ( .BOTH. , #61177 ) ;
#30183 = DIRECTION ( 'NONE',  ( -0.000000000000000000, -0.000000000000000000, -1.000000000000000000 ) ) ;
#30184 = CARTESIAN_POINT ( 'NONE',  ( 4.716976649647099507, 117.7570736234661553, -6.492361379858953008 ) ) ;
#30185 = CARTESIAN_POINT ( 'NONE',  ( -94.25499999999999545, -4.716976649647092401, 6.492361379858946790 ) ) ;
#30186 =( NAMED_UNIT ( * ) PLANE_ANGLE_UNIT ( ) SI_UNIT ( $, .RADIAN. ) );
#30187 = AXIS2_PLACEMENT_3D ( 'NONE', #37872, #21631, #17082 ) ;
#30188 = CARTESIAN_POINT ( 'NONE',  ( -89.84499999999999886, -7.632228543268599452, 2.479861379858951054 ) ) ;
#30189 = CARTESIAN_POINT ( 'NONE',  ( 5.598654528085809545, 128.2549999999999670, -7.705886871421373741 ) ) ;
#30190 = CARTESIAN_POINT ( 'NONE',  ( -65.84499999999998465, -7.632228543268599452, 2.479861379858951054 ) ) ;
#30191 = CARTESIAN_POINT ( 'NONE',  ( -75.00000000000000000, 7.768687147774688384, -6.999999999999999112 ) ) ;
#30192 = AXIS2_PLACEMENT_3D ( 'NONE', #32612, #64973, #17523 ) ;
#30193 =( GEOMETRIC_REPRESENTATION_CONTEXT ( 3 ) GLOBAL_UNCERTAINTY_ASSIGNED_CONTEXT ( ( #63670 ) ) GLOBAL_UNIT_ASSIGNED_CONTEXT ( ( #57685, #21415, #37661 ) ) REPRESENTATION_CONTEXT ( 'NONE', 'WORKASPACE' ) );
#30194 = DIRECTION ( 'NONE',  ( 1.000000000000000000, 0.000000000000000000, 0.000000000000000000 ) ) ;
#30195 = EDGE_CURVE ( 'NONE', #7926, #66803, #54624, .T. ) ;
#30196 =( GEOMETRIC_REPRESENTATION_CONTEXT ( 3 ) GLOBAL_UNCERTAINTY_ASSIGNED_CONTEXT ( ( #25497 ) ) GLOBAL_UNIT_ASSIGNED_CONTEXT ( ( #41734, #25508, #68435 ) ) REPRESENTATION_CONTEXT ( 'NONE', 'WORKASPACE' ) );
#30197 = DIRECTION ( 'NONE',  ( 0.000000000000000000, 0.000000000000000000, -1.000000000000000000 ) ) ;
#30198 = SURFACE_SIDE_STYLE ('',( #4508 ) ) ;
#30199 = ORIENTED_EDGE ( 'NONE', *, *, #23202, .T. ) ;
#30200 = CARTESIAN_POINT ( 'NONE',  ( -116.9929263765337879, 8.102448949553171076, -5.886773742842744461 ) ) ;
#30201 = CARTESIAN_POINT ( 'NONE',  ( -125.8449999999999847, -7.632228543268599452, 2.479861379858951054 ) ) ;
#30202 = SURFACE_STYLE_FILL_AREA ( #8779 ) ;
#30203 =( GEOMETRIC_REPRESENTATION_CONTEXT ( 3 ) GLOBAL_UNCERTAINTY_ASSIGNED_CONTEXT ( ( #5286 ) ) GLOBAL_UNIT_ASSIGNED_CONTEXT ( ( #37377, #27086, #48620 ) ) REPRESENTATION_CONTEXT ( 'NONE', 'WORKASPACE' ) );
#30204 = CIRCLE ( 'NONE', #8892, 1.000000000000000888 ) ;
#30205 = DIRECTION ( 'NONE',  ( -1.156482317317870344E-15, -1.000000000000000000, -0.000000000000000000 ) ) ;
#30207 = CARTESIAN_POINT ( 'NONE',  ( 24.00000000000000355, 36.75000000000000000, 4.000000000000000000 ) ) ;
#30206 = CARTESIAN_POINT ( 'NONE',  ( -17.41962728626436530, -0.1139526552317604857, -2.000000000000000000 ) ) ;
#30208 = CYLINDRICAL_SURFACE ( 'NONE', #43004, 1.000000000000000888 ) ;
#30209 = VERTEX_POINT ( 'NONE', #22275 ) ;
#30210 = ORIENTED_EDGE ( 'NONE', *, *, #68145, .F. ) ;
#30211 = FACE_OUTER_BOUND ( 'NONE', #15075, .T. ) ;
#30212 = AXIS2_PLACEMENT_3D ( 'NONE', #52555, #4302, #39414 ) ;
#30213 = CARTESIAN_POINT ( 'NONE',  ( -2.607480562269157254, 147.0929263765338249, -8.024999999999939959 ) ) ;
#30214 = DIRECTION ( 'NONE',  ( 0.000000000000000000, -1.000000000000000000, 0.000000000000000000 ) ) ;
#30215 = CARTESIAN_POINT ( 'NONE',  ( 27.99999999999999645, 5.000000000000000000, 24.00402776293821816 ) ) ;
#30216 = CARTESIAN_POINT ( 'NONE',  ( -8.701243704650556410, -2.329718218673039853, 2.929003814506404790 ) ) ;
#30217 = EDGE_LOOP ( 'NONE', ( #66049, #15493, #9764, #52088 ) ) ;
#30218 = CARTESIAN_POINT ( 'NONE',  ( -134.3050000000000068, 8.437984349512086979, -1.550032578732815448E-15 ) ) ;
#30219 = VERTEX_POINT ( 'NONE', #1453 ) ;
#30220 = CARTESIAN_POINT ( 'NONE',  ( 0.000000000000000000, 0.000000000000000000, 0.000000000000000000 ) ) ;
#30221 = CARTESIAN_POINT ( 'NONE',  ( -122.7570736234661695, -5.598654528085801552, 7.705886871421367523 ) ) ;
#30222 = ORIENTED_EDGE ( 'NONE', *, *, #28474, .F. ) ;
#30223 = CARTESIAN_POINT ( 'NONE',  ( 44.50000000000000000, 10.36037961002804408, -3.500000000000000000 ) ) ;
#30224 = CARTESIAN_POINT ( 'NONE',  ( -47.50000000000000000, 14.49137674618942562, -9.500000000000000000 ) ) ;
#30225 = ORIENTED_EDGE ( 'NONE', *, *, #7555, .T. ) ;
#30226 = ADVANCED_FACE ( 'NONE', ( #33525, #6436 ), #6781, .F. ) ;
#30227 = CARTESIAN_POINT ( 'NONE',  ( -8.102448949553181734, 136.8949999999999534, -5.886773742842749790 ) ) ;
#30228 = SURFACE_STYLE_USAGE ( .BOTH. , #56988 ) ;
#30229 = ORIENTED_EDGE ( 'NONE', *, *, #48415, .F. ) ;
#30230 = CARTESIAN_POINT ( 'NONE',  ( 0.000000000000000000, 146.5549999999999784, -9.525000000000000355 ) ) ;
#30231 = VERTEX_POINT ( 'NONE', #22983 ) ;
#30232 = CARTESIAN_POINT ( 'NONE',  ( -4.716976649647097730, 120.2429263765338163, -6.492361379858953896 ) ) ;
#30233 = SURFACE_SIDE_STYLE ('',( #35559 ) ) ;
#30234 = AXIS2_PLACEMENT_3D ( 'NONE', #42376, #37450, #5354 ) ;
#30235 = ADVANCED_FACE ( 'NONE', ( #4796 ), #44481, .F. ) ;
#30236 = PLANE ( 'NONE',  #65813 ) ;
#30237 = ORIENTED_EDGE ( 'NONE', *, *, #18330, .T. ) ;
#30238 = EDGE_CURVE ( 'NONE', #36309, #12165, #11724, .T. ) ;
#30239 = CARTESIAN_POINT ( 'NONE',  ( 72.00000000000000000, 13.41640786499872284, -9.500000000000000000 ) ) ;
#30240 = ORIENTED_EDGE ( 'NONE', *, *, #41920, .F. ) ;
#30241 = AXIS2_PLACEMENT_3D ( 'NONE', #64941, #54725, #43892 ) ;
#30242 = SURFACE_SIDE_STYLE ('',( #9875 ) ) ;
#30243 = CARTESIAN_POINT ( 'NONE',  ( -11.00000000000000000, 8.000000000000000000, -3.500000000000017764 ) ) ;
#30244 = CARTESIAN_POINT ( 'NONE',  ( -151.8549999999999898, 4.716976649647094177, 6.492361379858945902 ) ) ;
#30246 = ORIENTED_EDGE ( 'NONE', *, *, #69649, .F. ) ;
#30245 = ADVANCED_FACE ( 'NONE', ( #47778 ), #42479, .F. ) ;
#30247 = DIRECTION ( 'NONE',  ( 0.6216216216216311485, -0.7833176619561784682, 0.000000000000000000 ) ) ;
#30248 = CIRCLE ( 'NONE', #37045, 0.5000000000000004441 ) ;
#30249 = ADVANCED_FACE ( 'NONE', ( #49371 ), #6096, .F. ) ;
#30250 = PRESENTATION_STYLE_ASSIGNMENT (( #51055 ) ) ;
#30251 = CIRCLE ( 'NONE', #15727, 5.000000000000000000 ) ;
#30252 = CARTESIAN_POINT ( 'NONE',  ( 57.49999999999998579, 30.74999999999999289, -3.750000000000000000 ) ) ;
#30253 = CARTESIAN_POINT ( 'NONE',  ( 74.65811388300841145, 19.88603796100278132, 6.000000000000000000 ) ) ;
#30254 = DIRECTION ( 'NONE',  ( -0.000000000000000000, 1.000000000000000000, -0.000000000000000000 ) ) ;
#30255 = VERTEX_POINT ( 'NONE', #61289 ) ;
#30256 = TOROIDAL_SURFACE ( 'NONE', #14567, 0.5000000000000000000, 0.2500000000000000000 ) ;
#30257 = FACE_OUTER_BOUND ( 'NONE', #37465, .T. ) ;
#30258 = ORIENTED_EDGE ( 'NONE', *, *, #4568, .T. ) ;
#30259 = FACE_OUTER_BOUND ( 'NONE', #10397, .T. ) ;
#30260 = EDGE_CURVE ( 'NONE', #1406, #33970, #38706, .T. ) ;
#30261 =( NAMED_UNIT ( * ) PLANE_ANGLE_UNIT ( ) SI_UNIT ( $, .RADIAN. ) );
#30262 = CARTESIAN_POINT ( 'NONE',  ( -78.35499999999997556, -4.716976649647093289, -6.492361379858945902 ) ) ;
#30263 = ORIENTED_EDGE ( 'NONE', *, *, #61031, .F. ) ;
#30264 = SURFACE_STYLE_USAGE ( .BOTH. , #25686 ) ;
#30265 = CYLINDRICAL_SURFACE ( 'NONE', #37470, 112.9999999999981526 ) ;
#30266 = SPHERICAL_SURFACE ( 'NONE', #35324, 1.000000000000000000 ) ;
#30267 = CIRCLE ( 'NONE', #22401, 17.42000000000001236 ) ;
#30268 = ORIENTED_EDGE ( 'NONE', *, *, #61855, .F. ) ;
#30269 =( NAMED_UNIT ( * ) SI_UNIT ( $, .STERADIAN. ) SOLID_ANGLE_UNIT ( ) );
#30270 = AXIS2_PLACEMENT_3D ( 'NONE', #54168, #31066, #22170 ) ;
#30271 =( LENGTH_UNIT ( ) NAMED_UNIT ( * ) SI_UNIT ( .MILLI., .METRE. ) );
#30272 = CARTESIAN_POINT ( 'NONE',  ( 9.058813317711337021, 135.5449999999999875, 2.943386871421375783 ) ) ;
#30273 = CARTESIAN_POINT ( 'NONE',  ( -96.29500000000000171, -2.607480562269069768, 8.024999999999991473 ) ) ;
#30274 = CYLINDRICAL_SURFACE ( 'NONE', #34129, 9.524999999999991473 ) ;
#30275 = LINE ( 'NONE', #36319, #42715 ) ;
#30276 = CARTESIAN_POINT ( 'NONE',  ( -9.827790563157511022E-16, 145.4429263765338192, 8.025000000000000355 ) ) ;
#30278 = VERTEX_POINT ( 'NONE', #66937 ) ;
#30277 = CIRCLE ( 'NONE', #65146, 0.5000000000000004441 ) ;
#30279 = CARTESIAN_POINT ( 'NONE',  ( -141.1429263765338078, 5.598654528085800663, -7.705886871421367523 ) ) ;
#30280 = CARTESIAN_POINT ( 'NONE',  ( -158.6949999999999648, -8.437984349512085203, 5.166775262442717831E-16 ) ) ;
#30281 = CARTESIAN_POINT ( 'NONE',  ( -24.75000000000000355, 37.00000000000000000, -3.000000000000000000 ) ) ;
#30282 = COLOUR_RGB ( '', 0.09019608, 0.27058824, 0.51372549) ;
#30283 = CONICAL_SURFACE ( 'NONE', #39335, 5.499999999999976907, 0.7853981633974309595 ) ;
#30284 = FILL_AREA_STYLE_COLOUR ( '', #28199 ) ;
#30285 = EDGE_LOOP ( 'NONE', ( #24312, #62180, #62524, #45334 ) ) ;
#30286 = CARTESIAN_POINT ( 'NONE',  ( 4.750000000000002665, 24.74999999999998579, 4.000000000000000000 ) ) ;
#30287 = ORIENTED_EDGE ( 'NONE', *, *, #21562, .F. ) ;
#30288 = AXIS2_PLACEMENT_3D ( 'NONE', #17960, #45433, #66853 ) ;
#30289 = SURFACE_SIDE_STYLE ('',( #56718 ) ) ;
#30290 =( GEOMETRIC_REPRESENTATION_CONTEXT ( 3 ) GLOBAL_UNCERTAINTY_ASSIGNED_CONTEXT ( ( #16625 ) ) GLOBAL_UNIT_ASSIGNED_CONTEXT ( ( #3002, #13963, #18871 ) ) REPRESENTATION_CONTEXT ( 'NONE', 'WORKASPACE' ) );
#30291 = LINE ( 'NONE', #35259, #39448 ) ;
#30292 = CARTESIAN_POINT ( 'NONE',  ( 66.24999999999998579, 34.24999999999999289, 3.750000000000000000 ) ) ;
#30293 = DIRECTION ( 'NONE',  ( 0.000000000000000000, 0.000000000000000000, -1.000000000000000000 ) ) ;
#30294 = AXIS2_PLACEMENT_3D ( 'NONE', #61365, #8959, #24419 ) ;
#30295 = ORIENTED_EDGE ( 'NONE', *, *, #47304, .F. ) ;
#30296 = CARTESIAN_POINT ( 'NONE',  ( -164.9049999999999727, 2.607480562269069324, -8.024999999999993250 ) ) ;
#30297 = VERTEX_POINT ( 'NONE', #56352 ) ;
#30298 = DIRECTION ( 'NONE',  ( 1.000000000000000000, 0.000000000000000000, 0.000000000000000000 ) ) ;
#30299 = CARTESIAN_POINT ( 'NONE',  ( -15.48999599679679662, 118.4999999999999716, 7.500000000000000000 ) ) ;
#30300 = ORIENTED_EDGE ( 'NONE', *, *, #56652, .T. ) ;
#30301 = EDGE_CURVE ( 'NONE', #48146, #60196, #24009, .T. ) ;
#30302 = COLOUR_RGB ( '', 0.72549020, 0.75294118, 0.79215686) ;
#30303 = FACE_OUTER_BOUND ( 'NONE', #31520, .T. ) ;
#30304 = CARTESIAN_POINT ( 'NONE',  ( -57.05707362346618083, 0.000000000000000000, 9.524999999999991473 ) ) ;
#30305 = CARTESIAN_POINT ( 'NONE',  ( 3.094860106618435136, 112.2949999999999733, -9.525000000000000355 ) ) ;
#30306 = CIRCLE ( 'NONE', #11258, 113.0000000000030127 ) ;
#30307 = EDGE_CURVE ( 'NONE', #32128, #45031, #25201, .T. ) ;
#30308 = STYLED_ITEM ( 'NONE', ( #65441 ), #25286 ) ;
#30309 = ORIENTED_EDGE ( 'NONE', *, *, #11826, .T. ) ;
#30310 = CARTESIAN_POINT ( 'NONE',  ( -142.5570736234661808, -1.166476076187852838E-15, -9.524999999999991473 ) ) ;
#30311 = CARTESIAN_POINT ( 'NONE',  ( -71.00499999999996703, 6.826472737025115478, 4.959722759717899443 ) ) ;
#30312 = CARTESIAN_POINT ( 'NONE',  ( -40.99999999999998579, 108.0041655821620168, -3.000000000000004441 ) ) ;
#30313 = ORIENTED_EDGE ( 'NONE', *, *, #9635, .F. ) ;
#30314 = CARTESIAN_POINT ( 'NONE',  ( -3.094860106618432471, 137.7049999999999841, -9.525000000000000355 ) ) ;
#30315 =( GEOMETRIC_REPRESENTATION_CONTEXT ( 3 ) GLOBAL_UNCERTAINTY_ASSIGNED_CONTEXT ( ( #62134 ) ) GLOBAL_UNIT_ASSIGNED_CONTEXT ( ( #66825, #61861, #45740 ) ) REPRESENTATION_CONTEXT ( 'NONE', 'WORKASPACE' ) );
#30316 =( NAMED_UNIT ( * ) SI_UNIT ( $, .STERADIAN. ) SOLID_ANGLE_UNIT ( ) );
#30317 = ADVANCED_FACE ( 'NONE', ( #61979 ), #40210, .T. ) ;
#30318 = FACE_OUTER_BOUND ( 'NONE', #40678, .T. ) ;
#30319 = CARTESIAN_POINT ( 'NONE',  ( 19.98288066869250201, 115.0281754944747235, 9.999999999997170264 ) ) ;
#30320 = FACE_OUTER_BOUND ( 'NONE', #58349, .T. ) ;
#30321 = EDGE_CURVE ( 'NONE', #11929, #30560, #52481, .T. ) ;
#30322 = SURFACE_STYLE_FILL_AREA ( #29997 ) ;
#30323 = EDGE_LOOP ( 'NONE', ( #1646, #7888 ) ) ;
#30324 = DIRECTION ( 'NONE',  ( -0.000000000000000000, -0.000000000000000000, -1.000000000000000000 ) ) ;
#30325 = CYLINDRICAL_SURFACE ( 'NONE', #56395, 4.999999999999999112 ) ;
#30326 = CARTESIAN_POINT ( 'NONE',  ( -179.1550000000000011, 7.632228543268600340, 2.479861379858949277 ) ) ;
#30327 = ORIENTED_EDGE ( 'NONE', *, *, #43064, .F. ) ;
#30328 = DIRECTION ( 'NONE',  ( 0.000000000000000000, 1.000000000000000000, 0.000000000000000000 ) ) ;
#30329 = DIRECTION ( 'NONE',  ( 0.000000000000000000, 0.000000000000000000, 1.000000000000000000 ) ) ;
#30330 = DIRECTION ( 'NONE',  ( 0.7239014318309263674, -0.3935725838095961437, -0.5666280422522106397 ) ) ;
#30331 = ADVANCED_FACE ( 'NONE', ( #45518 ), #66579, .T. ) ;
#30332 =( NAMED_UNIT ( * ) SI_UNIT ( $, .STERADIAN. ) SOLID_ANGLE_UNIT ( ) );
#30333 = VERTEX_POINT ( 'NONE', #40917 ) ;
#30334 =( LENGTH_UNIT ( ) NAMED_UNIT ( * ) SI_UNIT ( .MILLI., .METRE. ) );
#30335 = CARTESIAN_POINT ( 'NONE',  ( 109.0067032876572455, 13.00000000000000178, -19.20378738324562207 ) ) ;
#30336 = ORIENTED_EDGE ( 'NONE', *, *, #25242, .T. ) ;
#30337 = CARTESIAN_POINT ( 'NONE',  ( -106.2549999999999955, -4.716976649647092401, 6.492361379858946790 ) ) ;
#30338 = EDGE_LOOP ( 'NONE', ( #951, #7280, #39278 ) ) ;
#30339 = COLOUR_RGB ( '', 0.09019608, 0.27058824, 0.51372549) ;
#30340 = CARTESIAN_POINT ( 'NONE',  ( -137.9070736234661751, -3.094860106618429807, 9.524999999999991473 ) ) ;
#30341 = COLOUR_RGB ( '', 0.09019608, 0.27058824, 0.51372549) ;
#30342 = DIRECTION ( 'NONE',  ( -1.000000000000000000, 0.000000000000000000, 0.000000000000000000 ) ) ;
#30343 = CARTESIAN_POINT ( 'NONE',  ( -3.094860106618432471, 142.5949999999999989, -9.525000000000000355 ) ) ;
#30344 = CARTESIAN_POINT ( 'NONE',  ( -78.50707362346615525, 8.102448949553176405, 5.886773742842740909 ) ) ;
#30345 = VECTOR ( 'NONE', #46000, 1000.000000000000000 ) ;
#30346 = PLANE ( 'NONE',  #29126 ) ;
#30347 = ORIENTED_EDGE ( 'NONE', *, *, #24553, .T. ) ;
#30348 = DIRECTION ( 'NONE',  ( 0.000000000000000000, -1.000000000000000000, 0.000000000000000000 ) ) ;
#30349 = STYLED_ITEM ( 'NONE', ( #45515 ), #52525 ) ;
#30350 = CARTESIAN_POINT ( 'NONE',  ( -19.96684271803530564, -11.98607768299615728, -0.6619469921969921566 ) ) ;
#30351 = DIRECTION ( 'NONE',  ( 1.000000000000000000, 0.000000000000000000, 0.000000000000000000 ) ) ;
#30352 = CARTESIAN_POINT ( 'NONE',  ( -118.2549999999999812, -4.716976649647092401, 6.492361379858946790 ) ) ;
#30353 = CARTESIAN_POINT ( 'NONE',  ( -9.058813317711338797, 110.3449999999999847, 2.943386871421373563 ) ) ;
#30354 = CARTESIAN_POINT ( 'NONE',  ( -125.3949999999999818, -6.826472737025115478, -4.959722759717899443 ) ) ;
#30355 = CIRCLE ( 'NONE', #40552, 16.99999999999998579 ) ;
#30356 = STYLED_ITEM ( 'NONE', ( #54083 ), #15754 ) ;
#30357 = DIRECTION ( 'NONE',  ( 0.000000000000000000, 1.000000000000000000, 0.000000000000000000 ) ) ;
#30358 = ORIENTED_EDGE ( 'NONE', *, *, #47156, .T. ) ;
#30359 = ADVANCED_FACE ( 'NONE', ( #29269 ), #56638, .F. ) ;
#30360 = AXIS2_PLACEMENT_3D ( 'NONE', #65260, #5452, #26901 ) ;
#30361 = SURFACE_STYLE_USAGE ( .BOTH. , #56079 ) ;
#30362 = FACE_OUTER_BOUND ( 'NONE', #1000, .T. ) ;
#30363 = CARTESIAN_POINT ( 'NONE',  ( -170.5429263765338135, 9.058813317711329915, 2.943386871421369566 ) ) ;
#30364 = AXIS2_PLACEMENT_3D ( 'NONE', #19571, #56870, #30109 ) ;
#30365 = FACE_OUTER_BOUND ( 'NONE', #61947, .T. ) ;
#30366 = CARTESIAN_POINT ( 'NONE',  ( -15.75000000000000000, 4.336808689942018722E-16, 24.00000000000000000 ) ) ;
#30367 = DIRECTION ( 'NONE',  ( -0.000000000000000000, -0.000000000000000000, -1.000000000000000000 ) ) ;
#30368 = ORIENTED_EDGE ( 'NONE', *, *, #30092, .F. ) ;
#30369 = CONICAL_SURFACE ( 'NONE', #59560, 3.100000000000000533, 0.7853981633974447263 ) ;
#30370 = CARTESIAN_POINT ( 'NONE',  ( -82.79292637653379927, -3.094860106618429807, 9.524999999999991473 ) ) ;
#30371 =( NAMED_UNIT ( * ) PLANE_ANGLE_UNIT ( ) SI_UNIT ( $, .RADIAN. ) );
#30372 = DIRECTION ( 'NONE',  ( 0.000000000000000000, 0.000000000000000000, -1.000000000000000000 ) ) ;
#30373 = AXIS2_PLACEMENT_3D ( 'NONE', #62671, #63721, #52513 ) ;
#30374 = COLOUR_RGB ( '', 0.66274510, 0.83137255, 0.94901961) ;
#30375 = DIRECTION ( 'NONE',  ( -6.938893903907222856E-15, -0.000000000000000000, -1.000000000000000000 ) ) ;
#30376 = FILL_AREA_STYLE ('',( #19143 ) ) ;
#30377 = EDGE_CURVE ( 'NONE', #40156, #13502, #37608, .T. ) ;
#30378 = CARTESIAN_POINT ( 'NONE',  ( -156.5070736234661410, 8.102448949553176405, 5.886773742842740909 ) ) ;
#30379 = ADVANCED_FACE ( 'NONE', ( #40563 ), #4331, .T. ) ;
#30380 = VERTEX_POINT ( 'NONE', #58117 ) ;
#30381 = CARTESIAN_POINT ( 'NONE',  ( -150.0570736234661808, 0.000000000000000000, 9.524999999999991473 ) ) ;
#30382 = FACE_OUTER_BOUND ( 'NONE', #54372, .T. ) ;
#30383 = AXIS2_PLACEMENT_3D ( 'NONE', #63111, #8960, #35353 ) ;
#30384 = CARTESIAN_POINT ( 'NONE',  ( 11.00000000000000000, 8.000000000000000000, 3.500000000000003997 ) ) ;
#30385 = ORIENTED_EDGE ( 'NONE', *, *, #23124, .T. ) ;
#30386 = DIRECTION ( 'NONE',  ( -0.000000000000000000, -1.000000000000000000, -0.000000000000000000 ) ) ;
#30387 =( GEOMETRIC_REPRESENTATION_CONTEXT ( 3 ) GLOBAL_UNCERTAINTY_ASSIGNED_CONTEXT ( ( #49001 ) ) GLOBAL_UNIT_ASSIGNED_CONTEXT ( ( #26256, #42838, #53678 ) ) REPRESENTATION_CONTEXT ( 'NONE', 'WORKASPACE' ) );
#30388 = DIRECTION ( 'NONE',  ( 1.000000000000000000, 0.000000000000000000, 0.000000000000000000 ) ) ;
#30389 = CARTESIAN_POINT ( 'NONE',  ( -6.826472737025120807, 133.5070736234661410, -4.959722759717907437 ) ) ;
#30390 = SURFACE_SIDE_STYLE ('',( #38680 ) ) ;
#30391 = ADVANCED_FACE ( 'NONE', ( #25727 ), #31707, .T. ) ;
#30392 = ORIENTED_EDGE ( 'NONE', *, *, #61100, .F. ) ;
#30393 = CARTESIAN_POINT ( 'NONE',  ( -103.8549999999999898, 4.716976649647094177, 6.492361379858945902 ) ) ;
#30394 = COLOUR_RGB ( '', 0.09019608, 0.27058824, 0.51372549) ;
#30395 = ORIENTED_EDGE ( 'NONE', *, *, #24615, .T. ) ;
#30396 = CARTESIAN_POINT ( 'NONE',  ( -103.7070736234671671, -3.094860106634834018, -9.524999999988075672 ) ) ;
#30397 = SURFACE_STYLE_FILL_AREA ( #16624 ) ;
#30398 = SURFACE_SIDE_STYLE ('',( #7584 ) ) ;
#30399 = ADVANCED_FACE ( 'NONE', ( #63379 ), #63713, .F. ) ;
#30400 = ORIENTED_EDGE ( 'NONE', *, *, #12769, .T. ) ;
#30401 = CARTESIAN_POINT ( 'NONE',  ( -74.99999999999998579, 50.00000000000000000, -6.500000000000000000 ) ) ;
#30402 = CARTESIAN_POINT ( 'NONE',  ( -77.39499999999999602, -6.826472737025115478, -4.959722759717899443 ) ) ;
#30403 = ORIENTED_EDGE ( 'NONE', *, *, #52082, .F. ) ;
#30404 = AXIS2_PLACEMENT_3D ( 'NONE', #64588, #31158, #16434 ) ;
#30405 = CARTESIAN_POINT ( 'NONE',  ( 18.25000000000000711, 33.99999999999999289, 4.000000000000000000 ) ) ;
#30406 = CARTESIAN_POINT ( 'NONE',  ( -40.99999999999998579, 107.7459666690149902, -3.075798416731281293 ) ) ;
#30407 = SURFACE_SIDE_STYLE ('',( #61725 ) ) ;
#30408 = ADVANCED_FACE ( 'NONE', ( #52846 ), #33441, .T. ) ;
#30409 = UNCERTAINTY_MEASURE_WITH_UNIT (LENGTH_MEASURE( 1.000000000000000082E-05 ), #29378, 'distance_accuracy_value', 'NONE');
#30410 = VERTEX_POINT ( 'NONE', #32061 ) ;
#30411 = DIRECTION ( 'NONE',  ( 0.000000000000000000, 0.000000000000000000, 1.000000000000000000 ) ) ;
#30412 = B_SPLINE_CURVE_WITH_KNOTS ( 'NONE', 3,
 ( #30745, #62750, #30053, #36439, #62425, #36053, #35357, #57496 ),
 .UNSPECIFIED., .F., .F.,
 ( 4, 2, 2, 4 ),
 ( 2.544316211733585141E-07, 0.002094919859796809478, 0.003142252573884625911, 0.004189585287972442777 ),
 .UNSPECIFIED. ) ;
#30413 = CARTESIAN_POINT ( 'NONE',  ( 44.50000000000000000, 10.36037961002804408, -3.500000000000000000 ) ) ;
#30414 = DIRECTION ( 'NONE',  ( 3.469446951953611033E-15, 0.000000000000000000, -1.000000000000000000 ) ) ;
#30415 = ORIENTED_EDGE ( 'NONE', *, *, #50668, .T. ) ;
#30416 = ORIENTED_EDGE ( 'NONE', *, *, #36248, .T. ) ;
#30417 = DIRECTION ( 'NONE',  ( 4.449603764765679692E-17, -0.9396926207859105373, 0.3420201433256630508 ) ) ;
#30418 = LINE ( 'NONE', #20232, #61084 ) ;
#30419 = CARTESIAN_POINT ( 'NONE',  ( -171.0570736234661808, 0.000000000000000000, 9.524999999999991473 ) ) ;
#30420 = STYLED_ITEM ( 'NONE', ( #69255 ), #59708 ) ;
#30421 =( NAMED_UNIT ( * ) SI_UNIT ( $, .STERADIAN. ) SOLID_ANGLE_UNIT ( ) );
#30422 = CARTESIAN_POINT ( 'NONE',  ( 5.598654528085809545, 118.1449999999999818, -7.705886871421373741 ) ) ;
#30423 = CARTESIAN_POINT ( 'NONE',  ( -104.3070736234661666, -10.01517768586948698, 6.132527647946031529E-16 ) ) ;
#30424 = MECHANICAL_DESIGN_GEOMETRIC_PRESENTATION_REPRESENTATION (  '', ( #58575 ), #67508 ) ;
#30425 = CARTESIAN_POINT ( 'NONE',  ( 4.716976649647096842, 112.7429263765338163, 6.492361379858953896 ) ) ;
#30426 = TOROIDAL_SURFACE ( 'NONE', #2261, 17.00000000000000355, 1.000000000000000000 ) ;
#30427 = CARTESIAN_POINT ( 'NONE',  ( 57.00000000000000000, 0.9999999999999991118, 80.00402776293826435 ) ) ;
#30428 = PRODUCT ( '11. Nut M10', '11. Nut M10', '', ( #12477 ) ) ;
#30429 = ORIENTED_EDGE ( 'NONE', *, *, #37632, .T. ) ;
#30430 =( BOUNDED_CURVE ( )  B_SPLINE_CURVE ( 2, ( #56095, #56443, #6870, #2588, #51184, #45600, #39265, #67348, #67017, #18807, #40290 ),
 .UNSPECIFIED., .F., .F. ) 
 B_SPLINE_CURVE_WITH_KNOTS ( ( 3, 2, 2, 2, 2, 3 ),
 ( 0.7500000000000000000, 0.7521739130434782483, 0.7543478260869564966, 0.7565217391304347450, 0.7586956521739129933, 0.7608695652173913526 ),
 .UNSPECIFIED. ) 
 CURVE ( )  GEOMETRIC_REPRESENTATION_ITEM ( )  RATIONAL_B_SPLINE_CURVE ( ( 1.000000000000000000, 0.9510565162951535312, 1.000000000000000000, 0.9510565162951535312, 1.000000000000000000, 0.9510565162951535312, 1.000000000000000000, 0.9510565162951535312, 1.000000000000000000, 0.9510565162951535312, 1.000000000000000000 ) ) 
 REPRESENTATION_ITEM ( '' )  );
#30433 = STYLED_ITEM ( 'NONE', ( #10161 ), #13616 ) ;
#30432 = DIRECTION ( 'NONE',  ( -0.000000000000000000, -0.000000000000000000, 1.000000000000000000 ) ) ;
#30431 = CARTESIAN_POINT ( 'NONE',  ( 0.000000000000000000, 0.000000000000000000, 0.000000000000000000 ) ) ;
#30434 = DIRECTION ( 'NONE',  ( -0.000000000000000000, -1.000000000000000000, -0.000000000000000000 ) ) ;
#30435 = CARTESIAN_POINT ( 'NONE',  ( -147.3549999999999898, -4.716976649647093289, -6.492361379858945902 ) ) ;
#30436 = CARTESIAN_POINT ( 'NONE',  ( -0.8084438751943111567, 110.6282398156186986, -9.370611995446433085 ) ) ;
#30437 = AXIS2_PLACEMENT_3D ( 'NONE', #39794, #40136, #14395 ) ;
#30438 = CARTESIAN_POINT ( 'NONE',  ( -151.4949999999999761, 6.826472737025113702, -4.959722759717902107 ) ) ;
#30439 = CARTESIAN_POINT ( 'NONE',  ( -152.3949999999999818, -6.826472737025113702, -4.959722759717900331 ) ) ;
#30440 = VERTEX_POINT ( 'NONE', #60173 ) ;
#30441 = EDGE_CURVE ( 'NONE', #20781, #40082, #28589, .T. ) ;
#30442 = AXIS2_PLACEMENT_3D ( 'NONE', #32222, #20980, #37566 ) ;
#30443 = DIRECTION ( 'NONE',  ( -0.000000000000000000, 1.000000000000000000, -0.000000000000000000 ) ) ;
#30444 = DIRECTION ( 'NONE',  ( 1.000000000000000000, -0.000000000000000000, -1.300977106640434891E-16 ) ) ;
#30445 = PRESENTATION_STYLE_ASSIGNMENT (( #16064 ) ) ;
#30446 = UNCERTAINTY_MEASURE_WITH_UNIT (LENGTH_MEASURE( 1.000000000000000082E-05 ), #6040, 'distance_accuracy_value', 'NONE');
#30447 = CARTESIAN_POINT ( 'NONE',  ( -68.00499999999998124, 6.826472737025116366, 4.959722759717898555 ) ) ;
#30448 = CARTESIAN_POINT ( 'NONE',  ( 57.24999999999999289, 28.24999999999998934, 3.750000000000000000 ) ) ;
#30449 = VECTOR ( 'NONE', #50921, 1000.000000000000000 ) ;
#30450 = CARTESIAN_POINT ( 'NONE',  ( -65.39499999999998181, -6.826472737025113702, -4.959722759717900331 ) ) ;
#30451 = CARTESIAN_POINT ( 'NONE',  ( 9.058813317711338797, 151.9550000000000125, -2.943386871421372675 ) ) ;
#30452 = CARTESIAN_POINT ( 'NONE',  ( -142.8570736234661638, -5.598654528085803328, -7.705886871421366635 ) ) ;
#30453 = PRESENTATION_LAYER_ASSIGNMENT (  '', '', ( #60781 ) ) ;
#30454 = DIRECTION ( 'NONE',  ( 0.000000000000000000, 1.000000000000000000, 0.000000000000000000 ) ) ;
#30455 = UNCERTAINTY_MEASURE_WITH_UNIT (LENGTH_MEASURE( 1.000000000000000082E-05 ), #37729, 'distance_accuracy_value', 'NONE');
#30456 =( BOUNDED_CURVE ( )  B_SPLINE_CURVE ( 2, ( #27030, #48563, #260, #54128, #25665, #47183, #68604, #20399, #58057, #9863, #12245 ),
 .UNSPECIFIED., .F., .F. ) 
 B_SPLINE_CURVE_WITH_KNOTS ( ( 3, 2, 2, 2, 2, 3 ),
 ( 0.9782608695652174058, 0.9804347826086956541, 0.9826086956521739024, 0.9847826086956521507, 0.9869565217391303991, 0.9891304347826086474 ),
 .UNSPECIFIED. ) 
 CURVE ( )  GEOMETRIC_REPRESENTATION_ITEM ( )  RATIONAL_B_SPLINE_CURVE ( ( 1.000000000000000000, 0.9510565162951535312, 1.000000000000000000, 0.9510565162951535312, 1.000000000000000000, 0.9510565162951535312, 1.000000000000000000, 0.9510565162951535312, 1.000000000000000000, 0.9510565162951535312, 1.000000000000000000 ) ) 
 REPRESENTATION_ITEM ( '' )  );
#30457 = CIRCLE ( 'NONE', #28186, 0.5000000000000004441 ) ;
#30458 = DIRECTION ( 'NONE',  ( -4.762568680546987317E-16, 5.551115123125782702E-17, 1.000000000000000000 ) ) ;
#30459 = CARTESIAN_POINT ( 'NONE',  ( 0.4644249260832968851, 42.85561104658234655, -45.52242297229210521 ) ) ;
#30460 = EDGE_CURVE ( 'NONE', #25339, #11319, #35802, .T. ) ;
#30461 = EDGE_CURVE ( 'NONE', #59113, #63964, #27447, .T. ) ;
#30462 = CARTESIAN_POINT ( 'NONE',  ( -2.525713312987405423, 110.7492558248162737, 8.932758862731871474 ) ) ;
#30463 = CARTESIAN_POINT ( 'NONE',  ( 3.000000000000030198, 0.000000000000000000, 3.772833609257260986E-15 ) ) ;
#30464 = STYLED_ITEM ( 'NONE', ( #58397 ), #28103 ) ;
#30465 = ADVANCED_FACE ( 'NONE', ( #6355 ), #39862, .T. ) ;
#30466 = FACE_OUTER_BOUND ( 'NONE', #29990, .T. ) ;
#30467 = EDGE_CURVE ( 'NONE', #16826, #27375, #65804, .T. ) ;
#30468 = CARTESIAN_POINT ( 'NONE',  ( -25.00000000000000000, 1.000000000000000000, -3.000000000000000000 ) ) ;
#30469 =( NAMED_UNIT ( * ) PLANE_ANGLE_UNIT ( ) SI_UNIT ( $, .RADIAN. ) );
#30470 = ORIENTED_EDGE ( 'NONE', *, *, #1916, .T. ) ;
#30471 = ORIENTED_EDGE ( 'NONE', *, *, #12634, .F. ) ;
#30472 = DIRECTION ( 'NONE',  ( 0.000000000000000000, -0.000000000000000000, 1.000000000000000000 ) ) ;
#30473 = AXIS2_PLACEMENT_3D ( 'NONE', #1441, #17705, #26816 ) ;
#30474 = DIRECTION ( 'NONE',  ( 1.000000000000000000, 0.000000000000000000, 0.000000000000000000 ) ) ;
#30475 = STYLED_ITEM ( 'NONE', ( #34931 ), #45982 ) ;
#30476 = EDGE_CURVE ( 'NONE', #68708, #360, #33106, .T. ) ;
#30477 = VECTOR ( 'NONE', #24150, 1000.000000000000000 ) ;
#30478 = CARTESIAN_POINT ( 'NONE',  ( 10.00000000000002132, 50.00000000000000000, 60.00000000000000000 ) ) ;
#30479 = DIRECTION ( 'NONE',  ( 0.000000000000000000, 0.000000000000000000, 1.000000000000000000 ) ) ;
#30480 = ADVANCED_FACE ( 'NONE', ( #43014 ), #65665, .T. ) ;
#30481 = ORIENTED_EDGE ( 'NONE', *, *, #23659, .T. ) ;
#30482 = PRESENTATION_LAYER_ASSIGNMENT (  '', '', ( #29342 ) ) ;
#30483 = ORIENTED_EDGE ( 'NONE', *, *, #2861, .T. ) ;
#30484 = VERTEX_POINT ( 'NONE', #670 ) ;
#30485 = CARTESIAN_POINT ( 'NONE',  ( -5.598654528085806881, 116.8549999999999898, -7.705886871421374629 ) ) ;
#30486 = DIRECTION ( 'NONE',  ( 0.000000000000000000, 0.000000000000000000, 1.000000000000000000 ) ) ;
#30487 = EDGE_LOOP ( 'NONE', ( #35302, #33402, #19232, #60986 ) ) ;
#30488 = PRESENTATION_LAYER_ASSIGNMENT (  '', '', ( #24872 ) ) ;
#30489 = FACE_OUTER_BOUND ( 'NONE', #13453, .T. ) ;
#30490 = CARTESIAN_POINT ( 'NONE',  ( -110.9950000000000045, -6.826472737025115478, 4.959722759717900331 ) ) ;
#30491 = VERTEX_POINT ( 'NONE', #45434 ) ;
#30492 = CARTESIAN_POINT ( 'NONE',  ( 44.91886116991580735, 9.999999999999980460, 3.201362207699192997 ) ) ;
#30493 = CARTESIAN_POINT ( 'NONE',  ( -164.1570736234661751, -9.058813317711329915, -2.943386871421370898 ) ) ;
#30494 = CARTESIAN_POINT ( 'NONE',  ( 71.50000000000000000, 14.49137674618942562, 9.500000000000000000 ) ) ;
#30495 = VERTEX_POINT ( 'NONE', #12666 ) ;
#30496 = CARTESIAN_POINT ( 'NONE',  ( -2.607480562269073765, 141.0929263765338249, -8.025000000000000355 ) ) ;
#30497 = DIRECTION ( 'NONE',  ( -0.000000000000000000, -0.000000000000000000, -1.000000000000000000 ) ) ;
#30498 = VECTOR ( 'NONE', #56435, 1000.000000000000000 ) ;
#30499 = CYLINDRICAL_SURFACE ( 'NONE', #17232, 3.000000000000000444 ) ;
#30500 = VECTOR ( 'NONE', #1501, 1000.000000000000000 ) ;
#30501 = EDGE_LOOP ( 'NONE', ( #23014, #13560, #13969, #55410 ) ) ;
#30502 = EDGE_LOOP ( 'NONE', ( #67384, #21759, #31471, #59150, #14076, #738 ) ) ;
#30503 = CARTESIAN_POINT ( 'NONE',  ( -9.827790563157511022E-16, 127.4429263765338192, 8.025000000000000355 ) ) ;
#30504 = PLANE ( 'NONE',  #30143 ) ;
#30505 = CARTESIAN_POINT ( 'NONE',  ( -140.3929263765338078, 8.102448949553176405, 5.886773742842740909 ) ) ;
#30506 = CARTESIAN_POINT ( 'NONE',  ( 179.4361977533490347, 5.000000000000000000, -103.7004518695263044 ) ) ;
#30507 = CARTESIAN_POINT ( 'NONE',  ( -127.8549999999999898, 4.716976649647094177, 6.492361379858945902 ) ) ;
#30508 =( NAMED_UNIT ( * ) PLANE_ANGLE_UNIT ( ) SI_UNIT ( $, .RADIAN. ) );
#30509 = EDGE_CURVE ( 'NONE', #30255, #21436, #38602, .T. ) ;
#30510 = CARTESIAN_POINT ( 'NONE',  ( -70.75000000000000000, -0.9999999999999995559, 19.00000000000000000 ) ) ;
#30511 = VECTOR ( 'NONE', #13299, 1000.000000000000227 ) ;
#30512 = DIRECTION ( 'NONE',  ( 1.000000000000000000, 0.000000000000000000, 0.000000000000000000 ) ) ;
#30513 = DIRECTION ( 'NONE',  ( 0.000000000000000000, 0.000000000000000000, 1.000000000000000000 ) ) ;
#30514 = DIRECTION ( 'NONE',  ( -1.000000000000000000, 0.000000000000000000, 0.000000000000000000 ) ) ;
#30515 = ORIENTED_EDGE ( 'NONE', *, *, #48985, .F. ) ;
#30516 = VERTEX_POINT ( 'NONE', #3098 ) ;
#30517 = FACE_BOUND ( 'NONE', #55068, .T. ) ;
#30518 = FILL_AREA_STYLE ('',( #4844 ) ) ;
#30519 = DIRECTION ( 'NONE',  ( 0.000000000000000000, 0.000000000000000000, -1.000000000000000000 ) ) ;
#30520 = CARTESIAN_POINT ( 'NONE',  ( 60.00000000000000000, 1.797044900979284448E-15, 9.500000000000000000 ) ) ;
#30521 = VERTEX_POINT ( 'NONE', #29177 ) ;
#30522 =( LENGTH_UNIT ( ) NAMED_UNIT ( * ) SI_UNIT ( .MILLI., .METRE. ) );
#30523 = CARTESIAN_POINT ( 'NONE',  ( -179.6049999999999898, 6.826472737025113702, -4.959722759717902107 ) ) ;
#30524 = SURFACE_SIDE_STYLE ('',( #3063 ) ) ;
#30525 = CARTESIAN_POINT ( 'NONE',  ( -50.45707362346615810, -9.058813317711329915, 2.943386871421371787 ) ) ;
#30526 = MECHANICAL_DESIGN_GEOMETRIC_PRESENTATION_REPRESENTATION (  '', ( #41786 ), #48574 ) ;
#30527 = CARTESIAN_POINT ( 'NONE',  ( -178.1949999999999648, 8.437984349512086979, -1.550032578732815448E-15 ) ) ;
#30528 =( NAMED_UNIT ( * ) SI_UNIT ( $, .STERADIAN. ) SOLID_ANGLE_UNIT ( ) );
#30529 = ORIENTED_EDGE ( 'NONE', *, *, #48963, .F. ) ;
#30530 = FILL_AREA_STYLE_COLOUR ( '', #25687 ) ;
#30531 = VECTOR ( 'NONE', #20489, 1000.000000000000000 ) ;
#30532 = VECTOR ( 'NONE', #67333, 1000.000000000000000 ) ;
#30533 = PRESENTATION_STYLE_ASSIGNMENT (( #57284 ) ) ;
#30534 = LINE ( 'NONE', #67152, #62993 ) ;
#30535 = CARTESIAN_POINT ( 'NONE',  ( -87.95499999999999829, -7.632228543268599452, 2.479861379858951054 ) ) ;
#30536 = CYLINDRICAL_SURFACE ( 'NONE', #17459, 1.000000000000000888 ) ;
#30537 = CARTESIAN_POINT ( 'NONE',  ( -168.8070736234661808, 10.01517768586948698, -1.839758294383808966E-15 ) ) ;
#30538 = CIRCLE ( 'NONE', #45211, 3.600000000000005862 ) ;
#30539 = FILL_AREA_STYLE_COLOUR ( '', #30302 ) ;
#30540 = CARTESIAN_POINT ( 'NONE',  ( -92.39499999999998181, -6.826472737025113702, -4.959722759717900331 ) ) ;
#30541 = CARTESIAN_POINT ( 'NONE',  ( -3.094860106618434248, 123.9049999999999727, 9.525000000000000355 ) ) ;
#30542 = CARTESIAN_POINT ( 'NONE',  ( -65.69499999999999318, -8.437984349512085203, 5.166775262442717831E-16 ) ) ;
#30543 = CARTESIAN_POINT ( 'NONE',  ( 20.54906699372407175, 114.6596276111864228, -10.28538896680103853 ) ) ;
#30544 = SURFACE_STYLE_FILL_AREA ( #8771 ) ;
#30545 = PRESENTATION_LAYER_ASSIGNMENT (  '', '', ( #12567 ) ) ;
#30546 = FACE_OUTER_BOUND ( 'NONE', #19637, .T. ) ;
#30547 = UNCERTAINTY_MEASURE_WITH_UNIT (LENGTH_MEASURE( 1.000000000000000082E-05 ), #20589, 'distance_accuracy_value', 'NONE');
#30548 = PLANE ( 'NONE',  #18033 ) ;
#30549 = ORIENTED_EDGE ( 'NONE', *, *, #6120, .T. ) ;
#30550 = EDGE_CURVE ( 'NONE', #63380, #52516, #7413, .T. ) ;
#30551 = CARTESIAN_POINT ( 'NONE',  ( -101.0929263765338106, 3.094860106618433360, 9.524999999999991473 ) ) ;
#30552 = CARTESIAN_POINT ( 'NONE',  ( -125.2449999999999903, -4.716976649647093289, -6.492361379858945902 ) ) ;
#30553 = CARTESIAN_POINT ( 'NONE',  ( -7.632228543268608334, 145.9570736234661581, 2.479861379858952830 ) ) ;
#30554 = ADVANCED_FACE ( 'NONE', ( #39796 ), #34817, .T. ) ;
#30555 = STYLED_ITEM ( 'NONE', ( #4671 ), #28790 ) ;
#30557 = DIRECTION ( 'NONE',  ( 0.000000000000000000, 0.000000000000000000, 1.000000000000000000 ) ) ;
#30556 = DIRECTION ( 'NONE',  ( 0.000000000000000000, 0.000000000000000000, -1.000000000000000000 ) ) ;
#30558 = DIRECTION ( 'NONE',  ( -1.084202172485503448E-16, 1.000000000000000000, 0.000000000000000000 ) ) ;
#30559 = ORIENTED_EDGE ( 'NONE', *, *, #59801, .F. ) ;
#30560 = VERTEX_POINT ( 'NONE', #7054 ) ;
#30561 = SURFACE_STYLE_FILL_AREA ( #9145 ) ;
#30562 =( BOUNDED_CURVE ( )  B_SPLINE_CURVE ( 3, ( #16656, #43069, #10663, #64473 ),
 .UNSPECIFIED., .F., .F. ) 
 B_SPLINE_CURVE_WITH_KNOTS ( ( 4, 4 ),
 ( 3.931838538365183489, 4.712388980384689674 ),
 .UNSPECIFIED. ) 
 CURVE ( )  GEOMETRIC_REPRESENTATION_ITEM ( )  RATIONAL_B_SPLINE_CURVE ( ( 1.000000000000000000, 0.9498695926598449413, 0.9498695926598449413, 1.000000000000000000 ) ) 
 REPRESENTATION_ITEM ( '' )  );
#30563 = STYLED_ITEM ( 'NONE', ( #42371 ), #25659 ) ;
#30564 = LINE ( 'NONE', #46106, #67518 ) ;
#30565 = CARTESIAN_POINT ( 'NONE',  ( -98.00707362346616947, -8.102448949553174629, -5.886773742842741797 ) ) ;
#30566 = VECTOR ( 'NONE', #33144, 1000.000000000000000 ) ;
#30567 = SURFACE_STYLE_USAGE ( .BOTH. , #14398 ) ;
#30568 = CYLINDRICAL_SURFACE ( 'NONE', #362, 1.000000000000000888 ) ;
#30569 = EDGE_CURVE ( 'NONE', #20128, #41095, #44226, .T. ) ;
#30570 = EDGE_LOOP ( 'NONE', ( #8232, #41223, #62195, #39799 ) ) ;
#30571 = CARTESIAN_POINT ( 'NONE',  ( -124.1049999999999756, -6.826472737025113702, 4.959722759717902107 ) ) ;
#30572 = ORIENTED_EDGE ( 'NONE', *, *, #64102, .T. ) ;
#30573 = CARTESIAN_POINT ( 'NONE',  ( 21.25000000000001066, 24.74999999999998224, 4.000000000000000000 ) ) ;
#30574 = CARTESIAN_POINT ( 'NONE',  ( -118.4070736234661751, 3.094860106618428031, -9.524999999999993250 ) ) ;
#30575 = VERTEX_POINT ( 'NONE', #55588 ) ;
#30576 = DIRECTION ( 'NONE',  ( 0.000000000000000000, 0.000000000000000000, -1.000000000000000000 ) ) ;
#30577 = PRESENTATION_STYLE_ASSIGNMENT (( #61903 ) ) ;
#30578 = ORIENTED_EDGE ( 'NONE', *, *, #22261, .T. ) ;
#30579 = DIRECTION ( 'NONE',  ( -9.811390859391774840E-17, 1.000000000000000000, 0.000000000000000000 ) ) ;
#30580 = CARTESIAN_POINT ( 'NONE',  ( -8.102448949553181734, 146.4950000000000045, 5.886773742842747126 ) ) ;
#30581 = ORIENTED_EDGE ( 'NONE', *, *, #51054, .T. ) ;
#30582 = CARTESIAN_POINT ( 'NONE',  ( -195.0000000000000000, 0.000000000000000000, 9.524999999999991473 ) ) ;
#30583 = CARTESIAN_POINT ( 'NONE',  ( -10.01517768586949408, 147.3049999999999500, -6.132527647946036459E-16 ) ) ;
#30584 = CYLINDRICAL_SURFACE ( 'NONE', #44086, 1.000000000000000000 ) ;
#30585 = PRESENTATION_STYLE_ASSIGNMENT (( #58052 ) ) ;
#30586 = VERTEX_POINT ( 'NONE', #67180 ) ;
#30587 = CARTESIAN_POINT ( 'NONE',  ( -2.607480562269075097, 112.2929263765337993, 8.025000000000000355 ) ) ;
#30588 = SURFACE_STYLE_FILL_AREA ( #45782 ) ;
#30589 = UNCERTAINTY_MEASURE_WITH_UNIT (LENGTH_MEASURE( 1.000000000000000082E-05 ), #44578, 'distance_accuracy_value', 'NONE');
#30590 = CARTESIAN_POINT ( 'NONE',  ( -68.49999999999998579, -1.919947267060472329E-14, 10.00000000000000000 ) ) ;
#30591 = CIRCLE ( 'NONE', #209, 0.2500000000000002220 ) ;
#30592 = CARTESIAN_POINT ( 'NONE',  ( -139.9429263765337907, 0.000000000000000000, 9.524999999999991473 ) ) ;
#30593 = LINE ( 'NONE', #35895, #35491 ) ;
#30594 = EDGE_CURVE ( 'NONE', #10826, #33018, #32937, .T. ) ;
#30595 = ORIENTED_EDGE ( 'NONE', *, *, #46685, .F. ) ;
#30596 = CIRCLE ( 'NONE', #12626, 0.5000000000000004441 ) ;
#30597 = CARTESIAN_POINT ( 'NONE',  ( 23.71231517720798010, 113.4999999999999858, 7.500000000000000000 ) ) ;
#30598 = ORIENTED_EDGE ( 'NONE', *, *, #15538, .T. ) ;
#30599 = CARTESIAN_POINT ( 'NONE',  ( -62.69292637653379785, 10.01517768586948698, -1.839758294383808571E-15 ) ) ;
#30600 = CARTESIAN_POINT ( 'NONE',  ( -4.250000000000001776, 21.99999999999998579, 4.000000000000000000 ) ) ;
#30601 = CARTESIAN_POINT ( 'NONE',  ( -157.1049999999999898, -6.826472737025115478, 4.959722759717900331 ) ) ;
#30603 = ORIENTED_EDGE ( 'NONE', *, *, #25023, .T. ) ;
#30602 = AXIS2_PLACEMENT_3D ( 'NONE', #66164, #17334, #54577 ) ;
#30604 = EDGE_CURVE ( 'NONE', #27455, #5374, #2406, .T. ) ;
#30605 = CARTESIAN_POINT ( 'NONE',  ( -184.0000000000000000, -8.446573402700972011, 1.153699593821606140 ) ) ;
#30606 = UNCERTAINTY_MEASURE_WITH_UNIT (LENGTH_MEASURE( 1.000000000000000082E-05 ), #20747, 'distance_accuracy_value', 'NONE');
#30607 = AXIS2_PLACEMENT_3D ( 'NONE', #38096, #64789, #64088 ) ;
#30608 = DIRECTION ( 'NONE',  ( 0.000000000000000000, 0.000000000000000000, 1.000000000000000000 ) ) ;
#30609 = CARTESIAN_POINT ( 'NONE',  ( -54.08341698273633824, -9.461864478049029969, 4.963675025618371706 ) ) ;
#30610 = CARTESIAN_POINT ( 'NONE',  ( 75.00000000000000000, 19.58219357181275555, 6.973972669042709960 ) ) ;
#30611 = ORIENTED_EDGE ( 'NONE', *, *, #17123, .F. ) ;
#30612 = EDGE_LOOP ( 'NONE', ( #60608, #43981 ) ) ;
#30613 = DIRECTION ( 'NONE',  ( 1.387778780781444413E-14, -1.000000000000000000, 0.000000000000000000 ) ) ;
#30614 = STYLED_ITEM ( 'NONE', ( #22049 ), #6977 ) ;
#30615 = MECHANICAL_DESIGN_GEOMETRIC_PRESENTATION_REPRESENTATION (  '', ( #4808 ), #9304 ) ;
#30616 = CARTESIAN_POINT ( 'NONE',  ( -64.10499999999997556, -6.826472737025115478, 4.959722759717900331 ) ) ;
#30617 = ORIENTED_EDGE ( 'NONE', *, *, #59722, .F. ) ;
#30618 = CARTESIAN_POINT ( 'NONE',  ( 57.00000000000000000, 13.00000000000000178, 60.00402776293827145 ) ) ;
#30619 = AXIS2_PLACEMENT_3D ( 'NONE', #23437, #17834, #35044 ) ;
#30620 = CARTESIAN_POINT ( 'NONE',  ( -41.49999999999997868, 10.49999999999998224, 3.000000000000000000 ) ) ;
#30621 = ORIENTED_EDGE ( 'NONE', *, *, #6583, .F. ) ;
#30622 = AXIS2_PLACEMENT_3D ( 'NONE', #65495, #64465, #33486 ) ;
#30623 = PRESENTATION_STYLE_ASSIGNMENT (( #9205 ) ) ;
#30624 = SURFACE_STYLE_USAGE ( .BOTH. , #37008 ) ;
#30625 = COLOUR_RGB ( '', 0.31764706, 0.68627451, 0.89019608) ;
#30627 = DIRECTION ( 'NONE',  ( 0.8660254037844387076, 0.000000000000000000, -0.4999999999999999445 ) ) ;
#30626 = CARTESIAN_POINT ( 'NONE',  ( 60.00000000000000000, 115.4999999999999574, -10.00000000000000000 ) ) ;
#30628 = CARTESIAN_POINT ( 'NONE',  ( -10.01517768586949231, 149.1950000000000216, -6.132527647946036459E-16 ) ) ;
#30629 = CARTESIAN_POINT ( 'NONE',  ( -94.49499999999999034, 6.826472737025113702, -4.959722759717902107 ) ) ;
#30630 = EDGE_CURVE ( 'NONE', #11216, #5105, #49990, .T. ) ;
#30631 = CARTESIAN_POINT ( 'NONE',  ( 57.00000000000000000, 16.00000000000000000, 60.00402776293825724 ) ) ;
#30632 = DIRECTION ( 'NONE',  ( 0.000000000000000000, 0.000000000000000000, -1.000000000000000000 ) ) ;
#30633 = UNCERTAINTY_MEASURE_WITH_UNIT (LENGTH_MEASURE( 1.000000000000000082E-05 ), #2426, 'distance_accuracy_value', 'NONE');
#30634 = CARTESIAN_POINT ( 'NONE',  ( -71.69292637653379074, 10.01517768586948698, -1.839758294383808966E-15 ) ) ;
#30635 = CIRCLE ( 'NONE', #40827, 26.49999999999999645 ) ;
#30636 = ORIENTED_EDGE ( 'NONE', *, *, #65878, .F. ) ;
#30637 = CARTESIAN_POINT ( 'NONE',  ( -143.2429263765338021, 5.598654528085804216, 7.705886871421366635 ) ) ;
#30638 = SHAPE_REPRESENTATION_RELATIONSHIP ( 'NONE' , 'NONE' ,  #10054, #13706 ) ;
#30639 = CARTESIAN_POINT ( 'NONE',  ( -156.2949999999999591, -2.607480562269069768, 8.024999999999991473 ) ) ;
#30640 = PRESENTATION_LAYER_ASSIGNMENT (  '', '', ( #41903 ) ) ;
#30641 = EDGE_CURVE ( 'NONE', #51351, #51980, #30815, .T. ) ;
#30642 = CARTESIAN_POINT ( 'NONE',  ( -3.000000000000000000, -3.499999999999999556, 24.00000000000000000 ) ) ;
#30643 = VECTOR ( 'NONE', #62597, 1000.000000000000000 ) ;
#30644 = CARTESIAN_POINT ( 'NONE',  ( -8.750000000000001776, 24.99999999999998579, -3.750000000000000000 ) ) ;
#30645 = FACE_OUTER_BOUND ( 'NONE', #10993, .T. ) ;
#30646 = ORIENTED_EDGE ( 'NONE', *, *, #44284, .T. ) ;
#30647 = DIRECTION ( 'NONE',  ( 0.000000000000000000, 0.000000000000000000, 1.000000000000000000 ) ) ;
#30648 = ORIENTED_EDGE ( 'NONE', *, *, #33756, .F. ) ;
#30649 = EDGE_CURVE ( 'NONE', #21587, #29817, #36937, .T. ) ;
#30650 = FACE_OUTER_BOUND ( 'NONE', #55546, .T. ) ;
#30651 =( GEOMETRIC_REPRESENTATION_CONTEXT ( 3 ) GLOBAL_UNCERTAINTY_ASSIGNED_CONTEXT ( ( #8076 ) ) GLOBAL_UNIT_ASSIGNED_CONTEXT ( ( #65736, #66070, #55528 ) ) REPRESENTATION_CONTEXT ( 'NONE', 'WORKASPACE' ) );
#30652 = CARTESIAN_POINT ( 'NONE',  ( -142.9429263765337907, 0.000000000000000000, 9.524999999999991473 ) ) ;
#30653 = CARTESIAN_POINT ( 'NONE',  ( 6.826472737025119919, 118.8929263765337936, 4.959722759717908325 ) ) ;
#30654 = DIRECTION ( 'NONE',  ( 0.000000000000000000, 1.000000000000000000, 0.000000000000000000 ) ) ;
#30655 = DIRECTION ( 'NONE',  ( -1.000000000000000000, 0.000000000000000000, 0.000000000000000000 ) ) ;
#30656 = AXIS2_PLACEMENT_3D ( 'NONE', #6898, #65299, #38266 ) ;
#30657 = EDGE_CURVE ( 'NONE', #62435, #52329, #31814, .T. ) ;
#30658 = ORIENTED_EDGE ( 'NONE', *, *, #40160, .T. ) ;
#30659 = CARTESIAN_POINT ( 'NONE',  ( -158.9050000000000011, 2.607480562269069324, -8.024999999999993250 ) ) ;
#30660 = CIRCLE ( 'NONE', #3672, 18.99999999999998934 ) ;
#30661 = ORIENTED_EDGE ( 'NONE', *, *, #52765, .F. ) ;
#30662 = CARTESIAN_POINT ( 'NONE',  ( -46.88569120782204891, 5.598654528085803328, -7.705886871421366635 ) ) ;
#30663 = DIRECTION ( 'NONE',  ( -0.8660254037844384856, 0.000000000000000000, 0.5000000000000004441 ) ) ;
#30664 = ORIENTED_EDGE ( 'NONE', *, *, #54408, .F. ) ;
#30665 = CYLINDRICAL_SURFACE ( 'NONE', #23666, 1.000000000000000888 ) ;
#30666 = DIRECTION ( 'NONE',  ( 1.000000000000000000, 0.000000000000000000, 0.000000000000000000 ) ) ;
#30667 = CARTESIAN_POINT ( 'NONE',  ( -3.094860106618432471, 112.5949999999999989, -9.525000000000000355 ) ) ;
#30668 = ORIENTED_EDGE ( 'NONE', *, *, #60745, .F. ) ;
#30669 = CARTESIAN_POINT ( 'NONE',  ( -58.49292637653379501, -8.102448949553174629, 5.886773742842742685 ) ) ;
#30670 = CARTESIAN_POINT ( 'NONE',  ( -5.598654528085808657, 120.7549999999999812, 7.705886871421373741 ) ) ;
#30671 = CARTESIAN_POINT ( 'NONE',  ( -77.90499999999997272, 2.607480562269069324, -8.024999999999993250 ) ) ;
#30672 = VERTEX_POINT ( 'NONE', #23921 ) ;
#30673 = CARTESIAN_POINT ( 'NONE',  ( 3.094860106618435136, 140.4050000000000011, -9.525000000000000355 ) ) ;
#30674 = UNCERTAINTY_MEASURE_WITH_UNIT (LENGTH_MEASURE( 1.000000000000000082E-05 ), #49968, 'distance_accuracy_value', 'NONE');
#30675 = CARTESIAN_POINT ( 'NONE',  ( 15.98999599679679839, 146.4999999999999716, -7.500000000000000000 ) ) ;
#30676 = CARTESIAN_POINT ( 'NONE',  ( -183.3519149756361912, 1.436423777000723276E-13, -9.173085024363883733 ) ) ;
#30677 = SURFACE_STYLE_USAGE ( .BOTH. , #3944 ) ;
#30678 = CYLINDRICAL_SURFACE ( 'NONE', #9249, 0.2500000000000002220 ) ;
#30679 = ORIENTED_EDGE ( 'NONE', *, *, #50513, .F. ) ;
#30680 = CIRCLE ( 'NONE', #305, 0.2500000000000002220 ) ;
#30681 = FILL_AREA_STYLE_COLOUR ( '', #27220 ) ;
#30682 = CARTESIAN_POINT ( 'NONE',  ( -7.766391886667105560, -1.733608113333017453, -0.5482146608018624301 ) ) ;
#30683 = CARTESIAN_POINT ( 'NONE',  ( -179.0050000000000239, 6.826472737025116366, 4.959722759717898555 ) ) ;
#30684 = VERTEX_POINT ( 'NONE', #56633 ) ;
#30685 = CARTESIAN_POINT ( 'NONE',  ( 8.003604573459384142, 111.5754815414098289, -2.762566347670379674 ) ) ;
#30686 = DIRECTION ( 'NONE',  ( -0.000000000000000000, 1.000000000000000000, 0.000000000000000000 ) ) ;
#30687 = ORIENTED_EDGE ( 'NONE', *, *, #12925, .T. ) ;
#30688 = FILL_AREA_STYLE_COLOUR ( '', #62369 ) ;
#30689 = EDGE_LOOP ( 'NONE', ( #46368, #2214, #54553, #66451 ) ) ;
#30690 = SURFACE_SIDE_STYLE ('',( #2250 ) ) ;
#30691 = FACE_OUTER_BOUND ( 'NONE', #38058, .T. ) ;
#30692 = CARTESIAN_POINT ( 'NONE',  ( -92.60500000000000398, 6.826472737025113702, -4.959722759717902107 ) ) ;
#30694 = ORIENTED_EDGE ( 'NONE', *, *, #1860, .T. ) ;
#30693 = AXIS2_PLACEMENT_3D ( 'NONE', #56440, #13881, #35348 ) ;
#30695 = CARTESIAN_POINT ( 'NONE',  ( -45.00000000000000000, 0.000000000000000000, 0.000000000000000000 ) ) ;
#30696 = CARTESIAN_POINT ( 'NONE',  ( 57.75000000000005684, 1.335737076502141715E-13, 3.750000000000000000 ) ) ;
#30697 = CARTESIAN_POINT ( 'NONE',  ( -140.4570736234661865, -9.058813317711329915, 2.943386871421371787 ) ) ;
#30698 = CARTESIAN_POINT ( 'NONE',  ( 9.058813317711338797, 153.8449999999999704, -2.943386871421372675 ) ) ;
#30699 = CARTESIAN_POINT ( 'NONE',  ( -76.70707362346617231, -3.094860106618431139, -9.524999999999991473 ) ) ;
#30700 = CIRCLE ( 'NONE', #29609, 12.50000000000000178 ) ;
#30701 = SURFACE_STYLE_FILL_AREA ( #51156 ) ;
#30702 = AXIS2_PLACEMENT_3D ( 'NONE', #62584, #46466, #68932 ) ;
#30703 = EDGE_LOOP ( 'NONE', ( #27824, #19842, #23929 ) ) ;
#30704 = CARTESIAN_POINT ( 'NONE',  ( 19.00000000000000000, 8.000000000000000000, 4.000000000000000000 ) ) ;
#30705 = DIRECTION ( 'NONE',  ( -1.000000000000000000, 0.000000000000000000, 3.469446951953610639E-15 ) ) ;
#30707 =( NAMED_UNIT ( * ) SI_UNIT ( $, .STERADIAN. ) SOLID_ANGLE_UNIT ( ) );
#30706 = SURFACE_STYLE_FILL_AREA ( #36406 ) ;
#30708 = CIRCLE ( 'NONE', #9405, 4.000000000000000000 ) ;
#30709 = AXIS2_PLACEMENT_3D ( 'NONE', #15133, #59725, #21756 ) ;
#30710 = CARTESIAN_POINT ( 'NONE',  ( -120.6549999999999869, -7.632228543268600340, -2.479861379858950166 ) ) ;
#30711 = CARTESIAN_POINT ( 'NONE',  ( -5.598654528085808657, 116.6449999999999818, 7.705886871421373741 ) ) ;
#30712 = CARTESIAN_POINT ( 'NONE',  ( -128.3949999999999534, -6.826472737025115478, -4.959722759717899443 ) ) ;
#30713 = EDGE_CURVE ( 'NONE', #63323, #5366, #8460, .T. ) ;
#30714 = DIRECTION ( 'NONE',  ( -0.000000000000000000, -1.000000000000000000, 0.000000000000000000 ) ) ;
#30715 = EDGE_LOOP ( 'NONE', ( #57890, #43327, #53480, #11919 ) ) ;
#30716 = EDGE_CURVE ( 'NONE', #7659, #38142, #6119, .T. ) ;
#30717 = FACE_OUTER_BOUND ( 'NONE', #42954, .T. ) ;
#30718 = PRESENTATION_LAYER_ASSIGNMENT (  '', '', ( #65531 ) ) ;
#30720 = EDGE_CURVE ( 'NONE', #41886, #21325, #34477, .T. ) ;
#30719 = DIRECTION ( 'NONE',  ( 0.000000000000000000, 0.000000000000000000, 1.000000000000000000 ) ) ;
#30721 = AXIS2_PLACEMENT_3D ( 'NONE', #59639, #64915, #11459 ) ;
#30722 = ORIENTED_EDGE ( 'NONE', *, *, #791, .T. ) ;
#30723 = CARTESIAN_POINT ( 'NONE',  ( 3.414213562373098032, 42.99999999999999289, -90.00000000000001421 ) ) ;
#30724 = CARTESIAN_POINT ( 'NONE',  ( -173.5429263765338135, 9.058813317711329915, 2.943386871421369566 ) ) ;
#30725 = CARTESIAN_POINT ( 'NONE',  ( -181.3449999999999989, 7.632228543268599452, -2.479861379858951942 ) ) ;
#30726 = EDGE_CURVE ( 'NONE', #11361, #52535, #24093, .T. ) ;
#30727 = EDGE_CURVE ( 'NONE', #68401, #51757, #63424, .T. ) ;
#30728 = DIRECTION ( 'NONE',  ( 0.000000000000000000, -0.000000000000000000, 1.000000000000000000 ) ) ;
#30729 = ADVANCED_FACE ( 'NONE', ( #8098 ), #65516, .F. ) ;
#30730 = AXIS2_PLACEMENT_3D ( 'NONE', #20018, #52755, #19685 ) ;
#30731 = DIRECTION ( 'NONE',  ( 0.000000000000000000, 1.000000000000000000, 0.000000000000000000 ) ) ;
#30732 = FACE_OUTER_BOUND ( 'NONE', #47752, .T. ) ;
#30733 = ORIENTED_EDGE ( 'NONE', *, *, #4335, .F. ) ;
#30734 = EDGE_CURVE ( 'NONE', #51601, #24199, #69273, .T. ) ;
#30735 = CARTESIAN_POINT ( 'NONE',  ( -81.89292637653382201, -8.102448949553172852, -5.886773742842741797 ) ) ;
#30736 = CONTEXT_DEPENDENT_SHAPE_REPRESENTATION ( #23972, #24391 ) ;
#30737 =( LENGTH_UNIT ( ) NAMED_UNIT ( * ) SI_UNIT ( .MILLI., .METRE. ) );
#30738 = DIRECTION ( 'NONE',  ( -0.000000000000000000, 0.000000000000000000, 1.000000000000000000 ) ) ;
#30739 = PRESENTATION_LAYER_ASSIGNMENT (  '', '', ( #16174 ) ) ;
#30740 = EDGE_CURVE ( 'NONE', #57872, #7256, #8787, .T. ) ;
#30741 = PRESENTATION_STYLE_ASSIGNMENT (( #57489 ) ) ;
#30742 = SURFACE_SIDE_STYLE ('',( #4333 ) ) ;
#30743 = AXIS2_PLACEMENT_3D ( 'NONE', #7816, #8867, #41259 ) ;
#30744 = ORIENTED_EDGE ( 'NONE', *, *, #2293, .T. ) ;
#30745 = CARTESIAN_POINT ( 'NONE',  ( 4.041451884327376121, 7.000000000000007105, 1.082903768654759569 ) ) ;
#30746 = FILL_AREA_STYLE ('',( #62751 ) ) ;
#30747 = VERTEX_POINT ( 'NONE', #68580 ) ;
#30748 = CARTESIAN_POINT ( 'NONE',  ( 6.667623377008403018, -2.231456886122029193, 6.451337545287477937 ) ) ;
#30749 = AXIS2_PLACEMENT_3D ( 'NONE', #68107, #51920, #3676 ) ;
#30750 = DIRECTION ( 'NONE',  ( -1.000000000000000000, 0.000000000000000000, 0.000000000000000000 ) ) ;
#30751 = CARTESIAN_POINT ( 'NONE',  ( -7.632228543268607446, 130.6570736234661467, -2.479861379858953718 ) ) ;
#30752 = SURFACE_STYLE_USAGE ( .BOTH. , #51892 ) ;
#30753 = VERTEX_POINT ( 'NONE', #63637 ) ;
#30754 = DIRECTION ( 'NONE',  ( 0.000000000000000000, 0.000000000000000000, 1.000000000000000000 ) ) ;
#30755 = CARTESIAN_POINT ( 'NONE',  ( -103.1049999999999756, -6.826472737025113702, 4.959722759717902107 ) ) ;
#30756 = CIRCLE ( 'NONE', #66729, 4.999999999999999112 ) ;
#30757 = UNCERTAINTY_MEASURE_WITH_UNIT (LENGTH_MEASURE( 1.000000000000000082E-05 ), #51067, 'distance_accuracy_value', 'NONE');
#30758 = FACE_OUTER_BOUND ( 'NONE', #6526, .T. ) ;
#30759 = ORIENTED_EDGE ( 'NONE', *, *, #16800, .T. ) ;
#30760 = COLOUR_RGB ( '', 0.08235294, 0.09019608, 0.10196078) ;
#30761 = CARTESIAN_POINT ( 'NONE',  ( 4.000000000000002665, 38.00000000000000711, -90.00000000000000000 ) ) ;
#30762 = AXIS2_PLACEMENT_3D ( 'NONE', #15392, #17712, #44134 ) ;
#30763 = CARTESIAN_POINT ( 'NONE',  ( -104.7570736234661695, -5.598654528085801552, 7.705886871421367523 ) ) ;
#30764 =( LENGTH_UNIT ( ) NAMED_UNIT ( * ) SI_UNIT ( .MILLI., .METRE. ) );
#30765 = CARTESIAN_POINT ( 'NONE',  ( -59.35479220832651492, -7.603157425156885196, -0.1359663579351287899 ) ) ;
#30766 = VERTEX_POINT ( 'NONE', #3458 ) ;
#30767 = COLOUR_RGB ( '', 0.66274510, 0.83137255, 0.94901961) ;
#30768 = FILL_AREA_STYLE_COLOUR ( '', #3600 ) ;
#30769 = CARTESIAN_POINT ( 'NONE',  ( -67.94499999999999318, -9.827790563157499189E-16, -8.024999999999991473 ) ) ;
#30770 = ORIENTED_EDGE ( 'NONE', *, *, #58684, .F. ) ;
#30771 = CARTESIAN_POINT ( 'NONE',  ( 0.000000000000000000, 0.000000000000000000, 32.50000000000000000 ) ) ;
#30772 = EDGE_CURVE ( 'NONE', #10461, #69624, #10180, .T. ) ;
#30773 = CIRCLE ( 'NONE', #56595, 0.5000000000000004441 ) ;
#30774 = STYLED_ITEM ( 'NONE', ( #10036 ), #7361 ) ;
#30775 = EDGE_LOOP ( 'NONE', ( #58713, #59540, #13627, #60051 ) ) ;
#30776 = DIRECTION ( 'NONE',  ( 0.000000000000000000, 0.000000000000000000, -1.000000000000000000 ) ) ;
#30777 =( NAMED_UNIT ( * ) SI_UNIT ( $, .STERADIAN. ) SOLID_ANGLE_UNIT ( ) );
#30778 = COLOUR_RGB ( '', 0.66274510, 0.83137255, 0.94901961) ;
#30779 = SURFACE_STYLE_USAGE ( .BOTH. , #67737 ) ;
#30780 = ORIENTED_EDGE ( 'NONE', *, *, #7480, .F. ) ;
#30781 = FACE_OUTER_BOUND ( 'NONE', #58039, .T. ) ;
#30782 = ORIENTED_EDGE ( 'NONE', *, *, #24450, .T. ) ;
#30783 = CARTESIAN_POINT ( 'NONE',  ( -71.62068965517238439, 63.58603185604027885, -7.000000000000000000 ) ) ;
#30784 = CARTESIAN_POINT ( 'NONE',  ( 48.00000000000000000, 99.99999999999992895, 7.500000000000000000 ) ) ;
#30785 = TOROIDAL_SURFACE ( 'NONE', #3802, 9.525000000000000355, 1.000000000000000888 ) ;
#30786 = AXIS2_PLACEMENT_3D ( 'NONE', #4084, #68847, #30479 ) ;
#30787 = CARTESIAN_POINT ( 'NONE',  ( -172.8570736234661922, -5.598654528085803328, -7.705886871421366635 ) ) ;
#30788 = CARTESIAN_POINT ( 'NONE',  ( 5.598654528085805993, 126.2449999999999903, 7.705886871421374629 ) ) ;
#30789 = CARTESIAN_POINT ( 'NONE',  ( -107.6070736234661638, -8.102448949553172852, 5.886773742842742685 ) ) ;
#30790 = CARTESIAN_POINT ( 'NONE',  ( 6.826472737025119919, 112.8929263765338078, 4.959722759717908325 ) ) ;
#30791 = CARTESIAN_POINT ( 'NONE',  ( -71.50000000000000000, 35.92875272052971525, -7.500000000000000000 ) ) ;
#30792 = ORIENTED_EDGE ( 'NONE', *, *, #62562, .F. ) ;
#30793 = DIRECTION ( 'NONE',  ( -1.000000000000000000, -0.000000000000000000, -0.000000000000000000 ) ) ;
#30794 = CARTESIAN_POINT ( 'NONE',  ( 45.00000000000000000, -1.469576158976824618E-14, 6.999999999999999112 ) ) ;
#30795 = DIRECTION ( 'NONE',  ( 0.000000000000000000, 0.000000000000000000, 1.000000000000000000 ) ) ;
#30796 = SURFACE_STYLE_USAGE ( .BOTH. , #19556 ) ;
#30797 = AXIS2_PLACEMENT_3D ( 'NONE', #24589, #51703, #67176 ) ;
#30798 = CARTESIAN_POINT ( 'NONE',  ( -149.7549999999999955, 4.716976649647091513, -6.492361379858946790 ) ) ;
#30799 = EDGE_CURVE ( 'NONE', #57684, #19536, #11587, .T. ) ;
#30800 = CARTESIAN_POINT ( 'NONE',  ( -75.00000000000000000, 8.749900610107138377, 6.882725987574753290 ) ) ;
#30801 = DIRECTION ( 'NONE',  ( 0.000000000000000000, 0.000000000000000000, -1.000000000000000000 ) ) ;
#30802 = CARTESIAN_POINT ( 'NONE',  ( -159.5949999999999989, 2.607480562269073321, 8.024999999999991473 ) ) ;
#30803 = AXIS2_PLACEMENT_3D ( 'NONE', #60174, #48977, #58797 ) ;
#30804 = CARTESIAN_POINT ( 'NONE',  ( -147.2949999999999875, -2.607480562269069768, 8.024999999999991473 ) ) ;
#30805 = EDGE_LOOP ( 'NONE', ( #55091, #16114, #6367, #56969 ) ) ;
#30806 = VECTOR ( 'NONE', #35221, 1000.000000000000000 ) ;
#30807 = EDGE_CURVE ( 'NONE', #53177, #4250, #68906, .T. ) ;
#30808 = DIRECTION ( 'NONE',  ( -0.7833176619561811327, 0.6216216216216278179, -0.000000000000000000 ) ) ;
#30809 = CARTESIAN_POINT ( 'NONE',  ( 26.00000000000001776, -3.148064030671221758, -29.68999999999999417 ) ) ;
#30810 = CARTESIAN_POINT ( 'NONE',  ( 22.25000000000000711, 33.74999999999999289, -4.000000000000000000 ) ) ;
#30811 = CIRCLE ( 'NONE', #36496, 1.499999999999997780 ) ;
#30812 = CARTESIAN_POINT ( 'NONE',  ( -61.85499999999998266, 4.716976649647094177, 6.492361379858945902 ) ) ;
#30813 = CARTESIAN_POINT ( 'NONE',  ( -39.62710692636852627, -13.39358289589475071, 2.720715303612538882 ) ) ;
#30814 = SURFACE_SIDE_STYLE ('',( #59531 ) ) ;
#30815 = CIRCLE ( 'NONE', #36500, 0.5000000000000004441 ) ;
#30816 = CARTESIAN_POINT ( 'NONE',  ( -59.69499999999998607, -8.437984349512086979, 5.166775262442717831E-16 ) ) ;
#30817 = CARTESIAN_POINT ( 'NONE',  ( -3.094860106618432471, 152.7049999999999841, -9.525000000000000355 ) ) ;
#30818 = DIRECTION ( 'NONE',  ( 0.000000000000000000, 0.000000000000000000, -1.000000000000000000 ) ) ;
#30819 = ADVANCED_FACE ( 'NONE', ( #9842 ), #66677, .F. ) ;
#30820 = PRESENTATION_STYLE_ASSIGNMENT (( #37555 ) ) ;
#30821 = STYLED_ITEM ( 'NONE', ( #11955 ), #27320 ) ;
#30822 = CONICAL_SURFACE ( 'NONE', #445, 4.499999999999976019, 0.7853981633974412846 ) ;
#30823 = ADVANCED_FACE ( 'NONE', ( #31254 ), #52754, .T. ) ;
#30824 = CARTESIAN_POINT ( 'NONE',  ( -177.5929263765339101, -3.094860106619935269, -9.524999999998900790 ) ) ;
#30825 = COLOUR_RGB ( '', 0.09019608, 0.27058824, 0.51372549) ;
#30826 = DIRECTION ( 'NONE',  ( 0.000000000000000000, -0.9944852160011111719, 0.1048768571002353378 ) ) ;
#30827 =( NAMED_UNIT ( * ) SI_UNIT ( $, .STERADIAN. ) SOLID_ANGLE_UNIT ( ) );
#30828 = DIRECTION ( 'NONE',  ( 1.000000000000000000, 0.000000000000000000, -0.000000000000000000 ) ) ;
#30829 = ORIENTED_EDGE ( 'NONE', *, *, #41274, .F. ) ;
#30831 = ORIENTED_EDGE ( 'NONE', *, *, #68089, .T. ) ;
#30830 = AXIS2_PLACEMENT_3D ( 'NONE', #25313, #9156, #68240 ) ;
#30832 = AXIS2_PLACEMENT_3D ( 'NONE', #9694, #41015, #56824 ) ;
#30833 = CARTESIAN_POINT ( 'NONE',  ( -1.387778780781445676E-14, 17.78868675966041835, 1.540743955509788682E-30 ) ) ;
#30834 = CARTESIAN_POINT ( 'NONE',  ( 17.75000000000000711, 30.74999999999999289, -3.750000000000000000 ) ) ;
#30835 = CARTESIAN_POINT ( 'NONE',  ( -20.55652580482692926, 114.6393193824117844, 10.28299520148690682 ) ) ;
#30836 = CARTESIAN_POINT ( 'NONE',  ( 23.50000000000041211, 24.55989583709592949, -27.18999999999997286 ) ) ;
#30837 = STYLED_ITEM ( 'NONE', ( #47914 ), #1993 ) ;
#30838 = SURFACE_STYLE_USAGE ( .BOTH. , #35784 ) ;
#30839 = EDGE_LOOP ( 'NONE', ( #60500, #61904, #57847, #12236 ) ) ;
#30840 = VERTEX_POINT ( 'NONE', #53099 ) ;
#30841 = LINE ( 'NONE', #31175, #48921 ) ;
#30842 = FACE_OUTER_BOUND ( 'NONE', #49807, .T. ) ;
#30843 = CARTESIAN_POINT ( 'NONE',  ( 74.50000000000000000, 3.473944261090200865E-15, -10.00000000000000000 ) ) ;
#30844 = EDGE_LOOP ( 'NONE', ( #33194, #25527, #65010 ) ) ;
#30845 = CARTESIAN_POINT ( 'NONE',  ( 3.094860106618435136, 116.4049999999999869, -9.525000000000000355 ) ) ;
#30846 = DIRECTION ( 'NONE',  ( -1.982541115402068561E-16, 0.000000000000000000, 1.000000000000000000 ) ) ;
#30847 = EDGE_LOOP ( 'NONE', ( #15483, #18393, #28575 ) ) ;
#30848 = MECHANICAL_DESIGN_GEOMETRIC_PRESENTATION_REPRESENTATION (  '', ( #15028 ), #64406 ) ;
#30849 = CYLINDRICAL_SURFACE ( 'NONE', #9233, 23.00000000000000000 ) ;
#30850 = CARTESIAN_POINT ( 'NONE',  ( -99.29499999999997328, -2.607480562269069768, 8.024999999999991473 ) ) ;
#30851 = ORIENTED_EDGE ( 'NONE', *, *, #7635, .T. ) ;
#30852 = CYLINDRICAL_SURFACE ( 'NONE', #62039, 1.000000000000000888 ) ;
#30853 = EDGE_CURVE ( 'NONE', #15864, #62763, #52092, .T. ) ;
#30854 = CARTESIAN_POINT ( 'NONE',  ( -46.54801840586653583, 4.937396119256769467, -6.795742752749552196 ) ) ;
#30855 = SPHERICAL_SURFACE ( 'NONE', #26246, 0.2500000000000000000 ) ;
#30856 = AXIS2_PLACEMENT_3D ( 'NONE', #8687, #25534, #13958 ) ;
#30857 = ORIENTED_EDGE ( 'NONE', *, *, #37615, .T. ) ;
#30858 = CARTESIAN_POINT ( 'NONE',  ( 8.437984349512095861, 158.1929263765337623, 1.550032578732817026E-15 ) ) ;
#30859 =( BOUNDED_CURVE ( )  B_SPLINE_CURVE ( 2, ( #25628, #68569, #63628, #67519, #10170, #31609, #46098, #19319, #20365, #62237, #63285 ),
 .UNSPECIFIED., .F., .F. ) 
 B_SPLINE_CURVE_WITH_KNOTS ( ( 3, 2, 2, 2, 2, 3 ),
 ( 0.3804347826086865170, 0.3826086956521647098, 0.3847826086956429026, 0.3869565217391210954, 0.3891304347825992882, 0.3913043478260775365 ),
 .UNSPECIFIED. ) 
 CURVE ( )  GEOMETRIC_REPRESENTATION_ITEM ( )  RATIONAL_B_SPLINE_CURVE ( ( 1.000000000000206279, 0.9510565162949473628, 1.000000000000000000, 0.9510565162951535312, 1.000000000000000000, 0.9510565162951535312, 1.000000000000000000, 0.9510565162951535312, 1.000000000000000000, 0.9510565162953660279, 0.9999999999997875033 ) ) 
 REPRESENTATION_ITEM ( '' )  );
#30860 = ADVANCED_FACE ( 'NONE', ( #67893 ), #15818, .F. ) ;
#30861 = CARTESIAN_POINT ( 'NONE',  ( -74.50000000000000000, -2.208799022165584366E-14, 9.500000000000000000 ) ) ;
#30862 = DIRECTION ( 'NONE',  ( -1.000000000000000000, -0.000000000000000000, -0.000000000000000000 ) ) ;
#30863 = EDGE_LOOP ( 'NONE', ( #46503, #8424, #61078, #2963 ) ) ;
#30864 = CARTESIAN_POINT ( 'NONE',  ( 0.000000000000000000, 154.9999999999999716, -23.00000000000000000 ) ) ;
#30865 = VERTEX_POINT ( 'NONE', #37988 ) ;
#30866 = SURFACE_STYLE_USAGE ( .BOTH. , #9436 ) ;
#30867 = FILL_AREA_STYLE ('',( #21018 ) ) ;
#30868 = SURFACE_SIDE_STYLE ('',( #64265 ) ) ;
#30869 = CARTESIAN_POINT ( 'NONE',  ( -127.4049999999999869, -2.607480562269069768, 8.024999999999991473 ) ) ;
#30870 = CARTESIAN_POINT ( 'NONE',  ( -183.9999999999999147, -5.631006485181712762, 5.770458336139917321 ) ) ;
#30871 = DIRECTION ( 'NONE',  ( 0.000000000000000000, 0.000000000000000000, -1.000000000000000000 ) ) ;
#30872 = AXIS2_PLACEMENT_3D ( 'NONE', #31381, #57803, #26110 ) ;
#30873 = VECTOR ( 'NONE', #31414, 1000.000000000000000 ) ;
#30874 = CARTESIAN_POINT ( 'NONE',  ( -125.5429263765337993, 9.058813317711329915, 2.943386871421369566 ) ) ;
#30875 = DIRECTION ( 'NONE',  ( -1.000000000000000000, 0.000000000000000000, 0.000000000000000000 ) ) ;
#30876 = DIRECTION ( 'NONE',  ( 0.000000000000000000, 1.000000000000000000, 0.000000000000000000 ) ) ;
#30877 = ORIENTED_EDGE ( 'NONE', *, *, #6111, .F. ) ;
#30878 = VERTEX_POINT ( 'NONE', #28038 ) ;
#30879 = DIRECTION ( 'NONE',  ( 0.000000000000000000, 0.000000000000000000, -1.000000000000000000 ) ) ;
#30880 = ADVANCED_FACE ( 'NONE', ( #59367 ), #22456, .T. ) ;
#30881 = EDGE_LOOP ( 'NONE', ( #67063, #28061, #23686 ) ) ;
#30882 = CARTESIAN_POINT ( 'NONE',  ( -154.7929263765341830, -3.094860106612178363, 9.525000000004535394 ) ) ;
#30883 = CARTESIAN_POINT ( 'NONE',  ( -174.5049999999999955, -6.826472737025115478, -4.959722759717899443 ) ) ;
#30884 = ADVANCED_FACE ( 'NONE', ( #22811 ), #48192, .F. ) ;
#30885 = DIRECTION ( 'NONE',  ( -1.000000000000000000, 0.000000000000000000, 0.000000000000000000 ) ) ;
#30886 = CARTESIAN_POINT ( 'NONE',  ( -47.15707362346616094, -9.058813317711329915, -2.943386871421370898 ) ) ;
#30887 = AXIS2_PLACEMENT_3D ( 'NONE', #23837, #66758, #18576 ) ;
#30888 = VECTOR ( 'NONE', #61451, 1000.000000000000000 ) ;
#30889 = CARTESIAN_POINT ( 'NONE',  ( -174.4449999999999932, 0.000000000000000000, 8.024999999999991473 ) ) ;
#30890 = CARTESIAN_POINT ( 'NONE',  ( -17.41962728626436530, -0.1139526552317604857, 12.50000000000000000 ) ) ;
#30891 = ORIENTED_EDGE ( 'NONE', *, *, #42173, .T. ) ;
#30892 = CARTESIAN_POINT ( 'NONE',  ( 8.246138225238285102, 3.717269627651449415, -3.339003878076450753E-15 ) ) ;
#30893 = EDGE_CURVE ( 'NONE', #49467, #14037, #1277, .T. ) ;
#30894 = CARTESIAN_POINT ( 'NONE',  ( -11.94499203678653032, 11.32543297781502289, -3.971327892791007841 ) ) ;
#30895 = CARTESIAN_POINT ( 'NONE',  ( -92.60500000000000398, 6.826472737025113702, -4.959722759717902107 ) ) ;
#30896 =( NAMED_UNIT ( * ) PLANE_ANGLE_UNIT ( ) SI_UNIT ( $, .RADIAN. ) );
#30897 = CARTESIAN_POINT ( 'NONE',  ( -74.82043395980159062, 36.18002821201687169, -9.907562454915460393 ) ) ;
#30898 = EDGE_CURVE ( 'NONE', #53938, #30278, #48890, .T. ) ;
#30899 = CARTESIAN_POINT ( 'NONE',  ( -85.79499999999997328, 2.607480562269069324, -8.024999999999993250 ) ) ;
#30900 = CARTESIAN_POINT ( 'NONE',  ( -1.166476076187854022E-15, 130.0549999999999784, 9.525000000000000355 ) ) ;
#30901 = CARTESIAN_POINT ( 'NONE',  ( -72.89499999999999602, 6.826472737025116366, 4.959722759717898555 ) ) ;
#30902 = CARTESIAN_POINT ( 'NONE',  ( 8.000000000000035527, 0.000000000000000000, -77.00402776293825013 ) ) ;
#30903 = MECHANICAL_DESIGN_GEOMETRIC_PRESENTATION_REPRESENTATION (  '', ( #35439 ), #47857 ) ;
#30904 = ADVANCED_FACE ( 'NONE', ( #16177 ), #65710, .T. ) ;
#30905 = DIRECTION ( 'NONE',  ( 0.000000000000000000, 1.000000000000000000, -0.000000000000000000 ) ) ;
#30906 = DIRECTION ( 'NONE',  ( 0.000000000000000000, 0.000000000000000000, 1.000000000000000000 ) ) ;
#30907 = PRESENTATION_LAYER_ASSIGNMENT (  '', '', ( #61249 ) ) ;
#30908 = CARTESIAN_POINT ( 'NONE',  ( 0.000000000000000000, 0.000000000000000000, 52.50000000000000000 ) ) ;
#30909 = PRESENTATION_STYLE_ASSIGNMENT (( #29877 ) ) ;
#30910 = EDGE_LOOP ( 'NONE', ( #18888, #35529, #3950, #42574 ) ) ;
#30911 = CARTESIAN_POINT ( 'NONE',  ( -107.6929263765338050, 10.01517768586948698, -1.839758294383808571E-15 ) ) ;
#30912 = ADVANCED_FACE ( 'NONE', ( #31967 ), #37300, .T. ) ;
#30913 = CARTESIAN_POINT ( 'NONE',  ( -132.7450000000000045, 4.716976649647094177, 6.492361379858945902 ) ) ;
#30914 = B_SPLINE_CURVE_WITH_KNOTS ( 'NONE', 3,
 ( #308, #64748, #16589, #27765, #17938, #12648, #11965, #12999 ),
 .UNSPECIFIED., .F., .F.,
 ( 4, 2, 2, 4 ),
 ( 2.544316211733585141E-07, 0.002094919859796805575, 0.003142252573884622441, 0.004189585287972440175 ),
 .UNSPECIFIED. ) ;
#30916 = DIRECTION ( 'NONE',  ( -0.000000000000000000, -0.000000000000000000, 1.000000000000000000 ) ) ;
#30915 = CARTESIAN_POINT ( 'NONE',  ( 4.716976649647099507, 135.7570736234661695, -6.492361379858953008 ) ) ;
#30917 = FILL_AREA_STYLE_COLOUR ( '', #19284 ) ;
#30918 = ORIENTED_EDGE ( 'NONE', *, *, #5312, .F. ) ;
#30919 = ORIENTED_EDGE ( 'NONE', *, *, #49800, .T. ) ;
#30920 = DIRECTION ( 'NONE',  ( 0.000000000000000000, 0.000000000000000000, 1.000000000000000000 ) ) ;
#30921 = DIRECTION ( 'NONE',  ( 0.000000000000000000, -1.000000000000000000, 0.000000000000000000 ) ) ;
#30922 =( GEOMETRIC_REPRESENTATION_CONTEXT ( 3 ) GLOBAL_UNCERTAINTY_ASSIGNED_CONTEXT ( ( #9613 ) ) GLOBAL_UNIT_ASSIGNED_CONTEXT ( ( #60216, #61252, #44772 ) ) REPRESENTATION_CONTEXT ( 'NONE', 'WORKASPACE' ) );
#30923 = MECHANICAL_DESIGN_GEOMETRIC_PRESENTATION_REPRESENTATION (  '', ( #50041 ), #57918 ) ;
#30924 = CARTESIAN_POINT ( 'NONE',  ( -97.55707362346618083, -1.166476076187852838E-15, -9.524999999999991473 ) ) ;
#30925 = DIRECTION ( 'NONE',  ( -0.000000000000000000, -0.000000000000000000, 1.000000000000000000 ) ) ;
#30926 = CARTESIAN_POINT ( 'NONE',  ( -9.568252947146932641, -1.861307952554191347, 1.427299755870870435 ) ) ;
#30927 = EDGE_LOOP ( 'NONE', ( #66166, #17821, #47780, #6320 ) ) ;
#30928 = CARTESIAN_POINT ( 'NONE',  ( -118.4049999999999869, -2.607480562269069768, 8.024999999999991473 ) ) ;
#30929 = ORIENTED_EDGE ( 'NONE', *, *, #27537, .T. ) ;
#30930 = CARTESIAN_POINT ( 'NONE',  ( -124.5570736234661808, -1.166476076187852838E-15, -9.524999999999991473 ) ) ;
#30931 = ORIENTED_EDGE ( 'NONE', *, *, #36279, .F. ) ;
#30932 = LINE ( 'NONE', #36952, #66162 ) ;
#30933 = LINE ( 'NONE', #41885, #57991 ) ;
#30934 = ORIENTED_EDGE ( 'NONE', *, *, #49266, .T. ) ;
#30935 = AXIS2_PLACEMENT_3D ( 'NONE', #38945, #6518, #65284 ) ;
#30936 = MECHANICAL_DESIGN_GEOMETRIC_PRESENTATION_REPRESENTATION (  '', ( #56770 ), #41071 ) ;
#30937 = FILL_AREA_STYLE ('',( #51365 ) ) ;
#30938 = CARTESIAN_POINT ( 'NONE',  ( 9.058813317711337021, 153.5449999999999875, 2.943386871421375783 ) ) ;
#30939 = CARTESIAN_POINT ( 'NONE',  ( -15.75000000000000000, -3.000000000000000000, 18.00000000000000000 ) ) ;
#30940 = ADVANCED_FACE ( 'NONE', ( #37653 ), #59049, .F. ) ;
#30941 = ORIENTED_EDGE ( 'NONE', *, *, #18435, .F. ) ;
#30942 = CARTESIAN_POINT ( 'NONE',  ( 9.058813317711338797, 148.9550000000000125, -2.943386871421372675 ) ) ;
#30943 = SURFACE_SIDE_STYLE ('',( #64345 ) ) ;
#30944 = FILL_AREA_STYLE ('',( #57695 ) ) ;
#30945 = ORIENTED_EDGE ( 'NONE', *, *, #31340, .F. ) ;
#30946 = CARTESIAN_POINT ( 'NONE',  ( 0.000000000000000000, 125.9429263765338192, -8.025000000000000355 ) ) ;
#30947 = DIRECTION ( 'NONE',  ( -0.000000000000000000, -0.000000000000000000, -1.000000000000000000 ) ) ;
#30948 = DIRECTION ( 'NONE',  ( 0.000000000000000000, 0.000000000000000000, -1.000000000000000000 ) ) ;
#30949 = DIRECTION ( 'NONE',  ( 0.000000000000000000, 0.000000000000000000, -1.000000000000000000 ) ) ;
#30950 = AXIS2_PLACEMENT_3D ( 'NONE', #36262, #245, #4177 ) ;
#30951 = CARTESIAN_POINT ( 'NONE',  ( -34.99999999999999289, 99.99999999999998579, -3.500000000000000000 ) ) ;
#30952 = ORIENTED_EDGE ( 'NONE', *, *, #26819, .F. ) ;
#30953 = CARTESIAN_POINT ( 'NONE',  ( 41.05151532188900632, 107.6719357445258538, 3.224518739502659770 ) ) ;
#30954 = VERTEX_POINT ( 'NONE', #5558 ) ;
#30955 = CARTESIAN_POINT ( 'NONE',  ( -60.14292637653380069, 5.598654528085800663, -7.705886871421367523 ) ) ;
#30956 =( NAMED_UNIT ( * ) SI_UNIT ( $, .STERADIAN. ) SOLID_ANGLE_UNIT ( ) );
#30957 = LINE ( 'NONE', #47193, #52028 ) ;
#30958 = CARTESIAN_POINT ( 'NONE',  ( -149.0049999999999386, 6.826472737025116366, 4.959722759717898555 ) ) ;
#30959 = ORIENTED_EDGE ( 'NONE', *, *, #9728, .T. ) ;
#30960 = PRESENTATION_STYLE_ASSIGNMENT (( #9544 ) ) ;
#30961 = CIRCLE ( 'NONE', #36601, 5.499999999999976907 ) ;
#30962 = EDGE_CURVE ( 'NONE', #44609, #30484, #34393, .T. ) ;
#30963 = DIRECTION ( 'NONE',  ( 1.000000000000000000, -0.000000000000000000, 0.000000000000000000 ) ) ;
#30964 = CARTESIAN_POINT ( 'NONE',  ( 1.224646799147353256E-15, 2.299999999999999822, 10.00000000000000000 ) ) ;
#30965 = CARTESIAN_POINT ( 'NONE',  ( -70.19292637653380496, -10.01517768586948698, 6.132527647946031529E-16 ) ) ;
#30966 = CARTESIAN_POINT ( 'NONE',  ( 6.826472737025121695, 146.4929263765338305, -4.959722759717905660 ) ) ;
#30967 = ORIENTED_EDGE ( 'NONE', *, *, #22798, .T. ) ;
#30968 = ORIENTED_EDGE ( 'NONE', *, *, #6575, .T. ) ;
#30969 = CARTESIAN_POINT ( 'NONE',  ( 22.64869388986209486, 27.05257840322770591, 27.33874645186988417 ) ) ;
#30970 = SURFACE_SIDE_STYLE ('',( #67580 ) ) ;
#30971 = EDGE_CURVE ( 'NONE', #58002, #55641, #45340, .T. ) ;
#30972 = CARTESIAN_POINT ( 'NONE',  ( -69.35499999999998977, -4.716976649647093289, -6.492361379858945902 ) ) ;
#30973 = ORIENTED_EDGE ( 'NONE', *, *, #39165, .T. ) ;
#30974 = CARTESIAN_POINT ( 'NONE',  ( 12.75000000000000533, 27.74999999999998224, 4.000000000000000000 ) ) ;
#30975 = EDGE_CURVE ( 'NONE', #33218, #4344, #64568, .T. ) ;
#30976 = PRESENTATION_STYLE_ASSIGNMENT (( #30264 ) ) ;
#30977 = CARTESIAN_POINT ( 'NONE',  ( -90.20707362346733760, 3.094860106637524755, 9.524999999986121679 ) ) ;
#30978 = DIRECTION ( 'NONE',  ( 0.000000000000000000, 0.000000000000000000, 1.000000000000000000 ) ) ;
#30979 = ORIENTED_EDGE ( 'NONE', *, *, #39590, .F. ) ;
#30980 = EDGE_CURVE ( 'NONE', #56480, #30491, #7494, .T. ) ;
#30981 = CARTESIAN_POINT ( 'NONE',  ( -74.11218598454972550, 9.325134922070571264, -6.185423913763112402 ) ) ;
#30982 = CARTESIAN_POINT ( 'NONE',  ( 3.999798566743343109, 50.36012635523414360, -7.189099757012595404 ) ) ;
#30983 = DIRECTION ( 'NONE',  ( -1.000000000000000000, -0.000000000000000000, -0.000000000000000000 ) ) ;
#30985 = FILL_AREA_STYLE ('',( #13415 ) ) ;
#30984 = PRESENTATION_STYLE_ASSIGNMENT (( #66909 ) ) ;
#30986 = ADVANCED_FACE ( 'NONE', ( #60413 ), #49814, .T. ) ;
#30987 = AXIS2_PLACEMENT_3D ( 'NONE', #26064, #20452, #15894 ) ;
#30988 = CARTESIAN_POINT ( 'NONE',  ( -8.102448949553181734, 149.4949999999999761, 5.886773742842747126 ) ) ;
#30989 = CARTESIAN_POINT ( 'NONE',  ( -100.4949999999999761, 6.826472737025113702, -4.959722759717902107 ) ) ;
#30990 = DIRECTION ( 'NONE',  ( 1.000000000000000000, 0.000000000000000000, 0.000000000000000000 ) ) ;
#30991 = VECTOR ( 'NONE', #64523, 1000.000000000000000 ) ;
#30992 = PRESENTATION_LAYER_ASSIGNMENT (  '', '', ( #29833 ) ) ;
#30993 =( BOUNDED_CURVE ( )  B_SPLINE_CURVE ( 2, ( #1110, #12415, #49386, #33543, #44833, #28593, #54297, #33876, #17050, #27551, #38532 ),
 .UNSPECIFIED., .F., .F. ) 
 B_SPLINE_CURVE_WITH_KNOTS ( ( 3, 2, 2, 2, 2, 3 ),
 ( 0.1086956521739105563, 0.1108695652173887630, 0.1130434782608669697, 0.1152173913043451903, 0.1173913043478233970, 0.1195652173913016036 ),
 .UNSPECIFIED. ) 
 CURVE ( )  GEOMETRIC_REPRESENTATION_ITEM ( )  RATIONAL_B_SPLINE_CURVE ( ( 1.000000000000055955, 0.9510565162950975759, 1.000000000000000000, 0.9510565162951535312, 1.000000000000000000, 0.9510565162951535312, 1.000000000000000000, 0.9510565162951535312, 1.000000000000000000, 0.9510565162952153706, 0.9999999999999381606 ) ) 
 REPRESENTATION_ITEM ( '' )  );
#30994 = CARTESIAN_POINT ( 'NONE',  ( 0.000000000000000000, 0.000000000000000000, 1.000000000000000000 ) ) ;
#30995 = VERTEX_POINT ( 'NONE', #23157 ) ;
#30996 = CARTESIAN_POINT ( 'NONE',  ( -130.4929263765338021, -8.102448949553172852, 5.886773742842742685 ) ) ;
#30997 =( LENGTH_UNIT ( ) NAMED_UNIT ( * ) SI_UNIT ( .MILLI., .METRE. ) );
#30998 = CARTESIAN_POINT ( 'NONE',  ( -153.2949999999999875, -2.607480562269069768, 8.024999999999991473 ) ) ;
#30999 =( LENGTH_UNIT ( ) NAMED_UNIT ( * ) SI_UNIT ( .MILLI., .METRE. ) );
#31000 = EDGE_CURVE ( 'NONE', #2274, #37986, #29615, .T. ) ;
#31001 = DIRECTION ( 'NONE',  ( 0.000000000000000000, 0.000000000000000000, -1.000000000000000000 ) ) ;
#31002 = COLOUR_RGB ( '', 0.40784314, 0.44705882, 0.49803922) ;
#31003 = PRESENTATION_STYLE_ASSIGNMENT (( #68308 ) ) ;
#31004 = EDGE_LOOP ( 'NONE', ( #42882, #55419, #67278 ) ) ;
#31005 = SURFACE_STYLE_FILL_AREA ( #41596 ) ;
#31006 = ORIENTED_EDGE ( 'NONE', *, *, #33980, .F. ) ;
#31007 = EDGE_CURVE ( 'NONE', #45578, #21243, #39697, .T. ) ;
#31008 = LINE ( 'NONE', #23238, #10586 ) ;
#31009 = CARTESIAN_POINT ( 'NONE',  ( -143.0929263765343364, 3.094860106627105090, 9.524999999993692512 ) ) ;
#31010 = CARTESIAN_POINT ( 'NONE',  ( -45.00000000000000000, 9.708372675170622301, 6.000000000000001776 ) ) ;
#31011 = DIRECTION ( 'NONE',  ( 1.000000000000000000, 0.000000000000000000, -1.300977106640434891E-16 ) ) ;
#31012 = CARTESIAN_POINT ( 'NONE',  ( -60.16623008473946044, -7.538574111777714748, -8.332478740366983261E-17 ) ) ;
#31013 = VERTEX_POINT ( 'NONE', #34043 ) ;
#31014 = CARTESIAN_POINT ( 'NONE',  ( -149.6049999999999898, 6.826472737025113702, -4.959722759717902107 ) ) ;
#31015 = ORIENTED_EDGE ( 'NONE', *, *, #53231, .T. ) ;
#31016 = SURFACE_SIDE_STYLE ('',( #47961 ) ) ;
#31017 = CARTESIAN_POINT ( 'NONE',  ( 13.75000000000000533, 30.74999999999999289, -4.000000000000000000 ) ) ;
#31018 = ORIENTED_EDGE ( 'NONE', *, *, #9466, .F. ) ;
#31019 = DIRECTION ( 'NONE',  ( 0.000000000000000000, -1.000000000000000000, 0.000000000000000000 ) ) ;
#31020 = DIRECTION ( 'NONE',  ( 0.000000000000000000, 0.000000000000000000, -1.000000000000000000 ) ) ;
#31021 = CARTESIAN_POINT ( 'NONE',  ( 0.000000000000000000, 124.4449999999999932, -9.525000000000000355 ) ) ;
#31022 = VECTOR ( 'NONE', #19925, 1000.000000000000000 ) ;
#31023 = ORIENTED_EDGE ( 'NONE', *, *, #7488, .T. ) ;
#31024 = CARTESIAN_POINT ( 'NONE',  ( 22.99999999999998934, 5.000000000000000000, 37.00402776293825724 ) ) ;
#31025 = CARTESIAN_POINT ( 'NONE',  ( 9.058813317711337021, 124.6549999999999869, 2.943386871421375783 ) ) ;
#31026 = CARTESIAN_POINT ( 'NONE',  ( -68.90499999999998693, 2.607480562269069324, -8.024999999999993250 ) ) ;
#31027 = CARTESIAN_POINT ( 'NONE',  ( -5.000000000000000000, 0.000000000000000000, 42.50000000000000000 ) ) ;
#31028 = ORIENTED_EDGE ( 'NONE', *, *, #43266, .F. ) ;
#31029 = CARTESIAN_POINT ( 'NONE',  ( -9.058813317711338797, 135.4549999999999841, 2.943386871421373563 ) ) ;
#31030 = CARTESIAN_POINT ( 'NONE',  ( -195.0000000000000000, 0.000000000000000000, 0.000000000000000000 ) ) ;
#31031 = MECHANICAL_DESIGN_GEOMETRIC_PRESENTATION_REPRESENTATION (  '', ( #61355 ), #33303 ) ;
#31032 = FACE_OUTER_BOUND ( 'NONE', #51654, .T. ) ;
#31033 = COLOUR_RGB ( '', 0.31764706, 0.68627451, 0.89019608) ;
#31034 = ADVANCED_FACE ( 'NONE', ( #28751 ), #12735, .T. ) ;
#31035 = VECTOR ( 'NONE', #60876, 1000.000000000000000 ) ;
#31036 = ORIENTED_EDGE ( 'NONE', *, *, #14891, .F. ) ;
#31037 = DIRECTION ( 'NONE',  ( 0.000000000000000000, 0.000000000000000000, -1.000000000000000000 ) ) ;
#31038 = CARTESIAN_POINT ( 'NONE',  ( 0.000000000000000000, 124.0570736234661524, -8.025000000000000355 ) ) ;
#31039 = LINE ( 'NONE', #62686, #19407 ) ;
#31040 = CARTESIAN_POINT ( 'NONE',  ( -182.6049999999999613, 6.826472737025113702, -4.959722759717902107 ) ) ;
#31041 = ORIENTED_EDGE ( 'NONE', *, *, #66811, .T. ) ;
#31042 = CARTESIAN_POINT ( 'NONE',  ( 8.253986449296842665, 111.5397190885544347, -1.986321737243862406 ) ) ;
#31043 = ADVANCED_FACE ( 'NONE', ( #55498 ), #3907, .F. ) ;
#31044 = DIRECTION ( 'NONE',  ( -1.000000000000000000, 0.000000000000000000, 0.000000000000000000 ) ) ;
#31045 = ORIENTED_EDGE ( 'NONE', *, *, #965, .F. ) ;
#31046 = CYLINDRICAL_SURFACE ( 'NONE', #35415, 0.2500000000000002220 ) ;
#31047 = CARTESIAN_POINT ( 'NONE',  ( -184.0000000000000000, 0.000000000000000000, 0.000000000000000000 ) ) ;
#31048 = VERTEX_POINT ( 'NONE', #41960 ) ;
#31049 = DIRECTION ( 'NONE',  ( -0.000000000000000000, 1.000000000000000000, -0.000000000000000000 ) ) ;
#31051 = EDGE_CURVE ( 'NONE', #2414, #55582, #15223, .T. ) ;
#31050 = DIRECTION ( 'NONE',  ( 0.000000000000000000, 0.000000000000000000, 1.000000000000000000 ) ) ;
#31052 = CARTESIAN_POINT ( 'NONE',  ( -96.05499999999999261, -9.827790563157499189E-16, -8.024999999999991473 ) ) ;
#31053 = ORIENTED_EDGE ( 'NONE', *, *, #26374, .F. ) ;
#31054 = SURFACE_SIDE_STYLE ('',( #62380 ) ) ;
#31055 = CARTESIAN_POINT ( 'NONE',  ( 0.000000000000000000, 2.500000000000000000, 0.000000000000000000 ) ) ;
#31056 = CARTESIAN_POINT ( 'NONE',  ( -129.2070736234661581, 3.094860106618433360, 9.524999999999991473 ) ) ;
#31057 = CARTESIAN_POINT ( 'NONE',  ( 9.058813317711337021, 147.5449999999999875, 2.943386871421375783 ) ) ;
#31058 = CARTESIAN_POINT ( 'NONE',  ( -72.80707362346615241, 10.01517768586948698, -1.839758294383808571E-15 ) ) ;
#31059 = VERTEX_POINT ( 'NONE', #57756 ) ;
#31060 = DIRECTION ( 'NONE',  ( 0.000000000000000000, 0.000000000000000000, -1.000000000000000000 ) ) ;
#31061 = DIRECTION ( 'NONE',  ( 0.000000000000000000, 0.000000000000000000, 1.000000000000000000 ) ) ;
#31063 = CARTESIAN_POINT ( 'NONE',  ( -99.89292637653379359, -8.102448949553174629, -5.886773742842741797 ) ) ;
#31062 = CARTESIAN_POINT ( 'NONE',  ( -195.0000000000000000, 1.166476076187852838E-15, -9.524999999999991473 ) ) ;
#31064 = ADVANCED_FACE ( 'NONE', ( #53176 ), #46542, .T. ) ;
#31065 = CARTESIAN_POINT ( 'NONE',  ( -112.7049999999999699, 2.607480562269073321, 8.024999999999991473 ) ) ;
#31066 = DIRECTION ( 'NONE',  ( -0.000000000000000000, -1.000000000000000000, -0.000000000000000000 ) ) ;
#31067 = CARTESIAN_POINT ( 'NONE',  ( 8.102448949553183510, 123.9949999999999903, -5.886773742842746238 ) ) ;
#31068 = CARTESIAN_POINT ( 'NONE',  ( -129.2949999999999875, -2.607480562269069768, 8.024999999999991473 ) ) ;
#31069 = CARTESIAN_POINT ( 'NONE',  ( 8.000000000000035527, 0.000000000000000000, 77.00402776293825013 ) ) ;
#31070 = DIRECTION ( 'NONE',  ( 0.000000000000000000, 0.000000000000000000, 1.000000000000000000 ) ) ;
#31071 = DIRECTION ( 'NONE',  ( -1.000000000000000000, 0.000000000000000000, 0.000000000000000000 ) ) ;
#31072 = ORIENTED_EDGE ( 'NONE', *, *, #56238, .T. ) ;
#31073 = CARTESIAN_POINT ( 'NONE',  ( -4.041451884327381450, -7.000000000000002665, 7.500000000000000000 ) ) ;
#31074 = CARTESIAN_POINT ( 'NONE',  ( -166.1929263765337907, -10.01517768586948698, 6.132527647946031529E-16 ) ) ;
#31075 = CARTESIAN_POINT ( 'NONE',  ( 7.794228634059951588, -4.500000000000003553, 0.000000000000000000 ) ) ;
#31076 = VECTOR ( 'NONE', #26547, 1000.000000000000000 ) ;
#31077 = AXIS2_PLACEMENT_3D ( 'NONE', #9619, #52531, #31037 ) ;
#31078 = CARTESIAN_POINT ( 'NONE',  ( -3.000000000000000000, -3.499999999999999556, 24.00000000000000000 ) ) ;
#31079 = CYLINDRICAL_SURFACE ( 'NONE', #44, 3.100000000000003642 ) ;
#31080 = CARTESIAN_POINT ( 'NONE',  ( -54.23088132574830666, -9.395153247374610217, -2.525443637521251006 ) ) ;
#31081 =( NAMED_UNIT ( * ) PLANE_ANGLE_UNIT ( ) SI_UNIT ( $, .RADIAN. ) );
#31082 = ORIENTED_EDGE ( 'NONE', *, *, #32902, .T. ) ;
#31083 = CARTESIAN_POINT ( 'NONE',  ( -86.39292637653380780, 8.102448949553176405, 5.886773742842740909 ) ) ;
#31084 = ITEM_DEFINED_TRANSFORMATION ( 'NONE', 'NONE', #30360,  #42840 ) ;
#31085 = CARTESIAN_POINT ( 'NONE',  ( 44.99999999999998579, 119.9999999999999716, -10.00000000000000000 ) ) ;
#31086 = CARTESIAN_POINT ( 'NONE',  ( -165.7429263765338305, -5.598654528085803328, -7.705886871421366635 ) ) ;
#31087 = SURFACE_SIDE_STYLE ('',( #15639 ) ) ;
#31088 = DIRECTION ( 'NONE',  ( -0.000000000000000000, -1.000000000000000000, 0.000000000000000000 ) ) ;
#31089 = COLOUR_RGB ( '', 0.66274510, 0.83137255, 0.94901961) ;
#31090 = CARTESIAN_POINT ( 'NONE',  ( -176.0049999999999670, 6.826472737025115478, 4.959722759717899443 ) ) ;
#31091 = VERTEX_POINT ( 'NONE', #63012 ) ;
#31092 = CARTESIAN_POINT ( 'NONE',  ( 29.00000000000000000, 38.70020753820971748, -89.00000000000000000 ) ) ;
#31093 = FILL_AREA_STYLE ('',( #13531 ) ) ;
#31094 = ORIENTED_EDGE ( 'NONE', *, *, #8840, .T. ) ;
#31095 = CARTESIAN_POINT ( 'NONE',  ( -111.4429263765338050, -1.166476076187852838E-15, -9.524999999999991473 ) ) ;
#31096 = SURFACE_SIDE_STYLE ('',( #46655 ) ) ;
#31097 = CARTESIAN_POINT ( 'NONE',  ( 4.716976649647096842, 143.8570736234661638, 6.492361379858953896 ) ) ;
#31098 =( NAMED_UNIT ( * ) PLANE_ANGLE_UNIT ( ) SI_UNIT ( $, .RADIAN. ) );
#31099 = ORIENTED_EDGE ( 'NONE', *, *, #56202, .F. ) ;
#31100 = CARTESIAN_POINT ( 'NONE',  ( -100.7070736234671955, -3.094860106635371810, -9.524999999987684873 ) ) ;
#31101 = CARTESIAN_POINT ( 'NONE',  ( -98.45499999999998408, 7.632228543268599452, -2.479861379858951942 ) ) ;
#31102 = PRESENTATION_STYLE_ASSIGNMENT (( #35370 ) ) ;
#31103 = ORIENTED_EDGE ( 'NONE', *, *, #26693, .F. ) ;
#31104 = LINE ( 'NONE', #10380, #41122 ) ;
#31105 = DIRECTION ( 'NONE',  ( 0.000000000000000000, 0.000000000000000000, -1.000000000000000000 ) ) ;
#31106 = EDGE_CURVE ( 'NONE', #15830, #33977, #20685, .T. ) ;
#31107 = VERTEX_POINT ( 'NONE', #46549 ) ;
#31108 = DIRECTION ( 'NONE',  ( 1.000000000000000000, 0.000000000000000000, 0.000000000000000000 ) ) ;
#31109 = CARTESIAN_POINT ( 'NONE',  ( -71.99500000000000455, -6.826472737025115478, 4.959722759717900331 ) ) ;
#31110 = ORIENTED_EDGE ( 'NONE', *, *, #66213, .F. ) ;
#31111 = DIRECTION ( 'NONE',  ( 0.000000000000000000, 0.000000000000000000, 1.000000000000000000 ) ) ;
#31112 = SURFACE_STYLE_USAGE ( .BOTH. , #42780 ) ;
#31113 = UNCERTAINTY_MEASURE_WITH_UNIT (LENGTH_MEASURE( 1.000000000000000082E-05 ), #40578, 'distance_accuracy_value', 'NONE');
#31114 = ORIENTED_EDGE ( 'NONE', *, *, #10323, .T. ) ;
#31115 = DIRECTION ( 'NONE',  ( -1.000000000000000000, -9.811390859391773608E-17, -0.000000000000000000 ) ) ;
#31116 = DIRECTION ( 'NONE',  ( -1.000000000000000000, -0.000000000000000000, -0.000000000000000000 ) ) ;
#31117 = VECTOR ( 'NONE', #54669, 1000.000000000000000 ) ;
#31118 = FACE_OUTER_BOUND ( 'NONE', #33996, .T. ) ;
#31120 = EDGE_CURVE ( 'NONE', #20333, #4257, #33038, .T. ) ;
#31119 =( LENGTH_UNIT ( ) NAMED_UNIT ( * ) SI_UNIT ( .MILLI., .METRE. ) );
#31121 = ORIENTED_EDGE ( 'NONE', *, *, #16402, .F. ) ;
#31122 = FACE_OUTER_BOUND ( 'NONE', #55425, .T. ) ;
#31123 = ADVANCED_FACE ( 'NONE', ( #19758 ), #35951, .T. ) ;
#31124 = VERTEX_POINT ( 'NONE', #30644 ) ;
#31125 = DIRECTION ( 'NONE',  ( 0.000000000000000000, 0.000000000000000000, -1.000000000000000000 ) ) ;
#31126 = PLANE ( 'NONE',  #44321 ) ;
#31127 = CYLINDRICAL_SURFACE ( 'NONE', #59143, 0.5000000000000004441 ) ;
#31128 = CARTESIAN_POINT ( 'NONE',  ( -158.6070736234661922, -8.102448949553172852, 5.886773742842742685 ) ) ;
#31129 = EDGE_CURVE ( 'NONE', #45103, #17595, #30756, .T. ) ;
#31130 = CARTESIAN_POINT ( 'NONE',  ( 9.058813317711338797, 123.8449999999999847, -2.943386871421372675 ) ) ;
#31131 = CARTESIAN_POINT ( 'NONE',  ( -100.2570736234661695, 5.598654528085800663, -7.705886871421367523 ) ) ;
#31132 = CARTESIAN_POINT ( 'NONE',  ( 7.632228543268607446, 113.0429263765338135, 2.479861379858954606 ) ) ;
#31133 = ADVANCED_FACE ( 'NONE', ( #44195 ), #16194, .T. ) ;
#31134 = ORIENTED_EDGE ( 'NONE', *, *, #30238, .T. ) ;
#31135 = CARTESIAN_POINT ( 'NONE',  ( -108.4429263765338050, -1.166476076187852838E-15, -9.524999999999991473 ) ) ;
#31137 = CARTESIAN_POINT ( 'NONE',  ( -114.5070736234661837, 8.102448949553176405, 5.886773742842740909 ) ) ;
#31136 = CARTESIAN_POINT ( 'NONE',  ( 44.43085292287548071, 10.23783787917552246, 3.499999999999995115 ) ) ;
#31138 = FILL_AREA_STYLE_COLOUR ( '', #37776 ) ;
#31139 = AXIS2_PLACEMENT_3D ( 'NONE', #42270, #59391, #26688 ) ;
#31140 = CARTESIAN_POINT ( 'NONE',  ( -140.3049999999999500, 8.437984349512085203, -1.550032578732815448E-15 ) ) ;
#31141 = CARTESIAN_POINT ( 'NONE',  ( 1.000000000000000000, 0.9999999999999991118, 79.00402776293826435 ) ) ;
#31142 = DIRECTION ( 'NONE',  ( 1.000000000000000000, 0.000000000000000000, 0.000000000000000000 ) ) ;
#31143 = CARTESIAN_POINT ( 'NONE',  ( -153.7450000000000045, 4.716976649647094177, 6.492361379858945902 ) ) ;
#31144 = CARTESIAN_POINT ( 'NONE',  ( -148.7950000000000159, 2.607480562269069324, -8.024999999999993250 ) ) ;
#31145 = ORIENTED_EDGE ( 'NONE', *, *, #25626, .F. ) ;
#31146 = CARTESIAN_POINT ( 'NONE',  ( 31.00000000000000711, 14.00000000000000000, -34.49999999999999289 ) ) ;
#31147 = APPLICATION_CONTEXT ( 'automotive_design' ) ;
#31148 = PRESENTATION_STYLE_ASSIGNMENT (( #37890 ) ) ;
#31149 = DIRECTION ( 'NONE',  ( 0.000000000000000000, 0.000000000000000000, 1.000000000000000000 ) ) ;
#31150 = UNCERTAINTY_MEASURE_WITH_UNIT (LENGTH_MEASURE( 1.000000000000000082E-05 ), #66588, 'distance_accuracy_value', 'NONE');
#31151 = CARTESIAN_POINT ( 'NONE',  ( -61.55499999999998550, 0.000000000000000000, 8.024999999999991473 ) ) ;
#31152 = DIRECTION ( 'NONE',  ( 0.000000000000000000, 0.000000000000000000, -1.000000000000000000 ) ) ;
#31153 = CARTESIAN_POINT ( 'NONE',  ( -10.01517768586949231, 159.3049999999999784, -6.132527647946036459E-16 ) ) ;
#31154 = CARTESIAN_POINT ( 'NONE',  ( -24.00000000000000000, 1.000000000000000000, -3.000000000000000000 ) ) ;
#31155 = PRESENTATION_STYLE_ASSIGNMENT (( #9749 ) ) ;
#31156 = UNCERTAINTY_MEASURE_WITH_UNIT (LENGTH_MEASURE( 1.000000000000000082E-05 ), #61759, 'distance_accuracy_value', 'NONE');
#31157 = DIRECTION ( 'NONE',  ( 1.000000000000000000, 1.290205704087214075E-15, 4.021988422452563222E-16 ) ) ;
#31158 = DIRECTION ( 'NONE',  ( 0.000000000000000000, 1.000000000000000000, 0.000000000000000000 ) ) ;
#31159 = CARTESIAN_POINT ( 'NONE',  ( -82.25707362346616947, 5.598654528085800663, -7.705886871421367523 ) ) ;
#31160 = AXIS2_PLACEMENT_3D ( 'NONE', #55179, #49945, #44694 ) ;
#31161 = FACE_OUTER_BOUND ( 'NONE', #13361, .T. ) ;
#31162 = CARTESIAN_POINT ( 'NONE',  ( -27.34027958857958396, -7.539040513630480334, -3.506716401632803404E-16 ) ) ;
#31163 = CYLINDRICAL_SURFACE ( 'NONE', #40959, 1.999999999999998224 ) ;
#31164 = CARTESIAN_POINT ( 'NONE',  ( 71.99999999999998579, 119.9999999999997868, -9.500000000000000000 ) ) ;
#31165 = VERTEX_POINT ( 'NONE', #17097 ) ;
#31166 = VERTEX_POINT ( 'NONE', #33248 ) ;
#31167 = CARTESIAN_POINT ( 'NONE',  ( -83.49999999999998579, -3.499999999999999556, 24.00000000000000000 ) ) ;
#31168 =( BOUNDED_CURVE ( )  B_SPLINE_CURVE ( 3, ( #16410, #21280, #37883, #48081 ),
 .UNSPECIFIED., .F., .F. ) 
 B_SPLINE_CURVE_WITH_KNOTS ( ( 4, 4 ),
 ( 0.000000000000000000, 1.570796326794893227 ),
 .UNSPECIFIED. ) 
 CURVE ( )  GEOMETRIC_REPRESENTATION_ITEM ( )  RATIONAL_B_SPLINE_CURVE ( ( 1.000000000000000000, 0.8047378541243658256, 0.8047378541243658256, 1.000000000000000000 ) ) 
 REPRESENTATION_ITEM ( '' )  );
#31169 = FACE_OUTER_BOUND ( 'NONE', #42731, .T. ) ;
#31170 = CARTESIAN_POINT ( 'NONE',  ( 22.65111520450740201, 24.94462592285371727, -27.33786404998805608 ) ) ;
#31171 = AXIS2_PLACEMENT_3D ( 'NONE', #41762, #31495, #37182 ) ;
#31172 = FILL_AREA_STYLE ('',( #41093 ) ) ;
#31173 = ORIENTED_EDGE ( 'NONE', *, *, #46362, .F. ) ;
#31174 = ORIENTED_EDGE ( 'NONE', *, *, #23054, .F. ) ;
#31175 = CARTESIAN_POINT ( 'NONE',  ( -74.75000000000000000, -4.000000000000000000, 0.000000000000000000 ) ) ;
#31176 = VECTOR ( 'NONE', #47738, 1000.000000000000000 ) ;
#31177 = DIRECTION ( 'NONE',  ( -1.000000000000000000, 0.000000000000000000, -3.717264591378879477E-17 ) ) ;
#31178 = CARTESIAN_POINT ( 'NONE',  ( -101.2429263765338021, 5.598654528085804216, 7.705886871421366635 ) ) ;
#31179 = ORIENTED_EDGE ( 'NONE', *, *, #5546, .F. ) ;
#31180 = CARTESIAN_POINT ( 'NONE',  ( 0.000000000000000000, 116.5549999999999926, -9.525000000000000355 ) ) ;
#31181 = DIRECTION ( 'NONE',  ( -0.000000000000000000, -0.000000000000000000, 1.000000000000000000 ) ) ;
#31182 = DIRECTION ( 'NONE',  ( 1.000000000000000000, 0.000000000000000000, 0.000000000000000000 ) ) ;
#31183 = ADVANCED_FACE ( 'NONE', ( #45498 ), #6485, .T. ) ;
#31184 = CARTESIAN_POINT ( 'NONE',  ( -104.6949999999999790, -8.437984349512085203, 5.166775262442717831E-16 ) ) ;
#31185 = VERTEX_POINT ( 'NONE', #27926 ) ;
#31186 = EDGE_CURVE ( 'NONE', #13184, #18616, #49437, .T. ) ;
#31187 = DIRECTION ( 'NONE',  ( 0.000000000000000000, 1.000000000000000000, -0.000000000000000000 ) ) ;
#31188 = DIRECTION ( 'NONE',  ( -0.000000000000000000, 1.000000000000000000, -0.000000000000000000 ) ) ;
#31189 = ORIENTED_EDGE ( 'NONE', *, *, #56471, .T. ) ;
#31190 = CARTESIAN_POINT ( 'NONE',  ( -4.716976649647098618, 157.1429263765338078, 6.492361379858953008 ) ) ;
#31191 = SURFACE_SIDE_STYLE ('',( #168 ) ) ;
#31192 = CARTESIAN_POINT ( 'NONE',  ( 52.75000000000000000, 24.74999999999998224, 4.000000000000000000 ) ) ;
#31193 = FACE_OUTER_BOUND ( 'NONE', #23265, .T. ) ;
#31194 = VERTEX_POINT ( 'NONE', #22694 ) ;
#31195 =( NAMED_UNIT ( * ) PLANE_ANGLE_UNIT ( ) SI_UNIT ( $, .RADIAN. ) );
#31196 = ADVANCED_FACE ( 'NONE', ( #23983 ), #17448, .F. ) ;
#31197 = ORIENTED_EDGE ( 'NONE', *, *, #19924, .F. ) ;
#31198 = FACE_OUTER_BOUND ( 'NONE', #42082, .T. ) ;
#31199 =( NAMED_UNIT ( * ) SI_UNIT ( $, .STERADIAN. ) SOLID_ANGLE_UNIT ( ) );
#31200 = CARTESIAN_POINT ( 'NONE',  ( 44.99999999999998579, 119.9999999999999716, 7.500000000000000000 ) ) ;
#31201 = CARTESIAN_POINT ( 'NONE',  ( -32.02323290426848956, -8.704246530741336585, 6.357025138609439630 ) ) ;
#31202 = FACE_OUTER_BOUND ( 'NONE', #1720, .T. ) ;
#31203 = SURFACE_STYLE_USAGE ( .BOTH. , #65923 ) ;
#31204 = DIRECTION ( 'NONE',  ( 0.000000000000000000, 0.000000000000000000, 1.000000000000000000 ) ) ;
#31205 = CARTESIAN_POINT ( 'NONE',  ( -74.08452722063037754, 9.430195807687217879, 6.039972492249782832 ) ) ;
#31206 = ADVANCED_FACE ( 'NONE', ( #60316 ), #30274, .T. ) ;
#31207 = DIRECTION ( 'NONE',  ( -1.000000000000000000, 0.000000000000000000, -0.000000000000000000 ) ) ;
#31208 = CARTESIAN_POINT ( 'NONE',  ( -13.75000000000000533, 30.74999999999999289, 3.750000000000000000 ) ) ;
#31209 = CARTESIAN_POINT ( 'NONE',  ( 0.000000000000000000, 87.30187232391182306, 0.000000000000000000 ) ) ;
#31210 = ORIENTED_EDGE ( 'NONE', *, *, #35340, .F. ) ;
#31211 = ORIENTED_EDGE ( 'NONE', *, *, #7543, .F. ) ;
#31212 = DIRECTION ( 'NONE',  ( -1.000000000000000000, 0.000000000000000000, 0.000000000000000000 ) ) ;
#31213 = AXIS2_PLACEMENT_3D ( 'NONE', #34355, #55805, #57185 ) ;
#31214 = PRESENTATION_STYLE_ASSIGNMENT (( #36900 ) ) ;
#31215 = CARTESIAN_POINT ( 'NONE',  ( -182.2429263765338021, 5.598654528085804216, 7.705886871421366635 ) ) ;
#31216 = CARTESIAN_POINT ( 'NONE',  ( 74.50000000000000000, 19.30628705663858469, 6.500000000000000000 ) ) ;
#31217 = ORIENTED_EDGE ( 'NONE', *, *, #32621, .F. ) ;
#31218 = CARTESIAN_POINT ( 'NONE',  ( -181.4050000000000011, -2.607480562269069768, 8.024999999999991473 ) ) ;
#31219 = DIRECTION ( 'NONE',  ( -1.000000000000000000, -0.000000000000000000, 3.469446951953610639E-15 ) ) ;
#31220 = DIRECTION ( 'NONE',  ( 1.000000000000000000, 0.000000000000000000, 0.000000000000000000 ) ) ;
#31221 = CARTESIAN_POINT ( 'NONE',  ( -178.9449999999999932, -9.827790563157499189E-16, -8.024999999999991473 ) ) ;
#31222 = VECTOR ( 'NONE', #48095, 1000.000000000000000 ) ;
#31223 = CARTESIAN_POINT ( 'NONE',  ( -180.7449999999999761, 4.716976649647094177, 6.492361379858945902 ) ) ;
#31224 = ORIENTED_EDGE ( 'NONE', *, *, #1863, .T. ) ;
#31225 = CARTESIAN_POINT ( 'NONE',  ( -195.0000000000000000, 1.166476076187852838E-15, -9.524999999999991473 ) ) ;
#31226 = CARTESIAN_POINT ( 'NONE',  ( -1.804616585955809649, -2.331456807317426438, 9.000000000000000000 ) ) ;
#31227 = CARTESIAN_POINT ( 'NONE',  ( -5.000000000000000000, 0.000000000000000000, 0.2499999999999941436 ) ) ;
#31228 = CARTESIAN_POINT ( 'NONE',  ( -94.85499999999998977, 4.716976649647094177, 6.492361379858945902 ) ) ;
#31229 = DIRECTION ( 'NONE',  ( -0.000000000000000000, -1.000000000000000000, -0.000000000000000000 ) ) ;
#31231 = CARTESIAN_POINT ( 'NONE',  ( -74.77251601432477912, 35.95471203479432631, -9.923951063487390201 ) ) ;
#31230 = STYLED_ITEM ( 'NONE', ( #19481 ), #67535 ) ;
#31232 = CARTESIAN_POINT ( 'NONE',  ( -90.14499999999999602, -4.716976649647092401, 6.492361379858946790 ) ) ;
#31233 = CARTESIAN_POINT ( 'NONE',  ( -5.598654528085806881, 122.8549999999999898, -7.705886871421374629 ) ) ;
#31234 = CARTESIAN_POINT ( 'NONE',  ( -61.04499999999998749, 7.632228543268600340, 2.479861379858949277 ) ) ;
#31235 = DIRECTION ( 'NONE',  ( 1.000000000000000000, 0.000000000000000000, 0.000000000000000000 ) ) ;
#31236 = DIRECTION ( 'NONE',  ( -0.000000000000000000, -1.000000000000000000, -0.000000000000000000 ) ) ;
#31237 =( LENGTH_UNIT ( ) NAMED_UNIT ( * ) SI_UNIT ( .MILLI., .METRE. ) );
#31238 = UNCERTAINTY_MEASURE_WITH_UNIT (LENGTH_MEASURE( 1.000000000000000082E-05 ), #46990, 'distance_accuracy_value', 'NONE');
#31239 = EDGE_CURVE ( 'NONE', #24120, #57001, #67243, .T. ) ;
#31240 = CARTESIAN_POINT ( 'NONE',  ( -74.69292637653377653, 10.01517768586948698, -1.839758294383808966E-15 ) ) ;
#31241 = PLANE ( 'NONE',  #44998 ) ;
#31242 = ORIENTED_EDGE ( 'NONE', *, *, #39255, .T. ) ;
#31243 = FILL_AREA_STYLE ('',( #62577 ) ) ;
#31244 = DIRECTION ( 'NONE',  ( 0.000000000000000000, 0.000000000000000000, -1.000000000000000000 ) ) ;
#31245 = VERTEX_POINT ( 'NONE', #61590 ) ;
#31246 = AXIS2_PLACEMENT_3D ( 'NONE', #44053, #44408, #23247 ) ;
#31247 = ORIENTED_EDGE ( 'NONE', *, *, #56645, .T. ) ;
#31248 = FILL_AREA_STYLE_COLOUR ( '', #12715 ) ;
#31249 = CARTESIAN_POINT ( 'NONE',  ( -175.2570736234661695, 5.598654528085800663, -7.705886871421367523 ) ) ;
#31250 = CIRCLE ( 'NONE', #44821, 1.000000000000000888 ) ;
#31251 = CARTESIAN_POINT ( 'NONE',  ( 3.000000000000002665, 42.00000000000000000, -80.00402776293826435 ) ) ;
#31252 = FILL_AREA_STYLE ('',( #53439 ) ) ;
#31253 = STYLED_ITEM ( 'NONE', ( #18073 ), #50834 ) ;
#31254 = FACE_OUTER_BOUND ( 'NONE', #4170, .T. ) ;
#31256 = DIRECTION ( 'NONE',  ( 1.000000000000000000, 0.000000000000000000, 0.000000000000000000 ) ) ;
#31255 = MECHANICAL_DESIGN_GEOMETRIC_PRESENTATION_REPRESENTATION (  '', ( #39200 ), #38054 ) ;
#31257 = VERTEX_POINT ( 'NONE', #13419 ) ;
#31258 = CARTESIAN_POINT ( 'NONE',  ( -119.3049999999999926, 8.437984349512086979, -1.550032578732815448E-15 ) ) ;
#31260 = EDGE_CURVE ( 'NONE', #60615, #56838, #29607, .T. ) ;
#31259 = ORIENTED_EDGE ( 'NONE', *, *, #51267, .F. ) ;
#31261 = SURFACE_STYLE_USAGE ( .BOTH. , #69605 ) ;
#31262 = ADVANCED_FACE ( 'NONE', ( #19396 ), #56331, .T. ) ;
#31263 = ORIENTED_EDGE ( 'NONE', *, *, #68796, .F. ) ;
#31264 =( NAMED_UNIT ( * ) SI_UNIT ( $, .STERADIAN. ) SOLID_ANGLE_UNIT ( ) );
#31265 = ORIENTED_EDGE ( 'NONE', *, *, #31787, .T. ) ;
#31266 = CIRCLE ( 'NONE', #876, 4.000000000000000000 ) ;
#31267 = FILL_AREA_STYLE_COLOUR ( '', #15294 ) ;
#31268 = CARTESIAN_POINT ( 'NONE',  ( -1.166476076187854022E-15, 149.9449999999999932, 9.525000000000000355 ) ) ;
#31269 = DIRECTION ( 'NONE',  ( 1.000000000000000000, -0.000000000000000000, -0.000000000000000000 ) ) ;
#31270 = EDGE_CURVE ( 'NONE', #13709, #4040, #56630, .T. ) ;
#31271 = AXIS2_PLACEMENT_3D ( 'NONE', #48473, #37592, #4452 ) ;
#31272 = ORIENTED_EDGE ( 'NONE', *, *, #965, .T. ) ;
#31273 = CARTESIAN_POINT ( 'NONE',  ( -55.55707362346618083, -1.166476076187852838E-15, -9.524999999999991473 ) ) ;
#31275 = EDGE_CURVE ( 'NONE', #20368, #19233, #40953, .T. ) ;
#31274 = CARTESIAN_POINT ( 'NONE',  ( 5.598654528085809545, 152.2549999999999670, -7.705886871421373741 ) ) ;
#31276 = SURFACE_STYLE_USAGE ( .BOTH. , #30943 ) ;
#31277 = CARTESIAN_POINT ( 'NONE',  ( -71.50000000000000000, 35.92875272052971525, 7.000000000000000000 ) ) ;
#31278 = EDGE_LOOP ( 'NONE', ( #45768, #63141, #43609, #43059 ) ) ;
#31279 = CARTESIAN_POINT ( 'NONE',  ( 4.716976649647099507, 125.6429263765338220, -6.492361379858953008 ) ) ;
#31280 = DIRECTION ( 'NONE',  ( 1.000000000000000000, 0.000000000000000000, -1.300977106640435137E-16 ) ) ;
#31281 = UNCERTAINTY_MEASURE_WITH_UNIT (LENGTH_MEASURE( 1.000000000000000082E-05 ), #62710, 'distance_accuracy_value', 'NONE');
#31282 = CONICAL_SURFACE ( 'NONE', #50387, 4.499999999999976019, 0.7853981633974412846 ) ;
#31283 = SURFACE_STYLE_FILL_AREA ( #68955 ) ;
#31284 = CARTESIAN_POINT ( 'NONE',  ( 6.000000000000017764, 26.00000000000000355, -24.00000000000000355 ) ) ;
#31285 = FACE_OUTER_BOUND ( 'NONE', #29890, .T. ) ;
#31286 = ORIENTED_EDGE ( 'NONE', *, *, #29636, .T. ) ;
#31287 = CARTESIAN_POINT ( 'NONE',  ( -40.83001745922079806, 108.1251451958518146, -3.311254650320285542 ) ) ;
#31288 = EDGE_CURVE ( 'NONE', #65490, #9180, #52488, .T. ) ;
#31289 = ORIENTED_EDGE ( 'NONE', *, *, #64740, .T. ) ;
#31290 = CARTESIAN_POINT ( 'NONE',  ( -54.74292637653380211, -5.598654528085803328, -7.705886871421366635 ) ) ;
#31291 = LINE ( 'NONE', #52106, #30028 ) ;
#31292 = CARTESIAN_POINT ( 'NONE',  ( 12.72792206135785875, 115.4999999999999574, 10.00000000000000000 ) ) ;
#31293 = CARTESIAN_POINT ( 'NONE',  ( -156.6550000000000011, -7.632228543268600340, -2.479861379858950166 ) ) ;
#31294 = VERTEX_POINT ( 'NONE', #53163 ) ;
#31295 = SURFACE_SIDE_STYLE ('',( #62616 ) ) ;
#31296 = UNCERTAINTY_MEASURE_WITH_UNIT (LENGTH_MEASURE( 1.000000000000000082E-05 ), #54723, 'distance_accuracy_value', 'NONE');
#31297 = AXIS2_PLACEMENT_3D ( 'NONE', #18939, #36217, #29860 ) ;
#31298 = LINE ( 'NONE', #59087, #24020 ) ;
#31299 = EDGE_CURVE ( 'NONE', #4136, #3674, #49920, .T. ) ;
#31300 = CARTESIAN_POINT ( 'NONE',  ( -70.49292637653378790, -8.102448949553174629, 5.886773742842742685 ) ) ;
#31301 = SURFACE_SIDE_STYLE ('',( #63333 ) ) ;
#31302 = ORIENTED_EDGE ( 'NONE', *, *, #53904, .F. ) ;
#31303 = ORIENTED_EDGE ( 'NONE', *, *, #47807, .T. ) ;
#31304 = FACE_OUTER_BOUND ( 'NONE', #38682, .T. ) ;
#31305 = VECTOR ( 'NONE', #26952, 1000.000000000000000 ) ;
#31306 = CARTESIAN_POINT ( 'NONE',  ( 53.24999999999999289, 27.74999999999998579, -3.750000000000000000 ) ) ;
#31307 = CARTESIAN_POINT ( 'NONE',  ( -63.50499999999998124, -6.826472737025115478, -4.959722759717899443 ) ) ;
#31308 = ORIENTED_EDGE ( 'NONE', *, *, #20898, .T. ) ;
#31309 = DIRECTION ( 'NONE',  ( -1.000000000000000000, 0.000000000000000000, 0.000000000000000000 ) ) ;
#31310 = DIRECTION ( 'NONE',  ( 0.000000000000000000, 0.000000000000000000, -1.000000000000000000 ) ) ;
#31311 = AXIS2_PLACEMENT_3D ( 'NONE', #8468, #3106, #30576 ) ;
#31312 = FACE_OUTER_BOUND ( 'NONE', #3473, .T. ) ;
#31313 = DIRECTION ( 'NONE',  ( 0.000000000000000000, 0.000000000000000000, -1.000000000000000000 ) ) ;
#31314 = CIRCLE ( 'NONE', #40331, 3.100000000000000533 ) ;
#31315 = ORIENTED_EDGE ( 'NONE', *, *, #63836, .F. ) ;
#31316 = DIRECTION ( 'NONE',  ( 0.000000000000000000, 0.000000000000000000, 1.000000000000000000 ) ) ;
#31317 = COLOUR_RGB ( '', 0.40784314, 0.44705882, 0.49803922) ;
#31318 = DIRECTION ( 'NONE',  ( 0.7071067811865500152, 8.659560562354963673E-17, -0.7071067811865450192 ) ) ;
#31319 = AXIS2_PLACEMENT_3D ( 'NONE', #6068, #54924, #6751 ) ;
#31320 = CARTESIAN_POINT ( 'NONE',  ( -114.8949999999999818, 6.826472737025115478, 4.959722759717899443 ) ) ;
#31321 = B_SPLINE_CURVE_WITH_KNOTS ( 'NONE', 3,
 ( #19138, #19494, #45915, #57485, #8615, #2583 ),
 .UNSPECIFIED., .F., .F.,
 ( 4, 2, 4 ),
 ( 0.000000000000000000, 0.0007817461686317332984, 0.001563492337263466597 ),
 .UNSPECIFIED. ) ;
#31322 = CARTESIAN_POINT ( 'NONE',  ( -9.058813317711337021, 146.0449999999999875, -2.943386871421374895 ) ) ;
#31323 = CARTESIAN_POINT ( 'NONE',  ( -93.29499999999998749, -2.607480562269069768, 8.024999999999991473 ) ) ;
#31324 =( NAMED_UNIT ( * ) PLANE_ANGLE_UNIT ( ) SI_UNIT ( $, .RADIAN. ) );
#31325 =( GEOMETRIC_REPRESENTATION_CONTEXT ( 3 ) GLOBAL_UNCERTAINTY_ASSIGNED_CONTEXT ( ( #11582 ) ) GLOBAL_UNIT_ASSIGNED_CONTEXT ( ( #4760, #21635, #32196 ) ) REPRESENTATION_CONTEXT ( 'NONE', 'WORKASPACE' ) );
#31326 = UNCERTAINTY_MEASURE_WITH_UNIT (LENGTH_MEASURE( 1.000000000000000082E-05 ), #60743, 'distance_accuracy_value', 'NONE');
#31327 = CIRCLE ( 'NONE', #23490, 0.5000000000000004441 ) ;
#31328 = ADVANCED_FACE ( 'NONE', ( #25026 ), #36676, .T. ) ;
#31329 = ORIENTED_EDGE ( 'NONE', *, *, #50065, .T. ) ;
#31330 = CARTESIAN_POINT ( 'NONE',  ( -136.7929263765338135, -3.094860106618429807, 9.524999999999991473 ) ) ;
#31331 = CARTESIAN_POINT ( 'NONE',  ( 74.99999999999998579, 50.00000000000000000, -9.500000000000000000 ) ) ;
#31332 = CARTESIAN_POINT ( 'NONE',  ( -153.5949999999999989, 2.607480562269073321, 8.024999999999991473 ) ) ;
#31333 = CARTESIAN_POINT ( 'NONE',  ( 44.99999999999977973, 149.9999999999999716, -9.500000000000000000 ) ) ;
#31334 = CIRCLE ( 'NONE', #2043, 9.000000000000007105 ) ;
#31335 = PRESENTATION_STYLE_ASSIGNMENT (( #52834 ) ) ;
#31336 = DIRECTION ( 'NONE',  ( 1.776356839400250465E-15, 0.000000000000000000, 1.000000000000000000 ) ) ;
#31337 = ORIENTED_EDGE ( 'NONE', *, *, #21944, .T. ) ;
#31338 = VERTEX_POINT ( 'NONE', #53500 ) ;
#31339 = FILL_AREA_STYLE_COLOUR ( '', #2643 ) ;
#31340 = EDGE_CURVE ( 'NONE', #36018, #60418, #19569, .T. ) ;
#31341 = PRESENTATION_LAYER_ASSIGNMENT (  '', '', ( #44906 ) ) ;
#31342 = CARTESIAN_POINT ( 'NONE',  ( -45.76754978044866817, 8.860682567649741159, 6.389379348043552120 ) ) ;
#31343 = SURFACE_STYLE_USAGE ( .BOTH. , #65084 ) ;
#31344 =( LENGTH_UNIT ( ) NAMED_UNIT ( * ) SI_UNIT ( .MILLI., .METRE. ) );
#31345 = CIRCLE ( 'NONE', #51550, 4.999999999999999112 ) ;
#31346 = ORIENTED_EDGE ( 'NONE', *, *, #23418, .F. ) ;
#31347 = CARTESIAN_POINT ( 'NONE',  ( -152.1549999999999727, 7.632228543268600340, 2.479861379858949277 ) ) ;
#31348 = EDGE_CURVE ( 'NONE', #19536, #7659, #4226, .T. ) ;
#31349 = ADVANCED_FACE ( 'NONE', ( #3893 ), #54360, .T. ) ;
#31350 = VERTEX_POINT ( 'NONE', #67961 ) ;
#31351 = LINE ( 'NONE', #64064, #54850 ) ;
#31352 = EDGE_LOOP ( 'NONE', ( #59327, #61320, #44663, #45449 ) ) ;
#31353 = AXIS2_PLACEMENT_3D ( 'NONE', #8648, #2958, #24447 ) ;
#31354 = SURFACE_STYLE_USAGE ( .BOTH. , #26434 ) ;
#31355 = CARTESIAN_POINT ( 'NONE',  ( -3.094860106618434248, 116.7949999999999591, 9.525000000000000355 ) ) ;
#31356 = FILL_AREA_STYLE_COLOUR ( '', #4744 ) ;
#31357 = CIRCLE ( 'NONE', #2120, 5.499999999999976907 ) ;
#31358 = AXIS2_PLACEMENT_3D ( 'NONE', #59556, #5386, #42752 ) ;
#31359 = VERTEX_POINT ( 'NONE', #68293 ) ;
#31360 = DIRECTION ( 'NONE',  ( -1.000000000000000000, -0.000000000000000000, 4.625929269271505635E-16 ) ) ;
#31362 = EDGE_CURVE ( 'NONE', #43417, #46008, #42079, .T. ) ;
#31361 = CARTESIAN_POINT ( 'NONE',  ( -5.598654528085808657, 117.7549999999999812, 7.705886871421373741 ) ) ;
#31363 = CARTESIAN_POINT ( 'NONE',  ( -63.05499999999998550, -9.827790563157499189E-16, -8.024999999999991473 ) ) ;
#31364 = DIRECTION ( 'NONE',  ( -0.000000000000000000, -0.000000000000000000, -1.000000000000000000 ) ) ;
#31365 = ORIENTED_EDGE ( 'NONE', *, *, #69206, .T. ) ;
#31366 = CARTESIAN_POINT ( 'NONE',  ( 8.102448949553183510, 146.1049999999999898, -5.886773742842746238 ) ) ;
#31367 = UNCERTAINTY_MEASURE_WITH_UNIT (LENGTH_MEASURE( 1.000000000000000082E-05 ), #59264, 'distance_accuracy_value', 'NONE');
#31368 = CARTESIAN_POINT ( 'NONE',  ( -4.041451884327380562, 2.500000000000000000, -7.000000000000003553 ) ) ;
#31369 = EDGE_CURVE ( 'NONE', #9217, #9855, #16920, .T. ) ;
#31370 =( NAMED_UNIT ( * ) PLANE_ANGLE_UNIT ( ) SI_UNIT ( $, .RADIAN. ) );
#31371 = ORIENTED_EDGE ( 'NONE', *, *, #25177, .F. ) ;
#31372 = VECTOR ( 'NONE', #15618, 1000.000000000000000 ) ;
#31373 = LINE ( 'NONE', #69045, #28363 ) ;
#31374 = CARTESIAN_POINT ( 'NONE',  ( -182.1549999999999727, 7.632228543268600340, 2.479861379858949277 ) ) ;
#31375 = EDGE_LOOP ( 'NONE', ( #32180, #6384, #20664, #17560 ) ) ;
#31376 = CARTESIAN_POINT ( 'NONE',  ( 6.766228288048925954, 111.1834974234494098, 5.697616492254868881 ) ) ;
#31377 = AXIS2_PLACEMENT_3D ( 'NONE', #3344, #24836, #24153 ) ;
#31378 = FILL_AREA_STYLE_COLOUR ( '', #69448 ) ;
#31379 = SURFACE_STYLE_USAGE ( .BOTH. , #10986 ) ;
#31380 = ORIENTED_EDGE ( 'NONE', *, *, #54570, .T. ) ;
#31381 = CARTESIAN_POINT ( 'NONE',  ( -21.02379604162863913, 109.9999999999999858, 10.50000000000000000 ) ) ;
#31382 = DIRECTION ( 'NONE',  ( 0.000000000000000000, 0.000000000000000000, -1.000000000000000000 ) ) ;
#31383 = VERTEX_POINT ( 'NONE', #303 ) ;
#31384 = PRESENTATION_LAYER_ASSIGNMENT (  '', '', ( #47159 ) ) ;
#31385 = CARTESIAN_POINT ( 'NONE',  ( -3.414918479307654575, -7.000000000000001776, 0.7696370661448970196 ) ) ;
#31386 = CARTESIAN_POINT ( 'NONE',  ( -93.95499999999998408, -7.632228543268599452, 2.479861379858951054 ) ) ;
#31387 = ORIENTED_EDGE ( 'NONE', *, *, #17873, .T. ) ;
#31388 = DIRECTION ( 'NONE',  ( 1.000000000000000000, 0.000000000000000000, 0.000000000000000000 ) ) ;
#31389 =( LENGTH_UNIT ( ) NAMED_UNIT ( * ) SI_UNIT ( .MILLI., .METRE. ) );
#31390 = CARTESIAN_POINT ( 'NONE',  ( -131.7570736234661695, -5.598654528085801552, 7.705886871421367523 ) ) ;
#31392 = EDGE_CURVE ( 'NONE', #12794, #38350, #48250, .T. ) ;
#31391 = STYLED_ITEM ( 'NONE', ( #11832 ), #1111 ) ;
#31393 = AXIS2_PLACEMENT_3D ( 'NONE', #8651, #62781, #56479 ) ;
#31394 = DIRECTION ( 'NONE',  ( -0.000000000000000000, -1.000000000000000000, -0.000000000000000000 ) ) ;
#31395 = DIRECTION ( 'NONE',  ( -0.000000000000000000, -1.000000000000000000, -0.000000000000000000 ) ) ;
#31396 = CARTESIAN_POINT ( 'NONE',  ( -75.50707362346616947, 8.102448949553176405, 5.886773742842740909 ) ) ;
#31397 = ORIENTED_EDGE ( 'NONE', *, *, #69121, .F. ) ;
#31398 = FACE_OUTER_BOUND ( 'NONE', #29548, .T. ) ;
#31399 = CARTESIAN_POINT ( 'NONE',  ( -18.05120619030912721, -11.32434288914918596, 3.974503633080903597 ) ) ;
#31400 = PRESENTATION_STYLE_ASSIGNMENT (( #32119 ) ) ;
#31401 = STYLED_ITEM ( 'NONE', ( #14540 ), #42953 ) ;
#31402 = CARTESIAN_POINT ( 'NONE',  ( -114.0549999999999926, -9.827790563157499189E-16, -8.024999999999991473 ) ) ;
#31403 = CARTESIAN_POINT ( 'NONE',  ( 69.74999999999998579, 37.00000000000000000, -3.000000000000000000 ) ) ;
#31404 = CARTESIAN_POINT ( 'NONE',  ( -3.094860106618434248, 119.7949999999999733, 9.525000000000000355 ) ) ;
#31405 = CARTESIAN_POINT ( 'NONE',  ( -127.0449999999999875, 7.632228543268600340, 2.479861379858949277 ) ) ;
#31406 = CIRCLE ( 'NONE', #16838, 0.2500000000000002220 ) ;
#31407 = AXIS2_PLACEMENT_3D ( 'NONE', #56039, #13474, #7853 ) ;
#31408 = CARTESIAN_POINT ( 'NONE',  ( 65.00000000000000000, 1.797044900979284448E-15, 11.50000000000003730 ) ) ;
#31409 = VECTOR ( 'NONE', #33190, 1000.000000000000000 ) ;
#31410 = DIRECTION ( 'NONE',  ( 0.000000000000000000, 0.000000000000000000, -1.000000000000000000 ) ) ;
#31411 = ORIENTED_EDGE ( 'NONE', *, *, #19047, .T. ) ;
#31412 = CARTESIAN_POINT ( 'NONE',  ( -164.6929263765338476, 10.01517768586948698, -1.839758294383808571E-15 ) ) ;
#31413 =( NAMED_UNIT ( * ) SI_UNIT ( $, .STERADIAN. ) SOLID_ANGLE_UNIT ( ) );
#31414 = DIRECTION ( 'NONE',  ( -1.000000000000000000, -0.000000000000000000, -0.000000000000000000 ) ) ;
#31415 = TOROIDAL_SURFACE ( 'NONE', #2124, 7.249999999999999112, 0.2500000000000000000 ) ;
#31416 = CARTESIAN_POINT ( 'NONE',  ( -20.57648123223239622, 114.4999999999999574, -10.27659574468085246 ) ) ;
#31417 = DIRECTION ( 'NONE',  ( 1.000000000000000000, 0.000000000000000000, -0.000000000000000000 ) ) ;
#31418 = VERTEX_POINT ( 'NONE', #12285 ) ;
#31419 = CARTESIAN_POINT ( 'NONE',  ( -76.64292637653380780, -5.598654528085801552, 7.705886871421367523 ) ) ;
#31420 = STYLED_ITEM ( 'NONE', ( #13338 ), #16422 ) ;
#31421 = LINE ( 'NONE', #16680, #20620 ) ;
#31422 = CYLINDRICAL_SURFACE ( 'NONE', #10266, 4.999999999999997335 ) ;
#31423 = EDGE_CURVE ( 'NONE', #54731, #28244, #6114, .T. ) ;
#31424 = PRESENTATION_STYLE_ASSIGNMENT (( #20900 ) ) ;
#31425 =( NAMED_UNIT ( * ) SI_UNIT ( $, .STERADIAN. ) SOLID_ANGLE_UNIT ( ) );
#31426 = DIRECTION ( 'NONE',  ( -1.000000000000000000, 0.000000000000000000, 0.000000000000000000 ) ) ;
#31427 = AXIS2_PLACEMENT_3D ( 'NONE', #5617, #27069, #298 ) ;
#31428 = CARTESIAN_POINT ( 'NONE',  ( -175.2549999999999955, -4.716976649647092401, 6.492361379858946790 ) ) ;
#31429 = EDGE_CURVE ( 'NONE', #12421, #56786, #16111, .T. ) ;
#31430 = ORIENTED_EDGE ( 'NONE', *, *, #39762, .T. ) ;
#31431 = DIRECTION ( 'NONE',  ( 0.000000000000000000, 0.000000000000000000, -1.000000000000000000 ) ) ;
#31432 =( NAMED_UNIT ( * ) PLANE_ANGLE_UNIT ( ) SI_UNIT ( $, .RADIAN. ) );
#31433 = CARTESIAN_POINT ( 'NONE',  ( -73.70707362346617231, -3.094860106618431139, -9.524999999999991473 ) ) ;
#31434 = VERTEX_POINT ( 'NONE', #11266 ) ;
#31435 = CARTESIAN_POINT ( 'NONE',  ( -109.9429263765338050, 0.000000000000000000, 9.524999999999991473 ) ) ;
#31436 = AXIS2_PLACEMENT_3D ( 'NONE', #16719, #22663, #59225 ) ;
#31437 = VECTOR ( 'NONE', #19371, 1000.000000000000000 ) ;
#31438 = CARTESIAN_POINT ( 'NONE',  ( 8.437984349512095861, 138.3070736234661808, 1.550032578732817026E-15 ) ) ;
#31439 = LINE ( 'NONE', #62757, #23685 ) ;
#31440 = ORIENTED_EDGE ( 'NONE', *, *, #50357, .F. ) ;
#31441 = VECTOR ( 'NONE', #52823, 1000.000000000000000 ) ;
#31442 = DIRECTION ( 'NONE',  ( -1.000000000000000000, 0.000000000000000000, 0.000000000000000000 ) ) ;
#31443 = CARTESIAN_POINT ( 'NONE',  ( -91.70499999999998408, 2.607480562269072433, 8.024999999999991473 ) ) ;
#31444 = UNCERTAINTY_MEASURE_WITH_UNIT (LENGTH_MEASURE( 1.000000000000000082E-05 ), #21067, 'distance_accuracy_value', 'NONE');
#31445 = CARTESIAN_POINT ( 'NONE',  ( -15.98999599679679839, 117.9999999999999716, 7.500000000000000000 ) ) ;
#31446 = ORIENTED_EDGE ( 'NONE', *, *, #31423, .T. ) ;
#31447 = CARTESIAN_POINT ( 'NONE',  ( -36.12863118297439513, -11.74752507246378386, 1.561659418384358400 ) ) ;
#31448 = EDGE_CURVE ( 'NONE', #59410, #44068, #21837, .T. ) ;
#31449 = CARTESIAN_POINT ( 'NONE',  ( 8.437984349512095861, 143.1929263765337907, 1.550032578732816828E-15 ) ) ;
#31450 = DIRECTION ( 'NONE',  ( 1.000000000000000000, 0.000000000000000000, 0.000000000000000000 ) ) ;
#31451 = CARTESIAN_POINT ( 'NONE',  ( -57.58629378005873889, -7.761720733523185700, -0.7755720678490086728 ) ) ;
#31452 = CIRCLE ( 'NONE', #1065, 1.000000000000000000 ) ;
#31453 = COLOUR_RGB ( '', 0.66274510, 0.83137255, 0.94901961) ;
#31454 = VERTEX_POINT ( 'NONE', #28107 ) ;
#31455 = CARTESIAN_POINT ( 'NONE',  ( 15.48999599679679662, 118.4999999999999716, -7.500000000000000000 ) ) ;
#31456 = CARTESIAN_POINT ( 'NONE',  ( -71.69499999999999318, -8.437984349512085203, 5.166775262442717831E-16 ) ) ;
#31458 = ORIENTED_EDGE ( 'NONE', *, *, #15387, .F. ) ;
#31457 = CIRCLE ( 'NONE', #8988, 0.5000000000000004441 ) ;
#31459 = DIRECTION ( 'NONE',  ( 0.000000000000000000, 0.000000000000000000, -1.000000000000000000 ) ) ;
#31460 = CARTESIAN_POINT ( 'NONE',  ( -124.5570736234661808, -1.166476076187852838E-15, -9.524999999999991473 ) ) ;
#31461 = CIRCLE ( 'NONE', #10151, 0.5000000000000004441 ) ;
#31462 = ORIENTED_EDGE ( 'NONE', *, *, #22553, .T. ) ;
#31463 = CARTESIAN_POINT ( 'NONE',  ( 48.74999999999999289, 24.99999999999998579, -3.750000000000000000 ) ) ;
#31464 = FILL_AREA_STYLE_COLOUR ( '', #23563 ) ;
#31465 = AXIS2_PLACEMENT_3D ( 'NONE', #1179, #12839, #65619 ) ;
#31466 =( NAMED_UNIT ( * ) SI_UNIT ( $, .STERADIAN. ) SOLID_ANGLE_UNIT ( ) );
#31467 = CARTESIAN_POINT ( 'NONE',  ( -74.08452722063037754, 9.430195807687217879, 6.000000000000000888 ) ) ;
#31468 = ORIENTED_EDGE ( 'NONE', *, *, #10953, .T. ) ;
#31469 = CARTESIAN_POINT ( 'NONE',  ( -20.71231517720797655, 149.4999999999999716, 10.00000000000000000 ) ) ;
#31470 = AXIS2_PLACEMENT_3D ( 'NONE', #40465, #61885, #62918 ) ;
#31471 = ORIENTED_EDGE ( 'NONE', *, *, #65674, .T. ) ;
#31472 = PLANE ( 'NONE',  #2083 ) ;
#31473 = CARTESIAN_POINT ( 'NONE',  ( -149.5429263765338135, 9.058813317711329915, 2.943386871421369566 ) ) ;
#31475 = AXIS2_PLACEMENT_3D ( 'NONE', #8764, #62218, #8431 ) ;
#31474 = CARTESIAN_POINT ( 'NONE',  ( -40.96656732556692759, 108.0254117342835229, 3.574171091744781315 ) ) ;
#31476 = CARTESIAN_POINT ( 'NONE',  ( -157.2570736234661979, 5.598654528085800663, -7.705886871421367523 ) ) ;
#31477 = EDGE_CURVE ( 'NONE', #4847, #32128, #43673, .T. ) ;
#31478 = TOROIDAL_SURFACE ( 'NONE', #1082, 17.00000000000000355, 1.000000000000000000 ) ;
#31479 = CARTESIAN_POINT ( 'NONE',  ( 5.598654528085805993, 120.2449999999999903, 7.705886871421374629 ) ) ;
#31480 = CARTESIAN_POINT ( 'NONE',  ( -99.50707362346614104, 8.102448949553176405, 5.886773742842740909 ) ) ;
#31481 =( GEOMETRIC_REPRESENTATION_CONTEXT ( 3 ) GLOBAL_UNCERTAINTY_ASSIGNED_CONTEXT ( ( #19214 ) ) GLOBAL_UNIT_ASSIGNED_CONTEXT ( ( #26735, #37374, #15893 ) ) REPRESENTATION_CONTEXT ( 'NONE', 'WORKASPACE' ) );
#31482 = CARTESIAN_POINT ( 'NONE',  ( 27.00000000000001776, 15.00000000000000000, 34.49999999999999289 ) ) ;
#31483 = ORIENTED_EDGE ( 'NONE', *, *, #53682, .F. ) ;
#31484 =( GEOMETRIC_REPRESENTATION_CONTEXT ( 3 ) GLOBAL_UNCERTAINTY_ASSIGNED_CONTEXT ( ( #68472 ) ) GLOBAL_UNIT_ASSIGNED_CONTEXT ( ( #20347, #30896, #47123 ) ) REPRESENTATION_CONTEXT ( 'NONE', 'WORKASPACE' ) );
#31485 = DIRECTION ( 'NONE',  ( 0.000000000000000000, 1.000000000000000000, 0.000000000000000000 ) ) ;
#31486 = LINE ( 'NONE', #26214, #5400 ) ;
#31487 = CARTESIAN_POINT ( 'NONE',  ( -137.1550000000000011, 7.632228543268600340, 2.479861379858949277 ) ) ;
#31488 = DIRECTION ( 'NONE',  ( 1.000000000000000000, 0.000000000000000000, -0.000000000000000000 ) ) ;
#31489 = DIRECTION ( 'NONE',  ( 0.000000000000000000, 0.000000000000000000, 1.000000000000000000 ) ) ;
#31490 = CARTESIAN_POINT ( 'NONE',  ( -158.2450000000000045, -4.716976649647093289, -6.492361379858945902 ) ) ;
#31491 = CARTESIAN_POINT ( 'NONE',  ( -135.5949999999999989, 2.607480562269072433, 8.024999999999991473 ) ) ;
#31492 = CIRCLE ( 'NONE', #2206, 23.00000000000000000 ) ;
#31493 = EDGE_LOOP ( 'NONE', ( #62539, #63229, #37322, #41288 ) ) ;
#31494 = CARTESIAN_POINT ( 'NONE',  ( -9.827790563157511022E-16, 128.5570736234661524, 8.025000000000000355 ) ) ;
#31495 = DIRECTION ( 'NONE',  ( 1.000000000000000000, 0.000000000000000000, -1.300977106640434891E-16 ) ) ;
#31496 = AXIS2_PLACEMENT_3D ( 'NONE', #7718, #50642, #23901 ) ;
#31497 = CARTESIAN_POINT ( 'NONE',  ( 0.000000000000000000, 2.000000000000000444, 3.000000000000000444 ) ) ;
#31498 = CARTESIAN_POINT ( 'NONE',  ( -49.70499999999996987, 2.607480562269073321, 8.024999999999991473 ) ) ;
#31499 = CARTESIAN_POINT ( 'NONE',  ( 5.598654528085809545, 158.2549999999999670, -7.705886871421373741 ) ) ;
#31500 = CARTESIAN_POINT ( 'NONE',  ( -52.19292637653380496, -10.01517768586948698, 6.132527647946031529E-16 ) ) ;
#31501 = CARTESIAN_POINT ( 'NONE',  ( 4.000000000000030198, 37.76051491742381216, 89.34202014332566932 ) ) ;
#31502 = ADVANCED_FACE ( 'NONE', ( #22525 ), #44024, .T. ) ;
#31503 = VECTOR ( 'NONE', #51103, 1000.000000000000000 ) ;
#31504 = MECHANICAL_DESIGN_GEOMETRIC_PRESENTATION_REPRESENTATION (  '', ( #4541 ), #7916 ) ;
#31505 = CARTESIAN_POINT ( 'NONE',  ( -154.8570736234661922, -5.598654528085803328, -7.705886871421366635 ) ) ;
#31506 = AXIS2_PLACEMENT_3D ( 'NONE', #33356, #54784, #22810 ) ;
#31507 = CARTESIAN_POINT ( 'NONE',  ( 41.50000000000002132, 26.00000000000000355, -24.00000000000001421 ) ) ;
#31508 = DIRECTION ( 'NONE',  ( -1.000000000000000000, 0.000000000000000000, 0.000000000000000000 ) ) ;
#31509 = AXIS2_PLACEMENT_3D ( 'NONE', #8181, #40201, #7812 ) ;
#31510 = PRESENTATION_LAYER_ASSIGNMENT (  '', '', ( #11286 ) ) ;
#31511 = CARTESIAN_POINT ( 'NONE',  ( -81.35707362346616378, 5.598654528085804216, 7.705886871421366635 ) ) ;
#31512 = DIRECTION ( 'NONE',  ( 1.000000000000000000, 0.000000000000000000, 0.000000000000000000 ) ) ;
#31513 = AXIS2_PLACEMENT_3D ( 'NONE', #60930, #38147, #49054 ) ;
#31514 = SURFACE_STYLE_FILL_AREA ( #42145 ) ;
#31515 = ADVANCED_FACE ( 'NONE', ( #54521 ), #40999, .F. ) ;
#31516 = VECTOR ( 'NONE', #6643, 1000.000000000000000 ) ;
#31517 = CARTESIAN_POINT ( 'NONE',  ( -2.607480562268991608, 139.2929263765338419, 8.025000000000060751 ) ) ;
#31518 = CARTESIAN_POINT ( 'NONE',  ( 0.000000000000000000, -2.500000000000000000, 0.000000000000000000 ) ) ;
#31519 = DIRECTION ( 'NONE',  ( -0.000000000000000000, -1.000000000000000000, 0.000000000000000000 ) ) ;
#31520 = EDGE_LOOP ( 'NONE', ( #22072, #20875, #32094, #45374 ) ) ;
#31521 = VERTEX_POINT ( 'NONE', #27424 ) ;
#31522 = LINE ( 'NONE', #53356, #28457 ) ;
#31523 = EDGE_CURVE ( 'NONE', #61248, #57942, #28543, .T. ) ;
#31524 = AXIS2_PLACEMENT_3D ( 'NONE', #46642, #2928, #61693 ) ;
#31525 = CARTESIAN_POINT ( 'NONE',  ( -9.827790563157511022E-16, 110.5570736234661524, 8.025000000000000355 ) ) ;
#31526 = PRODUCT_DEFINITION_FORMATION_WITH_SPECIFIED_SOURCE ( 'ANY', '', #9133, .NOT_KNOWN. ) ;
#31527 = EDGE_CURVE ( 'NONE', #27365, #25944, #45489, .T. ) ;
#31528 = CARTESIAN_POINT ( 'NONE',  ( -20.17763807713225432, 115.4773716707933460, 10.00000000000000000 ) ) ;
#31529 =( GEOMETRIC_REPRESENTATION_CONTEXT ( 3 ) GLOBAL_UNCERTAINTY_ASSIGNED_CONTEXT ( ( #61428 ) ) GLOBAL_UNIT_ASSIGNED_CONTEXT ( ( #35686, #63095, #62406 ) ) REPRESENTATION_CONTEXT ( 'NONE', 'WORKASPACE' ) );
#31530 = VERTEX_POINT ( 'NONE', #50301 ) ;
#31531 = ORIENTED_EDGE ( 'NONE', *, *, #19367, .T. ) ;
#31532 = CARTESIAN_POINT ( 'NONE',  ( 0.000000000000000000, -1.999999999999995337, 0.000000000000000000 ) ) ;
#31533 = EDGE_CURVE ( 'NONE', #19777, #15724, #8437, .T. ) ;
#31534 = CARTESIAN_POINT ( 'NONE',  ( -17.75000000000000711, 31.24999999999999289, -3.750000000000000000 ) ) ;
#31535 = FACE_BOUND ( 'NONE', #16166, .T. ) ;
#31536 = ORIENTED_EDGE ( 'NONE', *, *, #25693, .F. ) ;
#31537 = CARTESIAN_POINT ( 'NONE',  ( 3.094860106618431583, 121.2049999999999841, 9.525000000000000355 ) ) ;
#31538 = DIRECTION ( 'NONE',  ( 1.000000000000000000, 0.000000000000000000, 0.000000000000000000 ) ) ;
#31539 = FILL_AREA_STYLE ('',( #10109 ) ) ;
#31540 = TOROIDAL_SURFACE ( 'NONE', #34915, 1.000000000000000000, 0.5000000000000000000 ) ;
#31541 = DIRECTION ( 'NONE',  ( 0.000000000000000000, 1.000000000000000000, -0.000000000000000000 ) ) ;
#31542 = CARTESIAN_POINT ( 'NONE',  ( -103.9449999999999932, -9.827790563157499189E-16, -8.024999999999991473 ) ) ;
#31543 = ORIENTED_EDGE ( 'NONE', *, *, #69300, .T. ) ;
#31544 = CARTESIAN_POINT ( 'NONE',  ( 1.613420992953035871, 154.3163448595890088, -9.236620315407188642 ) ) ;
#31545 = SURFACE_STYLE_USAGE ( .BOTH. , #41446 ) ;
#31546 = AXIS2_PLACEMENT_3D ( 'NONE', #36218, #25955, #42898 ) ;
#31547 = ORIENTED_EDGE ( 'NONE', *, *, #25950, .F. ) ;
#31548 = CARTESIAN_POINT ( 'NONE',  ( 7.632228543268608334, 158.3429263765338249, -2.479861379858951942 ) ) ;
#31549 = DIRECTION ( 'NONE',  ( 1.000000000000000000, -0.000000000000000000, -0.000000000000000000 ) ) ;
#31550 = AXIS2_PLACEMENT_3D ( 'NONE', #16506, #48173, #20716 ) ;
#31551 = DIRECTION ( 'NONE',  ( 0.000000000000000000, 0.000000000000000000, -1.000000000000000000 ) ) ;
#31552 = DIRECTION ( 'NONE',  ( -0.000000000000000000, 1.000000000000000000, -0.000000000000000000 ) ) ;
#31553 = CIRCLE ( 'NONE', #59670, 0.5000000000000004441 ) ;
#31554 = CARTESIAN_POINT ( 'NONE',  ( -63.05707362346617373, 0.000000000000000000, 9.524999999999991473 ) ) ;
#31555 = VERTEX_POINT ( 'NONE', #2020 ) ;
#31556 = CARTESIAN_POINT ( 'NONE',  ( 2.607480562269071989, 127.5929263765338249, 8.025000000000002132 ) ) ;
#31557 = CARTESIAN_POINT ( 'NONE',  ( 13.25000000000000355, 28.24999999999998934, 4.000000000000000000 ) ) ;
#31558 = DIRECTION ( 'NONE',  ( 0.000000000000000000, 0.000000000000000000, 1.000000000000000000 ) ) ;
#31559 = CARTESIAN_POINT ( 'NONE',  ( -34.27411267550463236, -10.24482008810693578, 4.106145367377594724 ) ) ;
#31560 = PRESENTATION_LAYER_ASSIGNMENT (  '', '', ( #15833 ) ) ;
#31561 = DIRECTION ( 'NONE',  ( 0.000000000000000000, -1.000000000000000000, 0.000000000000000000 ) ) ;
#31562 = LINE ( 'NONE', #36194, #22774 ) ;
#31563 = CARTESIAN_POINT ( 'NONE',  ( 7.750000000000019540, 4.481368979606759023E-15, 3.750000000000000000 ) ) ;
#31564 = CARTESIAN_POINT ( 'NONE',  ( 13.25000000000000355, 27.99999999999998934, -3.750000000000000000 ) ) ;
#31565 = DIRECTION ( 'NONE',  ( -0.000000000000000000, 0.000000000000000000, -1.000000000000000000 ) ) ;
#31566 = VERTEX_POINT ( 'NONE', #56607 ) ;
#31567 = COLOUR_RGB ( '', 0.08235294, 0.09019608, 0.10196078) ;
#31568 = ORIENTED_EDGE ( 'NONE', *, *, #1701, .T. ) ;
#31569 = CARTESIAN_POINT ( 'NONE',  ( 3.062509476195515228E-31, -2.500728763858896269E-15, 12.50000000000000000 ) ) ;
#31570 = DIRECTION ( 'NONE',  ( -1.000000000000000000, -0.000000000000000000, -0.000000000000000000 ) ) ;
#31571 = ORIENTED_EDGE ( 'NONE', *, *, #63624, .F. ) ;
#31572 = FILL_AREA_STYLE_COLOUR ( '', #38295 ) ;
#31573 = CARTESIAN_POINT ( 'NONE',  ( -173.0049999999999670, 6.826472737025116366, 4.959722759717898555 ) ) ;
#31574 = DIRECTION ( 'NONE',  ( 1.000000000000000000, 0.000000000000000000, 0.000000000000000000 ) ) ;
#31575 = CYLINDRICAL_SURFACE ( 'NONE', #13357, 0.2500000000000002220 ) ;
#31576 = AXIS2_PLACEMENT_3D ( 'NONE', #66073, #12605, #7353 ) ;
#31577 = CARTESIAN_POINT ( 'NONE',  ( -180.8949999999999534, 6.826472737025116366, 4.959722759717898555 ) ) ;
#31578 = CARTESIAN_POINT ( 'NONE',  ( -163.1949999999999932, 8.437984349512086979, -1.550032578732815448E-15 ) ) ;
#31579 = CIRCLE ( 'NONE', #35971, 0.5000000000000004441 ) ;
#31580 = ORIENTED_EDGE ( 'NONE', *, *, #45397, .F. ) ;
#31581 = DIRECTION ( 'NONE',  ( -1.000000000000000000, 0.000000000000000000, 0.000000000000000000 ) ) ;
#31582 = CARTESIAN_POINT ( 'NONE',  ( -1.135663242406173001, -2.431311185535292907, 9.000000000000003553 ) ) ;
#31583 = CARTESIAN_POINT ( 'NONE',  ( -9.999952640014225125, 12.00001973332723004, 0.3289108581718978574 ) ) ;
#31584 = CARTESIAN_POINT ( 'NONE',  ( -81.95499999999998408, -7.632228543268599452, 2.479861379858951054 ) ) ;
#31585 = FILL_AREA_STYLE_COLOUR ( '', #38815 ) ;
#31587 = CYLINDRICAL_SURFACE ( 'NONE', #46152, 0.5000000000000004441 ) ;
#31586 =( GEOMETRIC_REPRESENTATION_CONTEXT ( 3 ) GLOBAL_UNCERTAINTY_ASSIGNED_CONTEXT ( ( #13599 ) ) GLOBAL_UNIT_ASSIGNED_CONTEXT ( ( #10340, #63783, #37106 ) ) REPRESENTATION_CONTEXT ( 'NONE', 'WORKASPACE' ) );
#31588 = STYLED_ITEM ( 'NONE', ( #38803 ), #27916 ) ;
#31589 = CARTESIAN_POINT ( 'NONE',  ( -74.72360438755690382, 36.39190877706418092, -9.990989611936115011 ) ) ;
#31590 = CARTESIAN_POINT ( 'NONE',  ( -90.74499999999999034, 4.716976649647094177, 6.492361379858945902 ) ) ;
#31591 = CARTESIAN_POINT ( 'NONE',  ( 3.094860106618435136, 131.4049999999999727, -9.525000000000000355 ) ) ;
#31592 = CARTESIAN_POINT ( 'NONE',  ( 74.50000000000000000, 19.30628705663858469, 6.500000000000000000 ) ) ;
#31593 = ADVANCED_FACE ( 'NONE', ( #2753 ), #55207, .T. ) ;
#31594 = DIRECTION ( 'NONE',  ( 0.000000000000000000, 0.000000000000000000, -1.000000000000000000 ) ) ;
#31595 = AXIS2_PLACEMENT_3D ( 'NONE', #9920, #36692, #58436 ) ;
#31596 = EDGE_CURVE ( 'NONE', #52352, #56993, #50640, .T. ) ;
#31597 = SHAPE_REPRESENTATION ( '3. Padlock', ( #42840 ), #60796 ) ;
#31598 = CARTESIAN_POINT ( 'NONE',  ( -1.745454270680677045, -2.292880170256994976, -7.000000000000003553 ) ) ;
#31599 = ADVANCED_FACE ( 'NONE', ( #60827 ), #8072, .F. ) ;
#31600 = ORIENTED_EDGE ( 'NONE', *, *, #12713, .T. ) ;
#31601 = AXIS2_PLACEMENT_3D ( 'NONE', #63183, #26229, #14654 ) ;
#31602 = PRODUCT_DEFINITION_SHAPE ( 'NONE', 'NONE',  #45995 ) ;
#31603 = DIRECTION ( 'NONE',  ( -1.000000000000000000, 0.000000000000000000, 0.000000000000000000 ) ) ;
#31604 = ADVANCED_FACE ( 'NONE', ( #46084 ), #34455, .T. ) ;
#31605 = AXIS2_PLACEMENT_3D ( 'NONE', #15616, #26480, #37090 ) ;
#31606 = EDGE_CURVE ( 'NONE', #59067, #53774, #14999, .T. ) ;
#31607 = DIRECTION ( 'NONE',  ( 0.000000000000000000, 0.000000000000000000, -1.000000000000000000 ) ) ;
#31608 = EDGE_CURVE ( 'NONE', #23846, #42940, #68214, .T. ) ;
#31609 = CARTESIAN_POINT ( 'NONE',  ( -131.6929263765337907, 10.01517768586948698, -1.839758294383808966E-15 ) ) ;
#31610 = ORIENTED_EDGE ( 'NONE', *, *, #31007, .T. ) ;
#31611 = ORIENTED_EDGE ( 'NONE', *, *, #45146, .F. ) ;
#31612 = CYLINDRICAL_SURFACE ( 'NONE', #10474, 18.00000000000000355 ) ;
#31614 = EDGE_CURVE ( 'NONE', #65139, #54390, #43227, .T. ) ;
#31613 = MECHANICAL_DESIGN_GEOMETRIC_PRESENTATION_REPRESENTATION (  '', ( #61943 ), #9144 ) ;
#31615 = CARTESIAN_POINT ( 'NONE',  ( -175.5570736234661808, -1.166476076187852838E-15, -9.524999999999991473 ) ) ;
#31616 = EDGE_CURVE ( 'NONE', #16451, #62857, #35908, .T. ) ;
#31617 = SURFACE_STYLE_FILL_AREA ( #57674 ) ;
#31618 = AXIS2_PLACEMENT_3D ( 'NONE', #67794, #19592, #9411 ) ;
#31619 = CARTESIAN_POINT ( 'NONE',  ( -195.0000000000000000, 0.000000000000000000, 0.000000000000000000 ) ) ;
#31620 =( NAMED_UNIT ( * ) SI_UNIT ( $, .STERADIAN. ) SOLID_ANGLE_UNIT ( ) );
#31621 = ORIENTED_EDGE ( 'NONE', *, *, #19725, .F. ) ;
#31622 = CARTESIAN_POINT ( 'NONE',  ( -122.0049999999999812, 6.826472737025115478, 4.959722759717899443 ) ) ;
#31623 = ORIENTED_EDGE ( 'NONE', *, *, #39926, .F. ) ;
#31624 = DIRECTION ( 'NONE',  ( -0.000000000000000000, -0.000000000000000000, -1.000000000000000000 ) ) ;
#31625 = CARTESIAN_POINT ( 'NONE',  ( -195.0000000000000000, 1.166476076187852838E-15, -9.524999999999991473 ) ) ;
#31626 = VERTEX_POINT ( 'NONE', #3800 ) ;
#31627 = DIRECTION ( 'NONE',  ( 0.000000000000000000, 0.000000000000000000, -1.000000000000000000 ) ) ;
#31628 = ORIENTED_EDGE ( 'NONE', *, *, #34952, .T. ) ;
#31629 = MECHANICAL_DESIGN_GEOMETRIC_PRESENTATION_REPRESENTATION (  '', ( #57495 ), #32798 ) ;
#31630 = CARTESIAN_POINT ( 'NONE',  ( -57.74999999999999289, 0.000000000000000000, -7.000000000000000000 ) ) ;
#31631 = CARTESIAN_POINT ( 'NONE',  ( 3.094860106618435136, 145.2949999999999875, -9.525000000000000355 ) ) ;
#31632 = FACE_OUTER_BOUND ( 'NONE', #9555, .T. ) ;
#31633 = ORIENTED_EDGE ( 'NONE', *, *, #62711, .F. ) ;
#31634 = COLOUR_RGB ( '', 0.09019608, 0.27058824, 0.51372549) ;
#31635 = LINE ( 'NONE', #30582, #17312 ) ;
#31636 = CARTESIAN_POINT ( 'NONE',  ( -1.166476076187854022E-15, 148.0549999999999784, 9.525000000000000355 ) ) ;
#31637 = CARTESIAN_POINT ( 'NONE',  ( -135.8070736234661808, 10.01517768586948698, -1.839758294383808966E-15 ) ) ;
#31638 = CARTESIAN_POINT ( 'NONE',  ( 32.00000000000001421, 43.00000000000000000, -36.50000000000000000 ) ) ;
#31639 = ORIENTED_EDGE ( 'NONE', *, *, #1983, .T. ) ;
#31640 = CARTESIAN_POINT ( 'NONE',  ( 6.826472737025119919, 124.8929263765338220, 4.959722759717908325 ) ) ;
#31641 = LINE ( 'NONE', #20398, #59248 ) ;
#31642 = FILL_AREA_STYLE ('',( #42948 ) ) ;
#31643 = VECTOR ( 'NONE', #4360, 1000.000000000000000 ) ;
#31644 = CARTESIAN_POINT ( 'NONE',  ( -98.84292637653379643, 9.058813317711329915, -2.943386871421373119 ) ) ;
#31645 = DIRECTION ( 'NONE',  ( 0.000000000000000000, 0.000000000000000000, -1.000000000000000000 ) ) ;
#31646 = VERTEX_POINT ( 'NONE', #57293 ) ;
#31647 = CARTESIAN_POINT ( 'NONE',  ( -40.96599324808799736, 108.0258340745533161, -3.573232801688257076 ) ) ;
#31648 = ORIENTED_EDGE ( 'NONE', *, *, #66709, .T. ) ;
#31650 = B_SPLINE_CURVE_WITH_KNOTS ( 'NONE', 3,
 ( #48199, #54111, #4893, #22118, #64330, #26673, #63976, #58042, #21775, #9848 ),
 .UNSPECIFIED., .F., .F.,
 ( 4, 2, 2, 2, 4 ),
 ( 0.000000000000000000, 0.0004159702800446777042, 0.0008319405600893554084, 0.001247910840134033167, 0.001663881120178710817 ),
 .UNSPECIFIED. ) ;
#31649 = CARTESIAN_POINT ( 'NONE',  ( -53.99292637653379501, 8.102448949553171076, -5.886773742842744461 ) ) ;
#31651 = FACE_OUTER_BOUND ( 'NONE', #51196, .T. ) ;
#31652 = CARTESIAN_POINT ( 'NONE',  ( 60.00000000000000000, 110.4999999999999858, 9.500000000000000000 ) ) ;
#31653 = CARTESIAN_POINT ( 'NONE',  ( -152.7549999999999955, 4.716976649647091513, -6.492361379858946790 ) ) ;
#31654 = CARTESIAN_POINT ( 'NONE',  ( -72.05707362346616662, 0.000000000000000000, 9.524999999999991473 ) ) ;
#31655 = CARTESIAN_POINT ( 'NONE',  ( -48.50000000000000000, 14.49137674618942562, -7.000000000000000000 ) ) ;
#31656 = EDGE_CURVE ( 'NONE', #18616, #62752, #69251, .T. ) ;
#31657 = PRESENTATION_LAYER_ASSIGNMENT (  '', '', ( #64190 ) ) ;
#31658 = SURFACE_STYLE_USAGE ( .BOTH. , #21105 ) ;
#31659 = LINE ( 'NONE', #42287, #23757 ) ;
#31660 = SURFACE_SIDE_STYLE ('',( #21451 ) ) ;
#31661 = EDGE_LOOP ( 'NONE', ( #16717, #68789, #11282, #69601 ) ) ;
#31662 = VECTOR ( 'NONE', #12501, 1000.000000000000000 ) ;
#31663 = ORIENTED_EDGE ( 'NONE', *, *, #49641, .F. ) ;
#31664 = CYLINDRICAL_SURFACE ( 'NONE', #45231, 0.2500000000000002220 ) ;
#31665 = AXIS2_PLACEMENT_3D ( 'NONE', #9978, #21916, #58163 ) ;
#31666 = CARTESIAN_POINT ( 'NONE',  ( -15.98999599679679839, 146.4999999999999716, -7.500000000000000000 ) ) ;
#31667 = CARTESIAN_POINT ( 'NONE',  ( -66.20499999999996987, -2.607480562269071545, -8.024999999999991473 ) ) ;
#31668 = VERTEX_POINT ( 'NONE', #56955 ) ;
#31669 = DIRECTION ( 'NONE',  ( 0.000000000000000000, 0.000000000000000000, -1.000000000000000000 ) ) ;
#31670 = DIRECTION ( 'NONE',  ( -1.000000000000000000, 0.000000000000000000, 0.000000000000000000 ) ) ;
#31671 =( GEOMETRIC_REPRESENTATION_CONTEXT ( 3 ) GLOBAL_UNCERTAINTY_ASSIGNED_CONTEXT ( ( #60273 ) ) GLOBAL_UNIT_ASSIGNED_CONTEXT ( ( #2943, #23400, #61378 ) ) REPRESENTATION_CONTEXT ( 'NONE', 'WORKASPACE' ) );
#31672 = FILL_AREA_STYLE ('',( #36996 ) ) ;
#31673 = CIRCLE ( 'NONE', #20433, 1.000000000000000888 ) ;
#31674 = FACE_OUTER_BOUND ( 'NONE', #66771, .T. ) ;
#31675 = ORIENTED_EDGE ( 'NONE', *, *, #16761, .T. ) ;
#31676 = CARTESIAN_POINT ( 'NONE',  ( 12.25000000000000355, 30.74999999999998579, 4.000000000000000000 ) ) ;
#31677 = DIRECTION ( 'NONE',  ( -1.000000000000000000, 0.000000000000000000, 0.000000000000000000 ) ) ;
#31678 = COLOUR_RGB ( '', 0.31764706, 0.68627451, 0.89019608) ;
#31680 = LINE ( 'NONE', #55200, #44937 ) ;
#31679 = CARTESIAN_POINT ( 'NONE',  ( -26.79538245034556709, -7.499999999999997335, 1.000000000000000000 ) ) ;
#31681 = PRESENTATION_LAYER_ASSIGNMENT (  '', '', ( #64210 ) ) ;
#31682 = EDGE_CURVE ( 'NONE', #6337, #51799, #21845, .T. ) ;
#31683 = CARTESIAN_POINT ( 'NONE',  ( -117.8949999999999676, 6.826472737025115478, 4.959722759717899443 ) ) ;
#31684 = CARTESIAN_POINT ( 'NONE',  ( 5.598654528085809545, 151.1449999999999818, -7.705886871421373741 ) ) ;
#31685 = CARTESIAN_POINT ( 'NONE',  ( -84.14499999999998181, -4.716976649647092401, 6.492361379858946790 ) ) ;
#31686 = VECTOR ( 'NONE', #34085, 1000.000000000000000 ) ;
#31687 = FACE_OUTER_BOUND ( 'NONE', #63061, .T. ) ;
#31688 = EDGE_CURVE ( 'NONE', #61072, #18963, #66776, .T. ) ;
#31689 = VECTOR ( 'NONE', #63428, 1000.000000000000000 ) ;
#31690 = FACE_OUTER_BOUND ( 'NONE', #31278, .T. ) ;
#31691 = VERTEX_POINT ( 'NONE', #31592 ) ;
#31692 = CARTESIAN_POINT ( 'NONE',  ( -131.0929263765337964, 3.094860106618433360, 9.524999999999991473 ) ) ;
#31693 = DIRECTION ( 'NONE',  ( -1.000000000000000000, 0.000000000000000000, 0.000000000000000000 ) ) ;
#31694 = CARTESIAN_POINT ( 'NONE',  ( -153.1450000000000102, -4.716976649647092401, 6.492361379858946790 ) ) ;
#31695 = DIRECTION ( 'NONE',  ( 0.000000000000000000, 0.000000000000000000, 1.000000000000000000 ) ) ;
#31696 = EDGE_CURVE ( 'NONE', #22643, #56835, #30811, .T. ) ;
#31697 =( NAMED_UNIT ( * ) SI_UNIT ( $, .STERADIAN. ) SOLID_ANGLE_UNIT ( ) );
#31698 = DIRECTION ( 'NONE',  ( 0.000000000000000000, 0.000000000000000000, 1.000000000000000000 ) ) ;
#31699 = EDGE_LOOP ( 'NONE', ( #13371, #63311, #14065, #54311 ) ) ;
#31700 = VERTEX_POINT ( 'NONE', #25616 ) ;
#31701 = AXIS2_PLACEMENT_3D ( 'NONE', #27349, #11890, #5550 ) ;
#31702 = DIRECTION ( 'NONE',  ( 1.000000000000000000, 0.000000000000000000, 0.000000000000000000 ) ) ;
#31703 = ADVANCED_FACE ( 'NONE', ( #42225 ), #20352, .F. ) ;
#31704 = LINE ( 'NONE', #53184, #60766 ) ;
#31705 = CYLINDRICAL_SURFACE ( 'NONE', #28022, 1.000000000000000888 ) ;
#31706 = AXIS2_PLACEMENT_3D ( 'NONE', #45618, #50173, #29014 ) ;
#31707 = CYLINDRICAL_SURFACE ( 'NONE', #65620, 0.2500000000000002220 ) ;
#31708 = ORIENTED_EDGE ( 'NONE', *, *, #28224, .F. ) ;
#31709 = CARTESIAN_POINT ( 'NONE',  ( -151.5550000000000068, 0.000000000000000000, 8.024999999999991473 ) ) ;
#31710 = ORIENTED_EDGE ( 'NONE', *, *, #38638, .F. ) ;
#31711 = DIRECTION ( 'NONE',  ( 1.000000000000000000, 0.000000000000000000, 0.000000000000000000 ) ) ;
#31712 =( GEOMETRIC_REPRESENTATION_CONTEXT ( 3 ) GLOBAL_UNCERTAINTY_ASSIGNED_CONTEXT ( ( #48376 ) ) GLOBAL_UNIT_ASSIGNED_CONTEXT ( ( #64071, #33456, #60508 ) ) REPRESENTATION_CONTEXT ( 'NONE', 'WORKASPACE' ) );
#31713 = ORIENTED_EDGE ( 'NONE', *, *, #32247, .F. ) ;
#31714 = PRESENTATION_LAYER_ASSIGNMENT (  '', '', ( #27171 ) ) ;
#31715 = DIRECTION ( 'NONE',  ( 1.000000000000000000, -6.162975822039156098E-33, -1.300977106640435137E-16 ) ) ;
#31716 = CARTESIAN_POINT ( 'NONE',  ( -8.102448949553181734, 122.4949999999999903, 5.886773742842747126 ) ) ;
#31717 = CARTESIAN_POINT ( 'NONE',  ( 75.00000000000000000, 20.36037961002804053, 6.000000000000000888 ) ) ;
#31718 = STYLED_ITEM ( 'NONE', ( #48737 ), #54644 ) ;
#31719 = EDGE_LOOP ( 'NONE', ( #2801, #6193, #46115, #10068 ) ) ;
#31720 = CARTESIAN_POINT ( 'NONE',  ( -1.166476076187854022E-15, 124.0549999999999784, 9.525000000000000355 ) ) ;
#31721 = CARTESIAN_POINT ( 'NONE',  ( -64.25499999999998124, -4.716976649647092401, 6.492361379858946790 ) ) ;
#31722 = CARTESIAN_POINT ( 'NONE',  ( -40.78947371891996454, 108.1536491252650052, -3.151596837137513596 ) ) ;
#31723 = ORIENTED_EDGE ( 'NONE', *, *, #4048, .T. ) ;
#31724 = CARTESIAN_POINT ( 'NONE',  ( -5.598654528085806881, 146.8549999999999898, -7.705886871421374629 ) ) ;
#31725 = LINE ( 'NONE', #52866, #60224 ) ;
#31726 = CARTESIAN_POINT ( 'NONE',  ( 60.00000000000000000, 1.797044900979284448E-15, -10.00000000000000000 ) ) ;
#31727 = STYLED_ITEM ( 'NONE', ( #11503 ), #19120 ) ;
#31728 = CARTESIAN_POINT ( 'NONE',  ( 18.00000000000000711, 31.24999999999999289, -3.750000000000000000 ) ) ;
#31729 = ORIENTED_EDGE ( 'NONE', *, *, #28707, .T. ) ;
#31730 = CARTESIAN_POINT ( 'NONE',  ( -79.99999999999998579, 50.00000000000000000, 11.50000000000003730 ) ) ;
#31731 = CARTESIAN_POINT ( 'NONE',  ( 74.59262096826685706, 19.64589727361707361, -6.500000000000001776 ) ) ;
#31732 = CARTESIAN_POINT ( 'NONE',  ( -180.9550000000000125, -7.632228543268599452, 2.479861379858951054 ) ) ;
#31733 = VERTEX_POINT ( 'NONE', #36597 ) ;
#31734 = DIRECTION ( 'NONE',  ( 0.000000000000000000, 0.000000000000000000, 1.000000000000000000 ) ) ;
#31735 = EDGE_CURVE ( 'NONE', #5084, #32321, #2701, .T. ) ;
#31736 = CARTESIAN_POINT ( 'NONE',  ( 33.00000000000002132, 15.00000000000000000, 79.00402776293826435 ) ) ;
#31737 = ORIENTED_EDGE ( 'NONE', *, *, #52172, .T. ) ;
#31738 = CARTESIAN_POINT ( 'NONE',  ( 33.00000000000002132, 14.00000000000000000, 80.00402776293826435 ) ) ;
#31739 = EDGE_LOOP ( 'NONE', ( #61985, #38545, #8820, #50527 ) ) ;
#31740 =( NAMED_UNIT ( * ) PLANE_ANGLE_UNIT ( ) SI_UNIT ( $, .RADIAN. ) );
#31741 = CARTESIAN_POINT ( 'NONE',  ( -91.25499999999999545, -4.716976649647092401, 6.492361379858946790 ) ) ;
#31742 = ORIENTED_EDGE ( 'NONE', *, *, #28726, .F. ) ;
#31743 = CARTESIAN_POINT ( 'NONE',  ( 0.000000000000000000, 2.500000000000000000, 0.000000000000000000 ) ) ;
#31744 = SURFACE_STYLE_USAGE ( .BOTH. , #42372 ) ;
#31745 = CARTESIAN_POINT ( 'NONE',  ( -129.9570736234661865, 9.058813317711329915, -2.943386871421373119 ) ) ;
#31746 = DIRECTION ( 'NONE',  ( 0.000000000000000000, 1.000000000000000000, 0.000000000000000000 ) ) ;
#31747 = CARTESIAN_POINT ( 'NONE',  ( 8.102448949553179958, 150.3949999999999818, 5.886773742842750679 ) ) ;
#31748 = CARTESIAN_POINT ( 'NONE',  ( -61.25707362346617657, 5.598654528085800663, -7.705886871421367523 ) ) ;
#31749 = COLOUR_RGB ( '', 0.40784314, 0.44705882, 0.49803922) ;
#31750 = ORIENTED_EDGE ( 'NONE', *, *, #9965, .T. ) ;
#31751 =( NAMED_UNIT ( * ) SI_UNIT ( $, .STERADIAN. ) SOLID_ANGLE_UNIT ( ) );
#31753 = DIRECTION ( 'NONE',  ( 0.000000000000000000, 1.000000000000000000, 0.000000000000000000 ) ) ;
#31752 = CONICAL_SURFACE ( 'NONE', #10435, 5.000000000000000000, 0.7853981633974482790 ) ;
#31755 = CARTESIAN_POINT ( 'NONE',  ( 31.00000000000000711, -60.04052944165106709, -35.50000000000000000 ) ) ;
#31754 = CARTESIAN_POINT ( 'NONE',  ( 10.00000000000001954, 42.00000000000000000, 28.38386403503541899 ) ) ;
#31756 = EDGE_CURVE ( 'NONE', #24967, #17136, #60037, .T. ) ;
#31757 = CARTESIAN_POINT ( 'NONE',  ( -109.1050000000000040, -6.826472737025115478, 4.959722759717900331 ) ) ;
#31758 = CLOSED_SHELL ( 'NONE', ( #59640, #47581, #24240, #2964, #3225, #47716, #4762, #2480, #7089, #62650, #47566, #7154, #6421, #27297, #8044, #15558, #53148, #44541, #18597, #21435, #52130, #14752, #5378, #12550, #22808, #53749, #67584, #62498, #20672, #44415, #42931, #37413, #20512, #61608, #46195, #10910, #61514, #31043, #25449, #41324, #17674, #12127, #30912, #31593, #23119, #63843, #45420, #64739, #58940, #20431, #36016, #31196, #45667, #6184, #18491, #6414, #34795, #2463, #7064, #4045, #22178, #44706, #20093, #67605, #13341, #68306, #53785, #48812, #63694, #43412, #29540, #10169, #46002, #17696, #38867, #23504, #54436, #68714, #72, #21601, #63612, #38738, #54250, #49057, #63453, #55835, #720, #9444, #30986, #49531, #45724, #58229, #48658, #50025, #22212, #5787, #55304, #38081, #54141, #8439, #44623, #35933, #40218, #33502, #48901, #1538, #41180, #31328, #7310, #44546, #63301, #69428, #30013, #34634, #28315, #10505, #15056, #54087, #9147, #15674, #15144, #27758, #66071, #37469, #30009, #63284, #51705, #3548, #6028, #43745, #741, #49421, #65523, #26238, #65920, #13675, #32908, #27173, #28556, #24811, #39769, #58871, #44672, #29281, #48027, #28844, #10974, #27550, #63553, #26804, #28564, #22246, #23957, #1393, #28565, #21931, #52674, #29105, #47558, #22893, #30331, #58111, #62091, #51871, #30317, #8450, #66154, #51170, #26127, #3278, #11265, #53423, #43136, #60902, #37834, #40985, #36915, #11835, #56733, #64886, #39855, #44899, #46338, #61006, #7094, #2012, #20629, #69023, #31502, #13347, #1401, #64405, #38430, #69536, #4849, #40937, #15414, #39181, #56528, #22317, #16883, #21407, #53251, #47794, #37296, #31133 ) ) ;
#31759 = EDGE_CURVE ( 'NONE', #32017, #41477, #69052, .T. ) ;
#31760 = CARTESIAN_POINT ( 'NONE',  ( -3.094860106618434248, 116.7949999999999591, 9.525000000000000355 ) ) ;
#31761 = AXIS2_PLACEMENT_3D ( 'NONE', #920, #22471, #43967 ) ;
#31762 = CARTESIAN_POINT ( 'NONE',  ( -116.2449999999999903, -4.716976649647093289, -6.492361379858945902 ) ) ;
#31763 = CONICAL_SURFACE ( 'NONE', #2491, 7.000000000000000888, 0.7853981633974500554 ) ;
#31764 = CARTESIAN_POINT ( 'NONE',  ( 3.046771365092978190, 72.00000000000001421, 12.50000000000000000 ) ) ;
#31765 = EDGE_CURVE ( 'NONE', #22278, #30219, #24934, .T. ) ;
#31766 = VECTOR ( 'NONE', #27125, 1000.000000000000000 ) ;
#31767 = CARTESIAN_POINT ( 'NONE',  ( -117.7429263765338021, -5.598654528085803328, -7.705886871421366635 ) ) ;
#31768 = EDGE_CURVE ( 'NONE', #66883, #38684, #9125, .T. ) ;
#31769 = ORIENTED_EDGE ( 'NONE', *, *, #33550, .F. ) ;
#31770 = CARTESIAN_POINT ( 'NONE',  ( -159.8929263765337794, -8.102448949553172852, -5.886773742842741797 ) ) ;
#31771 =( LENGTH_UNIT ( ) NAMED_UNIT ( * ) SI_UNIT ( .MILLI., .METRE. ) );
#31772 = DIRECTION ( 'NONE',  ( 0.000000000000000000, -0.000000000000000000, 1.000000000000000000 ) ) ;
#31773 = EDGE_CURVE ( 'NONE', #65192, #39245, #28019, .T. ) ;
#31774 = MECHANICAL_DESIGN_GEOMETRIC_PRESENTATION_REPRESENTATION (  '', ( #30614 ), #16093 ) ;
#31775 = AXIS2_PLACEMENT_3D ( 'NONE', #59793, #28092, #61175 ) ;
#31776 = DIRECTION ( 'NONE',  ( 1.000000000000000000, 0.000000000000000000, 0.000000000000000000 ) ) ;
#31777 = EDGE_CURVE ( 'NONE', #33694, #37046, #35404, .T. ) ;
#31778 = DIRECTION ( 'NONE',  ( 0.000000000000000000, 1.000000000000000000, -0.000000000000000000 ) ) ;
#31779 = LINE ( 'NONE', #69091, #21142 ) ;
#31780 = DIRECTION ( 'NONE',  ( 0.000000000000000000, 0.000000000000000000, 1.000000000000000000 ) ) ;
#31781 = ORIENTED_EDGE ( 'NONE', *, *, #54570, .F. ) ;
#31782 = CARTESIAN_POINT ( 'NONE',  ( -74.84292637653381064, 9.058813317711329915, -2.943386871421373119 ) ) ;
#31783 = ITEM_DEFINED_TRANSFORMATION ( 'NONE', 'NONE', #38312,  #42840 ) ;
#31784 = DIRECTION ( 'NONE',  ( -1.000000000000000000, -9.811390859391773608E-17, 0.000000000000000000 ) ) ;
#31785 = CARTESIAN_POINT ( 'NONE',  ( -166.1929263765337907, -10.01517768586948698, 6.132527647946031529E-16 ) ) ;
#31786 = COLOUR_RGB ( '', 0.72549020, 0.75294118, 0.79215686) ;
#31787 = EDGE_CURVE ( 'NONE', #33115, #42499, #42626, .T. ) ;
#31788 =( NAMED_UNIT ( * ) SI_UNIT ( $, .STERADIAN. ) SOLID_ANGLE_UNIT ( ) );
#31789 = CARTESIAN_POINT ( 'NONE',  ( -60.00000000000000000, -2.024042244987997205E-14, -10.49999999999999822 ) ) ;
#31790 = CARTESIAN_POINT ( 'NONE',  ( 3.249999999999998668, 36.74999999999999289, 4.000000000000000000 ) ) ;
#31791 = CARTESIAN_POINT ( 'NONE',  ( -179.1550000000000011, 7.632228543268600340, 2.479861379858949277 ) ) ;
#31792 = VERTEX_POINT ( 'NONE', #65341 ) ;
#31793 = DIRECTION ( 'NONE',  ( 1.000000000000000000, 0.000000000000000000, 0.000000000000000000 ) ) ;
#31794 = COLOUR_RGB ( '', 0.72549020, 0.75294118, 0.79215686) ;
#31795 = COLOUR_RGB ( '', 0.09019608, 0.27058824, 0.51372549) ;
#31796 = CARTESIAN_POINT ( 'NONE',  ( -182.6070736234661638, -8.102448949553174629, 5.886773742842742685 ) ) ;
#31797 = CARTESIAN_POINT ( 'NONE',  ( 2.607480562269076430, 144.9070736234661751, -8.025000000000000355 ) ) ;
#31798 = AXIS2_PLACEMENT_3D ( 'NONE', #67457, #40761, #67120 ) ;
#31799 = ORIENTED_EDGE ( 'NONE', *, *, #30509, .T. ) ;
#31800 = DIRECTION ( 'NONE',  ( 1.000000000000000000, 0.000000000000000000, -0.000000000000000000 ) ) ;
#31801 = CARTESIAN_POINT ( 'NONE',  ( -97.25499999999999545, -4.716976649647092401, 6.492361379858946790 ) ) ;
#31802 = CARTESIAN_POINT ( 'NONE',  ( -83.49999999999998579, -2.499999999999999556, 0.000000000000000000 ) ) ;
#31803 = ORIENTED_EDGE ( 'NONE', *, *, #39826, .F. ) ;
#31804 = CARTESIAN_POINT ( 'NONE',  ( 4.793834890952473948, -1.308853920463818987, -9.000000000000007105 ) ) ;
#31805 = SURFACE_STYLE_FILL_AREA ( #57875 ) ;
#31806 = CARTESIAN_POINT ( 'NONE',  ( -76.16421356237310647, 3.244476573706588632E-16, 19.41421356237309581 ) ) ;
#31807 = ORIENTED_EDGE ( 'NONE', *, *, #35025, .F. ) ;
#31808 = AXIS2_PLACEMENT_3D ( 'NONE', #44341, #17584, #27039 ) ;
#31809 = DIRECTION ( 'NONE',  ( -0.000000000000000000, -0.000000000000000000, -1.000000000000000000 ) ) ;
#31810 = CARTESIAN_POINT ( 'NONE',  ( -71.84499999999999886, -7.632228543268599452, 2.479861379858951054 ) ) ;
#31811 = ORIENTED_EDGE ( 'NONE', *, *, #54927, .T. ) ;
#31812 = DIRECTION ( 'NONE',  ( -1.000000000000000000, 0.000000000000000000, 0.000000000000000000 ) ) ;
#31813 = CARTESIAN_POINT ( 'NONE',  ( -121.2570736234661695, 5.598654528085800663, -7.705886871421367523 ) ) ;
#31814 = CIRCLE ( 'NONE', #5958, 9.525000000000000355 ) ;
#31815 = ORIENTED_EDGE ( 'NONE', *, *, #17446, .T. ) ;
#31816 = DIRECTION ( 'NONE',  ( -1.000000000000000000, 0.000000000000000000, 0.000000000000000000 ) ) ;
#31817 = DIRECTION ( 'NONE',  ( -0.000000000000000000, -0.000000000000000000, -1.000000000000000000 ) ) ;
#31818 = CIRCLE ( 'NONE', #21740, 1.000000000000000888 ) ;
#31819 = PRESENTATION_LAYER_ASSIGNMENT (  '', '', ( #43086 ) ) ;
#31820 = CARTESIAN_POINT ( 'NONE',  ( 4.000000000000002665, 43.00000000000000000, 0.000000000000000000 ) ) ;
#31821 = EDGE_LOOP ( 'NONE', ( #60932, #55859, #18710, #44440, #58224, #31094 ) ) ;
#31822 = CARTESIAN_POINT ( 'NONE',  ( -40.49999999999998579, 107.7459666924148394, 3.000000000000000000 ) ) ;
#31823 = ORIENTED_EDGE ( 'NONE', *, *, #6847, .F. ) ;
#31824 = DIRECTION ( 'NONE',  ( 0.000000000000000000, 1.000000000000000000, 0.000000000000000000 ) ) ;
#31825 = LINE ( 'NONE', #63161, #31076 ) ;
#31826 = CARTESIAN_POINT ( 'NONE',  ( -156.0570736234661808, 0.000000000000000000, 9.524999999999991473 ) ) ;
#31827 = CARTESIAN_POINT ( 'NONE',  ( -8.102448949553179958, 124.8949999999999960, -5.886773742842749790 ) ) ;
#31828 = CARTESIAN_POINT ( 'NONE',  ( -92.90707362346614673, -3.094860106618429807, 9.524999999999991473 ) ) ;
#31829 = CIRCLE ( 'NONE', #342, 8.999999999999994671 ) ;
#31830 = ADVANCED_FACE ( 'NONE', ( #64661 ), #36546, .T. ) ;
#31831 = DIRECTION ( 'NONE',  ( 0.000000000000000000, 0.000000000000000000, 1.000000000000000000 ) ) ;
#31832 = ORIENTED_EDGE ( 'NONE', *, *, #66785, .F. ) ;
#31833 =( LENGTH_UNIT ( ) NAMED_UNIT ( * ) SI_UNIT ( .MILLI., .METRE. ) );
#31834 = EDGE_CURVE ( 'NONE', #24001, #56480, #42667, .T. ) ;
#31836 = FILL_AREA_STYLE ('',( #48417 ) ) ;
#31835 = DIRECTION ( 'NONE',  ( 0.000000000000000000, 0.000000000000000000, 1.000000000000000000 ) ) ;
#31837 = ADVANCED_FACE ( 'NONE', ( #26983 ), #16505, .F. ) ;
#31838 = PRESENTATION_LAYER_ASSIGNMENT (  '', '', ( #26369 ) ) ;
#31839 = CARTESIAN_POINT ( 'NONE',  ( -139.5549999999999784, 0.000000000000000000, 8.024999999999991473 ) ) ;
#31840 = CARTESIAN_POINT ( 'NONE',  ( 179.4361977533490347, 14.00000000000000000, -103.7004518695263044 ) ) ;
#31841 = CARTESIAN_POINT ( 'NONE',  ( 3.000000000000002665, 35.42594141563417054, -80.00402776293826435 ) ) ;
#31842 = CARTESIAN_POINT ( 'NONE',  ( -154.9449999999999932, -9.827790563157499189E-16, -8.024999999999991473 ) ) ;
#31843 = COLOUR_RGB ( '', 0.08235294, 0.09019608, 0.10196078) ;
#31844 = AXIS2_PLACEMENT_3D ( 'NONE', #21409, #10530, #54106 ) ;
#31845 = CARTESIAN_POINT ( 'NONE',  ( -143.2449999999999761, -4.716976649647093289, -6.492361379858945902 ) ) ;
#31846 = VERTEX_POINT ( 'NONE', #38308 ) ;
#31847 = CARTESIAN_POINT ( 'NONE',  ( -180.9570736234661865, 9.058813317711329915, -2.943386871421373119 ) ) ;
#31848 = MECHANICAL_DESIGN_GEOMETRIC_PRESENTATION_REPRESENTATION (  '', ( #9383 ), #18370 ) ;
#31849 = SURFACE_STYLE_FILL_AREA ( #57919 ) ;
#31850 = SURFACE_STYLE_FILL_AREA ( #53337 ) ;
#31851 = UNCERTAINTY_MEASURE_WITH_UNIT (LENGTH_MEASURE( 1.000000000000000082E-05 ), #24899, 'distance_accuracy_value', 'NONE');
#31852 = CARTESIAN_POINT ( 'NONE',  ( -58.70499999999997698, 2.607480562269073321, 8.024999999999991473 ) ) ;
#31853 = DIRECTION ( 'NONE',  ( -0.000000000000000000, -0.000000000000000000, 1.000000000000000000 ) ) ;
#31854 = ADVANCED_FACE ( 'NONE', ( #64300, #11526, #5202 ), #26647, .F. ) ;
#31855 =( NAMED_UNIT ( * ) SI_UNIT ( $, .STERADIAN. ) SOLID_ANGLE_UNIT ( ) );
#31856 = DIRECTION ( 'NONE',  ( -1.000000000000000000, 0.000000000000000000, 0.000000000000000000 ) ) ;
#31857 = MECHANICAL_DESIGN_GEOMETRIC_PRESENTATION_REPRESENTATION (  '', ( #57688 ), #321 ) ;
#31858 =( NAMED_UNIT ( * ) PLANE_ANGLE_UNIT ( ) SI_UNIT ( $, .RADIAN. ) );
#31859 = UNCERTAINTY_MEASURE_WITH_UNIT (LENGTH_MEASURE( 1.000000000000000082E-05 ), #19404, 'distance_accuracy_value', 'NONE');
#31860 = DIRECTION ( 'NONE',  ( -1.387778780781445676E-16, 0.9591247405308765961, 0.2829836251474255882 ) ) ;
#31861 = MECHANICAL_DESIGN_GEOMETRIC_PRESENTATION_REPRESENTATION (  '', ( #27265 ), #22903 ) ;
#31862 = PRESENTATION_STYLE_ASSIGNMENT (( #21660 ) ) ;
#31863 = DIRECTION ( 'NONE',  ( -0.000000000000000000, 0.000000000000000000, -1.000000000000000000 ) ) ;
#31864 =( NAMED_UNIT ( * ) PLANE_ANGLE_UNIT ( ) SI_UNIT ( $, .RADIAN. ) );
#31865 = VECTOR ( 'NONE', #43973, 1000.000000000000000 ) ;
#31866 = AXIS2_PLACEMENT_3D ( 'NONE', #68839, #20637, #20278 ) ;
#31867 = CARTESIAN_POINT ( 'NONE',  ( -23.21231517720797655, 117.4999999999999716, 10.00000000000000000 ) ) ;
#31868 = EDGE_CURVE ( 'NONE', #54091, #33883, #52243, .T. ) ;
#31869 = DIRECTION ( 'NONE',  ( 1.000000000000000000, 0.000000000000000000, 0.000000000000000000 ) ) ;
#31870 = FACE_OUTER_BOUND ( 'NONE', #9162, .T. ) ;
#31871 = VERTEX_POINT ( 'NONE', #13247 ) ;
#31872 = DIRECTION ( 'NONE',  ( 0.000000000000000000, -0.6691306063588591257, -0.7431448254773933559 ) ) ;
#31873 = EDGE_CURVE ( 'NONE', #4798, #30297, #66371, .T. ) ;
#31874 = CARTESIAN_POINT ( 'NONE',  ( -2.607480562269073765, 118.2070736234661439, -8.025000000000000355 ) ) ;
#31875 = VECTOR ( 'NONE', #36825, 1000.000000000000000 ) ;
#31876 = AXIS2_PLACEMENT_3D ( 'NONE', #56036, #8573, #56760 ) ;
#31877 = CARTESIAN_POINT ( 'NONE',  ( -46.64499999999998892, 4.716976649647091513, -6.492361379858946790 ) ) ;
#31878 = PRESENTATION_STYLE_ASSIGNMENT (( #21319 ) ) ;
#31879 = CARTESIAN_POINT ( 'NONE',  ( -24.00000000000000000, 1.000000000000000000, 3.000000000000000000 ) ) ;
#31880 = ORIENTED_EDGE ( 'NONE', *, *, #28702, .T. ) ;
#31881 = ORIENTED_EDGE ( 'NONE', *, *, #10585, .T. ) ;
#31882 = CARTESIAN_POINT ( 'NONE',  ( -8.082903768654762899, 3.516382302766490365E-15, 7.500000000000000000 ) ) ;
#31883 = DIRECTION ( 'NONE',  ( -0.5000000000000001110, -0.8660254037844384856, 0.000000000000000000 ) ) ;
#31884 = AXIS2_PLACEMENT_3D ( 'NONE', #5171, #48139, #69546 ) ;
#31885 = CARTESIAN_POINT ( 'NONE',  ( -20.88896767935282739, 150.0000000000000284, 9.626543325103073201 ) ) ;
#31886 = ORIENTED_EDGE ( 'NONE', *, *, #51616, .T. ) ;
#31887 = CARTESIAN_POINT ( 'NONE',  ( -8.102448949553181734, 123.6049999999999756, 5.886773742842747126 ) ) ;
#31888 = CARTESIAN_POINT ( 'NONE',  ( -85.34292637653381064, -9.058813317711329915, 2.943386871421371787 ) ) ;
#31889 = MECHANICAL_DESIGN_GEOMETRIC_PRESENTATION_REPRESENTATION (  '', ( #57729 ), #63342 ) ;
#31890 = PRESENTATION_LAYER_ASSIGNMENT (  '', '', ( #62224 ) ) ;
#31891 = CARTESIAN_POINT ( 'NONE',  ( 179.4361977533490347, 13.00000000000000178, -103.7004518695263044 ) ) ;
#31892 = CARTESIAN_POINT ( 'NONE',  ( -100.0450000000000017, 7.632228543268600340, 2.479861379858949277 ) ) ;
#31893 = ORIENTED_EDGE ( 'NONE', *, *, #27051, .T. ) ;
#31894 =( NAMED_UNIT ( * ) PLANE_ANGLE_UNIT ( ) SI_UNIT ( $, .RADIAN. ) );
#31895 = FILL_AREA_STYLE_COLOUR ( '', #53077 ) ;
#31896 = FILL_AREA_STYLE ('',( #47444 ) ) ;
#31897 = EDGE_LOOP ( 'NONE', ( #21548, #57322, #12364, #8708, #3092, #54894, #2695, #23211 ) ) ;
#31898 = CARTESIAN_POINT ( 'NONE',  ( 2.607480562269071989, 157.5929263765338249, 8.025000000000002132 ) ) ;
#31899 = CARTESIAN_POINT ( 'NONE',  ( 0.000000000000000000, 114.9999999999999574, 0.000000000000000000 ) ) ;
#31900 = PRESENTATION_STYLE_ASSIGNMENT (( #27293 ) ) ;
#31901 = AXIS2_PLACEMENT_3D ( 'NONE', #54948, #38843, #12051 ) ;
#31902 = EDGE_CURVE ( 'NONE', #29357, #43960, #37650, .T. ) ;
#31903 = LINE ( 'NONE', #42185, #4900 ) ;
#31904 = ORIENTED_EDGE ( 'NONE', *, *, #18853, .T. ) ;
#31905 = CARTESIAN_POINT ( 'NONE',  ( -19.89974874213239886, 114.9999999999999574, 10.49999999999999645 ) ) ;
#31906 = CYLINDRICAL_SURFACE ( 'NONE', #69210, 7.999999999999992895 ) ;
#31907 = VECTOR ( 'NONE', #32588, 1000.000000000000000 ) ;
#31908 = PRESENTATION_STYLE_ASSIGNMENT (( #10475 ) ) ;
#31909 =( BOUNDED_SURFACE ( )  B_SPLINE_SURFACE ( 1, 2, ( 
 ( #38630, #49160, #60032, #34345, #11844, #18161, #22757, #44254, #33314, #60708, #55794, #17502, #12521, #55450, #61401, #65658, #55083, #50533, #29032, #38975, #17826, #66342, #857, #28340, #33988, #7272, #40008, #60372, #13216, #50188, #27989, #28698, #56128, #12172, #22400, #33644, #7953, #7602, #49843, #23108, #34673, #1913, #1582, #23427, #65999, #65313, #44938, #54735, #39646, #61065, #12880, #17158, #2254, #23781, #45286, #66704, #18520, #6541, #35396, #13564, #41042, #14631, #67389, #62456, #35738, #41737, #51223, #56847, #30787, #9361, #29761, #67745, #46691, #29397, #8658, #19544, #14275, #20235, #45962, #63162, #30419, #8320, #57172, #36474, #24458, #2632, #2969, #57896, #36093, #19180, #3319, #14998, #9007, #40686, #51922, #62100, #50873, #3678, #35034, #25175, #19884, #24805, #24129, #57535, #52286, #30088, #68108, #4044, #41384, #51560, #45637, #46325, #62790, #13928, #25511, #47024, #68439, #67056, #18839, #40328, #61738, #56485, #9717, #27219, #43142, #21625, #48759, #52626, #11062, #42110, #58928, #26867, #63505, #26205, #64877, #48405, #5422, #95, #64552, #53316, #15357, #16393, #69141, #16730, #59238, #37868, #38194, #10738, #32186, #25858, #32508, #36811, #37162, #58570, #5773, #63834, #53637, #461, #10402, #58228, #21991, #20594, #47368, #31128, #53972, #5100, #10050, #43494, #4378, #26548, #68803, #69472, #31476, #52961, #64186, #4750, #47747, #20947, #42444, #15679, #31826, #48068, #21261, #42797, #16043, #37521, #54670, #7193, #65576, #2173, #54999, #28619, #49418, #1845, #1498, #17426, #44177, #59596, #32887, #50118, #38892, #11414, #7527, #23355, #44857, #28954, #54323, #60980, #22323, #39227, #66261, #43819, #6471, #45204, #18088, #55369, #39574, #12799, #33567, #65228, #34265, #1140, #66625, #55721, #50444, #18443, #60627, #12441, #6147, #23704, #17076, #60299, #12100, #27577, #6827, #33903, #49095, #28250, #38555, #780, #59948, #11766, #33231, #27906, #49762, #22675, #23027, #44523, #65926, #17756, #30016, #18774, #61331, #24725, #40965, #3967, #50794, #62705, #29315, #39928, #2544, #25097, #24053, #8919, #40252, #34956, #45561, #51479, #46610, #8237, #3237, #46243, #52204, #61654, #45881, #41303, #19816, #13484, #8582, #57097, #13141, #19101, #67663, #19462, #30697, #56402, #25439, #62383, #29680, #14202, #46950, #51149, #34596, #2897, #68361, #68029, #24385, #13848, #56051, #35659, #67311, #30340, #40605, #7866, #51845, #66981, #3592, #14532, #35312, #62019, #36011, #57455, #56769, #9278, #42709, #42373, #21551, #20514, #63072, #68718, #43062, #64108, #42022, #26122, #48322, #58493, #63430, #63757, #15275, #17, #20870, #52549, #5021, #48000, #47658, #20144, #15963, #37443, #4670, #37081, #58841, #69400, #31390, #41654, #15609, #10656, #9973, #32112, #10320, #69064, #52887, #14912, #57812, #53564, #31745, #36395, #9638, #5350, #26792, #31056, #47289, #4294, #36742, #25776, #58158, #53233, #26474, #21190, #52075, #9157, #3830, #46836, #56980, #45767, #25314, #3104, #68585, #62933, #68241, #41883, #62590, #35875, #29549, #20023, #67185, #40834, #62253, #9512, #67534, #14404, #30930, #14079, #40481, #25646, #24271, #51020, #34821, #41520, #8794, #18975, #14779, #47166, #30221, #52428, #3465, #61900, #56276, #67899, #57321, #20382, #13721, #36258, #2781, #13362, #35179, #57682, #56640, #4173, #8466, #29903, #51361, #24962, #8104, #24598, #46472, #19691, #46114, #19335, #35542, #51713, #41189, #30574, #40691, #61067, #2972, #18523, #56488, #67392, #50191, #1917, #50876, #23785, #23432, #55797, #61404, #61742, #24133, #12885, #19184, #2258, #45640, #66345, #18841, #40011, #34348, #7604, #6915, #49847, #67059, #29036, #28343, #24461, #40332, #13569, #45966, #1586, #8323, #39308, #56132, #35037, #60712, #44941, #62104, #29765, #2635, #51226, #13931, #50536, #12526, #35400, #18165, #23111, #44606, #66003, #17829, #7957, #29401, #33991, #55453, #7276, #45289, #66706, #28701, #13219, #39650, #34678, #14634, #14277, #69144, #67749, #24810, #8661, #20596, #30789, #19548, #42112, #20949, #52289, #52964, #47027, #35741, #30090, #41740, #57899, #42446, #41046, #10055, #46329, #56850, #62460, #63508, #57176, #25861, #9009, #51925, #30423, #68442, #15359, #25178, #20238, #63165, #63837, #3680, #62793, #58231, #52628, #46694, #9364, #68110, #51564, #36096, #25513, #15002, #47749, #19888, #15683, #9720, #41386, #36476, #3323, #57538, #4047, #31131, #4383, #36814, #47370, #68805, #31480, #4752, #26207, #464, #5424, #22677, #5777, #42801, #32892, #27581, #11064, #1143, #22326, #43823, #6149, #54327, #32188, #59241, #11770, #32511, #54673, #33234, #69474, #38197, #17079, #16732, #26550, #37523, #65579, #37870, #10741, #43496, #53975, #37165, #65230, #44180, #782, #64554, #38558, #53639, #58574, #43145, #27223, #48761, #31828, #58930, #21994, #99, #49097, #26871, #27908, #59599, #10405, #64880, #53318, #6474, #48409, #59953, #21629, #16396, #11417, #5103, #49420, #48071, #21265, #64189, #16046, #13488, #40255, #17759, #60983, #18777, #2901, #50799, #65930, #18446, #66629, #8242, #28624, #23709, #33570, #44527, #1848, #44860, #56406, #38896, #23031, #29684, #66985, #39931, #49765, #66266, #51153, #23359, #34960, #28957, #61657, #24388, #60630, #12445, #61335, #34269, #33907, #55374, #45885, #17430, #50448, #13144, #2548, #55003, #60301, #2177, #45208, #12104, #55725, #7196, #39578, #39231, #50121, #6831, #24057, #28254, #1503, #18092, #29319, #12802, #7530, #34599, #56054, #7870, #45564, #51848, #9281, #14204, #19466, #67314, #19103, #56773, #41306, #68363, #30344, #35662, #62388, #40609, #40969, #4673, #52552, #57100, #62707, #9976, #25442, #8921, #30699, #3595, #52890, #36014, #3240, #63076, #57814, #14537, #31396, #4298, #25781, #46612, #52207, #47293, #14915, #25100, #26126, #57458, #36399, #68033, #9641, #3971, #19819, #46954, #62023, #13852, #31058, #20148, #35317, #15279, #68721, #20518, #36745, #8586, #42026, #30019, #41658, #63432, #51483, #58160, #24728, #46246, #67666, #21192, #53896, #43067, #6401, #32803, #54596, #11337, #5352, #27500, #64112, #47662, #53567, #48327, #21553, #42375, #69403, #37793, #10659, #43422, #48002, #38480, #48681, #69067, #64470, #11689, #65145, #58846, #38122, #42714, #26794, #27149, #33159, #19, #20873, #15966, #59516, #43743, #16990, #715, #37447, #16314, #49025, #63761, #54244, #26477, #383, #21910, #59874, #32114, #5698, #15612, #5024, #59167, #10994, #37086, #58497, #53236, #10322, #22245, #64808, #31748, #32433, #16652, #6063, #24912, #40432, #8752, #19647, #2363, #23883, #3064, #45732, #45392, #66815, #8055, #13674, #14032, #46069, #34776, #41143, #24227, #67486, #18625, #40789, #61847, #56230, #13316, #27831, #1056, #19283, #29507, #49334, #46429, #62207, #35492, #67852, #22599, #30179, #60229, #8418, #56939, #12032, #67145, #17352, #35136, #62546, #51666, #3419, #2734, #33489, #14363, #40103, #35832, #57278, #44102, #65500, #29853, #51319, #38814, #54918, #6745, #50972, #18934, #29135, #56589, #24555, #50626, #61493, #36209, #21367, #19975, #46793, #30525, #42533, #52715, #41474, #63931, #42893, #4483, #5189, #68899, #57637, #52027, #63600, #10144, #64286, #62889, #31931, #68197, #9110, #14735, #15780, #9459, #47841, #30886, #4134, #52384, #20699, #37263, #47117, #42210 ),
 ( #25601, #25951, #16138, #36908, #68540, #15445, #20339, #37616, #47476, #41842, #4852, #69238, #58321, #3783, #58663, #10493, #63258, #31577, #15106, #53059, #26632, #21034, #53409, #26299, #36579, #48155, #57998, #25270, #69564, #9811, #31221, #38647, #11862, #5515, #28004, #21727, #16822, #38294, #55103, #43578, #60048, #6930, #59694, #16494, #1599, #202, #26967, #10831, #22773, #32983, #43241, #44272, #23127, #54418, #28354, #49175, #37958, #32274, #43918, #33327, #44617, #64646, #12188, #48503, #59018, #59332, #65671, #11161, #49515, #32606, #54072, #5877, #875, #17517, #27321, #22415, #65329, #66014, #48853, #64969, #60383, #54748, #550, #11512, #22078, #53723, #6238, #27666, #17173, #49861, #6558, #17841, #1243, #38992, #33660, #46342, #34362, #12542, #12897, #67761, #24474, #55811, #13231, #51577, #67071, #7615, #2648, #29050, #24825, #7971, #44951, #35052, #29778, #34689, #3334, #45977, #67403, #18538, #24144, #19198, #56499, #45301, #39320, #56143, #8333, #50548, #51239, #50887, #66722, #23801, #60723, #34005, #2984, #40025, #55465, #56862, #40706, #62117, #8677, #7289, #13944, #1926, #18849, #35412, #61414, #29417, #45652, #28716, #61083, #40344, #2271, #30103, #39662, #50206, #61754, #23445, #13583, #66358, #18179, #30802, #10065, #62806, #68453, #68817, #53331, #20252, #26560, #14648, #31490, #15694, #37177, #42456, #19901, #63177, #20963, #5112, #52973, #68120, #20609, #42122, #10416, #52303, #25870, #35754, #46707, #4059, #47037, #58586, #41055, #25189, #31842, #69155, #63514, #51940, #41756, #48082, #25525, #19561, #31143, #63850, #62471, #36113, #57550, #15372, #36488, #9377, #15012, #14289, #57190, #52638, #36827, #4769, #9020, #30438, #4395, #47388, #3694, #57911, #9737, #58242, #41400, #26219, #47760, #33245, #42814, #33581, #17442, #11783, #48422, #12118, #37538, #22691, #64202, #59967, #53989, #11430, #16412, #21643, #69484, #21281, #58943, #43507, #797, #32525, #37885, #38569, #65241, #64565, #22004, #44192, #64893, #38907, #65590, #32202, #22339, #49433, #43158, #6846, #10755, #16742, #474, #59253, #6158, #38208, #28270, #54682, #16058, #6482, #27238, #1154, #11076, #53649, #59611, #5436, #5791, #27921, #60312, #55018, #26883, #112, #32907, #48772, #54340, #27590, #49111, #43834, #17093, #40618, #60997, #56068, #65942, #7208, #34279, #7542, #19112, #1516, #55387, #62034, #29695, #50810, #12457, #28971, #13862, #55737, #45895, #61343, #51164, #35328, #23371, #44870, #24069, #66643, #66278, #18102, #24401, #67323, #13153, #45573, #34970, #17771, #2909, #34608, #7883, #56782, #18458, #39592, #2189, #28637, #12815, #8597, #13496, #23042, #49777, #44538, #61666, #50130, #39241, #60640, #33920, #1859, #40264, #50461, #29331, #23719, #45218, #39941, #2561, #66993, #18786, #56419, #8253, #46625, #68733, #25792, #25109, #52219, #4684, #3980, #47674, #26137, #62398, #31068, #9986, #51859, #37097, #40980, #46965, #30712, #3606, #36411, #25451, #58507, #15290, #30031, #63443, #57467, #31405, #68043, #51492, #36025, #68372, #20163, #24739, #19829, #41669, #62722, #47307, #30354, #20880, #52564, #3251, #63087, #63774, #69078, #41319, #20530, #14551, #9293, #9653, #15622, #14927, #57825, #4309, #46255, #67678, #42038, #36754, #19476, #42384, #58170, #52899, #14215, #35678, #57110, #8934, #59525, #27508, #64123, #48689, #69413, #21923, #6410, #724, #43752, #53903, #42725, #22256, #29, #65508, #59883, #65153, #38825, #11345, #32814, #26486, #49035, #15975, #37802, #59177, #27842, #64482, #54254, #49344, #11004, #37458, #22608, #21202, #48011, #31762, #16998, #5709, #58861, #38490, #44111, #27158, #1064, #394, #10668, #53250, #64818, #6074, #17359, #32122, #33170, #53575, #10331, #5362, #11700, #26803, #54605, #48337, #21564, #43077, #43434, #5036, #16326, #16665, #38130, #32442, #12371, #66190, #61588, #55990, #49695, #12729, #1429, #60238, #39504, #28893, #45137, #51080, #7118, #24326, #61268, #39162, #50378, #67242, #55296, #33497, #33834, #19028, #45496, #28547, #34201, #2833, #18378, #50049, #23629, #1785, #45818, #2106, #65864, #7797, #50726, #55652, #12037, #66912, #18714, #60912, #66555, #40187, #29244, #18013, #54929, #7468, #2471, #23295, #23982, #34882, #39864, #13418, #56329, #28184, #8165, #13078, #34531, #6754, #29606, #44792, #22958, #17694, #44460, #60553, #4225, #13780, #4596, #58096, #52487, #19395, #52821, #8518, #63353, #35238, #30989, #25025, #52137, #57034, #62314, #40540, #61954, #29953, #14462, #41577, #3519, #8853, #9571, #36316, #35596, #62640, #15208, #35941, #9907, #36675, #3162, #62998, #20445, #14136, #47589, #51418, #57386, #41241, #30273, #46890, #9211, #68996, #25701, #56698, #47222, #67960, #41947, #51771, #24653, #46535, #30629, #3892, #46170, #19745, #25368, #68291, #57740, #40892, #31323, #14839, #67597, #20077, #26055, #68640, #32038, #11264, #64038, #69664, #302, #54520, #21478, #27761, #15882, #32719, #16919, #38402, #43672, #21129, #64392, #22177, #6331, #54174, #69335, #21836, #43348, #11616, #53499, #27074, #37014, #47934, #5282, #48249, #59805, #42309, #26403, #33083, #649, #64744, #53161, #42988, #49265, #26727, #20802, #32362, #65065, #63697, #37366, #58772, #16586, #37718, #10589, #16240, #15541, #38041, #59108, #10927, #58422, #53823, #10248, #31685, #4955, #59433, #42633, #5622, #48609, #5984, #27423, #48951, #44375, #7387, #66104, #29522, #55912, #8070, #34453, #28455, #50639, #17617, #974, #7028, #1703, #44714, #65432, #22875, #60824, #33755, #66464, #1345, #61506, #2019, #22524, #17933, #34793, #18638, #12284, #61188, #65780, #49966, #50300, #56245, #23221, #44022, #39082, #12997, #66830, #40118, #23897, #60476, #39423, #2378, #17281, #7714, #49611, #23544, #45054, #13334, #55205, #28819, #38745, #28106, #12644, #34108, #60152, #11962, #6666, #33418, #45410, #18288, #54847, #55566, #39773, #29153, #47128, #62560, #30901, #41853, #24570, #46083, #25285, #67869, #67502, #19302, #25615, #68554, #14377, #46807, #36224, #18947, #4146, #35848, #57292, #15119, #19662, #40807, #3429, #8436, #14048, #52399, #14749, #24243, #36596, #20351, #62905, #29869, #63274, #40450, #58014, #45745, #41489, #35508, #9124, #62222, #3079, #50986, #2751, #61866, #24932, #52044, #56953, #8769, #19988, #30190, #30542, #51683, #46444, #67161, #13692, #35151, #41158, #3799, #68213, #57651, #9478, #9825, #56606, #51335, #6857, #6168, #49787, #28281, #64579, #33256, #12126, #54002, #39251, #43171, #49119, #32918, #5804, #38579, #27599, #60651, #17452, #31234, #65602, #59622, #33592, #48781, #52729, #38221, #54350, #806, #25962, #27247, #22349, #64903, #27933, #32537, #23053, #54689, #4497, #43844, #65950, #1525, #43515, #22701, #482, #11440, #11791, #17779, #65252, #47491, #22013, #44199, #44550, #124, #55031, #16751, #17104, #21653, #16421, #38917, #11087, #6490, #49447, #37892, #59978, #1165, #59261, #60320, #66653, #39953, #51500, #33931, #18114, #3262, #62042, #13510, #44882, #61354, #46269, #18468, #8605, #24080, #13872, #24750, #55747, #7552, #56430, #29341, #28984, #50472, #56793, #30041, #45585, #8261, #67336, #50140, #35337, #67002, #18795, #67690, #50818, #2201, #34619, #39604, #45227, #19484, #45905, #55395, #40990, #12468, #24408, #61009, #7218, #1871, #28647, #23379, #2919, #12824 ) ),
 .UNSPECIFIED., .F., .F., .F. ) 
 B_SPLINE_SURFACE_WITH_KNOTS ( ( 2, 2 ),
 ( 3, 2, 2, 2, 2, 2, 2, 2, 2, 2, 2, 2, 2, 2, 2, 2, 2, 2, 2, 2, 2, 2, 2, 2, 2, 2, 2, 2, 2, 2, 2, 2, 2, 2, 2, 2, 2, 2, 2, 2, 2, 2, 2, 2, 2, 2, 2, 2, 2, 2, 2, 2, 2, 2, 2, 2, 2, 2, 2, 2, 2, 2, 2, 2, 2, 2, 2, 2, 2, 2, 2, 2, 2, 2, 2, 2, 2, 2, 2, 2, 2, 2, 2, 2, 2, 2, 2, 2, 2, 2, 2, 2, 2, 2, 2, 2, 2, 2, 2, 2, 2, 2, 2, 2, 2, 2, 2, 2, 2, 2, 2, 2, 2, 2, 2, 2, 2, 2, 2, 2, 2, 2, 2, 2, 2, 2, 2, 2, 2, 2, 2, 2, 2, 2, 2, 2, 2, 2, 2, 2, 2, 2, 2, 2, 2, 2, 2, 2, 2, 2, 2, 2, 2, 2, 2, 2, 2, 2, 2, 2, 2, 2, 2, 2, 2, 2, 2, 2, 2, 2, 2, 2, 2, 2, 2, 2, 2, 2, 2, 2, 2, 2, 2, 2, 2, 2, 2, 2, 2, 2, 2, 2, 2, 2, 2, 2, 2, 2, 2, 2, 2, 2, 2, 2, 2, 2, 2, 2, 2, 2, 2, 2, 2, 2, 2, 2, 2, 2, 2, 2, 2, 2, 2, 2, 2, 2, 2, 2, 2, 2, 2, 2, 2, 2, 2, 2, 2, 2, 2, 2, 2, 2, 2, 2, 2, 2, 2, 2, 2, 2, 2, 2, 2, 2, 2, 2, 2, 2, 2, 2, 2, 2, 2, 2, 2, 2, 2, 2, 2, 2, 2, 2, 2, 2, 2, 2, 2, 2, 2, 2, 2, 2, 2, 2, 2, 2, 2, 2, 2, 2, 2, 2, 2, 2, 2, 2, 2, 2, 2, 2, 2, 2, 2, 2, 2, 2, 2, 2, 2, 2, 2, 2, 2, 2, 2, 2, 2, 2, 2, 2, 2, 2, 2, 2, 2, 2, 2, 2, 2, 2, 2, 2, 2, 2, 2, 2, 2, 2, 2, 2, 2, 2, 2, 2, 2, 2, 2, 2, 2, 2, 2, 2, 2, 2, 2, 2, 2, 2, 2, 2, 2, 2, 2, 2, 2, 2, 2, 2, 2, 2, 2, 2, 2, 2, 2, 2, 2, 2, 2, 2, 2, 2, 2, 2, 2, 2, 2, 2, 2, 2, 2, 2, 2, 2, 2, 2, 2, 2, 2, 2, 2, 2, 2, 2, 2, 2, 2, 2, 2, 2, 2, 2, 2, 2, 2, 2, 2, 2, 2, 2, 2, 2, 2, 2, 2, 2, 2, 2, 2, 2, 2, 2, 2, 2, 2, 2, 2, 2, 2, 2, 2, 2, 2, 2, 2, 2, 2, 2, 2, 2, 2, 2, 2, 2, 2, 2, 3 ),
 ( 0.000000000000000000, 1.000000000000000000 ),
 ( 0.000000000000000000, 0.002173913043478260896, 0.004347826086956521792, 0.006521739130434782254, 0.008695652173913043584, 0.01086956521739130405, 0.01304347826086956451, 0.01521739130434782671, 0.01739130434782608717, 0.01956521739130434936, 0.02173913043478260809, 0.02391304347826087029, 0.02608695652173912902, 0.02826086956521739121, 0.03043478260869565341, 0.03260869565217391214, 0.03478260869565217434, 0.03695652173913043653, 0.03913043478260869873, 0.04130434782608695399, 0.04347826086956521618, 0.04565217391304347838, 0.04782608695652174058, 0.05000000000000000278, 0.05217391304347825803, 0.05434782608695652023, 0.05652173913043478243, 0.05869565217391304462, 0.06086956521739130682, 0.06304347826086956208, 0.06521739130434782428, 0.06739130434782608647, 0.06956521739130434867, 0.07173913043478261087, 0.07391304347826087306, 0.07608695652173913526, 0.07826086956521739746, 0.08043478260869564578, 0.08260869565217390798, 0.08478260869565217017, 0.08695652173913043237, 0.08913043478260869457, 0.09130434782608695676, 0.09347826086956521896, 0.09565217391304348116, 0.09782608695652174335, 0.1000000000000000056, 0.1021739130434782677, 0.1043478260869565161, 0.1065217391304347783, 0.1086956521739130405, 0.1108695652173913027, 0.1130434782608695649, 0.1152173913043478271, 0.1173913043478260892, 0.1195652173913043514, 0.1217391304347826136, 0.1239130434782608758, 0.1260869565217391242, 0.1282608695652174002, 0.1304347826086956486, 0.1326086956521739246, 0.1347826086956521729, 0.1369565217391304213, 0.1391304347826086973, 0.1413043478260869457, 0.1434782608695652217, 0.1456521739130434701, 0.1478260869565217461, 0.1499999999999999944, 0.1521739130434782705, 0.1543478260869565188, 0.1565217391304347949, 0.1586956521739130432, 0.1608695652173912916, 0.1630434782608695676, 0.1652173913043478160, 0.1673913043478260920, 0.1695652173913043403, 0.1717391304347826164, 0.1739130434782608647, 0.1760869565217391408, 0.1782608695652173891, 0.1804347826086956652, 0.1826086956521739135, 0.1847826086956521618, 0.1869565217391304379, 0.1891304347826086862, 0.1913043478260869623, 0.1934782608695652106, 0.1956521739130434867, 0.1978260869565217350, 0.2000000000000000111, 0.2021739130434782594, 0.2043478260869565355, 0.2065217391304347838, 0.2086956521739130321, 0.2108695652173913082, 0.2130434782608695565, 0.2152173913043478326, 0.2173913043478260809, 0.2195652173913043570, 0.2217391304347826053, 0.2239130434782608814, 0.2260869565217391297, 0.2282608695652173780, 0.2304347826086956541, 0.2326086956521739024, 0.2347826086956521785, 0.2369565217391304268, 0.2391304347826087029, 0.2413043478260869512, 0.2434782608695652273, 0.2456521739130434756, 0.2478260869565217517, 0.2500000000000000000, 0.2521739130434782483, 0.2543478260869564966, 0.2565217391304348005, 0.2586956521739130488, 0.2608695652173912971, 0.2630434782608695454, 0.2652173913043478493, 0.2673913043478260976, 0.2695652173913043459, 0.2717391304347825942, 0.2739130434782608425, 0.2760869565217391464, 0.2782608695652173947, 0.2804347826086956430, 0.2826086956521738913, 0.2847826086956521952, 0.2869565217391304435, 0.2891304347826086918, 0.2913043478260869401, 0.2934782608695652439, 0.2956521739130434923, 0.2978260869565217406, 0.2999999999999999889, 0.3021739130434782372, 0.3043478260869565410, 0.3065217391304347894, 0.3086956521739130377, 0.3108695652173912860, 0.3130434782608695898, 0.3152173913043478382, 0.3173913043478260865, 0.3195652173913043348, 0.3217391304347825831, 0.3239130434782608869, 0.3260869565217391353, 0.3282608695652173836, 0.3304347826086956319, 0.3326086956521739357, 0.3347826086956521840, 0.3369565217391304324, 0.3391304347826086807, 0.3413043478260869290, 0.3434782608695652328, 0.3456521739130434812, 0.3478260869565217295, 0.3499999999999999778, 0.3521739130434782816, 0.3543478260869565299, 0.3565217391304347783, 0.3586956521739130266, 0.3608695652173913304, 0.3630434782608695787, 0.3652173913043478271, 0.3673913043478260754, 0.3695652173913043237, 0.3717391304347826275, 0.3739130434782608758, 0.3760869565217391242, 0.3782608695652173725, 0.3804347826086956763, 0.3826086956521739246, 0.3847826086956521729, 0.3869565217391304213, 0.3891304347826086696, 0.3913043478260869734, 0.3934782608695652217, 0.3956521739130434701, 0.3978260869565217184, 0.4000000000000000222, 0.4021739130434782705, 0.4043478260869565188, 0.4065217391304347672, 0.4086956521739130710, 0.4108695652173913193, 0.4130434782608695676, 0.4152173913043478160, 0.4173913043478260643, 0.4195652173913043681, 0.4217391304347826164, 0.4239130434782608647, 0.4260869565217391131, 0.4282608695652174169, 0.4304347826086956652, 0.4326086956521739135, 0.4347826086956521618, 0.4369565217391304102, 0.4391304347826087140, 0.4413043478260869623, 0.4434782608695652106, 0.4456521739130434590, 0.4478260869565217628, 0.4500000000000000111, 0.4521739130434782594, 0.4543478260869565077, 0.4565217391304347561, 0.4586956521739130599, 0.4608695652173913082, 0.4630434782608695565, 0.4652173913043478048, 0.4673913043478261087, 0.4695652173913043570, 0.4717391304347826053, 0.4739130434782608536, 0.4760869565217391575, 0.4782608695652174058, 0.4804347826086956541, 0.4826086956521739024, 0.4847826086956521507, 0.4869565217391304546, 0.4891304347826087029, 0.4913043478260869512, 0.4934782608695651995, 0.4956521739130435034, 0.4978260869565217517, 0.5000000000000000000, 0.5021739130434782483, 0.5043478260869564966, 0.5065217391304347450, 0.5086956521739129933, 0.5108695652173913526, 0.5130434782608696009, 0.5152173913043478493, 0.5173913043478260976, 0.5195652173913043459, 0.5217391304347825942, 0.5239130434782608425, 0.5260869565217390909, 0.5282608695652173392, 0.5304347826086956985, 0.5326086956521739468, 0.5347826086956521952, 0.5369565217391304435, 0.5391304347826086918, 0.5413043478260869401, 0.5434782608695651884, 0.5456521739130434367, 0.5478260869565216851, 0.5500000000000000444, 0.5521739130434782927, 0.5543478260869565410, 0.5565217391304347894, 0.5586956521739130377, 0.5608695652173912860, 0.5630434782608695343, 0.5652173913043477826, 0.5673913043478261420, 0.5695652173913043903, 0.5717391304347826386, 0.5739130434782608869, 0.5760869565217391353, 0.5782608695652173836, 0.5804347826086956319, 0.5826086956521738802, 0.5847826086956521285, 0.5869565217391304879, 0.5891304347826087362, 0.5913043478260869845, 0.5934782608695652328, 0.5956521739130434812, 0.5978260869565217295, 0.5999999999999999778, 0.6021739130434782261, 0.6043478260869564744, 0.6065217391304348338, 0.6086956521739130821, 0.6108695652173913304, 0.6130434782608695787, 0.6152173913043478271, 0.6173913043478260754, 0.6195652173913043237, 0.6217391304347825720, 0.6239130434782608203, 0.6260869565217391797, 0.6282608695652174280, 0.6304347826086956763, 0.6326086956521739246, 0.6347826086956521729, 0.6369565217391304213, 0.6391304347826086696, 0.6413043478260869179, 0.6434782608695651662, 0.6456521739130435256, 0.6478260869565217739, 0.6500000000000000222, 0.6521739130434782705, 0.6543478260869565188, 0.6565217391304347672, 0.6586956521739130155, 0.6608695652173912638, 0.6630434782608695121, 0.6652173913043478715, 0.6673913043478261198, 0.6695652173913043681, 0.6717391304347826164, 0.6739130434782608647, 0.6760869565217391131, 0.6782608695652173614, 0.6804347826086956097, 0.6826086956521738580, 0.6847826086956522174, 0.6869565217391304657, 0.6891304347826087140, 0.6913043478260869623, 0.6934782608695652106, 0.6956521739130434590, 0.6978260869565217073, 0.6999999999999999556, 0.7021739130434783149, 0.7043478260869565633, 0.7065217391304348116, 0.7086956521739130599, 0.7108695652173913082, 0.7130434782608695565, 0.7152173913043478048, 0.7173913043478260532, 0.7195652173913043015, 0.7217391304347826608, 0.7239130434782609091, 0.7260869565217391575, 0.7282608695652174058, 0.7304347826086956541, 0.7326086956521739024, 0.7347826086956521507, 0.7369565217391303991, 0.7391304347826086474, 0.7413043478260870067, 0.7434782608695652550, 0.7456521739130435034, 0.7478260869565217517, 0.7500000000000000000, 0.7521739130434782483, 0.7543478260869564966, 0.7565217391304347450, 0.7586956521739129933, 0.7608695652173913526, 0.7630434782608696009, 0.7652173913043478493, 0.7673913043478260976, 0.7695652173913043459, 0.7717391304347825942, 0.7739130434782608425, 0.7760869565217390909, 0.7782608695652173392, 0.7804347826086956985, 0.7826086956521739468, 0.7847826086956521952, 0.7869565217391304435, 0.7891304347826086918, 0.7913043478260869401, 0.7934782608695651884, 0.7956521739130434367, 0.7978260869565216851, 0.8000000000000000444, 0.8021739130434782927, 0.8043478260869565410, 0.8065217391304347894, 0.8086956521739130377, 0.8108695652173912860, 0.8130434782608695343, 0.8152173913043477826, 0.8173913043478261420, 0.8195652173913043903, 0.8217391304347826386, 0.8239130434782608869, 0.8260869565217391353, 0.8282608695652173836, 0.8304347826086956319, 0.8326086956521738802, 0.8347826086956521285, 0.8369565217391304879, 0.8391304347826087362, 0.8413043478260869845, 0.8434782608695652328, 0.8456521739130434812, 0.8478260869565217295, 0.8499999999999999778, 0.8521739130434782261, 0.8543478260869564744, 0.8565217391304348338, 0.8586956521739130821, 0.8608695652173913304, 0.8630434782608695787, 0.8652173913043478271, 0.8673913043478260754, 0.8695652173913043237, 0.8717391304347825720, 0.8739130434782608203, 0.8760869565217391797, 0.8782608695652174280, 0.8804347826086956763, 0.8826086956521739246, 0.8847826086956521729, 0.8869565217391304213, 0.8891304347826086696, 0.8913043478260869179, 0.8934782608695651662, 0.8956521739130435256, 0.8978260869565217739, 0.9000000000000000222, 0.9021739130434782705, 0.9043478260869565188, 0.9065217391304347672, 0.9086956521739130155, 0.9108695652173912638, 0.9130434782608695121, 0.9152173913043478715, 0.9173913043478261198, 0.9195652173913043681, 0.9217391304347826164, 0.9239130434782608647, 0.9260869565217391131, 0.9282608695652173614, 0.9304347826086956097, 0.9326086956521738580, 0.9347826086956522174, 0.9369565217391304657, 0.9391304347826087140, 0.9413043478260869623, 0.9434782608695652106, 0.9456521739130434590, 0.9478260869565217073, 0.9499999999999999556, 0.9521739130434783149, 0.9543478260869565633, 0.9565217391304348116, 0.9586956521739130599, 0.9608695652173913082, 0.9630434782608695565, 0.9652173913043478048, 0.9673913043478260532, 0.9695652173913043015, 0.9717391304347826608, 0.9739130434782609091, 0.9760869565217391575, 0.9782608695652174058, 0.9804347826086956541, 0.9826086956521739024, 0.9847826086956521507, 0.9869565217391303991, 0.9891304347826086474, 0.9913043478260870067 ),
 .UNSPECIFIED. ) 
 GEOMETRIC_REPRESENTATION_ITEM ( )  RATIONAL_B_SPLINE_SURFACE ( (
 ( 1.000000000000000000, 0.9510565162951535312, 1.000000000000000000, 0.9510565162951535312, 1.000000000000000000, 0.9510565162951535312, 1.000000000000000000, 0.9510565162951535312, 1.000000000000000000, 0.9510565162951535312, 1.000000000000000000, 0.9510565162951535312, 1.000000000000000000, 0.9510565162951535312, 1.000000000000000000, 0.9510565162951535312, 1.000000000000000000, 0.9510565162951535312, 1.000000000000000000, 0.9510565162951535312, 1.000000000000000000, 0.9510565162951535312, 1.000000000000000000, 0.9510565162951535312, 1.000000000000000000, 0.9510565162951535312, 1.000000000000000000, 0.9510565162951535312, 1.000000000000000000, 0.9510565162951535312, 1.000000000000000000, 0.9510565162951535312, 1.000000000000000000, 0.9510565162951535312, 1.000000000000000000, 0.9510565162951535312, 1.000000000000000000, 0.9510565162951535312, 1.000000000000000000, 0.9510565162951535312, 1.000000000000000000, 0.9510565162951535312, 1.000000000000000000, 0.9510565162951535312, 1.000000000000000000, 0.9510565162951535312, 1.000000000000000000, 0.9510565162951535312, 1.000000000000000000, 0.9510565162951535312, 1.000000000000000000, 0.9510565162951535312, 1.000000000000000000, 0.9510565162951535312, 1.000000000000000000, 0.9510565162951535312, 1.000000000000000000, 0.9510565162951535312, 1.000000000000000000, 0.9510565162951535312, 1.000000000000000000, 0.9510565162951535312, 1.000000000000000000, 0.9510565162951535312, 1.000000000000000000, 0.9510565162951535312, 1.000000000000000000, 0.9510565162951535312, 1.000000000000000000, 0.9510565162951535312, 1.000000000000000000, 0.9510565162951535312, 1.000000000000000000, 0.9510565162951535312, 1.000000000000000000, 0.9510565162951535312, 1.000000000000000000, 0.9510565162951535312, 1.000000000000000000, 0.9510565162951535312, 1.000000000000000000, 0.9510565162951535312, 1.000000000000000000, 0.9510565162951535312, 1.000000000000000000, 0.9510565162951535312, 1.000000000000000000, 0.9510565162951535312, 1.000000000000000000, 0.9510565162951535312, 1.000000000000000000, 0.9510565162951535312, 1.000000000000000000, 0.9510565162951535312, 1.000000000000000000, 0.9510565162951535312, 1.000000000000000000, 0.9510565162951535312, 1.000000000000000000, 0.9510565162951535312, 1.000000000000000000, 0.9510565162951535312, 1.000000000000000000, 0.9510565162951535312, 1.000000000000000000, 0.9510565162951535312, 1.000000000000000000, 0.9510565162951535312, 1.000000000000000000, 0.9510565162951535312, 1.000000000000000000, 0.9510565162951535312, 1.000000000000000000, 0.9510565162951535312, 1.000000000000000000, 0.9510565162951535312, 1.000000000000000000, 0.9510565162951535312, 1.000000000000000000, 0.9510565162951535312, 1.000000000000000000, 0.9510565162951535312, 1.000000000000000000, 0.9510565162951535312, 1.000000000000000000, 0.9510565162951535312, 1.000000000000000000, 0.9510565162951535312, 1.000000000000000000, 0.9510565162951535312, 1.000000000000000000, 0.9510565162951535312, 1.000000000000000000, 0.9510565162951535312, 1.000000000000000000, 0.9510565162951535312, 1.000000000000000000, 0.9510565162951535312, 1.000000000000000000, 0.9510565162951535312, 1.000000000000000000, 0.9510565162951535312, 1.000000000000000000, 0.9510565162951535312, 1.000000000000000000, 0.9510565162951535312, 1.000000000000000000, 0.9510565162951535312, 1.000000000000000000, 0.9510565162951535312, 1.000000000000000000, 0.9510565162951535312, 1.000000000000000000, 0.9510565162951535312, 1.000000000000000000, 0.9510565162951535312, 1.000000000000000000, 0.9510565162951535312, 1.000000000000000000, 0.9510565162951535312, 1.000000000000000000, 0.9510565162951535312, 1.000000000000000000, 0.9510565162951535312, 1.000000000000000000, 0.9510565162951535312, 1.000000000000000000, 0.9510565162951535312, 1.000000000000000000, 0.9510565162951535312, 1.000000000000000000, 0.9510565162951535312, 1.000000000000000000, 0.9510565162951535312, 1.000000000000000000, 0.9510565162951535312, 1.000000000000000000, 0.9510565162951535312, 1.000000000000000000, 0.9510565162951535312, 1.000000000000000000, 0.9510565162951535312, 1.000000000000000000, 0.9510565162951535312, 1.000000000000000000, 0.9510565162951535312, 1.000000000000000000, 0.9510565162951535312, 1.000000000000000000, 0.9510565162951535312, 1.000000000000000000, 0.9510565162951535312, 1.000000000000000000, 0.9510565162951535312, 1.000000000000000000, 0.9510565162951535312, 1.000000000000000000, 0.9510565162951535312, 1.000000000000000000, 0.9510565162951535312, 1.000000000000000000, 0.9510565162951535312, 1.000000000000000000, 0.9510565162951535312, 1.000000000000000000, 0.9510565162951535312, 1.000000000000000000, 0.9510565162951535312, 1.000000000000000000, 0.9510565162951535312, 1.000000000000000000, 0.9510565162951535312, 1.000000000000000000, 0.9510565162951535312, 1.000000000000000000, 0.9510565162951535312, 1.000000000000000000, 0.9510565162951535312, 1.000000000000000000, 0.9510565162951535312, 1.000000000000000000, 0.9510565162951535312, 1.000000000000000000, 0.9510565162951535312, 1.000000000000000000, 0.9510565162951535312, 1.000000000000000000, 0.9510565162951535312, 1.000000000000000000, 0.9510565162951535312, 1.000000000000000000, 0.9510565162951535312, 1.000000000000000000, 0.9510565162951535312, 1.000000000000000000, 0.9510565162951535312, 1.000000000000000000, 0.9510565162951535312, 1.000000000000000000, 0.9510565162951535312, 1.000000000000000000, 0.9510565162951535312, 1.000000000000000000, 0.9510565162951535312, 1.000000000000000000, 0.9510565162951535312, 1.000000000000000000, 0.9510565162951535312, 1.000000000000000000, 0.9510565162951535312, 1.000000000000000000, 0.9510565162951535312, 1.000000000000000000, 0.9510565162951535312, 1.000000000000000000, 0.9510565162951535312, 1.000000000000000000, 0.9510565162951535312, 1.000000000000000000, 0.9510565162951535312, 1.000000000000000000, 0.9510565162951535312, 1.000000000000000000, 0.9510565162951535312, 1.000000000000000000, 0.9510565162951535312, 1.000000000000000000, 0.9510565162951535312, 1.000000000000000000, 0.9510565162951535312, 1.000000000000000000, 0.9510565162951535312, 1.000000000000000000, 0.9510565162951535312, 1.000000000000000000, 0.9510565162951535312, 1.000000000000000000, 0.9510565162951535312, 1.000000000000000000, 0.9510565162951535312, 1.000000000000000000, 0.9510565162951535312, 1.000000000000000000, 0.9510565162951535312, 1.000000000000000000, 0.9510565162951535312, 1.000000000000000000, 0.9510565162951535312, 1.000000000000000000, 0.9510565162951535312, 1.000000000000000000, 0.9510565162951535312, 1.000000000000000000, 0.9510565162951535312, 1.000000000000000000, 0.9510565162951535312, 1.000000000000000000, 0.9510565162951535312, 1.000000000000000000, 0.9510565162951535312, 1.000000000000000000, 0.9510565162951535312, 1.000000000000000000, 0.9510565162951535312, 1.000000000000000000, 0.9510565162951535312, 1.000000000000000000, 0.9510565162951535312, 1.000000000000000000, 0.9510565162951535312, 1.000000000000000000, 0.9510565162951535312, 1.000000000000000000, 0.9510565162951535312, 1.000000000000000000, 0.9510565162951535312, 1.000000000000000000, 0.9510565162951535312, 1.000000000000000000, 0.9510565162951535312, 1.000000000000000000, 0.9510565162951535312, 1.000000000000000000, 0.9510565162951535312, 1.000000000000000000, 0.9510565162951535312, 1.000000000000000000, 0.9510565162951535312, 1.000000000000000000, 0.9510565162951535312, 1.000000000000000000, 0.9510565162951535312, 1.000000000000000000, 0.9510565162951535312, 1.000000000000000000, 0.9510565162951535312, 1.000000000000000000, 0.9510565162951535312, 1.000000000000000000, 0.9510565162951535312, 1.000000000000000000, 0.9510565162951535312, 1.000000000000000000, 0.9510565162951535312, 1.000000000000000000, 0.9510565162951535312, 1.000000000000000000, 0.9510565162951535312, 1.000000000000000000, 0.9510565162951535312, 1.000000000000000000, 0.9510565162951535312, 1.000000000000000000, 0.9510565162951535312, 1.000000000000000000, 0.9510565162951535312, 1.000000000000000000, 0.9510565162951535312, 1.000000000000000000, 0.9510565162951535312, 1.000000000000000000, 0.9510565162951535312, 1.000000000000000000, 0.9510565162951535312, 1.000000000000000000, 0.9510565162951535312, 1.000000000000000000, 0.9510565162951535312, 1.000000000000000000, 0.9510565162951535312, 1.000000000000000000, 0.9510565162951535312, 1.000000000000000000, 0.9510565162951535312, 1.000000000000000000, 0.9510565162951535312, 1.000000000000000000, 0.9510565162951535312, 1.000000000000000000, 0.9510565162951535312, 1.000000000000000000, 0.9510565162951535312, 1.000000000000000000, 0.9510565162951535312, 1.000000000000000000, 0.9510565162951535312, 1.000000000000000000, 0.9510565162951535312, 1.000000000000000000, 0.9510565162951535312, 1.000000000000000000, 0.9510565162951535312, 1.000000000000000000, 0.9510565162951535312, 1.000000000000000000, 0.9510565162951535312, 1.000000000000000000, 0.9510565162951535312, 1.000000000000000000, 0.9510565162951535312, 1.000000000000000000, 0.9510565162951535312, 1.000000000000000000, 0.9510565162951535312, 1.000000000000000000, 0.9510565162951535312, 1.000000000000000000, 0.9510565162951535312, 1.000000000000000000, 0.9510565162951535312, 1.000000000000000000, 0.9510565162951535312, 1.000000000000000000, 0.9510565162951535312, 1.000000000000000000, 0.9510565162951535312, 1.000000000000000000, 0.9510565162951535312, 1.000000000000000000, 0.9510565162951535312, 1.000000000000000000, 0.9510565162951535312, 1.000000000000000000, 0.9510565162951535312, 1.000000000000000000, 0.9510565162951535312, 1.000000000000000000, 0.9510565162951535312, 1.000000000000000000, 0.9510565162951535312, 1.000000000000000000, 0.9510565162951535312, 1.000000000000000000, 0.9510565162951535312, 1.000000000000000000, 0.9510565162951535312, 1.000000000000000000, 0.9510565162951535312, 1.000000000000000000, 0.9510565162951535312, 1.000000000000000000, 0.9510565162951535312, 1.000000000000000000, 0.9510565162951535312, 1.000000000000000000, 0.9510565162951535312, 1.000000000000000000, 0.9510565162951535312, 1.000000000000000000, 0.9510565162951535312, 1.000000000000000000, 0.9510565162951535312, 1.000000000000000000, 0.9510565162951535312, 1.000000000000000000, 0.9510565162951535312, 1.000000000000000000, 0.9510565162951535312, 1.000000000000000000, 0.9510565162951535312, 1.000000000000000000, 0.9510565162951535312, 1.000000000000000000, 0.9510565162951535312, 1.000000000000000000, 0.9510565162951535312, 1.000000000000000000, 0.9510565162951535312, 1.000000000000000000, 0.9510565162951535312, 1.000000000000000000, 0.9510565162951535312, 1.000000000000000000, 0.9510565162951535312, 1.000000000000000000, 0.9510565162951535312, 1.000000000000000000, 0.9510565162951535312, 1.000000000000000000, 0.9510565162951535312, 1.000000000000000000, 0.9510565162951535312, 1.000000000000000000, 0.9510565162951535312, 1.000000000000000000, 0.9510565162951535312, 1.000000000000000000, 0.9510565162951535312, 1.000000000000000000, 0.9510565162951535312, 1.000000000000000000, 0.9510565162951535312, 1.000000000000000000, 0.9510565162951535312, 1.000000000000000000, 0.9510565162951535312, 1.000000000000000000, 0.9510565162951535312, 1.000000000000000000, 0.9510565162951535312, 1.000000000000000000, 0.9510565162951535312, 1.000000000000000000, 0.9510565162951535312, 1.000000000000000000, 0.9510565162951535312, 1.000000000000000000, 0.9510565162951535312, 1.000000000000000000, 0.9510565162951535312, 1.000000000000000000, 0.9510565162951535312, 1.000000000000000000, 0.9510565162951535312, 1.000000000000000000, 0.9510565162951535312, 1.000000000000000000, 0.9510565162951535312, 1.000000000000000000, 0.9510565162951535312, 1.000000000000000000, 0.9510565162951535312, 1.000000000000000000, 0.9510565162951535312, 1.000000000000000000, 0.9510565162951535312, 1.000000000000000000, 0.9510565162951535312, 1.000000000000000000, 0.9510565162951535312, 1.000000000000000000, 0.9510565162951535312, 1.000000000000000000, 0.9510565162951535312, 1.000000000000000000, 0.9510565162951535312, 1.000000000000000000, 0.9510565162951535312, 1.000000000000000000, 0.9510565162951535312, 1.000000000000000000, 0.9510565162951535312, 1.000000000000000000, 0.9510565162951535312, 1.000000000000000000, 0.9510565162951535312, 1.000000000000000000, 0.9510565162951535312, 1.000000000000000000, 0.9510565162951535312, 1.000000000000000000, 0.9510565162951535312, 1.000000000000000000, 0.9510565162951535312, 1.000000000000000000, 0.9510565162951535312, 1.000000000000000000, 0.9510565162951535312, 1.000000000000000000, 0.9510565162951535312, 1.000000000000000000, 0.9510565162951535312, 1.000000000000000000, 0.9510565162951535312, 1.000000000000000000, 0.9510565162951535312, 1.000000000000000000, 0.9510565162951535312, 1.000000000000000000, 0.9510565162951535312, 1.000000000000000000, 0.9510565162951535312, 1.000000000000000000, 0.9510565162951535312, 1.000000000000000000, 0.9510565162951535312, 1.000000000000000000, 0.9510565162951535312, 1.000000000000000000, 0.9510565162951535312, 1.000000000000000000, 0.9510565162951535312, 1.000000000000000000, 0.9510565162951535312, 1.000000000000000000, 0.9510565162951535312, 1.000000000000000000, 0.9510565162951535312, 1.000000000000000000, 0.9510565162951535312, 1.000000000000000000, 0.9510565162951535312, 1.000000000000000000, 0.9510565162951535312, 1.000000000000000000, 0.9510565162951535312, 1.000000000000000000, 0.9510565162951535312, 1.000000000000000000, 0.9510565162951535312, 1.000000000000000000, 0.9510565162951535312, 1.000000000000000000, 0.9510565162951535312, 1.000000000000000000, 0.9510565162951535312, 1.000000000000000000, 0.9510565162951535312, 1.000000000000000000, 0.9510565162951535312, 1.000000000000000000, 0.9510565162951535312, 1.000000000000000000, 0.9510565162951535312, 1.000000000000000000, 0.9510565162951535312, 1.000000000000000000, 0.9510565162951535312, 1.000000000000000000, 0.9510565162951535312, 1.000000000000000000, 0.9510565162951535312, 1.000000000000000000, 0.9510565162951535312, 1.000000000000000000, 0.9510565162951535312, 1.000000000000000000, 0.9510565162951535312, 1.000000000000000000, 0.9510565162951535312, 1.000000000000000000, 0.9510565162951535312, 1.000000000000000000, 0.9510565162951535312, 1.000000000000000000, 0.9510565162951535312, 1.000000000000000000, 0.9510565162951535312, 1.000000000000000000, 0.9510565162951535312, 1.000000000000000000, 0.9510565162951535312, 1.000000000000000000, 0.9510565162951535312, 1.000000000000000000, 0.9510565162951535312, 1.000000000000000000, 0.9510565162951535312, 1.000000000000000000, 0.9510565162951535312, 1.000000000000000000, 0.9510565162951535312, 1.000000000000000000, 0.9510565162951535312, 1.000000000000000000, 0.9510565162951535312, 1.000000000000000000, 0.9510565162951535312, 1.000000000000000000, 0.9510565162951535312, 1.000000000000000000, 0.9510565162951535312, 1.000000000000000000, 0.9510565162951535312, 1.000000000000000000, 0.9510565162951535312, 1.000000000000000000, 0.9510565162951535312, 1.000000000000000000, 0.9510565162951535312, 1.000000000000000000, 0.9510565162951535312, 1.000000000000000000, 0.9510565162951535312, 1.000000000000000000, 0.9510565162951535312, 1.000000000000000000, 0.9510565162951535312, 1.000000000000000000, 0.9510565162951535312, 1.000000000000000000, 0.9510565162951535312, 1.000000000000000000, 0.9510565162951535312, 1.000000000000000000, 0.9510565162951535312, 1.000000000000000000, 0.9510565162951535312, 1.000000000000000000, 0.9510565162951535312, 1.000000000000000000, 0.9510565162951535312, 1.000000000000000000, 0.9510565162951535312, 1.000000000000000000, 0.9510565162951535312, 1.000000000000000000, 0.9510565162951535312, 1.000000000000000000, 0.9510565162951535312, 1.000000000000000000, 0.9510565162951535312, 1.000000000000000000, 0.9510565162951535312, 1.000000000000000000, 0.9510565162951535312, 1.000000000000000000, 0.9510565162951535312, 1.000000000000000000, 0.9510565162951535312, 1.000000000000000000, 0.9510565162951535312, 1.000000000000000000, 0.9510565162951535312, 1.000000000000000000, 0.9510565162951535312, 1.000000000000000000, 0.9510565162951535312, 1.000000000000000000, 0.9510565162951535312, 1.000000000000000000, 0.9510565162951535312, 1.000000000000000000, 0.9510565162951535312, 1.000000000000000000, 0.9510565162951535312, 1.000000000000000000, 0.9510565162951535312, 1.000000000000000000, 0.9510565162951535312, 1.000000000000000000, 0.9510565162951535312, 1.000000000000000000, 0.9510565162951535312, 1.000000000000000000, 0.9510565162951535312, 1.000000000000000000, 0.9510565162951535312, 1.000000000000000000, 0.9510565162951535312, 1.000000000000000000, 0.9510565162951535312, 1.000000000000000000, 0.9510565162951535312, 1.000000000000000000, 0.9510565162951535312, 1.000000000000000000, 0.9510565162951535312, 1.000000000000000000, 0.9510565162951535312, 1.000000000000000000, 0.9510565162951535312, 1.000000000000000000, 0.9510565162951535312, 1.000000000000000000, 0.9510565162951535312, 1.000000000000000000, 0.9510565162951535312, 1.000000000000000000, 0.9510565162951535312, 1.000000000000000000, 0.9510565162951535312, 1.000000000000000000, 0.9510565162951535312, 1.000000000000000000, 0.9510565162951535312, 1.000000000000000000, 0.9510565162951535312, 1.000000000000000000, 0.9510565162951535312, 1.000000000000000000, 0.9510565162951535312, 1.000000000000000000, 0.9510565162951535312, 1.000000000000000000, 0.9510565162951535312, 1.000000000000000000, 0.9510565162951535312, 1.000000000000000000, 0.9510565162951535312, 1.000000000000000000, 0.9510565162951535312, 1.000000000000000000, 0.9510565162951535312, 1.000000000000000000, 0.9510565162951535312, 1.000000000000000000, 0.9510565162951535312, 1.000000000000000000, 0.9510565162951535312, 1.000000000000000000, 0.9510565162951535312, 1.000000000000000000, 0.9510565162951535312, 1.000000000000000000, 0.9510565162951535312, 1.000000000000000000, 0.9510565162951535312, 1.000000000000000000, 0.9510565162951535312, 1.000000000000000000, 0.9510565162951535312, 1.000000000000000000, 0.9510565162951535312, 1.000000000000000000, 0.9510565162951535312, 1.000000000000000000, 0.9510565162951535312, 1.000000000000000000, 0.9510565162951535312, 1.000000000000000000, 0.9510565162951535312, 1.000000000000000000, 0.9510565162951535312, 1.000000000000000000, 0.9510565162951535312, 1.000000000000000000, 0.9510565162951535312, 1.000000000000000000, 0.9510565162951535312, 1.000000000000000000, 0.9510565162951535312, 1.000000000000000000, 0.9510565162951535312, 1.000000000000000000, 0.9510565162951535312, 1.000000000000000000, 0.9510565162951535312, 1.000000000000000000, 0.9510565162951535312, 1.000000000000000000, 0.9510565162951535312, 1.000000000000000000, 0.9510565162951535312, 1.000000000000000000, 0.9510565162951535312, 1.000000000000000000, 0.9510565162951535312, 1.000000000000000000, 0.9510565162951535312, 1.000000000000000000, 0.9510565162951535312, 1.000000000000000000, 0.9510565162951535312, 1.000000000000000000, 0.9510565162951535312, 1.000000000000000000, 0.9510565162951535312, 1.000000000000000000, 0.9510565162951535312, 1.000000000000000000, 0.9510565162951535312, 1.000000000000000000, 0.9510565162951535312, 1.000000000000000000, 0.9510565162951535312, 1.000000000000000000, 0.9510565162951535312, 1.000000000000000000, 0.9510565162951535312, 1.000000000000000000, 0.9510565162951535312, 1.000000000000000000, 0.9510565162951535312, 1.000000000000000000, 0.9510565162951535312, 1.000000000000000000, 0.9510565162951535312, 1.000000000000000000, 0.9510565162951535312, 1.000000000000000000, 0.9510565162951535312, 1.000000000000000000, 0.9510565162951535312, 1.000000000000000000, 0.9510565162951535312, 1.000000000000000000, 0.9510565162951535312, 1.000000000000000000, 0.9510565162951535312, 1.000000000000000000, 0.9510565162951535312, 1.000000000000000000, 0.9510565162951535312, 1.000000000000000000, 0.9510565162951535312, 1.000000000000000000, 0.9510565162951535312, 1.000000000000000000, 0.9510565162951535312, 1.000000000000000000, 0.9510565162951535312, 1.000000000000000000, 0.9510565162951535312, 1.000000000000000000, 0.9510565162951535312, 1.000000000000000000, 0.9510565162951535312, 1.000000000000000000, 0.9510565162951535312, 1.000000000000000000, 0.9510565162951535312, 1.000000000000000000, 0.9510565162951535312, 1.000000000000000000, 0.9510565162951535312, 1.000000000000000000, 0.9510565162951535312, 1.000000000000000000, 0.9510565162951535312, 1.000000000000000000, 0.9510565162951535312, 1.000000000000000000),
 ( 1.000000000000000000, 0.9510565162951535312, 1.000000000000000000, 0.9510565162951535312, 1.000000000000000000, 0.9510565162951535312, 1.000000000000000000, 0.9510565162951535312, 1.000000000000000000, 0.9510565162951535312, 1.000000000000000000, 0.9510565162951535312, 1.000000000000000000, 0.9510565162951535312, 1.000000000000000000, 0.9510565162951535312, 1.000000000000000000, 0.9510565162951535312, 1.000000000000000000, 0.9510565162951535312, 1.000000000000000000, 0.9510565162951535312, 1.000000000000000000, 0.9510565162951535312, 1.000000000000000000, 0.9510565162951535312, 1.000000000000000000, 0.9510565162951535312, 1.000000000000000000, 0.9510565162951535312, 1.000000000000000000, 0.9510565162951535312, 1.000000000000000000, 0.9510565162951535312, 1.000000000000000000, 0.9510565162951535312, 1.000000000000000000, 0.9510565162951535312, 1.000000000000000000, 0.9510565162951535312, 1.000000000000000000, 0.9510565162951535312, 1.000000000000000000, 0.9510565162951535312, 1.000000000000000000, 0.9510565162951535312, 1.000000000000000000, 0.9510565162951535312, 1.000000000000000000, 0.9510565162951535312, 1.000000000000000000, 0.9510565162951535312, 1.000000000000000000, 0.9510565162951535312, 1.000000000000000000, 0.9510565162951535312, 1.000000000000000000, 0.9510565162951535312, 1.000000000000000000, 0.9510565162951535312, 1.000000000000000000, 0.9510565162951535312, 1.000000000000000000, 0.9510565162951535312, 1.000000000000000000, 0.9510565162951535312, 1.000000000000000000, 0.9510565162951535312, 1.000000000000000000, 0.9510565162951535312, 1.000000000000000000, 0.9510565162951535312, 1.000000000000000000, 0.9510565162951535312, 1.000000000000000000, 0.9510565162951535312, 1.000000000000000000, 0.9510565162951535312, 1.000000000000000000, 0.9510565162951535312, 1.000000000000000000, 0.9510565162951535312, 1.000000000000000000, 0.9510565162951535312, 1.000000000000000000, 0.9510565162951535312, 1.000000000000000000, 0.9510565162951535312, 1.000000000000000000, 0.9510565162951535312, 1.000000000000000000, 0.9510565162951535312, 1.000000000000000000, 0.9510565162951535312, 1.000000000000000000, 0.9510565162951535312, 1.000000000000000000, 0.9510565162951535312, 1.000000000000000000, 0.9510565162951535312, 1.000000000000000000, 0.9510565162951535312, 1.000000000000000000, 0.9510565162951535312, 1.000000000000000000, 0.9510565162951535312, 1.000000000000000000, 0.9510565162951535312, 1.000000000000000000, 0.9510565162951535312, 1.000000000000000000, 0.9510565162951535312, 1.000000000000000000, 0.9510565162951535312, 1.000000000000000000, 0.9510565162951535312, 1.000000000000000000, 0.9510565162951535312, 1.000000000000000000, 0.9510565162951535312, 1.000000000000000000, 0.9510565162951535312, 1.000000000000000000, 0.9510565162951535312, 1.000000000000000000, 0.9510565162951535312, 1.000000000000000000, 0.9510565162951535312, 1.000000000000000000, 0.9510565162951535312, 1.000000000000000000, 0.9510565162951535312, 1.000000000000000000, 0.9510565162951535312, 1.000000000000000000, 0.9510565162951535312, 1.000000000000000000, 0.9510565162951535312, 1.000000000000000000, 0.9510565162951535312, 1.000000000000000000, 0.9510565162951535312, 1.000000000000000000, 0.9510565162951535312, 1.000000000000000000, 0.9510565162951535312, 1.000000000000000000, 0.9510565162951535312, 1.000000000000000000, 0.9510565162951535312, 1.000000000000000000, 0.9510565162951535312, 1.000000000000000000, 0.9510565162951535312, 1.000000000000000000, 0.9510565162951535312, 1.000000000000000000, 0.9510565162951535312, 1.000000000000000000, 0.9510565162951535312, 1.000000000000000000, 0.9510565162951535312, 1.000000000000000000, 0.9510565162951535312, 1.000000000000000000, 0.9510565162951535312, 1.000000000000000000, 0.9510565162951535312, 1.000000000000000000, 0.9510565162951535312, 1.000000000000000000, 0.9510565162951535312, 1.000000000000000000, 0.9510565162951535312, 1.000000000000000000, 0.9510565162951535312, 1.000000000000000000, 0.9510565162951535312, 1.000000000000000000, 0.9510565162951535312, 1.000000000000000000, 0.9510565162951535312, 1.000000000000000000, 0.9510565162951535312, 1.000000000000000000, 0.9510565162951535312, 1.000000000000000000, 0.9510565162951535312, 1.000000000000000000, 0.9510565162951535312, 1.000000000000000000, 0.9510565162951535312, 1.000000000000000000, 0.9510565162951535312, 1.000000000000000000, 0.9510565162951535312, 1.000000000000000000, 0.9510565162951535312, 1.000000000000000000, 0.9510565162951535312, 1.000000000000000000, 0.9510565162951535312, 1.000000000000000000, 0.9510565162951535312, 1.000000000000000000, 0.9510565162951535312, 1.000000000000000000, 0.9510565162951535312, 1.000000000000000000, 0.9510565162951535312, 1.000000000000000000, 0.9510565162951535312, 1.000000000000000000, 0.9510565162951535312, 1.000000000000000000, 0.9510565162951535312, 1.000000000000000000, 0.9510565162951535312, 1.000000000000000000, 0.9510565162951535312, 1.000000000000000000, 0.9510565162951535312, 1.000000000000000000, 0.9510565162951535312, 1.000000000000000000, 0.9510565162951535312, 1.000000000000000000, 0.9510565162951535312, 1.000000000000000000, 0.9510565162951535312, 1.000000000000000000, 0.9510565162951535312, 1.000000000000000000, 0.9510565162951535312, 1.000000000000000000, 0.9510565162951535312, 1.000000000000000000, 0.9510565162951535312, 1.000000000000000000, 0.9510565162951535312, 1.000000000000000000, 0.9510565162951535312, 1.000000000000000000, 0.9510565162951535312, 1.000000000000000000, 0.9510565162951535312, 1.000000000000000000, 0.9510565162951535312, 1.000000000000000000, 0.9510565162951535312, 1.000000000000000000, 0.9510565162951535312, 1.000000000000000000, 0.9510565162951535312, 1.000000000000000000, 0.9510565162951535312, 1.000000000000000000, 0.9510565162951535312, 1.000000000000000000, 0.9510565162951535312, 1.000000000000000000, 0.9510565162951535312, 1.000000000000000000, 0.9510565162951535312, 1.000000000000000000, 0.9510565162951535312, 1.000000000000000000, 0.9510565162951535312, 1.000000000000000000, 0.9510565162951535312, 1.000000000000000000, 0.9510565162951535312, 1.000000000000000000, 0.9510565162951535312, 1.000000000000000000, 0.9510565162951535312, 1.000000000000000000, 0.9510565162951535312, 1.000000000000000000, 0.9510565162951535312, 1.000000000000000000, 0.9510565162951535312, 1.000000000000000000, 0.9510565162951535312, 1.000000000000000000, 0.9510565162951535312, 1.000000000000000000, 0.9510565162951535312, 1.000000000000000000, 0.9510565162951535312, 1.000000000000000000, 0.9510565162951535312, 1.000000000000000000, 0.9510565162951535312, 1.000000000000000000, 0.9510565162951535312, 1.000000000000000000, 0.9510565162951535312, 1.000000000000000000, 0.9510565162951535312, 1.000000000000000000, 0.9510565162951535312, 1.000000000000000000, 0.9510565162951535312, 1.000000000000000000, 0.9510565162951535312, 1.000000000000000000, 0.9510565162951535312, 1.000000000000000000, 0.9510565162951535312, 1.000000000000000000, 0.9510565162951535312, 1.000000000000000000, 0.9510565162951535312, 1.000000000000000000, 0.9510565162951535312, 1.000000000000000000, 0.9510565162951535312, 1.000000000000000000, 0.9510565162951535312, 1.000000000000000000, 0.9510565162951535312, 1.000000000000000000, 0.9510565162951535312, 1.000000000000000000, 0.9510565162951535312, 1.000000000000000000, 0.9510565162951535312, 1.000000000000000000, 0.9510565162951535312, 1.000000000000000000, 0.9510565162951535312, 1.000000000000000000, 0.9510565162951535312, 1.000000000000000000, 0.9510565162951535312, 1.000000000000000000, 0.9510565162951535312, 1.000000000000000000, 0.9510565162951535312, 1.000000000000000000, 0.9510565162951535312, 1.000000000000000000, 0.9510565162951535312, 1.000000000000000000, 0.9510565162951535312, 1.000000000000000000, 0.9510565162951535312, 1.000000000000000000, 0.9510565162951535312, 1.000000000000000000, 0.9510565162951535312, 1.000000000000000000, 0.9510565162951535312, 1.000000000000000000, 0.9510565162951535312, 1.000000000000000000, 0.9510565162951535312, 1.000000000000000000, 0.9510565162951535312, 1.000000000000000000, 0.9510565162951535312, 1.000000000000000000, 0.9510565162951535312, 1.000000000000000000, 0.9510565162951535312, 1.000000000000000000, 0.9510565162951535312, 1.000000000000000000, 0.9510565162951535312, 1.000000000000000000, 0.9510565162951535312, 1.000000000000000000, 0.9510565162951535312, 1.000000000000000000, 0.9510565162951535312, 1.000000000000000000, 0.9510565162951535312, 1.000000000000000000, 0.9510565162951535312, 1.000000000000000000, 0.9510565162951535312, 1.000000000000000000, 0.9510565162951535312, 1.000000000000000000, 0.9510565162951535312, 1.000000000000000000, 0.9510565162951535312, 1.000000000000000000, 0.9510565162951535312, 1.000000000000000000, 0.9510565162951535312, 1.000000000000000000, 0.9510565162951535312, 1.000000000000000000, 0.9510565162951535312, 1.000000000000000000, 0.9510565162951535312, 1.000000000000000000, 0.9510565162951535312, 1.000000000000000000, 0.9510565162951535312, 1.000000000000000000, 0.9510565162951535312, 1.000000000000000000, 0.9510565162951535312, 1.000000000000000000, 0.9510565162951535312, 1.000000000000000000, 0.9510565162951535312, 1.000000000000000000, 0.9510565162951535312, 1.000000000000000000, 0.9510565162951535312, 1.000000000000000000, 0.9510565162951535312, 1.000000000000000000, 0.9510565162951535312, 1.000000000000000000, 0.9510565162951535312, 1.000000000000000000, 0.9510565162951535312, 1.000000000000000000, 0.9510565162951535312, 1.000000000000000000, 0.9510565162951535312, 1.000000000000000000, 0.9510565162951535312, 1.000000000000000000, 0.9510565162951535312, 1.000000000000000000, 0.9510565162951535312, 1.000000000000000000, 0.9510565162951535312, 1.000000000000000000, 0.9510565162951535312, 1.000000000000000000, 0.9510565162951535312, 1.000000000000000000, 0.9510565162951535312, 1.000000000000000000, 0.9510565162951535312, 1.000000000000000000, 0.9510565162951535312, 1.000000000000000000, 0.9510565162951535312, 1.000000000000000000, 0.9510565162951535312, 1.000000000000000000, 0.9510565162951535312, 1.000000000000000000, 0.9510565162951535312, 1.000000000000000000, 0.9510565162951535312, 1.000000000000000000, 0.9510565162951535312, 1.000000000000000000, 0.9510565162951535312, 1.000000000000000000, 0.9510565162951535312, 1.000000000000000000, 0.9510565162951535312, 1.000000000000000000, 0.9510565162951535312, 1.000000000000000000, 0.9510565162951535312, 1.000000000000000000, 0.9510565162951535312, 1.000000000000000000, 0.9510565162951535312, 1.000000000000000000, 0.9510565162951535312, 1.000000000000000000, 0.9510565162951535312, 1.000000000000000000, 0.9510565162951535312, 1.000000000000000000, 0.9510565162951535312, 1.000000000000000000, 0.9510565162951535312, 1.000000000000000000, 0.9510565162951535312, 1.000000000000000000, 0.9510565162951535312, 1.000000000000000000, 0.9510565162951535312, 1.000000000000000000, 0.9510565162951535312, 1.000000000000000000, 0.9510565162951535312, 1.000000000000000000, 0.9510565162951535312, 1.000000000000000000, 0.9510565162951535312, 1.000000000000000000, 0.9510565162951535312, 1.000000000000000000, 0.9510565162951535312, 1.000000000000000000, 0.9510565162951535312, 1.000000000000000000, 0.9510565162951535312, 1.000000000000000000, 0.9510565162951535312, 1.000000000000000000, 0.9510565162951535312, 1.000000000000000000, 0.9510565162951535312, 1.000000000000000000, 0.9510565162951535312, 1.000000000000000000, 0.9510565162951535312, 1.000000000000000000, 0.9510565162951535312, 1.000000000000000000, 0.9510565162951535312, 1.000000000000000000, 0.9510565162951535312, 1.000000000000000000, 0.9510565162951535312, 1.000000000000000000, 0.9510565162951535312, 1.000000000000000000, 0.9510565162951535312, 1.000000000000000000, 0.9510565162951535312, 1.000000000000000000, 0.9510565162951535312, 1.000000000000000000, 0.9510565162951535312, 1.000000000000000000, 0.9510565162951535312, 1.000000000000000000, 0.9510565162951535312, 1.000000000000000000, 0.9510565162951535312, 1.000000000000000000, 0.9510565162951535312, 1.000000000000000000, 0.9510565162951535312, 1.000000000000000000, 0.9510565162951535312, 1.000000000000000000, 0.9510565162951535312, 1.000000000000000000, 0.9510565162951535312, 1.000000000000000000, 0.9510565162951535312, 1.000000000000000000, 0.9510565162951535312, 1.000000000000000000, 0.9510565162951535312, 1.000000000000000000, 0.9510565162951535312, 1.000000000000000000, 0.9510565162951535312, 1.000000000000000000, 0.9510565162951535312, 1.000000000000000000, 0.9510565162951535312, 1.000000000000000000, 0.9510565162951535312, 1.000000000000000000, 0.9510565162951535312, 1.000000000000000000, 0.9510565162951535312, 1.000000000000000000, 0.9510565162951535312, 1.000000000000000000, 0.9510565162951535312, 1.000000000000000000, 0.9510565162951535312, 1.000000000000000000, 0.9510565162951535312, 1.000000000000000000, 0.9510565162951535312, 1.000000000000000000, 0.9510565162951535312, 1.000000000000000000, 0.9510565162951535312, 1.000000000000000000, 0.9510565162951535312, 1.000000000000000000, 0.9510565162951535312, 1.000000000000000000, 0.9510565162951535312, 1.000000000000000000, 0.9510565162951535312, 1.000000000000000000, 0.9510565162951535312, 1.000000000000000000, 0.9510565162951535312, 1.000000000000000000, 0.9510565162951535312, 1.000000000000000000, 0.9510565162951535312, 1.000000000000000000, 0.9510565162951535312, 1.000000000000000000, 0.9510565162951535312, 1.000000000000000000, 0.9510565162951535312, 1.000000000000000000, 0.9510565162951535312, 1.000000000000000000, 0.9510565162951535312, 1.000000000000000000, 0.9510565162951535312, 1.000000000000000000, 0.9510565162951535312, 1.000000000000000000, 0.9510565162951535312, 1.000000000000000000, 0.9510565162951535312, 1.000000000000000000, 0.9510565162951535312, 1.000000000000000000, 0.9510565162951535312, 1.000000000000000000, 0.9510565162951535312, 1.000000000000000000, 0.9510565162951535312, 1.000000000000000000, 0.9510565162951535312, 1.000000000000000000, 0.9510565162951535312, 1.000000000000000000, 0.9510565162951535312, 1.000000000000000000, 0.9510565162951535312, 1.000000000000000000, 0.9510565162951535312, 1.000000000000000000, 0.9510565162951535312, 1.000000000000000000, 0.9510565162951535312, 1.000000000000000000, 0.9510565162951535312, 1.000000000000000000, 0.9510565162951535312, 1.000000000000000000, 0.9510565162951535312, 1.000000000000000000, 0.9510565162951535312, 1.000000000000000000, 0.9510565162951535312, 1.000000000000000000, 0.9510565162951535312, 1.000000000000000000, 0.9510565162951535312, 1.000000000000000000, 0.9510565162951535312, 1.000000000000000000, 0.9510565162951535312, 1.000000000000000000, 0.9510565162951535312, 1.000000000000000000, 0.9510565162951535312, 1.000000000000000000, 0.9510565162951535312, 1.000000000000000000, 0.9510565162951535312, 1.000000000000000000, 0.9510565162951535312, 1.000000000000000000, 0.9510565162951535312, 1.000000000000000000, 0.9510565162951535312, 1.000000000000000000, 0.9510565162951535312, 1.000000000000000000, 0.9510565162951535312, 1.000000000000000000, 0.9510565162951535312, 1.000000000000000000, 0.9510565162951535312, 1.000000000000000000, 0.9510565162951535312, 1.000000000000000000, 0.9510565162951535312, 1.000000000000000000, 0.9510565162951535312, 1.000000000000000000, 0.9510565162951535312, 1.000000000000000000, 0.9510565162951535312, 1.000000000000000000, 0.9510565162951535312, 1.000000000000000000, 0.9510565162951535312, 1.000000000000000000, 0.9510565162951535312, 1.000000000000000000, 0.9510565162951535312, 1.000000000000000000, 0.9510565162951535312, 1.000000000000000000, 0.9510565162951535312, 1.000000000000000000, 0.9510565162951535312, 1.000000000000000000, 0.9510565162951535312, 1.000000000000000000, 0.9510565162951535312, 1.000000000000000000, 0.9510565162951535312, 1.000000000000000000, 0.9510565162951535312, 1.000000000000000000, 0.9510565162951535312, 1.000000000000000000, 0.9510565162951535312, 1.000000000000000000, 0.9510565162951535312, 1.000000000000000000, 0.9510565162951535312, 1.000000000000000000, 0.9510565162951535312, 1.000000000000000000, 0.9510565162951535312, 1.000000000000000000, 0.9510565162951535312, 1.000000000000000000, 0.9510565162951535312, 1.000000000000000000, 0.9510565162951535312, 1.000000000000000000, 0.9510565162951535312, 1.000000000000000000, 0.9510565162951535312, 1.000000000000000000, 0.9510565162951535312, 1.000000000000000000, 0.9510565162951535312, 1.000000000000000000, 0.9510565162951535312, 1.000000000000000000, 0.9510565162951535312, 1.000000000000000000, 0.9510565162951535312, 1.000000000000000000, 0.9510565162951535312, 1.000000000000000000, 0.9510565162951535312, 1.000000000000000000, 0.9510565162951535312, 1.000000000000000000, 0.9510565162951535312, 1.000000000000000000, 0.9510565162951535312, 1.000000000000000000, 0.9510565162951535312, 1.000000000000000000, 0.9510565162951535312, 1.000000000000000000, 0.9510565162951535312, 1.000000000000000000, 0.9510565162951535312, 1.000000000000000000, 0.9510565162951535312, 1.000000000000000000, 0.9510565162951535312, 1.000000000000000000, 0.9510565162951535312, 1.000000000000000000, 0.9510565162951535312, 1.000000000000000000, 0.9510565162951535312, 1.000000000000000000, 0.9510565162951535312, 1.000000000000000000, 0.9510565162951535312, 1.000000000000000000, 0.9510565162951535312, 1.000000000000000000, 0.9510565162951535312, 1.000000000000000000, 0.9510565162951535312, 1.000000000000000000, 0.9510565162951535312, 1.000000000000000000, 0.9510565162951535312, 1.000000000000000000, 0.9510565162951535312, 1.000000000000000000, 0.9510565162951535312, 1.000000000000000000, 0.9510565162951535312, 1.000000000000000000, 0.9510565162951535312, 1.000000000000000000, 0.9510565162951535312, 1.000000000000000000, 0.9510565162951535312, 1.000000000000000000, 0.9510565162951535312, 1.000000000000000000, 0.9510565162951535312, 1.000000000000000000, 0.9510565162951535312, 1.000000000000000000, 0.9510565162951535312, 1.000000000000000000, 0.9510565162951535312, 1.000000000000000000, 0.9510565162951535312, 1.000000000000000000, 0.9510565162951535312, 1.000000000000000000, 0.9510565162951535312, 1.000000000000000000, 0.9510565162951535312, 1.000000000000000000, 0.9510565162951535312, 1.000000000000000000, 0.9510565162951535312, 1.000000000000000000, 0.9510565162951535312, 1.000000000000000000, 0.9510565162951535312, 1.000000000000000000, 0.9510565162951535312, 1.000000000000000000, 0.9510565162951535312, 1.000000000000000000, 0.9510565162951535312, 1.000000000000000000, 0.9510565162951535312, 1.000000000000000000, 0.9510565162951535312, 1.000000000000000000, 0.9510565162951535312, 1.000000000000000000, 0.9510565162951535312, 1.000000000000000000, 0.9510565162951535312, 1.000000000000000000, 0.9510565162951535312, 1.000000000000000000, 0.9510565162951535312, 1.000000000000000000, 0.9510565162951535312, 1.000000000000000000, 0.9510565162951535312, 1.000000000000000000, 0.9510565162951535312, 1.000000000000000000, 0.9510565162951535312, 1.000000000000000000, 0.9510565162951535312, 1.000000000000000000, 0.9510565162951535312, 1.000000000000000000, 0.9510565162951535312, 1.000000000000000000, 0.9510565162951535312, 1.000000000000000000, 0.9510565162951535312, 1.000000000000000000, 0.9510565162951535312, 1.000000000000000000, 0.9510565162951535312, 1.000000000000000000, 0.9510565162951535312, 1.000000000000000000, 0.9510565162951535312, 1.000000000000000000, 0.9510565162951535312, 1.000000000000000000, 0.9510565162951535312, 1.000000000000000000, 0.9510565162951535312, 1.000000000000000000, 0.9510565162951535312, 1.000000000000000000, 0.9510565162951535312, 1.000000000000000000, 0.9510565162951535312, 1.000000000000000000, 0.9510565162951535312, 1.000000000000000000, 0.9510565162951535312, 1.000000000000000000, 0.9510565162951535312, 1.000000000000000000, 0.9510565162951535312, 1.000000000000000000, 0.9510565162951535312, 1.000000000000000000, 0.9510565162951535312, 1.000000000000000000, 0.9510565162951535312, 1.000000000000000000, 0.9510565162951535312, 1.000000000000000000, 0.9510565162951535312, 1.000000000000000000, 0.9510565162951535312, 1.000000000000000000, 0.9510565162951535312, 1.000000000000000000, 0.9510565162951535312, 1.000000000000000000, 0.9510565162951535312, 1.000000000000000000, 0.9510565162951535312, 1.000000000000000000, 0.9510565162951535312, 1.000000000000000000, 0.9510565162951535312, 1.000000000000000000, 0.9510565162951535312, 1.000000000000000000) ) ) 
 REPRESENTATION_ITEM ( '' )  SURFACE ( )  );
#31910 = DIRECTION ( 'NONE',  ( 0.000000000000000000, 0.000000000000000000, 1.000000000000000000 ) ) ;
#31911 = CONICAL_SURFACE ( 'NONE', #10594, 9.000000000000007105, 0.7853981633974500554 ) ;
#31912 = EDGE_CURVE ( 'NONE', #20367, #737, #15203, .T. ) ;
#31913 =( NAMED_UNIT ( * ) SI_UNIT ( $, .STERADIAN. ) SOLID_ANGLE_UNIT ( ) );
#31915 = CARTESIAN_POINT ( 'NONE',  ( 5.590169943749474513, 0.000000000000000000, 0.000000000000000000 ) ) ;
#31914 = AXIS2_PLACEMENT_3D ( 'NONE', #57399, #20816, #9223 ) ;
#31916 = DIRECTION ( 'NONE',  ( 7.080503983578803083E-17, -1.000000000000000000, -0.000000000000000000 ) ) ;
#31917 = CARTESIAN_POINT ( 'NONE',  ( 43.75000000000000000, 18.74999999999998224, 3.750000000000000000 ) ) ;
#31918 = ORIENTED_EDGE ( 'NONE', *, *, #49723, .F. ) ;
#31919 = ORIENTED_EDGE ( 'NONE', *, *, #41307, .T. ) ;
#31920 = CARTESIAN_POINT ( 'NONE',  ( -23.21231517720797655, 117.4999999999999716, 9.500000000000000000 ) ) ;
#31921 = DIRECTION ( 'NONE',  ( 1.000000000000000000, -0.000000000000000000, -0.000000000000000000 ) ) ;
#31922 = LINE ( 'NONE', #21359, #25540 ) ;
#31923 = CIRCLE ( 'NONE', #42084, 5.000000000000000000 ) ;
#31924 = DIRECTION ( 'NONE',  ( -1.000000000000000000, 0.000000000000000000, 0.000000000000000000 ) ) ;
#31925 = ORIENTED_EDGE ( 'NONE', *, *, #61600, .T. ) ;
#31926 =( NAMED_UNIT ( * ) SI_UNIT ( $, .STERADIAN. ) SOLID_ANGLE_UNIT ( ) );
#31927 = EDGE_CURVE ( 'NONE', #46369, #39699, #40037, .T. ) ;
#31928 = CARTESIAN_POINT ( 'NONE',  ( -168.9549999999999841, -7.632228543268599452, 2.479861379858951054 ) ) ;
#31929 = LINE ( 'NONE', #64968, #39759 ) ;
#31930 = DIRECTION ( 'NONE',  ( -0.000000000000000000, -0.000000000000000000, 1.000000000000000000 ) ) ;
#31931 = CARTESIAN_POINT ( 'NONE',  ( -48.20707362346614389, 3.094860106618433360, 9.524999999999991473 ) ) ;
#31932 = AXIS2_PLACEMENT_3D ( 'NONE', #56369, #2865, #24354 ) ;
#31933 = CARTESIAN_POINT ( 'NONE',  ( -164.9949999999999761, -6.826472737025113702, 4.959722759717902107 ) ) ;
#31934 = ORIENTED_EDGE ( 'NONE', *, *, #62379, .T. ) ;
#31935 = CIRCLE ( 'NONE', #55537, 0.2500000000000000000 ) ;
#31936 = CARTESIAN_POINT ( 'NONE',  ( -4.390521455347703217, -1.510510638266201910, 9.000000000000001776 ) ) ;
#31937 = CARTESIAN_POINT ( 'NONE',  ( -8.750000000000001776, 24.74999999999998579, -3.750000000000000000 ) ) ;
#31938 = CARTESIAN_POINT ( 'NONE',  ( -81.20499999999999829, -2.607480562269071545, -8.024999999999991473 ) ) ;
#31939 = DIRECTION ( 'NONE',  ( -0.000000000000000000, -0.000000000000000000, -1.000000000000000000 ) ) ;
#31940 = CARTESIAN_POINT ( 'NONE',  ( -24.21231517720798010, 112.9999999999999858, -7.500000000000000000 ) ) ;
#31941 = CARTESIAN_POINT ( 'NONE',  ( -74.86949037884366476, 35.76270116634893270, -9.842748219889633887 ) ) ;
#31942 = EDGE_CURVE ( 'NONE', #48466, #14271, #33148, .T. ) ;
#31943 = VECTOR ( 'NONE', #16651, 1000.000000000000000 ) ;
#31944 = CARTESIAN_POINT ( 'NONE',  ( -79.04499999999998749, 7.632228543268600340, 2.479861379858949277 ) ) ;
#31945 = CARTESIAN_POINT ( 'NONE',  ( 3.094860106618435136, 134.4049999999999443, -9.525000000000000355 ) ) ;
#31946 = CARTESIAN_POINT ( 'NONE',  ( -135.0570736234661808, 0.000000000000000000, 9.524999999999991473 ) ) ;
#31947 = AXIS2_PLACEMENT_3D ( 'NONE', #8968, #51889, #63473 ) ;
#31948 = AXIS2_PLACEMENT_3D ( 'NONE', #32157, #27192, #38166 ) ;
#31949 = CARTESIAN_POINT ( 'NONE',  ( 2.755511676787088415, -7.000000000000004441, 0.5168645644872222888 ) ) ;
#31950 = FACE_OUTER_BOUND ( 'NONE', #12706, .T. ) ;
#31951 = UNCERTAINTY_MEASURE_WITH_UNIT (LENGTH_MEASURE( 1.000000000000000082E-05 ), #5223, 'distance_accuracy_value', 'NONE');
#31952 =( NAMED_UNIT ( * ) SI_UNIT ( $, .STERADIAN. ) SOLID_ANGLE_UNIT ( ) );
#31953 = CARTESIAN_POINT ( 'NONE',  ( -15.98999599679679839, 146.4999999999999716, 9.500000000000000000 ) ) ;
#31954 = VERTEX_POINT ( 'NONE', #34021 ) ;
#31955 = CYLINDRICAL_SURFACE ( 'NONE', #46079, 15.00000000000000000 ) ;
#31956 = VECTOR ( 'NONE', #59455, 1000.000000000000000 ) ;
#31957 = CYLINDRICAL_SURFACE ( 'NONE', #22484, 1.000000000000000888 ) ;
#31959 = DIRECTION ( 'NONE',  ( 1.000000000000000000, 0.000000000000000000, -1.040834085586083310E-14 ) ) ;
#31958 = LINE ( 'NONE', #5212, #22911 ) ;
#31960 = ORIENTED_EDGE ( 'NONE', *, *, #9938, .F. ) ;
#31961 = EDGE_LOOP ( 'NONE', ( #63811, #29828, #42935, #54884 ) ) ;
#31962 = VECTOR ( 'NONE', #64420, 1000.000000000000000 ) ;
#31963 = AXIS2_PLACEMENT_3D ( 'NONE', #10017, #26168, #30388 ) ;
#31964 = STYLED_ITEM ( 'NONE', ( #65781 ), #31515 ) ;
#31965 =( NAMED_UNIT ( * ) PLANE_ANGLE_UNIT ( ) SI_UNIT ( $, .RADIAN. ) );
#31966 = CARTESIAN_POINT ( 'NONE',  ( 71.49999999999998579, 119.9999999999997868, 7.000000000000000000 ) ) ;
#31967 = FACE_OUTER_BOUND ( 'NONE', #22918, .T. ) ;
#31968 = DIRECTION ( 'NONE',  ( -8.881784197001252323E-16, 0.000000000000000000, 1.000000000000000000 ) ) ;
#31969 = EDGE_LOOP ( 'NONE', ( #36865, #37660, #51495, #57725 ) ) ;
#31970 = CARTESIAN_POINT ( 'NONE',  ( -123.5049999999999955, -6.826472737025113702, -4.959722759717900331 ) ) ;
#31971 = VERTEX_POINT ( 'NONE', #67079 ) ;
#31972 = DIRECTION ( 'NONE',  ( 0.000000000000000000, 0.000000000000000000, 1.000000000000000000 ) ) ;
#31973 =( NAMED_UNIT ( * ) SI_UNIT ( $, .STERADIAN. ) SOLID_ANGLE_UNIT ( ) );
#31974 = ORIENTED_EDGE ( 'NONE', *, *, #42011, .F. ) ;
#31975 = CYLINDRICAL_SURFACE ( 'NONE', #21215, 3.499999999999999556 ) ;
#31976 = DIRECTION ( 'NONE',  ( -0.000000000000000000, -0.000000000000000000, -1.000000000000000000 ) ) ;
#31977 = ORIENTED_EDGE ( 'NONE', *, *, #55194, .F. ) ;
#31978 = DIRECTION ( 'NONE',  ( 1.000000000000000000, 7.703719777548942317E-32, 0.000000000000000000 ) ) ;
#31979 = CARTESIAN_POINT ( 'NONE',  ( 3.094860106618435136, 151.2949999999999875, -9.525000000000000355 ) ) ;
#31980 = FACE_OUTER_BOUND ( 'NONE', #17355, .T. ) ;
#31981 = MECHANICAL_DESIGN_GEOMETRIC_PRESENTATION_REPRESENTATION (  '', ( #29781 ), #55584 ) ;
#31982 = EDGE_LOOP ( 'NONE', ( #46215, #52793, #66252, #43991 ) ) ;
#31983 = AXIS2_PLACEMENT_3D ( 'NONE', #10341, #31772, #37107 ) ;
#31984 = CARTESIAN_POINT ( 'NONE',  ( -3.542344102440326825, 1.863645424029198194, 9.000000000000000000 ) ) ;
#31985 = SURFACE_STYLE_USAGE ( .BOTH. , #22130 ) ;
#31986 = CARTESIAN_POINT ( 'NONE',  ( 27.99999999999998934, 0.000000000000000000, 37.00402776293829987 ) ) ;
#31987 = EDGE_LOOP ( 'NONE', ( #12675, #34945, #51748, #16911 ) ) ;
#31988 = CARTESIAN_POINT ( 'NONE',  ( -6.826472737025120807, 129.3929263765338362, -4.959722759717907437 ) ) ;
#31989 = DIRECTION ( 'NONE',  ( -0.000000000000000000, -0.000000000000000000, 1.000000000000000000 ) ) ;
#31990 = UNCERTAINTY_MEASURE_WITH_UNIT (LENGTH_MEASURE( 1.000000000000000082E-05 ), #38482, 'distance_accuracy_value', 'NONE');
#31991 = CIRCLE ( 'NONE', #65682, 0.5000000000000004441 ) ;
#31992 = SURFACE_STYLE_USAGE ( .BOTH. , #58382 ) ;
#31993 = CARTESIAN_POINT ( 'NONE',  ( -76.75000000000000000, -0.9999999999999995559, 7.000000000000001776 ) ) ;
#31994 = ORIENTED_EDGE ( 'NONE', *, *, #16573, .F. ) ;
#31995 = EDGE_CURVE ( 'NONE', #24250, #11473, #2663, .T. ) ;
#31996 = CARTESIAN_POINT ( 'NONE',  ( 0.000000000000000000, 2.500000000000000000, 0.000000000000000000 ) ) ;
#31997 = ORIENTED_EDGE ( 'NONE', *, *, #16324, .F. ) ;
#31998 = MECHANICAL_DESIGN_GEOMETRIC_PRESENTATION_REPRESENTATION (  '', ( #47781 ), #43316 ) ;
#31999 = DIRECTION ( 'NONE',  ( -1.000000000000000000, 0.000000000000000000, 0.000000000000000000 ) ) ;
#32000 = CARTESIAN_POINT ( 'NONE',  ( 27.99999999999998224, 0.000000000000000000, 72.00402776293822171 ) ) ;
#32001 = COLOUR_RGB ( '', 0.40784314, 0.44705882, 0.49803922) ;
#32002 = CARTESIAN_POINT ( 'NONE',  ( -147.8050000000000068, -8.437984349512085203, 5.166775262442717831E-16 ) ) ;
#32003 = CARTESIAN_POINT ( 'NONE',  ( -176.3070736234661808, -10.01517768586948698, 6.132527647946031529E-16 ) ) ;
#32004 = PRESENTATION_STYLE_ASSIGNMENT (( #21807 ) ) ;
#32005 = UNCERTAINTY_MEASURE_WITH_UNIT (LENGTH_MEASURE( 1.000000000000000082E-05 ), #11715, 'distance_accuracy_value', 'NONE');
#32006 = CARTESIAN_POINT ( 'NONE',  ( -5.356721384544678166, -4.721886399977921478, 0.1324414877861183337 ) ) ;
#32007 = DIRECTION ( 'NONE',  ( 1.000000000000000000, 0.000000000000000000, 0.000000000000000000 ) ) ;
#32008 = DIRECTION ( 'NONE',  ( 1.000000000000000000, 0.000000000000000000, 0.000000000000000000 ) ) ;
#32009 = EDGE_LOOP ( 'NONE', ( #39099, #38793, #65389, #66957 ) ) ;
#32010 = EDGE_CURVE ( 'NONE', #19250, #63248, #37711, .T. ) ;
#32011 = AXIS2_PLACEMENT_3D ( 'NONE', #1228, #38977, #65659 ) ;
#32012 = ORIENTED_EDGE ( 'NONE', *, *, #47488, .T. ) ;
#32013 = CARTESIAN_POINT ( 'NONE',  ( 57.00000000000000000, 15.00000000000000000, -34.49999999999999289 ) ) ;
#32014 = DIRECTION ( 'NONE',  ( -0.000000000000000000, -1.000000000000000000, -0.000000000000000000 ) ) ;
#32015 = CARTESIAN_POINT ( 'NONE',  ( -64.85499999999997556, 4.716976649647094177, 6.492361379858945902 ) ) ;
#32017 = VERTEX_POINT ( 'NONE', #56510 ) ;
#32016 = AXIS2_PLACEMENT_3D ( 'NONE', #2215, #34639, #56099 ) ;
#32018 = DIRECTION ( 'NONE',  ( 1.000000000000000000, 0.000000000000000000, 0.000000000000000000 ) ) ;
#32019 = ADVANCED_FACE ( 'NONE', ( #55115 ), #49875, .T. ) ;
#32020 =( NAMED_UNIT ( * ) PLANE_ANGLE_UNIT ( ) SI_UNIT ( $, .RADIAN. ) );
#32021 = CARTESIAN_POINT ( 'NONE',  ( -30.10526806553660606, -8.499999999999996447, 0.2211649376128430600 ) ) ;
#32022 = DIRECTION ( 'NONE',  ( 0.000000000000000000, 1.000000000000000000, -0.000000000000000000 ) ) ;
#32023 = EDGE_CURVE ( 'NONE', #19539, #2934, #65685, .T. ) ;
#32024 = TOROIDAL_SURFACE ( 'NONE', #6159, 7.500000000000011546, 0.5000000000000000000 ) ;
#32025 = EDGE_CURVE ( 'NONE', #15837, #55021, #61198, .T. ) ;
#32026 = FILL_AREA_STYLE_COLOUR ( '', #53144 ) ;
#32027 = CARTESIAN_POINT ( 'NONE',  ( -97.64292637653380780, -5.598654528085801552, 7.705886871421367523 ) ) ;
#32028 = CIRCLE ( 'NONE', #16345, 0.5000000000000004441 ) ;
#32029 = EDGE_LOOP ( 'NONE', ( #31411, #1186, #26096, #22732 ) ) ;
#32030 =( BOUNDED_CURVE ( )  B_SPLINE_CURVE ( 3, ( #15402, #36861, #47792, #69194 ),
 .UNSPECIFIED., .F., .F. ) 
 B_SPLINE_CURVE_WITH_KNOTS ( ( 4, 4 ),
 ( -7.105427357601001859E-15, 1.570796326794896558 ),
 .UNSPECIFIED. ) 
 CURVE ( )  GEOMETRIC_REPRESENTATION_ITEM ( )  RATIONAL_B_SPLINE_CURVE ( ( 1.000000000000000000, 0.8047378541243632721, 0.8047378541243632721, 1.000000000000000000 ) ) 
 REPRESENTATION_ITEM ( '' )  );
#32031 = EDGE_CURVE ( 'NONE', #39091, #30142, #7374, .T. ) ;
#32032 = DIRECTION ( 'NONE',  ( 0.000000000000000000, 1.350863103983176297E-16, -1.000000000000000000 ) ) ;
#32033 = AXIS2_PLACEMENT_3D ( 'NONE', #24158, #29063, #8348 ) ;
#32034 = SURFACE_STYLE_FILL_AREA ( #49606 ) ;
#32035 =( NAMED_UNIT ( * ) SI_UNIT ( $, .STERADIAN. ) SOLID_ANGLE_UNIT ( ) );
#32036 = CARTESIAN_POINT ( 'NONE',  ( -108.5949999999999847, 2.607480562269072433, 8.024999999999991473 ) ) ;
#32037 = CARTESIAN_POINT ( 'NONE',  ( -10.01517768586949231, 146.1949999999999648, -6.132527647946036459E-16 ) ) ;
#32038 = CARTESIAN_POINT ( 'NONE',  ( -92.39499999999998181, -6.826472737025115478, -4.959722759717899443 ) ) ;
#32039 = CARTESIAN_POINT ( 'NONE',  ( -12.74999999999999822, 4.336808689942017736E-16, 7.000000000000001776 ) ) ;
#32040 = UNCERTAINTY_MEASURE_WITH_UNIT (LENGTH_MEASURE( 1.000000000000000082E-05 ), #12933, 'distance_accuracy_value', 'NONE');
#32041 = PRESENTATION_LAYER_ASSIGNMENT (  '', '', ( #53391 ) ) ;
#32042 = CARTESIAN_POINT ( 'NONE',  ( 72.00000000000000000, 36.32520566882265456, -7.500000000000000000 ) ) ;
#32043 = STYLED_ITEM ( 'NONE', ( #58658 ), #8442 ) ;
#32044 = ORIENTED_EDGE ( 'NONE', *, *, #60106, .F. ) ;
#32045 = CARTESIAN_POINT ( 'NONE',  ( -138.1429263765338078, 5.598654528085800663, -7.705886871421367523 ) ) ;
#32046 = SHAPE_REPRESENTATION_RELATIONSHIP ( 'NONE' , 'NONE' ,  #21747, #47271 ) ;
#32047 = CARTESIAN_POINT ( 'NONE',  ( -147.7449999999999761, 4.716976649647094177, 6.492361379858945902 ) ) ;
#32048 = CARTESIAN_POINT ( 'NONE',  ( -21.02379604162863913, 109.9999999999999858, -10.50000000000000000 ) ) ;
#32049 = AXIS2_PLACEMENT_3D ( 'NONE', #37187, #26570, #11792 ) ;
#32050 = CARTESIAN_POINT ( 'NONE',  ( -66.95707362346617231, 9.058813317711329915, -2.943386871421373119 ) ) ;
#32051 = PRESENTATION_LAYER_ASSIGNMENT (  '', '', ( #24159 ) ) ;
#32052 = CYLINDRICAL_SURFACE ( 'NONE', #40621, 1.000000000000000000 ) ;
#32053 = ORIENTED_EDGE ( 'NONE', *, *, #956, .F. ) ;
#32054 = ORIENTED_EDGE ( 'NONE', *, *, #22570, .F. ) ;
#32055 = CIRCLE ( 'NONE', #28668, 0.2500000000000002220 ) ;
#32056 = CARTESIAN_POINT ( 'NONE',  ( 3.499999999999999112, 34.24999999999998579, -3.750000000000000000 ) ) ;
#32057 = UNCERTAINTY_MEASURE_WITH_UNIT (LENGTH_MEASURE( 1.000000000000000082E-05 ), #49599, 'distance_accuracy_value', 'NONE');
#32058 = CARTESIAN_POINT ( 'NONE',  ( 31.00000000000000000, 42.00000000000000000, -80.00402776293826435 ) ) ;
#32059 = CARTESIAN_POINT ( 'NONE',  ( -48.50000000000000000, 99.99999999999992895, 7.500000000000000000 ) ) ;
#32060 =( NAMED_UNIT ( * ) PLANE_ANGLE_UNIT ( ) SI_UNIT ( $, .RADIAN. ) );
#32061 = CARTESIAN_POINT ( 'NONE',  ( 7.750000000000000000, 33.74999999999998579, -4.000000000000000000 ) ) ;
#32062 =( NAMED_UNIT ( * ) SI_UNIT ( $, .STERADIAN. ) SOLID_ANGLE_UNIT ( ) );
#32063 = EDGE_LOOP ( 'NONE', ( #45258, #61048, #25356, #65360 ) ) ;
#32064 = CARTESIAN_POINT ( 'NONE',  ( -150.9550000000000125, -7.632228543268599452, 2.479861379858951054 ) ) ;
#32065 =( GEOMETRIC_REPRESENTATION_CONTEXT ( 3 ) GLOBAL_UNCERTAINTY_ASSIGNED_CONTEXT ( ( #14420 ) ) GLOBAL_UNIT_ASSIGNED_CONTEXT ( ( #12066, #59911, #33196 ) ) REPRESENTATION_CONTEXT ( 'NONE', 'WORKASPACE' ) );
#32066 = VERTEX_POINT ( 'NONE', #28731 ) ;
#32067 = SURFACE_SIDE_STYLE ('',( #10617 ) ) ;
#32068 = DIRECTION ( 'NONE',  ( 0.000000000000000000, 0.000000000000000000, 1.000000000000000000 ) ) ;
#32069 = ORIENTED_EDGE ( 'NONE', *, *, #20176, .F. ) ;
#32070 = COLOUR_RGB ( '', 0.72549020, 0.75294118, 0.79215686) ;
#32071 = SURFACE_STYLE_USAGE ( .BOTH. , #37401 ) ;
#32072 =( NAMED_UNIT ( * ) SI_UNIT ( $, .STERADIAN. ) SOLID_ANGLE_UNIT ( ) );
#32073 = CARTESIAN_POINT ( 'NONE',  ( 10.01517768586949231, 123.6949999999999932, 1.839758294383810543E-15 ) ) ;
#32074 = DIRECTION ( 'NONE',  ( 0.000000000000000000, 0.000000000000000000, 1.000000000000000000 ) ) ;
#32075 = MECHANICAL_DESIGN_GEOMETRIC_PRESENTATION_REPRESENTATION (  '', ( #17486 ), #14113 ) ;
#32076 = ORIENTED_EDGE ( 'NONE', *, *, #30260, .F. ) ;
#32077 = CARTESIAN_POINT ( 'NONE',  ( 10.01517768586949408, 118.8049999999999926, 1.839758294383810543E-15 ) ) ;
#32078 = CARTESIAN_POINT ( 'NONE',  ( -66.65499999999998693, -7.632228543268600340, -2.479861379858950166 ) ) ;
#32079 = CIRCLE ( 'NONE', #55632, 8.000000000000007105 ) ;
#32080 = CARTESIAN_POINT ( 'NONE',  ( -116.5450000000000017, -7.632228543268600340, -2.479861379858950166 ) ) ;
#32081 = DIRECTION ( 'NONE',  ( 0.000000000000000000, 0.000000000000000000, -1.000000000000000000 ) ) ;
#32082 = ORIENTED_EDGE ( 'NONE', *, *, #2071, .F. ) ;
#32083 = CARTESIAN_POINT ( 'NONE',  ( -3.094860106618432471, 149.7049999999999272, -9.525000000000000355 ) ) ;
#32084 = LINE ( 'NONE', #32406, #69332 ) ;
#32085 = UNCERTAINTY_MEASURE_WITH_UNIT (LENGTH_MEASURE( 1.000000000000000082E-05 ), #6399, 'distance_accuracy_value', 'NONE');
#32086 = FILL_AREA_STYLE ('',( #43398 ) ) ;
#32087 = CARTESIAN_POINT ( 'NONE',  ( 68.00000000000000000, 2.776762340297169183E-15, 10.50000000000000000 ) ) ;
#32088 = FACE_OUTER_BOUND ( 'NONE', #47252, .T. ) ;
#32089 = ADVANCED_FACE ( 'NONE', ( #17854 ), #7985, .F. ) ;
#32090 = CARTESIAN_POINT ( 'NONE',  ( -4.000000000000000000, 4.336808689942018722E-16, -0.000000000000000000 ) ) ;
#32091 = EDGE_LOOP ( 'NONE', ( #13989, #11283, #63155, #19564 ) ) ;
#32092 = SURFACE_STYLE_FILL_AREA ( #57793 ) ;
#32093 = CARTESIAN_POINT ( 'NONE',  ( -171.9549999999999841, -7.632228543268599452, 2.479861379858951054 ) ) ;
#32094 = ORIENTED_EDGE ( 'NONE', *, *, #18379, .T. ) ;
#32095 = CARTESIAN_POINT ( 'NONE',  ( -87.50707362346615525, 8.102448949553176405, 5.886773742842740909 ) ) ;
#32096 = EDGE_CURVE ( 'NONE', #30006, #33741, #56742, .T. ) ;
#32097 = APPLICATION_CONTEXT ( 'automotive_design' ) ;
#32098 = MECHANICAL_DESIGN_GEOMETRIC_PRESENTATION_REPRESENTATION (  '', ( #14130 ), #44491 ) ;
#32099 = DIRECTION ( 'NONE',  ( 0.000000000000000000, -1.000000000000000000, 0.000000000000000000 ) ) ;
#32100 = PRESENTATION_STYLE_ASSIGNMENT (( #31379 ) ) ;
#32101 = DIRECTION ( 'NONE',  ( 1.000000000000000000, 0.000000000000000000, 0.000000000000000000 ) ) ;
#32102 = ORIENTED_EDGE ( 'NONE', *, *, #39837, .T. ) ;
#32103 =( NAMED_UNIT ( * ) SI_UNIT ( $, .STERADIAN. ) SOLID_ANGLE_UNIT ( ) );
#32104 = VECTOR ( 'NONE', #35246, 1000.000000000000000 ) ;
#32105 = SURFACE_SIDE_STYLE ('',( #15270 ) ) ;
#32106 = CARTESIAN_POINT ( 'NONE',  ( -93.80499999999999261, -8.437984349512085203, 5.166775262442717831E-16 ) ) ;
#32107 = ORIENTED_EDGE ( 'NONE', *, *, #67820, .T. ) ;
#32108 = DIRECTION ( 'NONE',  ( -0.000000000000000000, 1.000000000000000000, -0.000000000000000000 ) ) ;
#32109 = EDGE_CURVE ( 'NONE', #45911, #49280, #24136, .T. ) ;
#32110 = CARTESIAN_POINT ( 'NONE',  ( 6.062177826491068622, -2.500000000000000000, -3.500000000000001332 ) ) ;
#32111 = AXIS2_PLACEMENT_3D ( 'NONE', #39626, #3296, #44911 ) ;
#32112 = CARTESIAN_POINT ( 'NONE',  ( -131.0070736234661410, -8.102448949553172852, -5.886773742842741797 ) ) ;
#32113 = VECTOR ( 'NONE', #55504, 1000.000000000000000 ) ;
#32114 = CARTESIAN_POINT ( 'NONE',  ( -63.05707362346617373, 0.000000000000000000, 9.524999999999991473 ) ) ;
#32115 = EDGE_CURVE ( 'NONE', #1748, #2564, #69495, .T. ) ;
#32116 = CARTESIAN_POINT ( 'NONE',  ( -80.99292637653380211, 8.102448949553172852, -5.886773742842744461 ) ) ;
#32117 = ORIENTED_EDGE ( 'NONE', *, *, #63078, .F. ) ;
#32119 = SURFACE_STYLE_USAGE ( .BOTH. , #63769 ) ;
#32118 = FILL_AREA_STYLE ('',( #37454 ) ) ;
#32120 = CARTESIAN_POINT ( 'NONE',  ( -112.1049999999999756, -6.826472737025115478, 4.959722759717900331 ) ) ;
#32121 = CARTESIAN_POINT ( 'NONE',  ( -1.166476076187854022E-15, 119.9449999999999790, 9.525000000000000355 ) ) ;
#32122 = CARTESIAN_POINT ( 'NONE',  ( -114.1449999999999960, -4.716976649647092401, 6.492361379858946790 ) ) ;
#32123 = TOROIDAL_SURFACE ( 'NONE', #1738, 8.999999999999998224, 5.000000000000000000 ) ;
#32124 = AXIS2_PLACEMENT_3D ( 'NONE', #57013, #46871, #8828 ) ;
#32125 = CIRCLE ( 'NONE', #46797, 13.00000000000000178 ) ;
#32127 = CARTESIAN_POINT ( 'NONE',  ( -153.2070736234665844, 3.094860106624618190, 9.524999999995499067 ) ) ;
#32126 = FILL_AREA_STYLE ('',( #20885 ) ) ;
#32128 = VERTEX_POINT ( 'NONE', #31501 ) ;
#32129 = CARTESIAN_POINT ( 'NONE',  ( -163.0429263765338135, -9.058813317711329915, -2.943386871421370898 ) ) ;
#32130 = CARTESIAN_POINT ( 'NONE',  ( -173.3950000000000102, -6.826472737025115478, -4.959722759717899443 ) ) ;
#32131 = DIRECTION ( 'NONE',  ( 0.000000000000000000, 0.000000000000000000, 1.000000000000000000 ) ) ;
#32132 = CARTESIAN_POINT ( 'NONE',  ( -20.71462257042833599, 114.4999999999999574, -10.00000000000000000 ) ) ;
#32133 = SURFACE_SIDE_STYLE ('',( #20892 ) ) ;
#32134 = DIRECTION ( 'NONE',  ( 0.000000000000000000, 0.000000000000000000, -1.000000000000000000 ) ) ;
#32135 = ORIENTED_EDGE ( 'NONE', *, *, #9733, .F. ) ;
#32136 = CARTESIAN_POINT ( 'NONE',  ( -75.89292637653379359, -8.102448949553172852, -5.886773742842741797 ) ) ;
#32137 = CARTESIAN_POINT ( 'NONE',  ( 4.041451884327375232, 1.417096231345241097, -7.000000000000002665 ) ) ;
#32138 = CARTESIAN_POINT ( 'NONE',  ( -166.4929263765338021, -8.102448949553174629, 5.886773742842742685 ) ) ;
#32139 = EDGE_CURVE ( 'NONE', #33557, #26409, #14659, .T. ) ;
#32140 = AXIS2_PLACEMENT_3D ( 'NONE', #62468, #57187, #3689 ) ;
#32141 = CARTESIAN_POINT ( 'NONE',  ( 3.249999999999998668, 36.74999999999999289, 3.750000000000000000 ) ) ;
#32142 = CARTESIAN_POINT ( 'NONE',  ( -9.827790563157511022E-16, 146.5570736234661524, 8.025000000000000355 ) ) ;
#32143 = CARTESIAN_POINT ( 'NONE',  ( 108.3664351561509420, 13.00000000000000178, -18.43563588791578667 ) ) ;
#32144 = AXIS2_PLACEMENT_3D ( 'NONE', #57257, #45371, #40770 ) ;
#32145 = CARTESIAN_POINT ( 'NONE',  ( -183.8050000000000068, -8.437984349512086979, 5.166775262442717831E-16 ) ) ;
#32146 = EDGE_LOOP ( 'NONE', ( #37569, #44750, #38880, #5835 ) ) ;
#32147 = CYLINDRICAL_SURFACE ( 'NONE', #3258, 12.50000000000001066 ) ;
#32148 = CARTESIAN_POINT ( 'NONE',  ( 47.50000000000000000, 14.49137674618942562, -10.00000000000000000 ) ) ;
#32149 = DIRECTION ( 'NONE',  ( -0.000000000000000000, -0.000000000000000000, 1.000000000000000000 ) ) ;
#32150 = DIRECTION ( 'NONE',  ( 0.000000000000000000, -0.000000000000000000, -1.000000000000000000 ) ) ;
#32151 = DIRECTION ( 'NONE',  ( 0.000000000000000000, -1.000000000000000000, 0.000000000000000000 ) ) ;
#32152 = CARTESIAN_POINT ( 'NONE',  ( 7.632228543268608334, 144.4570736234661581, -2.479861379858951942 ) ) ;
#32153 = ORIENTED_EDGE ( 'NONE', *, *, #53382, .F. ) ;
#32154 = CARTESIAN_POINT ( 'NONE',  ( 4.500000000000002665, 24.99999999999998579, 3.750000000000000000 ) ) ;
#32155 = CARTESIAN_POINT ( 'NONE',  ( -97.10499999999998977, -6.826472737025113702, 4.959722759717902107 ) ) ;
#32156 = UNCERTAINTY_MEASURE_WITH_UNIT (LENGTH_MEASURE( 1.000000000000000082E-05 ), #29999, 'distance_accuracy_value', 'NONE');
#32157 = CARTESIAN_POINT ( 'NONE',  ( 17.15973193263811680, -3.000000000000000000, -2.000000000000000000 ) ) ;
#32158 = ORIENTED_EDGE ( 'NONE', *, *, #40446, .F. ) ;
#32159 = DIRECTION ( 'NONE',  ( 0.2413793103448194644, -0.9704308468600220117, 0.000000000000000000 ) ) ;
#32160 = ADVANCED_FACE ( 'NONE', ( #30115 ), #51592, .F. ) ;
#32161 = MECHANICAL_DESIGN_GEOMETRIC_PRESENTATION_REPRESENTATION (  '', ( #10825 ), #20926 ) ;
#32162 =( LENGTH_UNIT ( ) NAMED_UNIT ( * ) SI_UNIT ( .MILLI., .METRE. ) );
#32163 = ADVANCED_FACE ( 'NONE', ( #24841 ), #46356, .F. ) ;
#32164 = CARTESIAN_POINT ( 'NONE',  ( 0.000000000000000000, 1.000000000000000000, 4.000000000000000000 ) ) ;
#32165 = LINE ( 'NONE', #11041, #69298 ) ;
#32166 = AXIS2_PLACEMENT_3D ( 'NONE', #51836, #26467, #25088 ) ;
#32167 = SURFACE_STYLE_USAGE ( .BOTH. , #3742 ) ;
#32168 = ORIENTED_EDGE ( 'NONE', *, *, #44979, .T. ) ;
#32169 = SURFACE_STYLE_FILL_AREA ( #10715 ) ;
#32170 = CARTESIAN_POINT ( 'NONE',  ( -72.44499999999997897, 0.000000000000000000, 8.024999999999991473 ) ) ;
#32171 = EDGE_LOOP ( 'NONE', ( #14196, #50183, #34641, #48498 ) ) ;
#32172 = SURFACE_STYLE_FILL_AREA ( #21247 ) ;
#32173 = DIRECTION ( 'NONE',  ( -0.000000000000000000, -0.000000000000000000, -1.000000000000000000 ) ) ;
#32174 = EDGE_CURVE ( 'NONE', #52175, #19166, #66841, .T. ) ;
#32175 =( NAMED_UNIT ( * ) PLANE_ANGLE_UNIT ( ) SI_UNIT ( $, .RADIAN. ) );
#32176 = ORIENTED_EDGE ( 'NONE', *, *, #54460, .F. ) ;
#32177 = CARTESIAN_POINT ( 'NONE',  ( 31.00000000000001776, 50.00000000000000000, 59.99999999999999289 ) ) ;
#32178 = SURFACE_STYLE_FILL_AREA ( #21252 ) ;
#32179 = CARTESIAN_POINT ( 'NONE',  ( -119.1550000000000011, 7.632228543268600340, 2.479861379858949277 ) ) ;
#32180 = ORIENTED_EDGE ( 'NONE', *, *, #35177, .T. ) ;
#32181 = DIRECTION ( 'NONE',  ( 1.000000000000000000, 0.000000000000000000, -0.000000000000000000 ) ) ;
#32182 = EDGE_LOOP ( 'NONE', ( #18484, #20048, #19093, #52878 ) ) ;
#32183 = EDGE_CURVE ( 'NONE', #5042, #38669, #480, .T. ) ;
#32184 = CARTESIAN_POINT ( 'NONE',  ( -160.0429263765338135, -9.058813317711329915, -2.943386871421370898 ) ) ;
#32185 = CYLINDRICAL_SURFACE ( 'NONE', #51376, 17.00000000000000000 ) ;
#32186 = CARTESIAN_POINT ( 'NONE',  ( -160.8570736234661922, -5.598654528085803328, -7.705886871421366635 ) ) ;
#32187 = CARTESIAN_POINT ( 'NONE',  ( 0.000000000000000000, 124.4449999999999932, -9.525000000000000355 ) ) ;
#32188 = CARTESIAN_POINT ( 'NONE',  ( -97.10707362346617799, 8.102448949553171076, -5.886773742842744461 ) ) ;
#32189 = EDGE_CURVE ( 'NONE', #29900, #23421, #14302, .T. ) ;
#32190 = DIRECTION ( 'NONE',  ( 0.000000000000000000, 0.000000000000000000, -1.000000000000000000 ) ) ;
#32191 = PRODUCT ( 'MAS-684', 'MAS-684', '', ( #1174 ) ) ;
#32192 = ORIENTED_EDGE ( 'NONE', *, *, #15964, .T. ) ;
#32193 = PRESENTATION_STYLE_ASSIGNMENT (( #15688 ) ) ;
#32194 = UNCERTAINTY_MEASURE_WITH_UNIT (LENGTH_MEASURE( 1.000000000000000082E-05 ), #45735, 'distance_accuracy_value', 'NONE');
#32196 =( NAMED_UNIT ( * ) SI_UNIT ( $, .STERADIAN. ) SOLID_ANGLE_UNIT ( ) );
#32195 = DIRECTION ( 'NONE',  ( 1.000000000000000000, 0.000000000000000000, -0.000000000000000000 ) ) ;
#32197 =( GEOMETRIC_REPRESENTATION_CONTEXT ( 3 ) GLOBAL_UNCERTAINTY_ASSIGNED_CONTEXT ( ( #27679 ) ) GLOBAL_UNIT_ASSIGNED_CONTEXT ( ( #458, #33566, #10737 ) ) REPRESENTATION_CONTEXT ( 'NONE', 'WORKASPACE' ) );
#32198 = CARTESIAN_POINT ( 'NONE',  ( -137.9049999999999727, 2.607480562269068880, -8.024999999999993250 ) ) ;
#32199 = SURFACE_STYLE_USAGE ( .BOTH. , #10412 ) ;
#32200 = DIRECTION ( 'NONE',  ( 0.000000000000000000, -1.000000000000000000, 0.000000000000000000 ) ) ;
#32201 = CARTESIAN_POINT ( 'NONE',  ( 23.50000000000001776, 42.00000000000000000, -29.68999999999999417 ) ) ;
#32202 = CARTESIAN_POINT ( 'NONE',  ( -145.4949999999999477, 6.826472737025113702, -4.959722759717902107 ) ) ;
#32203 = VECTOR ( 'NONE', #69380, 1000.000000000000000 ) ;
#32204 = CARTESIAN_POINT ( 'NONE',  ( -140.6949999999999648, -8.437984349512086979, 5.166775262442717831E-16 ) ) ;
#32205 = ORIENTED_EDGE ( 'NONE', *, *, #33504, .F. ) ;
#32206 = SPHERICAL_SURFACE ( 'NONE', #23528, 1.000000000000000000 ) ;
#32207 = SURFACE_SIDE_STYLE ('',( #31849 ) ) ;
#32208 = DIRECTION ( 'NONE',  ( -0.000000000000000000, 1.000000000000000000, -0.000000000000000000 ) ) ;
#32209 = CARTESIAN_POINT ( 'NONE',  ( -54.05499999999999261, -9.827790563157499189E-16, -8.024999999999991473 ) ) ;
#32210 = DIRECTION ( 'NONE',  ( 0.000000000000000000, 0.000000000000000000, 1.000000000000000000 ) ) ;
#32211 = VECTOR ( 'NONE', #19163, 1000.000000000000000 ) ;
#32212 = CARTESIAN_POINT ( 'NONE',  ( -138.5929263765343649, -3.094860106628043894, -9.524999999993006838 ) ) ;
#32213 = PRESENTATION_STYLE_ASSIGNMENT (( #37553 ) ) ;
#32214 =( LENGTH_UNIT ( ) NAMED_UNIT ( * ) SI_UNIT ( .MILLI., .METRE. ) );
#32215 = CARTESIAN_POINT ( 'NONE',  ( -108.8929263765338078, -8.102448949553172852, -5.886773742842741797 ) ) ;
#32216 = DIRECTION ( 'NONE',  ( 1.387778780781445676E-16, -0.9591247405308765961, -0.2829836251474255882 ) ) ;
#32217 = CARTESIAN_POINT ( 'NONE',  ( -153.2929263765341830, 3.094860106611874162, -9.525000000004759215 ) ) ;
#32218 = EDGE_CURVE ( 'NONE', #4086, #41081, #69098, .T. ) ;
#32219 = COLOUR_RGB ( '', 0.31764706, 0.68627451, 0.89019608) ;
#32220 = DIRECTION ( 'NONE',  ( 0.4999999999999997780, -0.8660254037844387076, 0.000000000000000000 ) ) ;
#32221 = LINE ( 'NONE', #26575, #66313 ) ;
#32222 = CARTESIAN_POINT ( 'NONE',  ( 74.50000000000000000, -2.220952357103124925E-14, 6.999999999999999112 ) ) ;
#32223 = FILL_AREA_STYLE ('',( #15720 ) ) ;
#32224 = SURFACE_STYLE_USAGE ( .BOTH. , #58264 ) ;
#32225 = ORIENTED_EDGE ( 'NONE', *, *, #16085, .F. ) ;
#32226 = SURFACE_STYLE_FILL_AREA ( #12144 ) ;
#32227 = CARTESIAN_POINT ( 'NONE',  ( -4.716976649647097730, 115.3570736234661638, -6.492361379858953896 ) ) ;
#32228 = EDGE_CURVE ( 'NONE', #835, #28025, #9565, .T. ) ;
#32229 = CARTESIAN_POINT ( 'NONE',  ( 2.607480562268992941, 138.9070736234661751, -8.025000000000060751 ) ) ;
#32230 = FACE_OUTER_BOUND ( 'NONE', #13086, .T. ) ;
#32231 = VERTEX_POINT ( 'NONE', #15031 ) ;
#32232 = EDGE_LOOP ( 'NONE', ( #56558, #863, #64315, #39363 ) ) ;
#32233 = CIRCLE ( 'NONE', #27740, 0.2500000000000002220 ) ;
#32234 = LINE ( 'NONE', #31882, #54534 ) ;
#32235 = DIRECTION ( 'NONE',  ( 0.000000000000000000, 0.000000000000000000, 1.000000000000000000 ) ) ;
#32236 = EDGE_CURVE ( 'NONE', #63964, #38572, #9748, .T. ) ;
#32237 = CARTESIAN_POINT ( 'NONE',  ( 45.65811388300841855, 10.21937129433612235, -4.000000000000000000 ) ) ;
#32238 = ORIENTED_EDGE ( 'NONE', *, *, #48162, .T. ) ;
#32239 = ADVANCED_FACE ( 'NONE', ( #21654 ), #2762, .T. ) ;
#32240 = CARTESIAN_POINT ( 'NONE',  ( -8.102448949553181734, 126.0049999999999812, -5.886773742842749790 ) ) ;
#32241 = CARTESIAN_POINT ( 'NONE',  ( -184.0000000000000000, -7.358988424933670558, 3.200923985616050071 ) ) ;
#32242 = STYLED_ITEM ( 'NONE', ( #9951 ), #3494 ) ;
#32243 = SURFACE_STYLE_FILL_AREA ( #21328 ) ;
#32244 = CARTESIAN_POINT ( 'NONE',  ( -98.54499999999998749, -7.632228543268600340, -2.479861379858950166 ) ) ;
#32245 = ORIENTED_EDGE ( 'NONE', *, *, #54761, .T. ) ;
#32246 = CARTESIAN_POINT ( 'NONE',  ( 6.612677335615305907, 153.8894900351841102, -5.991805610726354203 ) ) ;
#32247 = EDGE_CURVE ( 'NONE', #9325, #16622, #26896, .T. ) ;
#32248 = ORIENTED_EDGE ( 'NONE', *, *, #39110, .F. ) ;
#32249 = CARTESIAN_POINT ( 'NONE',  ( -7.632228543268607446, 150.5429263765338135, -2.479861379858953718 ) ) ;
#32250 = FILL_AREA_STYLE_COLOUR ( '', #33554 ) ;
#32251 = ADVANCED_FACE ( 'NONE', ( #69168 ), #53342, .T. ) ;
#32252 =( NAMED_UNIT ( * ) SI_UNIT ( $, .STERADIAN. ) SOLID_ANGLE_UNIT ( ) );
#32253 = COLOUR_RGB ( '', 0.66274510, 0.83137255, 0.94901961) ;
#32254 = PRESENTATION_STYLE_ASSIGNMENT (( #26611 ) ) ;
#32255 = CARTESIAN_POINT ( 'NONE',  ( -62.30707362346616662, -10.01517768586948698, 6.132527647946031529E-16 ) ) ;
#32256 = ORIENTED_EDGE ( 'NONE', *, *, #63135, .F. ) ;
#32257 = CARTESIAN_POINT ( 'NONE',  ( -166.2570736234661695, 5.598654528085800663, -7.705886871421367523 ) ) ;
#32258 = CARTESIAN_POINT ( 'NONE',  ( 57.00000000000000000, 5.000000000000000000, 55.00402776293825724 ) ) ;
#32259 = CARTESIAN_POINT ( 'NONE',  ( 6.123233995736766282E-16, 1.999999999999998668, -5.000000000000000000 ) ) ;
#32260 = CARTESIAN_POINT ( 'NONE',  ( 61.99999999999998579, 33.74999999999999289, -3.750000000000000000 ) ) ;
#32261 = SURFACE_SIDE_STYLE ('',( #21712 ) ) ;
#32262 = DIRECTION ( 'NONE',  ( 0.000000000000000000, 0.3420201433256629953, -0.9396926207859104263 ) ) ;
#32263 = CARTESIAN_POINT ( 'NONE',  ( 4.716976649647099507, 116.6429263765338078, -6.492361379858953008 ) ) ;
#32264 = CARTESIAN_POINT ( 'NONE',  ( -8.442136150874093303, 153.4966052368478131, -1.192225150237072651 ) ) ;
#32265 = ORIENTED_EDGE ( 'NONE', *, *, #52741, .F. ) ;
#32266 = ORIENTED_EDGE ( 'NONE', *, *, #66561, .F. ) ;
#32267 = LINE ( 'NONE', #22407, #46722 ) ;
#32268 = CYLINDRICAL_SURFACE ( 'NONE', #65972, 9.524999999999991473 ) ;
#32269 = ORIENTED_EDGE ( 'NONE', *, *, #47742, .T. ) ;
#32270 = CARTESIAN_POINT ( 'NONE',  ( -167.3049999999999784, 8.437984349512085203, -1.550032578732815448E-15 ) ) ;
#32271 = FACE_OUTER_BOUND ( 'NONE', #65845, .T. ) ;
#32272 = EDGE_CURVE ( 'NONE', #18360, #9629, #50195, .T. ) ;
#32273 = LINE ( 'NONE', #20698, #17850 ) ;
#32274 = CARTESIAN_POINT ( 'NONE',  ( -174.8950000000000102, 6.826472737025116366, 4.959722759717898555 ) ) ;
#32275 = CARTESIAN_POINT ( 'NONE',  ( -166.3449999999999989, 7.632228543268599452, -2.479861379858951942 ) ) ;
#32276 = ADVANCED_FACE ( 'NONE', ( #64213 ), #11444, .F. ) ;
#32277 = ORIENTED_EDGE ( 'NONE', *, *, #36348, .T. ) ;
#32278 = CARTESIAN_POINT ( 'NONE',  ( -89.54292637653379927, 9.058813317711329915, 2.943386871421369566 ) ) ;
#32279 = CARTESIAN_POINT ( 'NONE',  ( -15.00000000000000000, 10.90871211463571200, -5.000000000000000000 ) ) ;
#32280 = CARTESIAN_POINT ( 'NONE',  ( -80.00500000000000966, 6.826472737025116366, 4.959722759717898555 ) ) ;
#32281 = FACE_OUTER_BOUND ( 'NONE', #17469, .T. ) ;
#32282 = CARTESIAN_POINT ( 'NONE',  ( -168.3570736234661922, 5.598654528085804216, 7.705886871421366635 ) ) ;
#32283 = CARTESIAN_POINT ( 'NONE',  ( -74.97675674235969723, 35.55359242983254831, -9.655596932388807119 ) ) ;
#32284 = PRESENTATION_LAYER_ASSIGNMENT (  '', '', ( #33397 ) ) ;
#32285 = CIRCLE ( 'NONE', #4191, 2.500000000000002220 ) ;
#32286 = CARTESIAN_POINT ( 'NONE',  ( -82.94499999999999318, -9.827790563157499189E-16, -8.024999999999991473 ) ) ;
#32287 = CARTESIAN_POINT ( 'NONE',  ( 3.094860106618435136, 140.4050000000000011, -9.525000000000000355 ) ) ;
#32288 = PRESENTATION_LAYER_ASSIGNMENT (  '', '', ( #26646 ) ) ;
#32289 = CARTESIAN_POINT ( 'NONE',  ( -134.0070736234661695, -8.102448949553174629, -5.886773742842741797 ) ) ;
#32290 = CARTESIAN_POINT ( 'NONE',  ( 1.401671290772266598, -7.000000000000003553, 0.1093172352041265755 ) ) ;
#32291 = DIRECTION ( 'NONE',  ( -2.312964634635740689E-15, 1.000000000000000000, 0.000000000000000000 ) ) ;
#32292 = CARTESIAN_POINT ( 'NONE',  ( -3.414270897523328241, -1.730686724747262373, -7.000000000000004441 ) ) ;
#32293 = FILL_AREA_STYLE_COLOUR ( '', #19181 ) ;
#32294 = EDGE_LOOP ( 'NONE', ( #23502, #46765, #4531, #51624 ) ) ;
#32295 = CARTESIAN_POINT ( 'NONE',  ( 6.767634268437461742, -2.367558512213881805, -2.278113600022080298 ) ) ;
#32296 = AXIS2_PLACEMENT_3D ( 'NONE', #55392, #6163, #6851 ) ;
#32297 = AXIS2_PLACEMENT_3D ( 'NONE', #53780, #47539, #47182 ) ;
#32298 = DIRECTION ( 'NONE',  ( 0.000000000000000000, -1.000000000000000000, -0.000000000000000000 ) ) ;
#32299 =( NAMED_UNIT ( * ) SI_UNIT ( $, .STERADIAN. ) SOLID_ANGLE_UNIT ( ) );
#32300 = EDGE_CURVE ( 'NONE', #59919, #43730, #59039, .T. ) ;
#32301 = CARTESIAN_POINT ( 'NONE',  ( -2.607480562268991608, 137.4070736234661467, 8.025000000000060751 ) ) ;
#32302 = VERTEX_POINT ( 'NONE', #49123 ) ;
#32303 = ORIENTED_EDGE ( 'NONE', *, *, #57243, .F. ) ;
#32304 = DIRECTION ( 'NONE',  ( 0.000000000000000000, 0.000000000000000000, -1.000000000000000000 ) ) ;
#32305 = CARTESIAN_POINT ( 'NONE',  ( -60.00000000000000000, -2.024042244987997205E-14, -7.000000000000000000 ) ) ;
#32306 = ADVANCED_FACE ( 'NONE', ( #54353 ), #33260, .T. ) ;
#32307 = DIRECTION ( 'NONE',  ( -0.000000000000000000, 1.000000000000000000, -0.000000000000000000 ) ) ;
#32308 = CARTESIAN_POINT ( 'NONE',  ( -45.00000000000000000, 1.166476076187854022E-15, -9.525000000000000355 ) ) ;
#32309 = ORIENTED_EDGE ( 'NONE', *, *, #26740, .T. ) ;
#32310 = CARTESIAN_POINT ( 'NONE',  ( -111.3549999999999898, -4.716976649647093289, -6.492361379858945902 ) ) ;
#32311 = EDGE_LOOP ( 'NONE', ( #41884, #57422, #49893, #7733 ) ) ;
#32312 = CARTESIAN_POINT ( 'NONE',  ( 7.632228543268608334, 129.4570736234661581, -2.479861379858951942 ) ) ;
#32313 = EDGE_CURVE ( 'NONE', #3787, #29002, #34983, .T. ) ;
#32314 = EDGE_LOOP ( 'NONE', ( #18924, #6484, #33474, #16887 ) ) ;
#32315 = PRESENTATION_STYLE_ASSIGNMENT (( #63645 ) ) ;
#32316 = FACE_OUTER_BOUND ( 'NONE', #34869, .T. ) ;
#32317 = ORIENTED_EDGE ( 'NONE', *, *, #54933, .F. ) ;
#32318 = LINE ( 'NONE', #21080, #44526 ) ;
#32319 =( BOUNDED_CURVE ( )  B_SPLINE_CURVE ( 2, ( #40039, #66738, #18556, #41072, #14662, #26572, #16072, #53661, #31505, #21657, #36840 ),
 .UNSPECIFIED., .F., .F. ) 
 B_SPLINE_CURVE_WITH_KNOTS ( ( 3, 2, 2, 2, 2, 3 ),
 ( 0.1956521739130388515, 0.1978260869565170443, 0.1999999999999952649, 0.2021739130434734855, 0.2043478260869517060, 0.2065217391304298988 ),
 .UNSPECIFIED. ) 
 CURVE ( )  GEOMETRIC_REPRESENTATION_ITEM ( )  RATIONAL_B_SPLINE_CURVE ( ( 1.000000000000104361, 0.9510565162950492812, 1.000000000000000000, 0.9510565162951535312, 1.000000000000000000, 0.9510565162951535312, 1.000000000000000000, 0.9510565162951535312, 1.000000000000000000, 0.9510565162952635543, 0.9999999999998899769 ) ) 
 REPRESENTATION_ITEM ( '' )  );
#32320 =( LENGTH_UNIT ( ) NAMED_UNIT ( * ) SI_UNIT ( .MILLI., .METRE. ) );
#32321 = VERTEX_POINT ( 'NONE', #56086 ) ;
#32322 = SURFACE_STYLE_FILL_AREA ( #6285 ) ;
#32323 = CARTESIAN_POINT ( 'NONE',  ( 22.99999999999999289, 0.000000000000000000, -37.00402776293825013 ) ) ;
#32324 =( LENGTH_UNIT ( ) NAMED_UNIT ( * ) SI_UNIT ( .MILLI., .METRE. ) );
#32325 = COLOUR_RGB ( '', 0.40784314, 0.44705882, 0.49803922) ;
#32326 = CARTESIAN_POINT ( 'NONE',  ( -130.9429263765338192, 0.000000000000000000, 9.524999999999991473 ) ) ;
#32327 = VERTEX_POINT ( 'NONE', #1874 ) ;
#32328 = CARTESIAN_POINT ( 'NONE',  ( 2.607480562269071989, 124.5929263765337964, 8.025000000000002132 ) ) ;
#32329 = CARTESIAN_POINT ( 'NONE',  ( -75.40896791924967602, 36.04473888234530676, -9.698837509433410276 ) ) ;
#32330 = AXIS2_PLACEMENT_3D ( 'NONE', #27206, #49081, #44509 ) ;
#32331 = EDGE_CURVE ( 'NONE', #5648, #68323, #34289, .T. ) ;
#32332 = CARTESIAN_POINT ( 'NONE',  ( 0.9115210089146371653, -9.000000000000005329, -1.741499739554841497E-15 ) ) ;
#32333 = DIRECTION ( 'NONE',  ( 0.000000000000000000, 0.000000000000000000, -1.000000000000000000 ) ) ;
#32334 = ORIENTED_EDGE ( 'NONE', *, *, #61347, .T. ) ;
#32335 = CARTESIAN_POINT ( 'NONE',  ( 4.357963766315031684, -6.451785339198144342, 0.7663918866669806595 ) ) ;
#32336 = ORIENTED_EDGE ( 'NONE', *, *, #20827, .T. ) ;
#32337 = CARTESIAN_POINT ( 'NONE',  ( -50.54292637653379217, 9.058813317711329915, 2.943386871421369566 ) ) ;
#32338 = DIRECTION ( 'NONE',  ( 0.000000000000000000, -0.000000000000000000, 1.000000000000000000 ) ) ;
#32339 = DIRECTION ( 'NONE',  ( 0.000000000000000000, -1.000000000000000000, 0.000000000000000000 ) ) ;
#32340 = CARTESIAN_POINT ( 'NONE',  ( -140.3049999999999500, 8.437984349512085203, -1.550032578732815448E-15 ) ) ;
#32341 = CARTESIAN_POINT ( 'NONE',  ( -6.020204320972970535, -1.861307952554190903, -7.572700244129129565 ) ) ;
#32342 = DIRECTION ( 'NONE',  ( 0.000000000000000000, 0.000000000000000000, 1.000000000000000000 ) ) ;
#32343 = SURFACE_STYLE_USAGE ( .BOTH. , #37690 ) ;
#32344 = CARTESIAN_POINT ( 'NONE',  ( 41.01803665359489770, 107.7206116573237580, 3.151333386623630606 ) ) ;
#32345 = ORIENTED_EDGE ( 'NONE', *, *, #24064, .F. ) ;
#32346 = ORIENTED_EDGE ( 'NONE', *, *, #36815, .F. ) ;
#32347 = FACE_OUTER_BOUND ( 'NONE', #36851, .T. ) ;
#32348 = CARTESIAN_POINT ( 'NONE',  ( -60.95499999999998408, -7.632228543268599452, 2.479861379858951054 ) ) ;
#32349 = ORIENTED_EDGE ( 'NONE', *, *, #31756, .F. ) ;
#32350 =( LENGTH_UNIT ( ) NAMED_UNIT ( * ) SI_UNIT ( .MILLI., .METRE. ) );
#32351 = FACE_OUTER_BOUND ( 'NONE', #21901, .T. ) ;
#32352 = CARTESIAN_POINT ( 'NONE',  ( 36.00000000000002842, 5.000000000000000000, 29.00402776293825724 ) ) ;
#32353 = SURFACE_STYLE_FILL_AREA ( #58761 ) ;
#32354 = EDGE_CURVE ( 'NONE', #54975, #23306, #42234, .T. ) ;
#32355 = CARTESIAN_POINT ( 'NONE',  ( 0.000000000000000000, 36.74999999999999289, 3.750000000000000000 ) ) ;
#32356 = ORIENTED_EDGE ( 'NONE', *, *, #25415, .T. ) ;
#32357 = CARTESIAN_POINT ( 'NONE',  ( 0.000000000000000000, 87.30187232391182306, 8.025000000000000355 ) ) ;
#32358 = LINE ( 'NONE', #5277, #55089 ) ;
#32359 = DIRECTION ( 'NONE',  ( 0.000000000000000000, -1.000000000000000000, 0.000000000000000000 ) ) ;
#32360 = CARTESIAN_POINT ( 'NONE',  ( -107.6949999999999790, -8.437984349512086979, 5.166775262442717831E-16 ) ) ;
#32361 = CARTESIAN_POINT ( 'NONE',  ( -8.102448949553181734, 157.8950000000000102, -5.886773742842749790 ) ) ;
#32362 = CARTESIAN_POINT ( 'NONE',  ( -86.54499999999998749, -7.632228543268600340, -2.479861379858950166 ) ) ;
#32363 = SURFACE_SIDE_STYLE ('',( #59109 ) ) ;
#32364 = VECTOR ( 'NONE', #69020, 1000.000000000000000 ) ;
#32365 = DIRECTION ( 'NONE',  ( 1.000000000000000000, 0.000000000000000000, 0.000000000000000000 ) ) ;
#32366 = CARTESIAN_POINT ( 'NONE',  ( 4.000000000000001776, 43.00000000000000000, -90.00000000000000000 ) ) ;
#32367 =( LENGTH_UNIT ( ) NAMED_UNIT ( * ) SI_UNIT ( .MILLI., .METRE. ) );
#32368 = VERTEX_POINT ( 'NONE', #1529 ) ;
#32369 = CARTESIAN_POINT ( 'NONE',  ( -132.2929263765338135, 3.094860106618428031, -9.524999999999993250 ) ) ;
#32370 = CARTESIAN_POINT ( 'NONE',  ( -148.1950000000000216, 8.437984349512085203, -1.550032578732815448E-15 ) ) ;
#32371 = EDGE_CURVE ( 'NONE', #66072, #52602, #50475, .T. ) ;
#32372 = FACE_OUTER_BOUND ( 'NONE', #55596, .T. ) ;
#32373 = FACE_OUTER_BOUND ( 'NONE', #52787, .T. ) ;
#32374 = ORIENTED_EDGE ( 'NONE', *, *, #34069, .T. ) ;
#32375 = EDGE_LOOP ( 'NONE', ( #14, #54186 ) ) ;
#32376 = FACE_OUTER_BOUND ( 'NONE', #36290, .T. ) ;
#32377 = CARTESIAN_POINT ( 'NONE',  ( 5.885195493260862776, -2.499999999999998668, 3.806542393196804763 ) ) ;
#32378 = CARTESIAN_POINT ( 'NONE',  ( -132.6570736234661751, 9.058813317711329915, 2.943386871421369566 ) ) ;
#32379 = CARTESIAN_POINT ( 'NONE',  ( -45.00000000000000000, 9.518682052515954339, 6.447728916822488721 ) ) ;
#32380 = DIRECTION ( 'NONE',  ( 0.000000000000000000, 0.000000000000000000, -1.000000000000000000 ) ) ;
#32381 = AXIS2_PLACEMENT_3D ( 'NONE', #61172, #18624, #44701 ) ;
#32382 = CARTESIAN_POINT ( 'NONE',  ( -117.1429263765337936, 5.598654528085800663, -7.705886871421367523 ) ) ;
#32383 = FACE_OUTER_BOUND ( 'NONE', #1664, .T. ) ;
#32384 = VERTEX_POINT ( 'NONE', #7898 ) ;
#32385 = CARTESIAN_POINT ( 'NONE',  ( -151.4049999999999443, -2.607480562269069768, 8.024999999999991473 ) ) ;
#32386 = EDGE_CURVE ( 'NONE', #20808, #10638, #33595, .T. ) ;
#32387 = ORIENTED_EDGE ( 'NONE', *, *, #5211, .F. ) ;
#32388 = CARTESIAN_POINT ( 'NONE',  ( 4.041451884327376121, 7.000000000000007105, 1.082903768654759569 ) ) ;
#32389 = LINE ( 'NONE', #20830, #21983 ) ;
#32390 = EDGE_LOOP ( 'NONE', ( #8490, #58916, #47941, #6397 ) ) ;
#32391 = CARTESIAN_POINT ( 'NONE',  ( -57.11117894258828898, -7.808072229298645084, -1.023575524669360748 ) ) ;
#32392 = EDGE_CURVE ( 'NONE', #69157, #7947, #23096, .T. ) ;
#32393 = CARTESIAN_POINT ( 'NONE',  ( -60.00000000000000000, -2.024042244987997205E-14, -12.00000000000000000 ) ) ;
#32394 = CARTESIAN_POINT ( 'NONE',  ( 9.058813317711338797, 123.8449999999999847, -2.943386871421372675 ) ) ;
#32395 = SURFACE_STYLE_USAGE ( .BOTH. , #15572 ) ;
#32396 = EDGE_LOOP ( 'NONE', ( #32838, #49550, #26745, #13359 ) ) ;
#32397 = LINE ( 'NONE', #16617, #20642 ) ;
#32399 = EDGE_CURVE ( 'NONE', #26318, #31846, #18797, .T. ) ;
#32398 = CARTESIAN_POINT ( 'NONE',  ( 9.058813317711337021, 133.6550000000000011, 2.943386871421375783 ) ) ;
#32400 = CARTESIAN_POINT ( 'NONE',  ( -62.15499999999998693, 7.632228543268600340, 2.479861379858949277 ) ) ;
#32401 = CONICAL_SURFACE ( 'NONE', #29019, 6.999999999999997335, 0.7853981633974500554 ) ;
#32402 = CARTESIAN_POINT ( 'NONE',  ( -123.5949999999999704, 2.607480562269073321, 8.024999999999991473 ) ) ;
#32403 = CARTESIAN_POINT ( 'NONE',  ( -55.11713571482079033, -8.499999999999996447, 6.664929171799898633 ) ) ;
#32404 = VERTEX_POINT ( 'NONE', #18119 ) ;
#32405 = CARTESIAN_POINT ( 'NONE',  ( 5.598654528085805993, 145.3549999999999898, 7.705886871421374629 ) ) ;
#32406 = CARTESIAN_POINT ( 'NONE',  ( 21.25000000000000711, 22.24999999999998224, -4.000000000000000000 ) ) ;
#32407 = SURFACE_STYLE_FILL_AREA ( #32086 ) ;
#32408 = AXIS2_PLACEMENT_3D ( 'NONE', #68887, #31565, #21024 ) ;
#32409 = EDGE_CURVE ( 'NONE', #16875, #8380, #20844, .T. ) ;
#32410 = CARTESIAN_POINT ( 'NONE',  ( 15.98999599679679839, 146.4999999999999716, 7.500000000000000000 ) ) ;
#32411 = DIRECTION ( 'NONE',  ( -1.000000000000000000, 4.336808689941999001E-16, -0.000000000000000000 ) ) ;
#32412 = STYLED_ITEM ( 'NONE', ( #4488 ), #19990 ) ;
#32413 = FACE_OUTER_BOUND ( 'NONE', #45210, .T. ) ;
#32414 = ORIENTED_EDGE ( 'NONE', *, *, #5321, .F. ) ;
#32415 = VECTOR ( 'NONE', #1650, 1000.000000000000000 ) ;
#32416 =( NAMED_UNIT ( * ) SI_UNIT ( $, .STERADIAN. ) SOLID_ANGLE_UNIT ( ) );
#32417 = CARTESIAN_POINT ( 'NONE',  ( -176.4550000000000125, 7.632228543268599452, -2.479861379858951942 ) ) ;
#32418 = ORIENTED_EDGE ( 'NONE', *, *, #35095, .F. ) ;
#32419 = CARTESIAN_POINT ( 'NONE',  ( 0.000000000000000000, -2.500000000000000000, 0.000000000000000000 ) ) ;
#32420 = PRESENTATION_LAYER_ASSIGNMENT (  '', '', ( #50410 ) ) ;
#32421 =( BOUNDED_CURVE ( )  B_SPLINE_CURVE ( 2, ( #4088, #15059, #10450, #48115, #5146, #62846, #14686, #26592, #4434, #36158, #25554 ),
 .UNSPECIFIED., .F., .F. ) 
 B_SPLINE_CURVE_WITH_KNOTS ( ( 3, 2, 2, 2, 2, 3 ),
 ( 0.5326086956521615123, 0.5347826086956397607, 0.5369565217391178980, 0.5391304347825961463, 0.5413043478260742836, 0.5434782608695525319 ),
 .UNSPECIFIED. ) 
 CURVE ( )  GEOMETRIC_REPRESENTATION_ITEM ( )  RATIONAL_B_SPLINE_CURVE ( ( 1.000000000000279998, 0.9510565162948735329, 1.000000000000000000, 0.9510565162951535312, 1.000000000000000000, 0.9510565162951535312, 1.000000000000000000, 0.9510565162951535312, 1.000000000000000000, 0.9510565162954385254, 0.9999999999997150057 ) ) 
 REPRESENTATION_ITEM ( '' )  );
#32422 = DIRECTION ( 'NONE',  ( 0.000000000000000000, -0.000000000000000000, 1.000000000000000000 ) ) ;
#32423 = EDGE_LOOP ( 'NONE', ( #1691, #17224, #29185, #48969, #32387 ) ) ;
#32424 = MECHANICAL_DESIGN_GEOMETRIC_PRESENTATION_REPRESENTATION (  '', ( #13345 ), #24581 ) ;
#32425 = AXIS2_PLACEMENT_3D ( 'NONE', #19025, #29242, #50723 ) ;
#32426 = CARTESIAN_POINT ( 'NONE',  ( -4.041451884327381450, -7.000000000000002665, 1.082903768654759791 ) ) ;
#32427 = PRESENTATION_STYLE_ASSIGNMENT (( #64461 ) ) ;
#32428 = CARTESIAN_POINT ( 'NONE',  ( -85.85499999999998977, 4.716976649647094177, 6.492361379858945902 ) ) ;
#32429 = ORIENTED_EDGE ( 'NONE', *, *, #64087, .T. ) ;
#32430 = DIRECTION ( 'NONE',  ( 0.000000000000000000, 0.000000000000000000, -1.000000000000000000 ) ) ;
#32431 = COLOUR_RGB ( '', 0.72549020, 0.75294118, 0.79215686) ;
#32432 = PLANE ( 'NONE',  #10410 ) ;
#32433 = CARTESIAN_POINT ( 'NONE',  ( -61.10707362346615668, 8.102448949553171076, -5.886773742842744461 ) ) ;
#32434 = DIRECTION ( 'NONE',  ( -0.000000000000000000, 1.000000000000000000, -0.000000000000000000 ) ) ;
#32435 = ORIENTED_EDGE ( 'NONE', *, *, #13825, .T. ) ;
#32436 = FILL_AREA_STYLE ('',( #387 ) ) ;
#32437 = MECHANICAL_DESIGN_GEOMETRIC_PRESENTATION_REPRESENTATION (  '', ( #5456 ), #29060 ) ;
#32439 = DIRECTION ( 'NONE',  ( -0.000000000000000000, -0.000000000000000000, 1.000000000000000000 ) ) ;
#32438 = SURFACE_STYLE_FILL_AREA ( #64814 ) ;
#32440 = CARTESIAN_POINT ( 'NONE',  ( -108.5049999999999812, -6.826472737025115478, -4.959722759717899443 ) ) ;
#32441 = CARTESIAN_POINT ( 'NONE',  ( -9.058813317711338797, 131.3449999999999989, 2.943386871421373563 ) ) ;
#32442 = CARTESIAN_POINT ( 'NONE',  ( -111.7449999999999903, 4.716976649647094177, 6.492361379858945902 ) ) ;
#32443 = SURFACE_SIDE_STYLE ('',( #49346 ) ) ;
#32444 = CARTESIAN_POINT ( 'NONE',  ( -17.75000000000000711, 30.74999999999999289, -3.750000000000000000 ) ) ;
#32445 = AXIS2_PLACEMENT_3D ( 'NONE', #45221, #54078, #13501 ) ;
#32446 = CARTESIAN_POINT ( 'NONE',  ( -165.2929263765338135, 3.094860106618428031, -9.524999999999993250 ) ) ;
#32447 = CARTESIAN_POINT ( 'NONE',  ( -177.4449999999999932, 0.000000000000000000, 8.024999999999991473 ) ) ;
#32448 = AXIS2_PLACEMENT_3D ( 'NONE', #66632, #24060, #65932 ) ;
#32449 = ADVANCED_FACE ( 'NONE', ( #12827 ), #65606, .F. ) ;
#32450 = VECTOR ( 'NONE', #10419, 1000.000000000000000 ) ;
#32451 = VECTOR ( 'NONE', #49486, 1000.000000000000000 ) ;
#32452 = CARTESIAN_POINT ( 'NONE',  ( 96.10348817448819148, 5.000000000000000000, 27.38099488609881149 ) ) ;
#32453 = CARTESIAN_POINT ( 'NONE',  ( -61.49292637653379501, -8.102448949553174629, 5.886773742842742685 ) ) ;
#32454 =( NAMED_UNIT ( * ) PLANE_ANGLE_UNIT ( ) SI_UNIT ( $, .RADIAN. ) );
#32455 = VERTEX_POINT ( 'NONE', #12472 ) ;
#32456 = CARTESIAN_POINT ( 'NONE',  ( -74.24292637653380211, 5.598654528085804216, 7.705886871421366635 ) ) ;
#32457 = AXIS2_PLACEMENT_3D ( 'NONE', #19177, #52623, #4375 ) ;
#32459 = EDGE_CURVE ( 'NONE', #23204, #20924, #32079, .T. ) ;
#32458 = DIRECTION ( 'NONE',  ( 1.000000000000000000, 0.000000000000000000, 0.000000000000000000 ) ) ;
#32460 = CARTESIAN_POINT ( 'NONE',  ( -74.99999999999998579, 50.00000000000000000, 6.999999999999988454 ) ) ;
#32461 = EDGE_CURVE ( 'NONE', #63556, #60379, #1168, .T. ) ;
#32462 = SURFACE_SIDE_STYLE ('',( #10356 ) ) ;
#32463 = CARTESIAN_POINT ( 'NONE',  ( -148.5570736234661808, -1.166476076187852838E-15, -9.524999999999991473 ) ) ;
#32464 = AXIS2_PLACEMENT_3D ( 'NONE', #32048, #985, #48962 ) ;
#32465 = ADVANCED_FACE ( 'NONE', ( #6860 ), #44201, .F. ) ;
#32466 = CARTESIAN_POINT ( 'NONE',  ( -182.6049999999999613, 6.826472737025113702, -4.959722759717902107 ) ) ;
#32467 = EDGE_CURVE ( 'NONE', #45842, #52933, #22436, .T. ) ;
#32468 = ORIENTED_EDGE ( 'NONE', *, *, #64937, .F. ) ;
#32469 = LINE ( 'NONE', #27183, #52736 ) ;
#32470 = SURFACE_SIDE_STYLE ('',( #36779 ) ) ;
#32471 = EDGE_CURVE ( 'NONE', #2398, #32974, #62043, .T. ) ;
#32472 = DIRECTION ( 'NONE',  ( 0.000000000000000000, 0.000000000000000000, 1.000000000000000000 ) ) ;
#32473 =( LENGTH_UNIT ( ) NAMED_UNIT ( * ) SI_UNIT ( .MILLI., .METRE. ) );
#32474 = AXIS2_PLACEMENT_3D ( 'NONE', #46960, #8591, #52558 ) ;
#32475 = CARTESIAN_POINT ( 'NONE',  ( 2.607480562269071989, 146.7070736234661013, 8.025000000000002132 ) ) ;
#32476 = APPLICATION_CONTEXT ( 'automotive_design' ) ;
#32477 = ORIENTED_EDGE ( 'NONE', *, *, #44832, .F. ) ;
#32479 = ADVANCED_FACE ( 'NONE', ( #13873, #63451 ), #57840, .T. ) ;
#32478 = CARTESIAN_POINT ( 'NONE',  ( 8.437984349512095861, 137.1929263765338192, 1.550032578732816828E-15 ) ) ;
#32480 = CARTESIAN_POINT ( 'NONE',  ( -95.30499999999997840, 8.437984349512086979, -1.550032578732815448E-15 ) ) ;
#32481 = AXIS2_PLACEMENT_3D ( 'NONE', #4766, #53330, #9736 ) ;
#32482 = DIRECTION ( 'NONE',  ( 0.000000000000000000, 1.000000000000000000, 0.000000000000000000 ) ) ;
#32483 = ORIENTED_EDGE ( 'NONE', *, *, #10985, .T. ) ;
#32484 = PRESENTATION_STYLE_ASSIGNMENT (( #11038 ) ) ;
#32485 = CARTESIAN_POINT ( 'NONE',  ( -127.7929263765345240, -3.094860106606396322, 9.525000000008734702 ) ) ;
#32486 = DIRECTION ( 'NONE',  ( -1.000000000000000000, -0.000000000000000000, -0.000000000000000000 ) ) ;
#32487 = SURFACE_SIDE_STYLE ('',( #58904 ) ) ;
#32488 = ORIENTED_EDGE ( 'NONE', *, *, #4924, .T. ) ;
#32489 = MECHANICAL_DESIGN_GEOMETRIC_PRESENTATION_REPRESENTATION (  '', ( #59452 ), #11163 ) ;
#32491 = CARTESIAN_POINT ( 'NONE',  ( -63.29499999999998749, -2.607480562269069768, 8.024999999999991473 ) ) ;
#32490 = AXIS2_PLACEMENT_3D ( 'NONE', #13557, #4035, #46680 ) ;
#32492 = ORIENTED_EDGE ( 'NONE', *, *, #6903, .T. ) ;
#32493 = CARTESIAN_POINT ( 'NONE',  ( -49.64292637653380780, -5.598654528085801552, 7.705886871421367523 ) ) ;
#32494 = LINE ( 'NONE', #4362, #25160 ) ;
#32495 = PRESENTATION_LAYER_ASSIGNMENT (  '', '', ( #40364 ) ) ;
#32496 = ORIENTED_EDGE ( 'NONE', *, *, #33058, .T. ) ;
#32497 = FILL_AREA_STYLE_COLOUR ( '', #64005 ) ;
#32498 = ORIENTED_EDGE ( 'NONE', *, *, #62353, .T. ) ;
#32499 = PRESENTATION_LAYER_ASSIGNMENT (  '', '', ( #43807 ) ) ;
#32500 = DIRECTION ( 'NONE',  ( -0.000000000000000000, -0.000000000000000000, 1.000000000000000000 ) ) ;
#32501 = CARTESIAN_POINT ( 'NONE',  ( -115.5549999999999926, 0.000000000000000000, 8.024999999999991473 ) ) ;
#32502 = ORIENTED_EDGE ( 'NONE', *, *, #50704, .T. ) ;
#32503 = CARTESIAN_POINT ( 'NONE',  ( -73.64292637653380780, -5.598654528085801552, 7.705886871421367523 ) ) ;
#32504 = EDGE_LOOP ( 'NONE', ( #64634, #64778, #48897, #49073 ) ) ;
#32505 = AXIS2_PLACEMENT_3D ( 'NONE', #15699, #37181, #15378 ) ;
#32506 =( NAMED_UNIT ( * ) SI_UNIT ( $, .STERADIAN. ) SOLID_ANGLE_UNIT ( ) );
#32507 = CIRCLE ( 'NONE', #31353, 0.2500000000000002220 ) ;
#32508 = CARTESIAN_POINT ( 'NONE',  ( -160.5570736234661808, -1.166476076187852838E-15, -9.524999999999991473 ) ) ;
#32509 = CIRCLE ( 'NONE', #10051, 0.5000000000000004441 ) ;
#32510 = CARTESIAN_POINT ( 'NONE',  ( 10.01517768586949408, 129.6949999999999648, 1.839758294383810543E-15 ) ) ;
#32511 = CARTESIAN_POINT ( 'NONE',  ( -96.65707362346617515, 9.058813317711329915, 2.943386871421369566 ) ) ;
#32512 = EDGE_CURVE ( 'NONE', #49909, #52976, #48946, .T. ) ;
#32513 =( GEOMETRIC_REPRESENTATION_CONTEXT ( 3 ) GLOBAL_UNCERTAINTY_ASSIGNED_CONTEXT ( ( #10218 ) ) GLOBAL_UNIT_ASSIGNED_CONTEXT ( ( #37828, #27867, #33195 ) ) REPRESENTATION_CONTEXT ( 'NONE', 'WORKASPACE' ) );
#32514 = CARTESIAN_POINT ( 'NONE',  ( 4.286263797015733637E-16, -2.500000000000000000, 3.499999999999997780 ) ) ;
#32515 = EDGE_LOOP ( 'NONE', ( #64371, #27027 ) ) ;
#32516 = VECTOR ( 'NONE', #26319, 1000.000000000000000 ) ;
#32517 = FACE_OUTER_BOUND ( 'NONE', #44407, .T. ) ;
#32519 = SURFACE_SIDE_STYLE ('',( #5108 ) ) ;
#32518 = DIRECTION ( 'NONE',  ( -1.000000000000000000, 0.000000000000000000, 0.000000000000000000 ) ) ;
#32520 = DIRECTION ( 'NONE',  ( -1.000000000000000000, 0.000000000000000000, 0.000000000000000000 ) ) ;
#32521 = CARTESIAN_POINT ( 'NONE',  ( -144.5049999999999670, -6.826472737025115478, -4.959722759717899443 ) ) ;
#32522 = FILL_AREA_STYLE ('',( #16739 ) ) ;
#32523 = CARTESIAN_POINT ( 'NONE',  ( 3.000000000000002665, 34.80256050929376954, -80.00402776293826435 ) ) ;
#32524 = FILL_AREA_STYLE ('',( #11075 ) ) ;
#32525 = CARTESIAN_POINT ( 'NONE',  ( -146.9950000000000045, -6.826472737025115478, 4.959722759717900331 ) ) ;
#32526 = AXIS2_PLACEMENT_3D ( 'NONE', #52484, #35235, #66910 ) ;
#32527 = CARTESIAN_POINT ( 'NONE',  ( -136.3449999999999989, 7.632228543268599452, -2.479861379858951942 ) ) ;
#32528 = VERTEX_POINT ( 'NONE', #30366 ) ;
#32529 = AXIS2_PLACEMENT_3D ( 'NONE', #16668, #49038, #46717 ) ;
#32530 = CARTESIAN_POINT ( 'NONE',  ( 45.00000000000000000, 10.69371294334678879, -3.912397846414704450 ) ) ;
#32531 =( NAMED_UNIT ( * ) PLANE_ANGLE_UNIT ( ) SI_UNIT ( $, .RADIAN. ) );
#32532 = LINE ( 'NONE', #22697, #26023 ) ;
#32533 = UNCERTAINTY_MEASURE_WITH_UNIT (LENGTH_MEASURE( 1.000000000000000082E-05 ), #2335, 'distance_accuracy_value', 'NONE');
#32534 = CARTESIAN_POINT ( 'NONE',  ( -53.30499999999998550, 8.437984349512085203, -1.550032578732815448E-15 ) ) ;
#32535 = DIRECTION ( 'NONE',  ( 1.000000000000000000, -0.000000000000000000, 0.000000000000000000 ) ) ;
#32536 = AXIS2_PLACEMENT_3D ( 'NONE', #63085, #46963, #16915 ) ;
#32537 = CARTESIAN_POINT ( 'NONE',  ( -58.94499999999998607, -9.827790563157499189E-16, -8.024999999999991473 ) ) ;
#32538 = EDGE_CURVE ( 'NONE', #35876, #6894, #64577, .T. ) ;
#32539 = CARTESIAN_POINT ( 'NONE',  ( -103.4070736234671699, 3.094860106602026040, -9.525000000011910828 ) ) ;
#32540 = SURFACE_SIDE_STYLE ('',( #37554 ) ) ;
#32541 = DIRECTION ( 'NONE',  ( 1.000000000000000000, 0.000000000000000000, 0.000000000000000000 ) ) ;
#32542 =( GEOMETRIC_REPRESENTATION_CONTEXT ( 3 ) GLOBAL_UNCERTAINTY_ASSIGNED_CONTEXT ( ( #11673 ) ) GLOBAL_UNIT_ASSIGNED_CONTEXT ( ( #5090, #69464, #30777 ) ) REPRESENTATION_CONTEXT ( 'NONE', 'WORKASPACE' ) );
#32543 = CIRCLE ( 'NONE', #61756, 0.2500000000000002220 ) ;
#32544 = CARTESIAN_POINT ( 'NONE',  ( -106.1929263765338050, -10.01517768586948698, 6.132527647946031529E-16 ) ) ;
#32545 = CARTESIAN_POINT ( 'NONE',  ( -6.799999999999981171, 26.00000000000000000, -24.00000000000001066 ) ) ;
#32546 = EDGE_CURVE ( 'NONE', #15417, #56786, #67693, .T. ) ;
#32547 = CARTESIAN_POINT ( 'NONE',  ( -184.0000000000000000, 0.000000000000000000, -8.524999999999977263 ) ) ;
#32548 = CARTESIAN_POINT ( 'NONE',  ( 61.74999999999998579, 30.99999999999999289, 3.750000000000000000 ) ) ;
#32549 =( NAMED_UNIT ( * ) SI_UNIT ( $, .STERADIAN. ) SOLID_ANGLE_UNIT ( ) );
#32550 = CARTESIAN_POINT ( 'NONE',  ( -71.75000000000000000, -0.9999999999999995559, 20.00000000000000000 ) ) ;
#32551 = ORIENTED_EDGE ( 'NONE', *, *, #57573, .F. ) ;
#32552 = DIRECTION ( 'NONE',  ( 0.000000000000000000, 0.000000000000000000, 1.000000000000000000 ) ) ;
#32553 = TOROIDAL_SURFACE ( 'NONE', #24666, 22.50000000000000000, 0.5000000000000000000 ) ;
#32554 = EDGE_CURVE ( 'NONE', #17689, #21587, #27530, .T. ) ;
#32555 = EDGE_LOOP ( 'NONE', ( #63977, #58234, #18506, #12120 ) ) ;
#32556 =( NAMED_UNIT ( * ) PLANE_ANGLE_UNIT ( ) SI_UNIT ( $, .RADIAN. ) );
#32557 = CARTESIAN_POINT ( 'NONE',  ( -2.607480562269075097, 116.4070736234661609, 8.025000000000000355 ) ) ;
#32560 = EDGE_CURVE ( 'NONE', #35304, #54767, #20887, .T. ) ;
#32559 = PRESENTATION_LAYER_ASSIGNMENT (  '', '', ( #40497 ) ) ;
#32558 = CARTESIAN_POINT ( 'NONE',  ( -20.51842522107655142, 114.9046575010689821, 10.00000000000000000 ) ) ;
#32561 = SURFACE_SIDE_STYLE ('',( #5465 ) ) ;
#32562 = AXIS2_PLACEMENT_3D ( 'NONE', #37903, #21662, #11097 ) ;
#32563 = ORIENTED_EDGE ( 'NONE', *, *, #45145, .F. ) ;
#32564 = EDGE_LOOP ( 'NONE', ( #35203, #27639, #58063 ) ) ;
#32565 = CARTESIAN_POINT ( 'NONE',  ( 28.00000000000000000, 0.000000000000000000, -89.00000000000000000 ) ) ;
#32566 = DIRECTION ( 'NONE',  ( 0.000000000000000000, 0.000000000000000000, 1.000000000000000000 ) ) ;
#32567 = CARTESIAN_POINT ( 'NONE',  ( -81.44292637653380496, -1.166476076187852838E-15, -9.524999999999991473 ) ) ;
#32568 = VERTEX_POINT ( 'NONE', #26812 ) ;
#32569 = CARTESIAN_POINT ( 'NONE',  ( -5.598654528085806881, 128.8549999999999898, -7.705886871421374629 ) ) ;
#32570 = DIRECTION ( 'NONE',  ( -1.000000000000000000, 0.000000000000000000, 0.000000000000000000 ) ) ;
#32571 = CARTESIAN_POINT ( 'NONE',  ( -19.89974874213239886, 114.9999999999999574, -10.49999999999999645 ) ) ;
#32572 =( GEOMETRIC_REPRESENTATION_CONTEXT ( 3 ) GLOBAL_UNCERTAINTY_ASSIGNED_CONTEXT ( ( #43990 ) ) GLOBAL_UNIT_ASSIGNED_CONTEXT ( ( #58330, #1254, #23455 ) ) REPRESENTATION_CONTEXT ( 'NONE', 'WORKASPACE' ) );
#32573 = DIRECTION ( 'NONE',  ( 0.000000000000000000, 0.000000000000000000, 1.000000000000000000 ) ) ;
#32574 = CARTESIAN_POINT ( 'NONE',  ( -90.29499999999997328, -2.607480562269069768, 8.024999999999991473 ) ) ;
#32575 = ORIENTED_EDGE ( 'NONE', *, *, #10119, .F. ) ;
#32576 =( GEOMETRIC_REPRESENTATION_CONTEXT ( 3 ) GLOBAL_UNCERTAINTY_ASSIGNED_CONTEXT ( ( #32646 ) ) GLOBAL_UNIT_ASSIGNED_CONTEXT ( ( #32367, #4604, #9910 ) ) REPRESENTATION_CONTEXT ( 'NONE', 'WORKASPACE' ) );
#32577 = CARTESIAN_POINT ( 'NONE',  ( 59.00000000000000000, 11.99999999999999822, 4.000000000000000000 ) ) ;
#32578 = FACE_OUTER_BOUND ( 'NONE', #28048, .T. ) ;
#32579 = ORIENTED_EDGE ( 'NONE', *, *, #53238, .F. ) ;
#32580 = CARTESIAN_POINT ( 'NONE',  ( -175.1929263765337623, -10.01517768586948698, 6.132527647946031529E-16 ) ) ;
#32581 =( LENGTH_UNIT ( ) NAMED_UNIT ( * ) SI_UNIT ( .MILLI., .METRE. ) );
#32582 =( GEOMETRIC_REPRESENTATION_CONTEXT ( 3 ) GLOBAL_UNCERTAINTY_ASSIGNED_CONTEXT ( ( #56512 ) ) GLOBAL_UNIT_ASSIGNED_CONTEXT ( ( #37966, #64977, #10154 ) ) REPRESENTATION_CONTEXT ( 'NONE', 'WORKASPACE' ) );
#32583 = CARTESIAN_POINT ( 'NONE',  ( -12.72792206135785698, 115.4999999999999574, -10.50000000000000000 ) ) ;
#32584 = VERTEX_POINT ( 'NONE', #10680 ) ;
#32585 = EDGE_LOOP ( 'NONE', ( #12086, #37257, #40743 ) ) ;
#32586 = SURFACE_SIDE_STYLE ('',( #15760 ) ) ;
#32587 = DIRECTION ( 'NONE',  ( 0.000000000000000000, 0.000000000000000000, -1.000000000000000000 ) ) ;
#32588 = DIRECTION ( 'NONE',  ( 1.000000000000000000, -1.189524669241239115E-16, -0.000000000000000000 ) ) ;
#32589 = DIRECTION ( 'NONE',  ( -0.9396926207859094271, -0.3420201433256660484, 0.000000000000000000 ) ) ;
#32590 = PRESENTATION_LAYER_ASSIGNMENT (  '', '', ( #34872 ) ) ;
#32591 = DIRECTION ( 'NONE',  ( -1.000000000000000000, -0.000000000000000000, -0.000000000000000000 ) ) ;
#32592 = ADVANCED_FACE ( 'NONE', ( #21932 ), #58178, .T. ) ;
#32593 = AXIS2_PLACEMENT_3D ( 'NONE', #26985, #10160, #31594 ) ;
#32594 = CARTESIAN_POINT ( 'NONE',  ( -69.29292637653378506, 3.094860106618428031, -9.524999999999993250 ) ) ;
#32595 = CARTESIAN_POINT ( 'NONE',  ( 6.826472737025121695, 116.4929263765338021, -4.959722759717905660 ) ) ;
#32596 = CARTESIAN_POINT ( 'NONE',  ( -8.487565887160236855, 153.5087057588630159, -0.9261705213943872694 ) ) ;
#32597 = EDGE_LOOP ( 'NONE', ( #66621, #56354, #31708, #21452 ) ) ;
#32598 = DIRECTION ( 'NONE',  ( 1.000000000000000000, 0.000000000000000000, 0.000000000000000000 ) ) ;
#32599 = LINE ( 'NONE', #59324, #38827 ) ;
#32600 = ORIENTED_EDGE ( 'NONE', *, *, #48169, .F. ) ;
#32601 = DIRECTION ( 'NONE',  ( -1.000000000000000000, 0.000000000000000000, 0.000000000000000000 ) ) ;
#32602 = CARTESIAN_POINT ( 'NONE',  ( -170.6050000000000182, 6.826472737025113702, -4.959722759717902107 ) ) ;
#32603 = DIRECTION ( 'NONE',  ( 0.000000000000000000, -1.000000000000000000, 0.000000000000000000 ) ) ;
#32604 = DIRECTION ( 'NONE',  ( 1.000000000000000000, 0.000000000000000000, 0.000000000000000000 ) ) ;
#32605 = PRESENTATION_LAYER_ASSIGNMENT (  '', '', ( #53905 ) ) ;
#32606 = CARTESIAN_POINT ( 'NONE',  ( -173.0949999999999989, -2.607480562269071545, -8.024999999999991473 ) ) ;
#32607 =( GEOMETRIC_REPRESENTATION_CONTEXT ( 3 ) GLOBAL_UNCERTAINTY_ASSIGNED_CONTEXT ( ( #56672 ) ) GLOBAL_UNIT_ASSIGNED_CONTEXT ( ( #53806, #20064, #4937 ) ) REPRESENTATION_CONTEXT ( 'NONE', 'WORKASPACE' ) );
#32608 = CARTESIAN_POINT ( 'NONE',  ( -164.2450000000000045, -4.716976649647093289, -6.492361379858945902 ) ) ;
#32609 = STYLED_ITEM ( 'NONE', ( #51354 ), #34512 ) ;
#32610 = ORIENTED_EDGE ( 'NONE', *, *, #66650, .F. ) ;
#32611 = PRODUCT_DEFINITION ( 'UNKNOWN', '', #36031, #18474 ) ;
#32612 = CARTESIAN_POINT ( 'NONE',  ( 0.000000000000000000, 87.30187232391182306, 0.000000000000000000 ) ) ;
#32613 = EDGE_CURVE ( 'NONE', #16463, #2411, #38898, .T. ) ;
#32614 = FACE_OUTER_BOUND ( 'NONE', #69001, .T. ) ;
#32615 = PRESENTATION_LAYER_ASSIGNMENT (  '', '', ( #4380 ) ) ;
#32616 = DIRECTION ( 'NONE',  ( 0.000000000000000000, 0.000000000000000000, 1.000000000000000000 ) ) ;
#32617 = CARTESIAN_POINT ( 'NONE',  ( -84.05499999999999261, -9.827790563157499189E-16, -8.024999999999991473 ) ) ;
#32618 = DIRECTION ( 'NONE',  ( 0.000000000000000000, 0.000000000000000000, 1.000000000000000000 ) ) ;
#32619 = AXIS2_PLACEMENT_3D ( 'NONE', #55316, #65533, #414 ) ;
#32620 = DIRECTION ( 'NONE',  ( 0.000000000000000000, -1.000000000000000000, -0.000000000000000000 ) ) ;
#32621 = EDGE_CURVE ( 'NONE', #39245, #42967, #11011, .T. ) ;
#32622 = CARTESIAN_POINT ( 'NONE',  ( -82.79499999999998749, 2.607480562269069324, -8.024999999999993250 ) ) ;
#32623 = EDGE_CURVE ( 'NONE', #50288, #2387, #8538, .T. ) ;
#32624 = CARTESIAN_POINT ( 'NONE',  ( -3.094860106618434248, 138.9049999999999727, 9.525000000000000355 ) ) ;
#32625 = CIRCLE ( 'NONE', #15848, 0.5000000000000004441 ) ;
#32626 = VECTOR ( 'NONE', #16833, 1000.000000000000000 ) ;
#32627 = CARTESIAN_POINT ( 'NONE',  ( -7.499999999999999112, 0.000000000000000000, 4.999999999999999112 ) ) ;
#32628 = UNCERTAINTY_MEASURE_WITH_UNIT (LENGTH_MEASURE( 1.000000000000000082E-05 ), #1515, 'distance_accuracy_value', 'NONE');
#32629 = MECHANICAL_DESIGN_GEOMETRIC_PRESENTATION_REPRESENTATION (  '', ( #40515 ), #26988 ) ;
#32631 = SURFACE_STYLE_USAGE ( .BOTH. , #26990 ) ;
#32630 = PRODUCT_DEFINITION_FORMATION_WITH_SPECIFIED_SOURCE ( 'ANY', '', #32768, .NOT_KNOWN. ) ;
#32632 = CARTESIAN_POINT ( 'NONE',  ( -90.44292637653379074, -1.166476076187852838E-15, -9.524999999999991473 ) ) ;
#32633 = ORIENTED_EDGE ( 'NONE', *, *, #59155, .T. ) ;
#32634 = EDGE_CURVE ( 'NONE', #66255, #21253, #37713, .T. ) ;
#32635 = STYLED_ITEM ( 'NONE', ( #34618 ), #34624 ) ;
#32636 = CARTESIAN_POINT ( 'NONE',  ( -51.29292637653378506, 3.094860106618428031, -9.524999999999993250 ) ) ;
#32637 = EDGE_CURVE ( 'NONE', #65035, #11384, #29861, .T. ) ;
#32639 =( NAMED_UNIT ( * ) PLANE_ANGLE_UNIT ( ) SI_UNIT ( $, .RADIAN. ) );
#32638 = CARTESIAN_POINT ( 'NONE',  ( 45.00000000000000000, 10.25709351175097694, -6.999999999999998224 ) ) ;
#32640 = EDGE_CURVE ( 'NONE', #9643, #13980, #17541, .T. ) ;
#32641 = CARTESIAN_POINT ( 'NONE',  ( -2.607480562269157254, 136.2070736234661581, -8.024999999999939959 ) ) ;
#32642 = ORIENTED_EDGE ( 'NONE', *, *, #62582, .T. ) ;
#32643 = VERTEX_POINT ( 'NONE', #37472 ) ;
#32644 = CARTESIAN_POINT ( 'NONE',  ( -6.826472737025120807, 135.3929263765338362, -4.959722759717907437 ) ) ;
#32645 = CIRCLE ( 'NONE', #13565, 0.2500000000000000000 ) ;
#32646 = UNCERTAINTY_MEASURE_WITH_UNIT (LENGTH_MEASURE( 1.000000000000000082E-05 ), #32367, 'distance_accuracy_value', 'NONE');
#32647 = COLOUR_RGB ( '', 0.66274510, 0.83137255, 0.94901961) ;
#32648 = AXIS2_PLACEMENT_3D ( 'NONE', #61857, #24563, #24922 ) ;
#32649 = FILL_AREA_STYLE ('',( #33691 ) ) ;
#32650 = ORIENTED_EDGE ( 'NONE', *, *, #66891, .F. ) ;
#32651 = CARTESIAN_POINT ( 'NONE',  ( -112.1049999999999756, -6.826472737025113702, 4.959722759717902107 ) ) ;
#32652 = ORIENTED_EDGE ( 'NONE', *, *, #19040, .F. ) ;
#32653 = FILL_AREA_STYLE ('',( #61121 ) ) ;
#32654 = DIRECTION ( 'NONE',  ( -0.000000000000000000, -0.000000000000000000, -1.000000000000000000 ) ) ;
#32655 = VERTEX_POINT ( 'NONE', #58873 ) ;
#32656 = SURFACE_SIDE_STYLE ('',( #33699 ) ) ;
#32657 = CARTESIAN_POINT ( 'NONE',  ( -6.239160159721276244, -2.499999999999999556, 3.193457606803197013 ) ) ;
#32658 = ORIENTED_EDGE ( 'NONE', *, *, #32546, .F. ) ;
#32659 =( GEOMETRIC_REPRESENTATION_CONTEXT ( 3 ) GLOBAL_UNCERTAINTY_ASSIGNED_CONTEXT ( ( #36451 ) ) GLOBAL_UNIT_ASSIGNED_CONTEXT ( ( #48361, #15997, #53595 ) ) REPRESENTATION_CONTEXT ( 'NONE', 'WORKASPACE' ) );
#32660 = CARTESIAN_POINT ( 'NONE',  ( 57.24999999999999289, 28.24999999999998934, 3.750000000000000000 ) ) ;
#32661 = COLOUR_RGB ( '', 0.31764706, 0.68627451, 0.89019608) ;
#32662 = CARTESIAN_POINT ( 'NONE',  ( -1.166476076187854022E-15, 155.9449999999999932, 9.525000000000000355 ) ) ;
#32663 = CYLINDRICAL_SURFACE ( 'NONE', #31761, 20.42000000000000526 ) ;
#32664 = ORIENTED_EDGE ( 'NONE', *, *, #65348, .T. ) ;
#32665 = VECTOR ( 'NONE', #19923, 1000.000000000000000 ) ;
#32666 = EDGE_LOOP ( 'NONE', ( #6001, #61834, #61921 ) ) ;
#32667 = LINE ( 'NONE', #59385, #8608 ) ;
#32668 = CARTESIAN_POINT ( 'NONE',  ( -14.33443387982028483, -10.92428437323945367, 4.966394326244869539 ) ) ;
#32669 = DIRECTION ( 'NONE',  ( 0.000000000000000000, 0.000000000000000000, 1.000000000000000000 ) ) ;
#32670 = B_SPLINE_CURVE_WITH_KNOTS ( 'NONE', 3,
 ( #50481, #12478, #49794, #33940, #23736, #66662, #54697, #12834, #17458, #27942, #38927, #55401 ),
 .UNSPECIFIED., .F., .F.,
 ( 4, 2, 2, 2, 2, 4 ),
 ( 0.000000000000000000, 0.001808836200486184593, 0.003617672400972369185, 0.004522090501215460072, 0.005426508601458550525, 0.007235344801944751381 ),
 .UNSPECIFIED. ) ;
#32671 = ORIENTED_EDGE ( 'NONE', *, *, #16237, .F. ) ;
#32672 = CARTESIAN_POINT ( 'NONE',  ( 4.716976649647096842, 133.7429263765338021, 6.492361379858953896 ) ) ;
#32673 = CARTESIAN_POINT ( 'NONE',  ( 30.75000000000001066, 16.24999999999997513, 3.750000000000000000 ) ) ;
#32674 = CARTESIAN_POINT ( 'NONE',  ( -47.50000000000000000, 14.49137674618942562, 9.500000000000000000 ) ) ;
#32675 = FILL_AREA_STYLE_COLOUR ( '', #43382 ) ;
#32676 = ORIENTED_EDGE ( 'NONE', *, *, #52474, .T. ) ;
#32677 = STYLED_ITEM ( 'NONE', ( #25928 ), #17923 ) ;
#32678 = FILL_AREA_STYLE_COLOUR ( '', #41966 ) ;
#32679 = ORIENTED_EDGE ( 'NONE', *, *, #62968, .F. ) ;
#32680 = CARTESIAN_POINT ( 'NONE',  ( -52.19292637653380496, -10.01517768586948698, 6.132527647946031529E-16 ) ) ;
#32681 = CARTESIAN_POINT ( 'NONE',  ( 0.000000000000000000, 0.000000000000000000, 12.50000000000000000 ) ) ;
#32682 = CARTESIAN_POINT ( 'NONE',  ( 44.25000000000000000, 21.74999999999998579, -4.000000000000000000 ) ) ;
#32683 = DIRECTION ( 'NONE',  ( -1.000000000000000000, 0.000000000000000000, 0.000000000000000000 ) ) ;
#32684 = CARTESIAN_POINT ( 'NONE',  ( -143.7549999999999955, 4.716976649647091513, -6.492361379858946790 ) ) ;
#32685 = CARTESIAN_POINT ( 'NONE',  ( -176.9070736234662604, -3.094860106617245421, 9.525000000000854783 ) ) ;
#32686 = SURFACE_STYLE_USAGE ( .BOTH. , #37687 ) ;
#32687 = UNCERTAINTY_MEASURE_WITH_UNIT (LENGTH_MEASURE( 1.000000000000000082E-05 ), #24936, 'distance_accuracy_value', 'NONE');
#32688 = CARTESIAN_POINT ( 'NONE',  ( -115.7949999999999875, 2.607480562269068880, -8.024999999999993250 ) ) ;
#32689 = CARTESIAN_POINT ( 'NONE',  ( -42.59457610709575448, -13.96731970680246171, 0.7787128058468592018 ) ) ;
#32690 = FILL_AREA_STYLE_COLOUR ( '', #32744 ) ;
#32691 = SURFACE_STYLE_FILL_AREA ( #43325 ) ;
#32692 = ORIENTED_EDGE ( 'NONE', *, *, #16570, .F. ) ;
#32693 =( GEOMETRIC_REPRESENTATION_CONTEXT ( 3 ) GLOBAL_UNCERTAINTY_ASSIGNED_CONTEXT ( ( #36841 ) ) GLOBAL_UNIT_ASSIGNED_CONTEXT ( ( #49351, #18023, #2111 ) ) REPRESENTATION_CONTEXT ( 'NONE', 'WORKASPACE' ) );
#32694 = ORIENTED_EDGE ( 'NONE', *, *, #66553, .F. ) ;
#32695 = CARTESIAN_POINT ( 'NONE',  ( -45.00000000000000000, 9.696054906849926880, 3.569578952172539399 ) ) ;
#32696 = CARTESIAN_POINT ( 'NONE',  ( -54.20499999999997698, -2.607480562269071545, -8.024999999999991473 ) ) ;
#32697 = ORIENTED_EDGE ( 'NONE', *, *, #69129, .T. ) ;
#32698 = SURFACE_STYLE_USAGE ( .BOTH. , #12623 ) ;
#32699 = DIRECTION ( 'NONE',  ( -1.000000000000000000, 0.000000000000000000, 0.000000000000000000 ) ) ;
#32700 = SURFACE_STYLE_FILL_AREA ( #48940 ) ;
#32701 = DIRECTION ( 'NONE',  ( -0.000000000000000000, 0.000000000000000000, -1.000000000000000000 ) ) ;
#32702 = VECTOR ( 'NONE', #41961, 1000.000000000000114 ) ;
#32703 = DIRECTION ( 'NONE',  ( 0.000000000000000000, 0.000000000000000000, -1.000000000000000000 ) ) ;
#32704 = DIRECTION ( 'NONE',  ( -1.000000000000000000, 0.000000000000000000, 0.000000000000000000 ) ) ;
#32705 = EDGE_LOOP ( 'NONE', ( #15900, #21975, #61392, #19256 ) ) ;
#32706 = CIRCLE ( 'NONE', #58524, 0.2500000000000002220 ) ;
#32707 = EDGE_CURVE ( 'NONE', #3021, #20470, #62448, .T. ) ;
#32708 = AXIS2_PLACEMENT_3D ( 'NONE', #15022, #3702, #25198 ) ;
#32709 = FILL_AREA_STYLE_COLOUR ( '', #42554 ) ;
#32710 =( NAMED_UNIT ( * ) PLANE_ANGLE_UNIT ( ) SI_UNIT ( $, .RADIAN. ) );
#32712 =( BOUNDED_SURFACE ( )  B_SPLINE_SURFACE ( 3, 2, ( 
 ( #66935, #13439, #19767 ),
 ( #13800, #35260, #56722 ),
 ( #29972, #51436, #3181 ),
 ( #24674, #46196, #14158 ),
 ( #35616, #57052, #41263 ),
 ( #59122, #27097, #52843 ),
 ( #37390, #5299, #48629 ),
 ( #31342, #21860, #4620 ),
 ( #21146, #63712, #64057 ),
 ( #42653, #57767, #26075 ),
 ( #326, #58793, #36340 ),
 ( #42328, #64763, #43372 ),
 ( #53518, #52503, #32379 ),
 ( #48269, #58115, #9593 ),
 ( #4246, #53848, #20823 ),
 ( #25724, #63377, #47246 ),
 ( #16266, #68666, #37740 ),
 ( #10610, #10943, #36698 ),
 ( #20465, #69687, #15561 ),
 ( #41969, #37034, #31010 ) ),
 .UNSPECIFIED., .F., .F., .F. ) 
 B_SPLINE_SURFACE_WITH_KNOTS ( ( 4, 2, 2, 2, 2, 2, 2, 2, 2, 4 ),
 ( 3, 3 ),
 ( 0.001620365016234687986, 0.002207270000664790163, 0.002500722492879841469, 0.002794174985094892774, 0.003087627477309944080, 0.003381079969524994951, 0.003527806215632520170, 0.003674532461740045823, 0.003821258707847571476, 0.003967984953955097129 ),
 ( 0.000000000000000000, 1.000000000000000000 ),
 .UNSPECIFIED. ) 
 GEOMETRIC_REPRESENTATION_ITEM ( )  RATIONAL_B_SPLINE_SURFACE ( (
 ( 1.000000000000000000, 0.7071067811865530128, 1.000000000000000000),
 ( 1.000000000000000000, 0.6778671762787942257, 1.000000000000000000),
 ( 1.000000000000000000, 0.6467717707946214478, 1.000000000000000000),
 ( 1.000000000000000000, 0.5961086003390576593, 1.000000000000000000),
 ( 1.000000000000000000, 0.5785481842583619638, 1.000000000000000000),
 ( 1.000000000000000000, 0.5417514570912689287, 1.000000000000000000),
 ( 1.000000000000000000, 0.5224568997727286890, 1.000000000000000000),
 ( 1.000000000000000000, 0.4825437615630544519, 1.000000000000000000),
 ( 1.000000000000000000, 0.4617081702730074788, 1.000000000000000000),
 ( 1.000000000000000000, 0.4191790061641540999, 1.000000000000000000),
 ( 1.000000000000000000, 0.3974966599963052905, 1.000000000000000000),
 ( 1.000000000000000000, 0.3653498311554732592, 1.000000000000000000),
 ( 1.000000000000000000, 0.3548631489840464726, 1.000000000000000000),
 ( 1.000000000000000000, 0.3350876751767114525, 1.000000000000000000),
 ( 1.000000000000000000, 0.3256829922529743682, 1.000000000000000000),
 ( 1.000000000000000000, 0.3094849113515740768, 1.000000000000000000),
 ( 1.000000000000000000, 0.3027429446060538876, 1.000000000000000000),
 ( 1.000000000000000000, 0.2932846354086147134, 1.000000000000000000),
 ( 1.000000000000000000, 0.2906862528186607841, 1.000000000000000000),
 ( 1.000000000000000000, 0.2907356542125085763, 1.000000000000000000) ) ) 
 REPRESENTATION_ITEM ( '' )  SURFACE ( )  );
#32711 = DIRECTION ( 'NONE',  ( -0.000000000000000000, -0.000000000000000000, -1.000000000000000000 ) ) ;
#32713 = DIRECTION ( 'NONE',  ( -1.000000000000000000, 0.000000000000000000, 0.000000000000000000 ) ) ;
#32714 = DIRECTION ( 'NONE',  ( 0.000000000000000000, 0.000000000000000000, 1.000000000000000000 ) ) ;
#32715 = MECHANICAL_DESIGN_GEOMETRIC_PRESENTATION_REPRESENTATION (  '', ( #7966 ), #17755 ) ;
#32716 = ADVANCED_FACE ( 'NONE', ( #53587 ), #5370, .F. ) ;
#32717 = CARTESIAN_POINT ( 'NONE',  ( -108.2949999999999733, -2.607480562269069768, 8.024999999999991473 ) ) ;
#32718 = CARTESIAN_POINT ( 'NONE',  ( -10.01517768586949231, 158.1949999999999932, -6.132527647946036459E-16 ) ) ;
#32719 = CARTESIAN_POINT ( 'NONE',  ( -91.04499999999998749, 7.632228543268600340, 2.479861379858949277 ) ) ;
#32720 = VECTOR ( 'NONE', #33104, 1000.000000000000000 ) ;
#32721 = CARTESIAN_POINT ( 'NONE',  ( 3.000000000000030198, 37.76051491742381216, 89.34202014332566932 ) ) ;
#32722 = DIRECTION ( 'NONE',  ( 0.000000000000000000, 0.000000000000000000, -1.000000000000000000 ) ) ;
#32723 = CARTESIAN_POINT ( 'NONE',  ( 3.000000000000002665, 42.58578643762690064, -89.58578643762690774 ) ) ;
#32724 = UNCERTAINTY_MEASURE_WITH_UNIT (LENGTH_MEASURE( 1.000000000000000082E-05 ), #37859, 'distance_accuracy_value', 'NONE');
#32725 = AXIS2_PLACEMENT_3D ( 'NONE', #17792, #33947, #2213 ) ;
#32726 = DIRECTION ( 'NONE',  ( 0.7681514953298231863, 0.000000000000000000, 0.6402681315062906942 ) ) ;
#32727 = EDGE_LOOP ( 'NONE', ( #64411, #56637, #20992, #62269, #37587 ) ) ;
#32728 = CARTESIAN_POINT ( 'NONE',  ( -120.8929263765338078, -8.102448949553172852, -5.886773742842741797 ) ) ;
#32729 =( NAMED_UNIT ( * ) SI_UNIT ( $, .STERADIAN. ) SOLID_ANGLE_UNIT ( ) );
#32730 = CARTESIAN_POINT ( 'NONE',  ( -148.0449999999999875, 7.632228543268600340, 2.479861379858949277 ) ) ;
#32732 = CARTESIAN_POINT ( 'NONE',  ( -4.041451884327381450, 7.000000000000006217, 1.082903768654761345 ) ) ;
#32731 = VECTOR ( 'NONE', #3266, 1000.000000000000000 ) ;
#32733 = EDGE_CURVE ( 'NONE', #39825, #56654, #3988, .T. ) ;
#32734 = CARTESIAN_POINT ( 'NONE',  ( -46.79499999999996618, 2.607480562269069324, -8.024999999999993250 ) ) ;
#32735 =( LENGTH_UNIT ( ) NAMED_UNIT ( * ) SI_UNIT ( .MILLI., .METRE. ) );
#32736 = VERTEX_POINT ( 'NONE', #45147 ) ;
#32737 = ORIENTED_EDGE ( 'NONE', *, *, #52618, .T. ) ;
#32738 =( BOUNDED_CURVE ( )  B_SPLINE_CURVE ( 2, ( #26092, #68330, #25743, #30669, #35978, #14174, #8883, #3562, #57782, #15244, #14879 ),
 .UNSPECIFIED., .F., .F. ) 
 B_SPLINE_CURVE_WITH_KNOTS ( ( 3, 2, 2, 2, 2, 3 ),
 ( 0.9130434782608695121, 0.9152173913043478715, 0.9173913043478261198, 0.9195652173913043681, 0.9217391304347826164, 0.9239130434782608647 ),
 .UNSPECIFIED. ) 
 CURVE ( )  GEOMETRIC_REPRESENTATION_ITEM ( )  RATIONAL_B_SPLINE_CURVE ( ( 1.000000000000000000, 0.9510565162951535312, 1.000000000000000000, 0.9510565162951535312, 1.000000000000000000, 0.9510565162951535312, 1.000000000000000000, 0.9510565162951535312, 1.000000000000000000, 0.9510565162951535312, 1.000000000000000000 ) ) 
 REPRESENTATION_ITEM ( '' )  );
#32739 = DIRECTION ( 'NONE',  ( -1.000000000000000000, -5.782411586589351722E-16, 0.000000000000000000 ) ) ;
#32740 = DIRECTION ( 'NONE',  ( 0.000000000000000000, 0.000000000000000000, 1.000000000000000000 ) ) ;
#32741 = CIRCLE ( 'NONE', #11399, 13.99999999999999822 ) ;
#32742 = DIRECTION ( 'NONE',  ( 0.000000000000000000, 0.000000000000000000, 1.000000000000000000 ) ) ;
#32743 = DIRECTION ( 'NONE',  ( -1.000000000000000000, 0.000000000000000000, -0.000000000000000000 ) ) ;
#32744 = COLOUR_RGB ( '', 0.72549020, 0.75294118, 0.79215686) ;
#32745 = CARTESIAN_POINT ( 'NONE',  ( -50.90707362346616804, -3.094860106618429807, 9.524999999999991473 ) ) ;
#32746 = SURFACE_STYLE_USAGE ( .BOTH. , #17787 ) ;
#32747 = VERTEX_POINT ( 'NONE', #12381 ) ;
#32748 = CARTESIAN_POINT ( 'NONE',  ( -137.3049999999999784, 8.437984349512086979, -1.550032578732815448E-15 ) ) ;
#32749 = EDGE_LOOP ( 'NONE', ( #4624, #65922, #1280, #24777 ) ) ;
#32750 = EDGE_CURVE ( 'NONE', #60504, #64131, #6423, .T. ) ;
#32751 = ORIENTED_EDGE ( 'NONE', *, *, #55673, .T. ) ;
#32752 = LINE ( 'NONE', #34139, #43674 ) ;
#32753 = DIRECTION ( 'NONE',  ( -0.000000000000000000, 0.000000000000000000, -1.000000000000000000 ) ) ;
#32754 = ORIENTED_EDGE ( 'NONE', *, *, #57522, .T. ) ;
#32755 = DIRECTION ( 'NONE',  ( 0.000000000000000000, 0.000000000000000000, -1.000000000000000000 ) ) ;
#32756 = EDGE_CURVE ( 'NONE', #15520, #58139, #42285, .T. ) ;
#32757 = DIRECTION ( 'NONE',  ( 1.000000000000000000, 0.000000000000000000, 0.000000000000000000 ) ) ;
#32758 = CARTESIAN_POINT ( 'NONE',  ( -5.598654528085806881, 127.7450000000000045, -7.705886871421374629 ) ) ;
#32759 = CARTESIAN_POINT ( 'NONE',  ( 0.4644249260832968851, 42.85561104658234655, -74.47757702770792321 ) ) ;
#32760 = ORIENTED_EDGE ( 'NONE', *, *, #7469, .T. ) ;
#32761 =( GEOMETRIC_REPRESENTATION_CONTEXT ( 3 ) GLOBAL_UNCERTAINTY_ASSIGNED_CONTEXT ( ( #38914 ) ) GLOBAL_UNIT_ASSIGNED_CONTEXT ( ( #19441, #40231, #13826 ) ) REPRESENTATION_CONTEXT ( 'NONE', 'WORKASPACE' ) );
#32762 = DIRECTION ( 'NONE',  ( 0.000000000000000000, -0.000000000000000000, -1.000000000000000000 ) ) ;
#32763 = CARTESIAN_POINT ( 'NONE',  ( 9.058813317711338797, 130.9549999999999841, -2.943386871421372675 ) ) ;
#32764 = CIRCLE ( 'NONE', #58620, 3.000000000000000444 ) ;
#32765 = CARTESIAN_POINT ( 'NONE',  ( -52.85499999999998266, 4.716976649647094177, 6.492361379858945902 ) ) ;
#32766 = CARTESIAN_POINT ( 'NONE',  ( -118.1949999999999790, 8.437984349512085203, -1.550032578732815448E-15 ) ) ;
#32767 = CARTESIAN_POINT ( 'NONE',  ( -41.08036663239577990, 107.6296822352908151, -3.281244196345766806 ) ) ;
#32768 = PRODUCT ( '5. Handle', '5. Handle', '', ( #60660 ) ) ;
#32769 = ORIENTED_EDGE ( 'NONE', *, *, #5650, .T. ) ;
#32770 = CARTESIAN_POINT ( 'NONE',  ( 5.598654528085809545, 143.2549999999999955, -7.705886871421373741 ) ) ;
#32771 = LINE ( 'NONE', #34499, #22117 ) ;
#32772 = UNCERTAINTY_MEASURE_WITH_UNIT (LENGTH_MEASURE( 1.000000000000000082E-05 ), #62827, 'distance_accuracy_value', 'NONE');
#32773 = CYLINDRICAL_SURFACE ( 'NONE', #19839, 12.50000000000001066 ) ;
#32774 = CIRCLE ( 'NONE', #29388, 0.2500000000000002220 ) ;
#32775 = FACE_OUTER_BOUND ( 'NONE', #19516, .T. ) ;
#32776 = DIRECTION ( 'NONE',  ( 0.7833176619561906806, -0.6216216216216158275, 0.000000000000000000 ) ) ;
#32777 = CIRCLE ( 'NONE', #54098, 0.2500000000000002220 ) ;
#32778 =( NAMED_UNIT ( * ) PLANE_ANGLE_UNIT ( ) SI_UNIT ( $, .RADIAN. ) );
#32779 = ORIENTED_EDGE ( 'NONE', *, *, #10095, .T. ) ;
#32780 = CARTESIAN_POINT ( 'NONE',  ( -33.39016983555134033, -9.443832887535089426, -2.000000000000000000 ) ) ;
#32781 =( NAMED_UNIT ( * ) SI_UNIT ( $, .STERADIAN. ) SOLID_ANGLE_UNIT ( ) );
#32782 = CARTESIAN_POINT ( 'NONE',  ( -175.7049999999999557, 2.607480562269073321, 8.024999999999991473 ) ) ;
#32784 = ORIENTED_EDGE ( 'NONE', *, *, #19378, .F. ) ;
#32783 = MECHANICAL_DESIGN_GEOMETRIC_PRESENTATION_REPRESENTATION (  '', ( #4703 ), #56363 ) ;
#32785 = CARTESIAN_POINT ( 'NONE',  ( 54.99999999999999289, 1.797044900979284448E-15, 6.999999999999988454 ) ) ;
#32786 = UNCERTAINTY_MEASURE_WITH_UNIT (LENGTH_MEASURE( 1.000000000000000082E-05 ), #39919, 'distance_accuracy_value', 'NONE');
#32787 = STYLED_ITEM ( 'NONE', ( #53116 ), #54527 ) ;
#32788 =( NAMED_UNIT ( * ) SI_UNIT ( $, .STERADIAN. ) SOLID_ANGLE_UNIT ( ) );
#32789 = CARTESIAN_POINT ( 'NONE',  ( -184.0000000000000000, -8.446573402700972011, 1.153699593821606140 ) ) ;
#32790 = DIRECTION ( 'NONE',  ( 0.000000000000000000, 0.000000000000000000, -1.000000000000000000 ) ) ;
#32791 = CARTESIAN_POINT ( 'NONE',  ( 10.00000000000001954, 42.00000000000000000, -29.68999999999999417 ) ) ;
#32792 = TOROIDAL_SURFACE ( 'NONE', #61828, 0.7500000000000000000, 0.2500000000000000000 ) ;
#32793 = ORIENTED_EDGE ( 'NONE', *, *, #28901, .F. ) ;
#32794 = CARTESIAN_POINT ( 'NONE',  ( -71.99999999999998579, 119.9999999999997868, -7.000000000000000000 ) ) ;
#32795 = CARTESIAN_POINT ( 'NONE',  ( -85.25499999999998124, -4.716976649647092401, 6.492361379858946790 ) ) ;
#32796 = VERTEX_POINT ( 'NONE', #17370 ) ;
#32797 = CARTESIAN_POINT ( 'NONE',  ( 60.00000000000000000, 1.797044900979284448E-15, -9.500000000000000000 ) ) ;
#32798 =( GEOMETRIC_REPRESENTATION_CONTEXT ( 3 ) GLOBAL_UNCERTAINTY_ASSIGNED_CONTEXT ( ( #61607 ) ) GLOBAL_UNIT_ASSIGNED_CONTEXT ( ( #37077, #59159, #32103 ) ) REPRESENTATION_CONTEXT ( 'NONE', 'WORKASPACE' ) );
#32799 = ADVANCED_FACE ( 'NONE', ( #29256 ), #1792, .F. ) ;
#32800 = CYLINDRICAL_SURFACE ( 'NONE', #22437, 8.000000000000014211 ) ;
#32801 = CARTESIAN_POINT ( 'NONE',  ( -48.50000000000000000, 14.49137674618942562, 9.500000000000000000 ) ) ;
#32802 = FILL_AREA_STYLE_COLOUR ( '', #30825 ) ;
#32803 = CARTESIAN_POINT ( 'NONE',  ( -69.65707362346616094, 9.058813317711329915, 2.943386871421369566 ) ) ;
#32804 = AXIS2_PLACEMENT_3D ( 'NONE', #62188, #45715, #41826 ) ;
#32805 = LINE ( 'NONE', #59170, #60562 ) ;
#32806 = EDGE_LOOP ( 'NONE', ( #11912, #39031, #16657, #31265 ) ) ;
#32807 = DIRECTION ( 'NONE',  ( -0.000000000000000000, -0.000000000000000000, -1.000000000000000000 ) ) ;
#32808 = AXIS2_PLACEMENT_3D ( 'NONE', #20935, #47354, #26185 ) ;
#32810 = LINE ( 'NONE', #53245, #69545 ) ;
#32809 = DIRECTION ( 'NONE',  ( 0.000000000000000000, 0.000000000000000000, 1.000000000000000000 ) ) ;
#32811 = CARTESIAN_POINT ( 'NONE',  ( -105.8050000000000068, -8.437984349512085203, 5.166775262442717831E-16 ) ) ;
#32812 = EDGE_CURVE ( 'NONE', #25904, #29039, #27851, .T. ) ;
#32813 = CARTESIAN_POINT ( 'NONE',  ( 0.000000000000000000, 127.4449999999999790, -9.525000000000000355 ) ) ;
#32814 = CARTESIAN_POINT ( 'NONE',  ( -118.4949999999999903, 6.826472737025113702, -4.959722759717902107 ) ) ;
#32815 = CIRCLE ( 'NONE', #8110, 0.5000000000000004441 ) ;
#32816 = ADVANCED_FACE ( 'NONE', ( #12044 ), #6766, .F. ) ;
#32818 = PLANE ( 'NONE',  #23550 ) ;
#32817 = DIRECTION ( 'NONE',  ( 0.000000000000000000, 0.000000000000000000, -1.000000000000000000 ) ) ;
#32819 = PRESENTATION_LAYER_ASSIGNMENT (  '', '', ( #54140 ) ) ;
#32820 = AXIS2_PLACEMENT_3D ( 'NONE', #59809, #43678, #33421 ) ;
#32821 = CARTESIAN_POINT ( 'NONE',  ( -151.9429263765338192, 0.000000000000000000, 9.524999999999991473 ) ) ;
#32822 = CARTESIAN_POINT ( 'NONE',  ( -172.7950000000000159, 2.607480562269068880, -8.024999999999993250 ) ) ;
#32823 = EDGE_CURVE ( 'NONE', #53539, #45684, #66565, .T. ) ;
#32824 = PRESENTATION_LAYER_ASSIGNMENT (  '', '', ( #56418 ) ) ;
#32825 = CARTESIAN_POINT ( 'NONE',  ( -41.40296580814450778, -13.81618002571821613, 2.682162060699885497 ) ) ;
#32826 = ORIENTED_EDGE ( 'NONE', *, *, #50271, .F. ) ;
#32827 = SURFACE_STYLE_FILL_AREA ( #6089 ) ;
#32828 = DIRECTION ( 'NONE',  ( 1.000000000000000000, -1.445602896647339656E-16, 0.000000000000000000 ) ) ;
#32829 = ORIENTED_EDGE ( 'NONE', *, *, #34384, .F. ) ;
#32830 = CARTESIAN_POINT ( 'NONE',  ( -77.69292637653380496, 10.01517768586948698, -1.839758294383808571E-15 ) ) ;
#32831 = CONTEXT_DEPENDENT_SHAPE_REPRESENTATION ( #33013, #44745 ) ;
#32832 = DIRECTION ( 'NONE',  ( -0.6216216216216191581, -0.7833176619561879050, 0.000000000000000000 ) ) ;
#32833 = CARTESIAN_POINT ( 'NONE',  ( 60.00000000000000000, -2.024042244987997205E-14, 7.500000000000000000 ) ) ;
#32834 = MECHANICAL_DESIGN_GEOMETRIC_PRESENTATION_REPRESENTATION (  '', ( #16047 ), #163 ) ;
#32835 = DIRECTION ( 'NONE',  ( 1.000000000000000000, 0.000000000000000000, 0.000000000000000000 ) ) ;
#32836 = DIRECTION ( 'NONE',  ( 1.000000000000000000, -0.000000000000000000, 0.000000000000000000 ) ) ;
#32837 = DIRECTION ( 'NONE',  ( -0.000000000000000000, 1.000000000000000000, 0.000000000000000000 ) ) ;
#32838 = ORIENTED_EDGE ( 'NONE', *, *, #58785, .T. ) ;
#32839 = CARTESIAN_POINT ( 'NONE',  ( -165.6550000000000011, -7.632228543268600340, -2.479861379858950166 ) ) ;
#32840 = PRESENTATION_LAYER_ASSIGNMENT (  '', '', ( #47502 ) ) ;
#32841 = ORIENTED_EDGE ( 'NONE', *, *, #66319, .F. ) ;
#32842 = DIRECTION ( 'NONE',  ( 1.000000000000000000, 0.000000000000000000, 0.000000000000000000 ) ) ;
#32843 = CYLINDRICAL_SURFACE ( 'NONE', #67948, 9.524999999999991473 ) ;
#32844 = DIRECTION ( 'NONE',  ( 1.000000000000000000, 0.000000000000000000, 0.000000000000000000 ) ) ;
#32845 = SURFACE_STYLE_FILL_AREA ( #10698 ) ;
#32846 = CARTESIAN_POINT ( 'NONE',  ( -182.1570736234661751, -9.058813317711329915, -2.943386871421370898 ) ) ;
#32847 = CARTESIAN_POINT ( 'NONE',  ( -6.826472737025120807, 154.5070736234661410, -4.959722759717907437 ) ) ;
#32848 =( BOUNDED_CURVE ( )  B_SPLINE_CURVE ( 2, ( #8711, #34725, #56537, #19238, #24512, #29812, #18579, #40745, #46028, #2315, #67441 ),
 .UNSPECIFIED., .F., .F. ) 
 B_SPLINE_CURVE_WITH_KNOTS ( ( 3, 2, 2, 2, 2, 3 ),
 ( 0.2826086956521672300, 0.2847826086956454783, 0.2869565217391236711, 0.2891304347826018084, 0.2913043478260800012, 0.2934782608695582495 ),
 .UNSPECIFIED. ) 
 CURVE ( )  GEOMETRIC_REPRESENTATION_ITEM ( )  RATIONAL_B_SPLINE_CURVE ( ( 1.000000000000149880, 0.9510565162950035401, 1.000000000000000000, 0.9510565162951535312, 1.000000000000000000, 0.9510565162951535312, 1.000000000000000000, 0.9510565162951535312, 1.000000000000000000, 0.9510565162953109608, 0.9999999999998425704 ) ) 
 REPRESENTATION_ITEM ( '' )  );
#32849 = CONICAL_SURFACE ( 'NONE', #2403, 9.000000000000000000, 0.7853981633974500554 ) ;
#32850 = VERTEX_POINT ( 'NONE', #55305 ) ;
#32851 = CARTESIAN_POINT ( 'NONE',  ( 74.89452121010485541, 0.000000000000000000, 66.39042820928573008 ) ) ;
#32852 = CARTESIAN_POINT ( 'NONE',  ( -96.35499999999997556, -4.716976649647093289, -6.492361379858945902 ) ) ;
#32853 = UNCERTAINTY_MEASURE_WITH_UNIT (LENGTH_MEASURE( 1.000000000000000082E-05 ), #15428, 'distance_accuracy_value', 'NONE');
#32854 = AXIS2_PLACEMENT_3D ( 'NONE', #3951, #30328, #20857 ) ;
#32855 = DIRECTION ( 'NONE',  ( 0.000000000000000000, 0.000000000000000000, -1.000000000000000000 ) ) ;
#32856 = ORIENTED_EDGE ( 'NONE', *, *, #20413, .F. ) ;
#32857 =( NAMED_UNIT ( * ) PLANE_ANGLE_UNIT ( ) SI_UNIT ( $, .RADIAN. ) );
#32858 = CARTESIAN_POINT ( 'NONE',  ( -57.74999999999999289, 0.000000000000000000, -7.000000000000000000 ) ) ;
#32859 = FILL_AREA_STYLE ('',( #43117 ) ) ;
#32860 = CARTESIAN_POINT ( 'NONE',  ( -15.98999599679679839, 118.4999999999999716, 7.500000000000000000 ) ) ;
#32861 = ORIENTED_EDGE ( 'NONE', *, *, #34384, .T. ) ;
#32862 = CIRCLE ( 'NONE', #35275, 0.5000000000000004441 ) ;
#32863 = COLOUR_RGB ( '', 0.31764706, 0.68627451, 0.89019608) ;
#32864 = PLANE ( 'NONE',  #34015 ) ;
#32865 = CARTESIAN_POINT ( 'NONE',  ( -64.79500000000000171, 2.607480562269068880, -8.024999999999993250 ) ) ;
#32866 = VERTEX_POINT ( 'NONE', #55661 ) ;
#32867 = LINE ( 'NONE', #65209, #20507 ) ;
#32868 = CIRCLE ( 'NONE', #27205, 8.000000000000007105 ) ;
#32869 = CARTESIAN_POINT ( 'NONE',  ( 15.98999599679679839, 146.4999999999999716, 7.500000000000000000 ) ) ;
#32870 = CARTESIAN_POINT ( 'NONE',  ( -45.00000000000000711, 8.681424763011792223, -5.653729937179757137 ) ) ;
#32871 = EDGE_LOOP ( 'NONE', ( #63934, #7056, #62364, #54269 ) ) ;
#32872 =( NAMED_UNIT ( * ) PLANE_ANGLE_UNIT ( ) SI_UNIT ( $, .RADIAN. ) );
#32873 = FILL_AREA_STYLE ('',( #65215 ) ) ;
#32874 = ORIENTED_EDGE ( 'NONE', *, *, #58964, .F. ) ;
#32875 = AXIS2_PLACEMENT_3D ( 'NONE', #59928, #33549, #33213 ) ;
#32876 = CARTESIAN_POINT ( 'NONE',  ( -18.00000000000000711, 33.99999999999999289, 3.750000000000000000 ) ) ;
#32877 = FACE_OUTER_BOUND ( 'NONE', #58500, .T. ) ;
#32879 = CLOSED_SHELL ( 'NONE', ( #16257, #38317, #21206, #35995, #38965, #9053, #32449, #40978, #58154, #10459, #43432, #28574, #15221, #60574, #48411, #4656, #68327, #1675, #8192, #66485, #59832, #25569, #24445, #18272, #13893, #24770 ) ) ;
#32878 = CARTESIAN_POINT ( 'NONE',  ( -114.3549999999999898, -4.716976649647093289, -6.492361379858945902 ) ) ;
#32880 = VERTEX_POINT ( 'NONE', #1439 ) ;
#32882 = CIRCLE ( 'NONE', #59836, 0.2500000000000002220 ) ;
#32881 = SURFACE_STYLE_FILL_AREA ( #59942 ) ;
#32883 = CARTESIAN_POINT ( 'NONE',  ( -73.79292637653378506, -3.094860106618429807, 9.524999999999991473 ) ) ;
#32884 = EDGE_CURVE ( 'NONE', #50288, #51977, #44802, .T. ) ;
#32885 = CARTESIAN_POINT ( 'NONE',  ( -160.9429263765338192, 0.000000000000000000, 9.524999999999991473 ) ) ;
#32886 = SURFACE_STYLE_FILL_AREA ( #11413 ) ;
#32887 = CARTESIAN_POINT ( 'NONE',  ( -153.3570736234661922, 5.598654528085804216, 7.705886871421366635 ) ) ;
#32888 = PRODUCT_DEFINITION_SHAPE ( 'NONE', 'NONE',  #69705 ) ;
#32889 = PRESENTATION_LAYER_ASSIGNMENT (  '', '', ( #53134 ) ) ;
#32890 = CARTESIAN_POINT ( 'NONE',  ( -9.058813317711337021, 137.0449999999999875, -2.943386871421374895 ) ) ;
#32891 = EDGE_CURVE ( 'NONE', #52874, #57448, #22969, .T. ) ;
#32892 = CARTESIAN_POINT ( 'NONE',  ( -98.30707362346616662, -10.01517768586948698, 6.132527647946031529E-16 ) ) ;
#32893 = STYLED_ITEM ( 'NONE', ( #2074 ), #55054 ) ;
#32894 = DIRECTION ( 'NONE',  ( 1.000000000000000000, 0.000000000000000000, 0.000000000000000000 ) ) ;
#32895 = ORIENTED_EDGE ( 'NONE', *, *, #44732, .T. ) ;
#32896 = FACE_OUTER_BOUND ( 'NONE', #62796, .T. ) ;
#32898 = FACE_BOUND ( 'NONE', #37604, .T. ) ;
#32897 = DIRECTION ( 'NONE',  ( 0.000000000000000000, 0.000000000000000000, 1.000000000000000000 ) ) ;
#32899 = DIRECTION ( 'NONE',  ( -0.000000000000000000, -1.000000000000000000, 0.000000000000000000 ) ) ;
#32900 = VECTOR ( 'NONE', #40434, 1000.000000000000114 ) ;
#32901 = CARTESIAN_POINT ( 'NONE',  ( -129.6550000000000011, -7.632228543268600340, -2.479861379858950166 ) ) ;
#32902 = EDGE_CURVE ( 'NONE', #58801, #28436, #18631, .T. ) ;
#32903 = DIRECTION ( 'NONE',  ( -1.000000000000000000, 0.000000000000000000, 0.000000000000000000 ) ) ;
#32904 = DIRECTION ( 'NONE',  ( 8.659560562354906974E-17, -0.7071067811865496822, 0.7071067811865453523 ) ) ;
#32905 = VECTOR ( 'NONE', #41747, 1000.000000000000000 ) ;
#32906 = CARTESIAN_POINT ( 'NONE',  ( 7.000000000000017764, 42.25685517452260598, -28.66913060635885913 ) ) ;
#32907 = CARTESIAN_POINT ( 'NONE',  ( -141.4449999999999932, 0.000000000000000000, 8.024999999999991473 ) ) ;
#32908 = ADVANCED_FACE ( 'NONE', ( #65872 ), #39170, .T. ) ;
#32909 = CARTESIAN_POINT ( 'NONE',  ( -126.5949999999999847, 2.607480562269072433, 8.024999999999991473 ) ) ;
#32910 = EDGE_CURVE ( 'NONE', #63831, #38837, #66933, .T. ) ;
#32911 = EDGE_LOOP ( 'NONE', ( #20031, #59310, #64261, #68924 ) ) ;
#32912 = CARTESIAN_POINT ( 'NONE',  ( 45.43546989188915575, 10.14515663062970319, -3.347022959407288223 ) ) ;
#32913 =( GEOMETRIC_REPRESENTATION_CONTEXT ( 3 ) GLOBAL_UNCERTAINTY_ASSIGNED_CONTEXT ( ( #17398 ) ) GLOBAL_UNIT_ASSIGNED_CONTEXT ( ( #61940, #51405, #8508 ) ) REPRESENTATION_CONTEXT ( 'NONE', 'WORKASPACE' ) );
#32914 = EDGE_CURVE ( 'NONE', #454, #39136, #56342, .T. ) ;
#32915 = CARTESIAN_POINT ( 'NONE',  ( -53.90499999999997272, 2.607480562269068880, -8.024999999999993250 ) ) ;
#32916 = FILL_AREA_STYLE ('',( #37186 ) ) ;
#32917 = AXIS2_PLACEMENT_3D ( 'NONE', #35569, #57009, #30247 ) ;
#32918 = CARTESIAN_POINT ( 'NONE',  ( -61.94499999999998607, -9.827790563157499189E-16, -8.024999999999991473 ) ) ;
#32919 = DIRECTION ( 'NONE',  ( -1.000000000000000000, 0.000000000000000000, 0.000000000000000000 ) ) ;
#32920 = DIRECTION ( 'NONE',  ( 0.000000000000000000, -1.000000000000000000, 0.000000000000000000 ) ) ;
#32921 = STYLED_ITEM ( 'NONE', ( #47824 ), #47693 ) ;
#32922 = SURFACE_STYLE_FILL_AREA ( #59627 ) ;
#32923 = CARTESIAN_POINT ( 'NONE',  ( -101.8429263765338106, 9.058813317711329915, -2.943386871421373119 ) ) ;
#32924 = CARTESIAN_POINT ( 'NONE',  ( 32.00000000000002842, 115.6078173946807226, 14.99999999999997868 ) ) ;
#32925 = CARTESIAN_POINT ( 'NONE',  ( -163.5570736234661524, -1.166476076187852838E-15, -9.524999999999991473 ) ) ;
#32926 =( NAMED_UNIT ( * ) SI_UNIT ( $, .STERADIAN. ) SOLID_ANGLE_UNIT ( ) );
#32927 = CARTESIAN_POINT ( 'NONE',  ( 30.50000000000001066, 15.74999999999997513, -3.750000000000000000 ) ) ;
#32928 = VERTEX_POINT ( 'NONE', #30281 ) ;
#32929 = DIRECTION ( 'NONE',  ( -1.000000000000000000, 0.000000000000000000, 0.000000000000000000 ) ) ;
#32930 = DIRECTION ( 'NONE',  ( 0.000000000000000000, 0.000000000000000000, -1.000000000000000000 ) ) ;
#32931 = ORIENTED_EDGE ( 'NONE', *, *, #22009, .F. ) ;
#32932 = DIRECTION ( 'NONE',  ( 0.000000000000000000, 0.000000000000000000, 1.000000000000000000 ) ) ;
#32933 = AXIS2_PLACEMENT_3D ( 'NONE', #4200, #35904, #42282 ) ;
#32934 = CARTESIAN_POINT ( 'NONE',  ( 7.632228543268607446, 114.1570736234661609, 2.479861379858954606 ) ) ;
#32935 = AXIS2_PLACEMENT_3D ( 'NONE', #64356, #26695, #48569 ) ;
#32936 = LINE ( 'NONE', #49813, #13630 ) ;
#32938 = CARTESIAN_POINT ( 'NONE',  ( 74.63815776008156888, 19.81286551027084997, -6.251809480268889274 ) ) ;
#32937 = CIRCLE ( 'NONE', #53182, 1.000000000000000888 ) ;
#32939 = DIRECTION ( 'NONE',  ( -0.000000000000000000, -0.000000000000000000, 1.000000000000000000 ) ) ;
#32940 = ORIENTED_EDGE ( 'NONE', *, *, #12347, .F. ) ;
#32941 = VERTEX_POINT ( 'NONE', #2844 ) ;
#32942 = VECTOR ( 'NONE', #31364, 1000.000000000000000 ) ;
#32943 = CARTESIAN_POINT ( 'NONE',  ( -5.185928986913076244, -2.291132984336064382, -5.017707510222360057 ) ) ;
#32944 = SURFACE_STYLE_USAGE ( .BOTH. , #11472 ) ;
#32945 = ORIENTED_EDGE ( 'NONE', *, *, #59710, .F. ) ;
#32946 = DIRECTION ( 'NONE',  ( -0.000000000000000000, -0.000000000000000000, 1.000000000000000000 ) ) ;
#32947 = CARTESIAN_POINT ( 'NONE',  ( -118.8570736234661780, -5.598654528085803328, -7.705886871421366635 ) ) ;
#32948 = CARTESIAN_POINT ( 'NONE',  ( -9.827790563157511022E-16, 148.4429263765338476, 8.025000000000000355 ) ) ;
#32949 = CARTESIAN_POINT ( 'NONE',  ( -88.04499999999998749, 7.632228543268600340, 2.479861379858949277 ) ) ;
#32950 = ORIENTED_EDGE ( 'NONE', *, *, #21464, .T. ) ;
#32951 = PRESENTATION_LAYER_ASSIGNMENT (  '', '', ( #25062 ) ) ;
#32952 = CARTESIAN_POINT ( 'NONE',  ( 6.856148508274209519, 153.8597198435754478, -5.665282084007170482 ) ) ;
#32953 = CARTESIAN_POINT ( 'NONE',  ( 4.250000000000001776, 21.99999999999998579, 3.750000000000000000 ) ) ;
#32954 = FACE_OUTER_BOUND ( 'NONE', #11470, .T. ) ;
#32955 = EDGE_LOOP ( 'NONE', ( #20561, #40215, #32671, #39324 ) ) ;
#32956 = CARTESIAN_POINT ( 'NONE',  ( 61.74999999999998579, 30.99999999999999289, -4.000000000000000000 ) ) ;
#32957 = FILL_AREA_STYLE ('',( #65649 ) ) ;
#32958 = DIRECTION ( 'NONE',  ( 1.000000000000000000, -0.000000000000000000, -0.000000000000000000 ) ) ;
#32959 = ADVANCED_FACE ( 'NONE', ( #8177 ), #4237, .T. ) ;
#32960 = ORIENTED_EDGE ( 'NONE', *, *, #37502, .T. ) ;
#32961 = DIRECTION ( 'NONE',  ( 0.000000000000000000, -1.000000000000000000, 0.000000000000000000 ) ) ;
#32963 = ORIENTED_EDGE ( 'NONE', *, *, #31927, .T. ) ;
#32962 = ADVANCED_FACE ( 'NONE', ( #14475 ), #35250, .T. ) ;
#32964 = LINE ( 'NONE', #22396, #43982 ) ;
#32965 = CARTESIAN_POINT ( 'NONE',  ( -16.75000000000000000, -0.9999999999999995559, 24.00000000000000000 ) ) ;
#32966 = FACE_BOUND ( 'NONE', #45108, .T. ) ;
#32967 = CARTESIAN_POINT ( 'NONE',  ( -30.38025804287906695, -8.500000000000000000, 7.999999999999979572 ) ) ;
#32968 = AXIS2_PLACEMENT_3D ( 'NONE', #36276, #46491, #4188 ) ;
#32969 = LINE ( 'NONE', #63913, #33103 ) ;
#32970 = CARTESIAN_POINT ( 'NONE',  ( -74.99999999999998579, 50.00000000000000000, 12.00000000000000000 ) ) ;
#32971 = EDGE_CURVE ( 'NONE', #11604, #5288, #12326, .T. ) ;
#32972 = CARTESIAN_POINT ( 'NONE',  ( -68.84292637653379643, 9.058813317711329915, -2.943386871421373119 ) ) ;
#32973 = CARTESIAN_POINT ( 'NONE',  ( -8.325601791849269517, 153.4724253098392239, -1.721597945495230153 ) ) ;
#32974 = VERTEX_POINT ( 'NONE', #30642 ) ;
#32975 = DIRECTION ( 'NONE',  ( -0.000000000000000000, -0.000000000000000000, 1.000000000000000000 ) ) ;
#32976 = FACE_OUTER_BOUND ( 'NONE', #41349, .T. ) ;
#32977 = ORIENTED_EDGE ( 'NONE', *, *, #42331, .F. ) ;
#32978 = SURFACE_STYLE_USAGE ( .BOTH. , #64966 ) ;
#32979 = AXIS2_PLACEMENT_3D ( 'NONE', #9313, #62416, #3271 ) ;
#32980 = CARTESIAN_POINT ( 'NONE',  ( -162.3549999999999898, -4.716976649647093289, -6.492361379858945902 ) ) ;
#32981 = CARTESIAN_POINT ( 'NONE',  ( 0.000000000000000000, 111.9999999999999858, 0.000000000000000000 ) ) ;
#32982 = CARTESIAN_POINT ( 'NONE',  ( -148.1070736234661354, 8.102448949553172852, -5.886773742842744461 ) ) ;
#32983 = CARTESIAN_POINT ( 'NONE',  ( -176.0949999999999704, -2.607480562269071545, -8.024999999999991473 ) ) ;
#32984 = EDGE_CURVE ( 'NONE', #66646, #17220, #34836, .T. ) ;
#32985 = CARTESIAN_POINT ( 'NONE',  ( -169.1949999999999932, 8.437984349512086979, -1.550032578732815448E-15 ) ) ;
#32986 = VERTEX_POINT ( 'NONE', #51427 ) ;
#32987 = CARTESIAN_POINT ( 'NONE',  ( 44.47787316461987928, 9.825957721539955614, 3.000913084730184366 ) ) ;
#32988 = EDGE_CURVE ( 'NONE', #20378, #11058, #25381, .T. ) ;
#32989 = CARTESIAN_POINT ( 'NONE',  ( -6.826472737025120807, 150.3929263765338078, -4.959722759717907437 ) ) ;
#32990 =( GEOMETRIC_REPRESENTATION_CONTEXT ( 3 ) GLOBAL_UNCERTAINTY_ASSIGNED_CONTEXT ( ( #15251 ) ) GLOBAL_UNIT_ASSIGNED_CONTEXT ( ( #14851, #4967, #31697 ) ) REPRESENTATION_CONTEXT ( 'NONE', 'WORKASPACE' ) );
#32992 = CARTESIAN_POINT ( 'NONE',  ( -87.65499999999998693, -7.632228543268600340, -2.479861379858950166 ) ) ;
#32991 = B_SPLINE_CURVE_WITH_KNOTS ( 'NONE', 1,
 ( #48320, #378 ),
 .UNSPECIFIED., .F., .F.,
 ( 2, 2 ),
 ( 0.000000000000000000, 1.000000000000000000 ),
 .UNSPECIFIED. ) ;
#32993 = CARTESIAN_POINT ( 'NONE',  ( 24.58198306468035099, 25.31001116168506471, 27.43556691332571873 ) ) ;
#32994 = CARTESIAN_POINT ( 'NONE',  ( -80.54499999999998749, -7.632228543268600340, -2.479861379858950166 ) ) ;
#32995 = CARTESIAN_POINT ( 'NONE',  ( 3.094860106618431583, 133.2049999999999841, 9.525000000000000355 ) ) ;
#32996 = SURFACE_STYLE_FILL_AREA ( #48517 ) ;
#32997 = CIRCLE ( 'NONE', #45444, 0.2500000000000002220 ) ;
#32998 = CARTESIAN_POINT ( 'NONE',  ( 7.647808743684392674, 154.4999999999999432, 5.677732506910178500 ) ) ;
#32999 = VECTOR ( 'NONE', #9107, 1000.000000000000000 ) ;
#33000 = SURFACE_STYLE_FILL_AREA ( #16155 ) ;
#33001 = ORIENTED_EDGE ( 'NONE', *, *, #31868, .T. ) ;
#33002 = CARTESIAN_POINT ( 'NONE',  ( 6.938426666069061000, -2.291132984336068823, -1.982292489777642164 ) ) ;
#33003 = CARTESIAN_POINT ( 'NONE',  ( -50.54292637653379217, 9.058813317711329915, 2.943386871421369566 ) ) ;
#33004 = AXIS2_PLACEMENT_3D ( 'NONE', #43906, #6543, #7274 ) ;
#33005 =( NAMED_UNIT ( * ) SI_UNIT ( $, .STERADIAN. ) SOLID_ANGLE_UNIT ( ) );
#33006 = DIRECTION ( 'NONE',  ( 0.000000000000000000, 1.000000000000000000, 0.000000000000000000 ) ) ;
#33007 = CARTESIAN_POINT ( 'NONE',  ( 0.000000000000000000, 131.9429263765338192, -8.025000000000000355 ) ) ;
#33008 = ORIENTED_EDGE ( 'NONE', *, *, #11042, .F. ) ;
#33009 = ORIENTED_EDGE ( 'NONE', *, *, #51404, .T. ) ;
#33010 = PRESENTATION_LAYER_ASSIGNMENT (  '', '', ( #29595 ) ) ;
#33011 = DIRECTION ( 'NONE',  ( 0.000000000000000000, -1.000000000000000000, 0.000000000000000000 ) ) ;
#33012 = EDGE_CURVE ( 'NONE', #12588, #16496, #63011, .T. ) ;
#33013 =( REPRESENTATION_RELATIONSHIP ('NONE','NONE', #5102, #38844 ) REPRESENTATION_RELATIONSHIP_WITH_TRANSFORMATION ( #11016 )SHAPE_REPRESENTATION_RELATIONSHIP( ) );
#33014 = AXIS2_PLACEMENT_3D ( 'NONE', #50358, #54582, #60533 ) ;
#33015 = DIRECTION ( 'NONE',  ( 1.000000000000000000, 0.000000000000000000, 0.000000000000000000 ) ) ;
#33016 = CARTESIAN_POINT ( 'NONE',  ( 23.71231517720798010, 112.9999999999999858, -7.500000000000000000 ) ) ;
#33017 = CARTESIAN_POINT ( 'NONE',  ( -69.95707362346617231, 9.058813317711329915, -2.943386871421373119 ) ) ;
#33018 = VERTEX_POINT ( 'NONE', #19409 ) ;
#33019 = CARTESIAN_POINT ( 'NONE',  ( -110.9049999999999727, 2.607480562269069324, -8.024999999999993250 ) ) ;
#33020 = ORIENTED_EDGE ( 'NONE', *, *, #58546, .T. ) ;
#33021 = FILL_AREA_STYLE_COLOUR ( '', #60226 ) ;
#33022 = COLOUR_RGB ( '', 0.66274510, 0.83137255, 0.94901961) ;
#33023 = EDGE_LOOP ( 'NONE', ( #57498, #60719, #38947, #54205 ) ) ;
#33024 = CARTESIAN_POINT ( 'NONE',  ( -20.94636006565341191, 149.9999999999999716, 9.500000000000000000 ) ) ;
#33025 = CARTESIAN_POINT ( 'NONE',  ( 26.00000000000001776, 42.00000000000000000, -35.50000000000000000 ) ) ;
#33026 = VERTEX_POINT ( 'NONE', #36328 ) ;
#33027 = CIRCLE ( 'NONE', #12829, 5.000000000000004441 ) ;
#33028 = DIRECTION ( 'NONE',  ( -0.000000000000000000, 0.000000000000000000, -1.000000000000000000 ) ) ;
#33029 = CARTESIAN_POINT ( 'NONE',  ( -9.058813317711337021, 158.0449999999999875, -2.943386871421374895 ) ) ;
#33030 = FILL_AREA_STYLE_COLOUR ( '', #23928 ) ;
#33031 = ORIENTED_EDGE ( 'NONE', *, *, #10582, .T. ) ;
#33032 = PRESENTATION_LAYER_ASSIGNMENT (  '', '', ( #19565 ) ) ;
#33033 = ORIENTED_EDGE ( 'NONE', *, *, #8144, .T. ) ;
#33034 = DIRECTION ( 'NONE',  ( -0.000000000000000000, -1.000000000000000000, -0.000000000000000000 ) ) ;
#33035 = DIRECTION ( 'NONE',  ( 1.000000000000000000, 0.000000000000000000, 0.000000000000000000 ) ) ;
#33036 = FILL_AREA_STYLE ('',( #17235 ) ) ;
#33037 = CARTESIAN_POINT ( 'NONE',  ( -129.4429263765338192, -1.166476076187852838E-15, -9.524999999999991473 ) ) ;
#33038 = CIRCLE ( 'NONE', #38701, 0.2500000000000002220 ) ;
#33039 = ORIENTED_EDGE ( 'NONE', *, *, #66382, .F. ) ;
#33040 = CARTESIAN_POINT ( 'NONE',  ( 8.437984349512095861, 131.1929263765338192, 1.550032578732817026E-15 ) ) ;
#33041 = CARTESIAN_POINT ( 'NONE',  ( -53.60138880980050402, -9.947368421755438561, -2.262137787255405819 ) ) ;
#33042 = CARTESIAN_POINT ( 'NONE',  ( 26.00000000000001776, 15.00000000000000000, 29.68999999999999417 ) ) ;
#33043 = EDGE_CURVE ( 'NONE', #3437, #1680, #9584, .T. ) ;
#33044 = CARTESIAN_POINT ( 'NONE',  ( -105.4429263765338050, -1.166476076187852838E-15, -9.524999999999991473 ) ) ;
#33045 = FACE_OUTER_BOUND ( 'NONE', #19693, .T. ) ;
#33046 = ADVANCED_FACE ( 'NONE', ( #61965 ), #45828, .T. ) ;
#33047 = ORIENTED_EDGE ( 'NONE', *, *, #39178, .F. ) ;
#33048 = CYLINDRICAL_SURFACE ( 'NONE', #45321, 0.2500000000000002220 ) ;
#33049 = ORIENTED_EDGE ( 'NONE', *, *, #14168, .T. ) ;
#33050 = CARTESIAN_POINT ( 'NONE',  ( -48.14292637653380780, 5.598654528085800663, -7.705886871421367523 ) ) ;
#33051 = FILL_AREA_STYLE ('',( #64359 ) ) ;
#33052 = MECHANICAL_DESIGN_GEOMETRIC_PRESENTATION_REPRESENTATION (  '', ( #24054 ), #35313 ) ;
#33053 = CARTESIAN_POINT ( 'NONE',  ( -138.8050000000000068, -8.437984349512085203, 5.166775262442717831E-16 ) ) ;
#33054 = CARTESIAN_POINT ( 'NONE',  ( 23.21231517720797655, 117.9999999999999716, 7.000000000000000000 ) ) ;
#33055 = VERTEX_POINT ( 'NONE', #17202 ) ;
#33056 = MECHANICAL_DESIGN_GEOMETRIC_PRESENTATION_REPRESENTATION (  '', ( #11703 ), #48803 ) ;
#33057 = CIRCLE ( 'NONE', #57765, 0.5000000000000004441 ) ;
#33058 = EDGE_CURVE ( 'NONE', #60543, #42295, #44968, .T. ) ;
#33059 = CARTESIAN_POINT ( 'NONE',  ( -105.8929263765337936, -8.102448949553174629, -5.886773742842741797 ) ) ;
#33060 = FILL_AREA_STYLE_COLOUR ( '', #66440 ) ;
#33061 = CARTESIAN_POINT ( 'NONE',  ( 41.84210526315788314, 107.2928455055531458, 4.000000000000000888 ) ) ;
#33062 = ORIENTED_EDGE ( 'NONE', *, *, #21590, .T. ) ;
#33064 = EDGE_CURVE ( 'NONE', #35517, #33393, #2028, .T. ) ;
#33063 = ORIENTED_EDGE ( 'NONE', *, *, #9393, .F. ) ;
#33065 = DIRECTION ( 'NONE',  ( 0.000000000000000000, 0.000000000000000000, 1.000000000000000000 ) ) ;
#33066 = CARTESIAN_POINT ( 'NONE',  ( -54.65499999999997982, -7.632228543268600340, -2.479861379858950166 ) ) ;
#33067 = EDGE_LOOP ( 'NONE', ( #36462, #50814, #32931, #29479 ) ) ;
#33068 = DIRECTION ( 'NONE',  ( 0.000000000000000000, -1.000000000000000000, -0.000000000000000000 ) ) ;
#33069 = CARTESIAN_POINT ( 'NONE',  ( 0.000000000000000000, 14.00000000000000000, 80.00402776293826435 ) ) ;
#33070 = CARTESIAN_POINT ( 'NONE',  ( 32.00000000000000000, 43.00000000000000000, -79.00402776293826435 ) ) ;
#33071 = EDGE_CURVE ( 'NONE', #18094, #50964, #43871, .T. ) ;
#33072 = CIRCLE ( 'NONE', #51047, 3.600000000000005862 ) ;
#33073 = SURFACE_STYLE_USAGE ( .BOTH. , #26394 ) ;
#33074 = CARTESIAN_POINT ( 'NONE',  ( -128.9929263765338021, 8.102448949553172852, -5.886773742842744461 ) ) ;
#33075 = ORIENTED_EDGE ( 'NONE', *, *, #20413, .T. ) ;
#33076 = FILL_AREA_STYLE ('',( #11607 ) ) ;
#33077 = EDGE_CURVE ( 'NONE', #60418, #58121, #20456, .T. ) ;
#33078 =( LENGTH_UNIT ( ) NAMED_UNIT ( * ) SI_UNIT ( .MILLI., .METRE. ) );
#33079 = CARTESIAN_POINT ( 'NONE',  ( 48.74999999999999289, 24.74999999999998579, 3.750000000000000000 ) ) ;
#33080 = DIRECTION ( 'NONE',  ( -0.000000000000000000, 1.000000000000000000, -0.000000000000000000 ) ) ;
#33081 = CARTESIAN_POINT ( 'NONE',  ( -107.0949999999999847, -2.607480562269071545, -8.024999999999991473 ) ) ;
#33082 = CARTESIAN_POINT ( 'NONE',  ( 8.102448949553181734, 156.3950000000000102, 5.886773742842750679 ) ) ;
#33083 = CARTESIAN_POINT ( 'NONE',  ( -87.74499999999999034, 4.716976649647094177, 6.492361379858945902 ) ) ;
#33084 = DIRECTION ( 'NONE',  ( 0.000000000000000000, 1.000000000000000000, -0.000000000000000000 ) ) ;
#33085 = CIRCLE ( 'NONE', #43277, 0.5000000000000004441 ) ;
#33086 = DIRECTION ( 'NONE',  ( 0.000000000000000000, -0.000000000000000000, 1.000000000000000000 ) ) ;
#33087 = DIRECTION ( 'NONE',  ( -1.000000000000000000, 0.000000000000000000, 0.000000000000000000 ) ) ;
#33088 = PRESENTATION_LAYER_ASSIGNMENT (  '', '', ( #16303 ) ) ;
#33089 = SURFACE_STYLE_USAGE ( .BOTH. , #22884 ) ;
#33090 = ORIENTED_EDGE ( 'NONE', *, *, #27142, .F. ) ;
#33091 = CARTESIAN_POINT ( 'NONE',  ( -126.5929263765337964, -3.094860106618431139, -9.524999999999991473 ) ) ;
#33092 =( NAMED_UNIT ( * ) SI_UNIT ( $, .STERADIAN. ) SOLID_ANGLE_UNIT ( ) );
#33093 = CARTESIAN_POINT ( 'NONE',  ( -151.3449999999999989, 7.632228543268599452, -2.479861379858951942 ) ) ;
#33094 = DIRECTION ( 'NONE',  ( 0.000000000000000000, 0.000000000000000000, 1.000000000000000000 ) ) ;
#33095 =( GEOMETRIC_REPRESENTATION_CONTEXT ( 3 ) GLOBAL_UNCERTAINTY_ASSIGNED_CONTEXT ( ( #42681 ) ) GLOBAL_UNIT_ASSIGNED_CONTEXT ( ( #12308, #64418, #5646 ) ) REPRESENTATION_CONTEXT ( 'NONE', 'WORKASPACE' ) );
#33096 = CARTESIAN_POINT ( 'NONE',  ( -34.99999999999992895, 112.4999999999999858, 10.00000000000000000 ) ) ;
#33097 = CYLINDRICAL_SURFACE ( 'NONE', #51904, 1.000000000000000000 ) ;
#33098 = ORIENTED_EDGE ( 'NONE', *, *, #30716, .F. ) ;
#33099 = ORIENTED_EDGE ( 'NONE', *, *, #32914, .F. ) ;
#33100 = CARTESIAN_POINT ( 'NONE',  ( 29.00000000000002842, 5.569094604152796002, -2.026984667724097466 ) ) ;
#33101 = DIRECTION ( 'NONE',  ( 1.000000000000000000, 0.000000000000000000, 0.000000000000000000 ) ) ;
#33102 = EDGE_CURVE ( 'NONE', #60684, #7860, #31461, .T. ) ;
#33103 = VECTOR ( 'NONE', #37244, 1000.000000000000000 ) ;
#33104 = DIRECTION ( 'NONE',  ( -1.445602896647337931E-16, 1.000000000000000000, 0.000000000000000000 ) ) ;
#33105 =( NAMED_UNIT ( * ) PLANE_ANGLE_UNIT ( ) SI_UNIT ( $, .RADIAN. ) );
#33106 = LINE ( 'NONE', #59826, #9510 ) ;
#33107 = DIRECTION ( 'NONE',  ( 0.000000000000000000, 0.000000000000000000, 1.000000000000000000 ) ) ;
#33108 = VERTEX_POINT ( 'NONE', #27345 ) ;
#33109 = CARTESIAN_POINT ( 'NONE',  ( -142.7049999999999557, 2.607480562269072433, 8.024999999999991473 ) ) ;
#33110 = VERTEX_POINT ( 'NONE', #59352 ) ;
#33111 = AXIS2_PLACEMENT_3D ( 'NONE', #9113, #19286, #21642 ) ;
#33112 = ORIENTED_EDGE ( 'NONE', *, *, #48035, .T. ) ;
#33113 = CARTESIAN_POINT ( 'NONE',  ( 0.000000000000000000, 0.000000000000000000, 32.50000000000000000 ) ) ;
#33114 = DIRECTION ( 'NONE',  ( 0.000000000000000000, 0.000000000000000000, 1.000000000000000000 ) ) ;
#33115 = VERTEX_POINT ( 'NONE', #22443 ) ;
#33116 = AXIS2_PLACEMENT_3D ( 'NONE', #12067, #11025, #60266 ) ;
#33117 = AXIS2_PLACEMENT_3D ( 'NONE', #64238, #16096, #32235 ) ;
#33118 = FACE_OUTER_BOUND ( 'NONE', #37504, .T. ) ;
#33119 = DIRECTION ( 'NONE',  ( -0.9486832980505138790, -0.3162277660168378857, 0.000000000000000000 ) ) ;
#33120 = CARTESIAN_POINT ( 'NONE',  ( 3.094860106618431583, 132.0949999999999989, 9.525000000000000355 ) ) ;
#33121 = FILL_AREA_STYLE ('',( #12321 ) ) ;
#33122 = VERTEX_POINT ( 'NONE', #60070 ) ;
#33123 = EDGE_CURVE ( 'NONE', #47020, #8712, #49465, .T. ) ;
#33124 = SURFACE_SIDE_STYLE ('',( #343 ) ) ;
#33125 = CARTESIAN_POINT ( 'NONE',  ( 8.102448949553179958, 130.5049999999999955, 5.886773742842750679 ) ) ;
#33126 = CARTESIAN_POINT ( 'NONE',  ( -50.90499999999997982, 2.607480562269069324, -8.024999999999993250 ) ) ;
#33127 = CARTESIAN_POINT ( 'NONE',  ( -119.6950000000000074, -8.437984349512085203, 5.166775262442717831E-16 ) ) ;
#33128 = CARTESIAN_POINT ( 'NONE',  ( -74.99999999999998579, 64.49137674618943095, 9.500000000000000000 ) ) ;
#33129 = ORIENTED_EDGE ( 'NONE', *, *, #4568, .F. ) ;
#33130 = CARTESIAN_POINT ( 'NONE',  ( -4.716976649647097730, 111.2429263765338163, -6.492361379858953896 ) ) ;
#33131 = DIRECTION ( 'NONE',  ( 0.000000000000000000, 1.000000000000000000, 0.000000000000000000 ) ) ;
#33132 = TOROIDAL_SURFACE ( 'NONE', #46633, 0.5000000000000000000, 0.2500000000000000000 ) ;
#33133 = DIRECTION ( 'NONE',  ( 1.000000000000000000, 0.000000000000000000, 0.000000000000000000 ) ) ;
#33134 = ADVANCED_FACE ( 'NONE', ( #11887 ), #46127, .T. ) ;
#33135 = STYLED_ITEM ( 'NONE', ( #10011 ), #38867 ) ;
#33136 = CARTESIAN_POINT ( 'NONE',  ( 11.00000000000001776, 26.00000000000000355, 20.49999999999999645 ) ) ;
#33137 = EDGE_CURVE ( 'NONE', #35896, #31107, #54441, .T. ) ;
#33138 = STYLED_ITEM ( 'NONE', ( #4272 ), #57712 ) ;
#33139 = DIRECTION ( 'NONE',  ( 1.000000000000000000, -0.000000000000000000, 0.000000000000000000 ) ) ;
#33140 = ORIENTED_EDGE ( 'NONE', *, *, #11434, .F. ) ;
#33141 = FILL_AREA_STYLE_COLOUR ( '', #23264 ) ;
#33142 = CARTESIAN_POINT ( 'NONE',  ( -168.0550000000000068, -9.827790563157499189E-16, -8.024999999999991473 ) ) ;
#33143 = ORIENTED_EDGE ( 'NONE', *, *, #69031, .F. ) ;
#33144 = DIRECTION ( 'NONE',  ( -0.7071067811865549002, 0.000000000000000000, -0.7071067811865401342 ) ) ;
#33145 = COLOUR_RGB ( '', 0.31764706, 0.68627451, 0.89019608) ;
#33146 = FILL_AREA_STYLE ('',( #11674 ) ) ;
#33147 = EDGE_CURVE ( 'NONE', #26491, #2459, #59532, .T. ) ;
#33148 = CIRCLE ( 'NONE', #68001, 0.5000000000000004441 ) ;
#33149 = SURFACE_SIDE_STYLE ('',( #65132 ) ) ;
#33150 = CARTESIAN_POINT ( 'NONE',  ( -45.00000000000000000, 9.708372675170618749, 3.611004237778676185 ) ) ;
#33151 =( BOUNDED_CURVE ( )  B_SPLINE_CURVE ( 2, ( #29719, #35698, #25132, #13886, #14580, #46645, #30049, #67016, #3274, #19848, #62054 ),
 .UNSPECIFIED., .F., .F. ) 
 B_SPLINE_CURVE_WITH_KNOTS ( ( 3, 2, 2, 2, 2, 3 ),
 ( 0.2647058823529411242, 0.2705882352941175739, 0.2764705882352940791, 0.2823529411764705843, 0.2882352941176470340, 0.2941176470588235392 ),
 .UNSPECIFIED. ) 
 CURVE ( )  GEOMETRIC_REPRESENTATION_ITEM ( )  RATIONAL_B_SPLINE_CURVE ( ( 1.000000000000000666, 0.9510565162951531981, 1.000000000000000000, 0.9510565162951535312, 1.000000000000000000, 0.9510565162951535312, 1.000000000000000000, 0.9510565162951535312, 1.000000000000000000, 0.9510565162951535312, 1.000000000000000000 ) ) 
 REPRESENTATION_ITEM ( '' )  );
#33152 = EDGE_LOOP ( 'NONE', ( #25668, #21612, #58462, #178 ) ) ;
#33153 = EDGE_CURVE ( 'NONE', #56538, #55506, #61778, .T. ) ;
#33154 = CARTESIAN_POINT ( 'NONE',  ( -45.21668476461162101, 8.382617247524212445, -3.000000000000000000 ) ) ;
#33155 = CARTESIAN_POINT ( 'NONE',  ( -6.898093598910797652, 2.361802048420727385, 6.052151411320861207 ) ) ;
#33156 = CARTESIAN_POINT ( 'NONE',  ( -90.05499999999997840, -9.827790563157499189E-16, -8.024999999999991473 ) ) ;
#33157 = ORIENTED_EDGE ( 'NONE', *, *, #16044, .F. ) ;
#33158 = PRESENTATION_STYLE_ASSIGNMENT (( #59166 ) ) ;
#33159 = CARTESIAN_POINT ( 'NONE',  ( -65.60707362346616378, -8.102448949553172852, 5.886773742842742685 ) ) ;
#33160 = COLOUR_RGB ( '', 0.66274510, 0.83137255, 0.94901961) ;
#33161 = PRESENTATION_LAYER_ASSIGNMENT (  '', '', ( #8456 ) ) ;
#33162 = CARTESIAN_POINT ( 'NONE',  ( -75.00000000000000000, 8.553059399042478361, -6.924772212933357984 ) ) ;
#33163 = ORIENTED_EDGE ( 'NONE', *, *, #48945, .F. ) ;
#33164 = FACE_OUTER_BOUND ( 'NONE', #40636, .T. ) ;
#33166 = FACE_OUTER_BOUND ( 'NONE', #66160, .T. ) ;
#33165 = DIRECTION ( 'NONE',  ( 1.000000000000000000, 0.000000000000000000, 0.000000000000000000 ) ) ;
#33167 = CARTESIAN_POINT ( 'NONE',  ( -102.3549999999999898, -4.716976649647093289, -6.492361379858945902 ) ) ;
#33168 = EDGE_CURVE ( 'NONE', #20521, #69477, #15786, .T. ) ;
#33169 = CARTESIAN_POINT ( 'NONE',  ( -8.102448949553181734, 130.8949999999999818, -5.886773742842749790 ) ) ;
#33170 = CARTESIAN_POINT ( 'NONE',  ( -113.9949999999999903, -6.826472737025115478, 4.959722759717900331 ) ) ;
#33171 = PRESENTATION_LAYER_ASSIGNMENT (  '', '', ( #5079 ) ) ;
#33172 = DIRECTION ( 'NONE',  ( 1.000000000000000000, -0.000000000000000000, -0.000000000000000000 ) ) ;
#33173 = ADVANCED_FACE ( 'NONE', ( #1945 ), #36015, .T. ) ;
#33174 = CARTESIAN_POINT ( 'NONE',  ( -15.98999599679679839, 146.4999999999999716, 7.000000000000000000 ) ) ;
#33175 = CARTESIAN_POINT ( 'NONE',  ( -153.7429263765338021, -5.598654528085803328, -7.705886871421366635 ) ) ;
#33176 = FILL_AREA_STYLE ('',( #59891 ) ) ;
#33177 = CARTESIAN_POINT ( 'NONE',  ( -174.4449999999999932, 0.000000000000000000, 8.024999999999991473 ) ) ;
#33178 = CARTESIAN_POINT ( 'NONE',  ( 2.000000000000008882, 50.00000000000000000, -59.99999999999999289 ) ) ;
#33179 = AXIS2_PLACEMENT_3D ( 'NONE', #54572, #692, #16968 ) ;
#33180 = DIRECTION ( 'NONE',  ( 1.000000000000000000, 0.000000000000000000, 0.000000000000000000 ) ) ;
#33181 = ORIENTED_EDGE ( 'NONE', *, *, #43175, .T. ) ;
#33182 = DIRECTION ( 'NONE',  ( -1.445602896647339656E-16, -1.000000000000000000, 0.000000000000000000 ) ) ;
#33183 = ORIENTED_EDGE ( 'NONE', *, *, #63536, .F. ) ;
#33184 = CARTESIAN_POINT ( 'NONE',  ( -65.39292637653379359, 8.102448949553176405, 5.886773742842740909 ) ) ;
#33185 = TOROIDAL_SURFACE ( 'NONE', #8497, 3.499999999999998668, 1.000000000000000000 ) ;
#33186 = CARTESIAN_POINT ( 'NONE',  ( 27.99999999999999645, 5.000000000000000000, -72.00402776293822171 ) ) ;
#33187 = PRESENTATION_STYLE_ASSIGNMENT (( #21581 ) ) ;
#33188 = AXIS2_PLACEMENT_3D ( 'NONE', #5122, #64583, #65255 ) ;
#33189 = CARTESIAN_POINT ( 'NONE',  ( -142.3429263765338249, -9.058813317711329915, 2.943386871421371787 ) ) ;
#33190 = DIRECTION ( 'NONE',  ( 0.000000000000000000, -1.000000000000000000, 0.000000000000000000 ) ) ;
#33191 = CARTESIAN_POINT ( 'NONE',  ( 30.99999999999999289, 5.000000000000000000, 24.00402776293822171 ) ) ;
#33192 = ORIENTED_EDGE ( 'NONE', *, *, #37858, .T. ) ;
#33193 = CARTESIAN_POINT ( 'NONE',  ( -173.1550000000000011, 7.632228543268600340, 2.479861379858949277 ) ) ;
#33194 = ORIENTED_EDGE ( 'NONE', *, *, #14593, .F. ) ;
#33195 =( NAMED_UNIT ( * ) SI_UNIT ( $, .STERADIAN. ) SOLID_ANGLE_UNIT ( ) );
#33197 = EDGE_CURVE ( 'NONE', #7813, #14819, #66743, .T. ) ;
#33196 =( NAMED_UNIT ( * ) SI_UNIT ( $, .STERADIAN. ) SOLID_ANGLE_UNIT ( ) );
#33198 = CYLINDRICAL_SURFACE ( 'NONE', #62169, 9.524999999999991473 ) ;
#33199 = CYLINDRICAL_SURFACE ( 'NONE', #17425, 0.5000000000000004441 ) ;
#33200 = CARTESIAN_POINT ( 'NONE',  ( -4.716976649647097730, 157.3570736234661638, -6.492361379858953896 ) ) ;
#33201 = AXIS2_PLACEMENT_3D ( 'NONE', #50199, #44946, #18173 ) ;
#33202 = ORIENTED_EDGE ( 'NONE', *, *, #51876, .F. ) ;
#33203 = EDGE_CURVE ( 'NONE', #50598, #63457, #39342, .T. ) ;
#33204 = CARTESIAN_POINT ( 'NONE',  ( -79.70499999999996987, 2.607480562269072433, 8.024999999999991473 ) ) ;
#33205 = PRESENTATION_STYLE_ASSIGNMENT (( #55337 ) ) ;
#33206 = SURFACE_SIDE_STYLE ('',( #59211 ) ) ;
#33207 = VECTOR ( 'NONE', #40903, 1000.000000000000000 ) ;
#33208 = EDGE_CURVE ( 'NONE', #45813, #60757, #29798, .T. ) ;
#33209 =( NAMED_UNIT ( * ) SI_UNIT ( $, .STERADIAN. ) SOLID_ANGLE_UNIT ( ) );
#33210 = CARTESIAN_POINT ( 'NONE',  ( 10.42000000000000348, -1.224646799147353651E-15, -12.50000000000000000 ) ) ;
#33211 = ORIENTED_EDGE ( 'NONE', *, *, #36584, .F. ) ;
#33212 = CARTESIAN_POINT ( 'NONE',  ( 44.99999999999998579, 119.9999999999999716, 7.000000000000000000 ) ) ;
#33213 = DIRECTION ( 'NONE',  ( 0.000000000000000000, 0.000000000000000000, -1.000000000000000000 ) ) ;
#33214 = CARTESIAN_POINT ( 'NONE',  ( -63.59499999999997755, 2.607480562269073321, 8.024999999999991473 ) ) ;
#33215 = ORIENTED_EDGE ( 'NONE', *, *, #42934, .T. ) ;
#33216 = CYLINDRICAL_SURFACE ( 'NONE', #64275, 9.524999999999991473 ) ;
#33217 = DIRECTION ( 'NONE',  ( -1.000000000000000000, 0.000000000000000000, 0.000000000000000000 ) ) ;
#33218 = VERTEX_POINT ( 'NONE', #19219 ) ;
#33219 =( NAMED_UNIT ( * ) PLANE_ANGLE_UNIT ( ) SI_UNIT ( $, .RADIAN. ) );
#33220 = DIRECTION ( 'NONE',  ( -1.000000000000000000, -0.000000000000000000, -0.000000000000000000 ) ) ;
#33221 = ORIENTED_EDGE ( 'NONE', *, *, #8206, .T. ) ;
#33222 = EDGE_CURVE ( 'NONE', #38944, #42646, #51727, .T. ) ;
#33223 = CARTESIAN_POINT ( 'NONE',  ( -184.0000000000000000, 6.735557395310425260E-16, -5.499999999999985789 ) ) ;
#33224 = CARTESIAN_POINT ( 'NONE',  ( -75.00000000000000000, 8.747695062214207340, 6.883368695986967545 ) ) ;
#33225 = CARTESIAN_POINT ( 'NONE',  ( -115.4049999999999727, -2.607480562269069768, 8.024999999999991473 ) ) ;
#33226 = EDGE_LOOP ( 'NONE', ( #49627, #17797, #57253, #15195, #12529, #43725, #50452 ) ) ;
#33227 = DIRECTION ( 'NONE',  ( 0.000000000000000000, -1.000000000000000000, 0.000000000000000000 ) ) ;
#33228 = FILL_AREA_STYLE_COLOUR ( '', #17353 ) ;
#33229 = STYLED_ITEM ( 'NONE', ( #615 ), #58308 ) ;
#33230 = CARTESIAN_POINT ( 'NONE',  ( -75.00000000000000000, -2.215169945516535778E-14, 10.00000000000000000 ) ) ;
#33231 = CARTESIAN_POINT ( 'NONE',  ( -146.7570736234661695, -5.598654528085801552, 7.705886871421367523 ) ) ;
#33232 = CARTESIAN_POINT ( 'NONE',  ( 9.058813317711337021, 129.5449999999999875, 2.943386871421375783 ) ) ;
#33233 = TOROIDAL_SURFACE ( 'NONE', #6255, 9.499999999999996447, 0.5000000000000000000 ) ;
#33234 = CARTESIAN_POINT ( 'NONE',  ( -96.35707362346616378, 5.598654528085804216, 7.705886871421366635 ) ) ;
#33235 = VECTOR ( 'NONE', #23995, 1000.000000000000000 ) ;
#33236 = FACE_OUTER_BOUND ( 'NONE', #56311, .T. ) ;
#33237 = VERTEX_POINT ( 'NONE', #45326 ) ;
#33238 = DIRECTION ( 'NONE',  ( -1.000000000000000000, 0.000000000000000000, 0.000000000000000000 ) ) ;
#33240 = LINE ( 'NONE', #36022, #25757 ) ;
#33239 = DIRECTION ( 'NONE',  ( -0.000000000000000000, -0.000000000000000000, -1.000000000000000000 ) ) ;
#33241 = DIRECTION ( 'NONE',  ( 0.000000000000000000, -0.000000000000000000, 1.000000000000000000 ) ) ;
#33242 = CARTESIAN_POINT ( 'NONE',  ( -132.8050000000000068, -8.437984349512085203, 5.166775262442717831E-16 ) ) ;
#33243 = CYLINDRICAL_SURFACE ( 'NONE', #4972, 0.2500000000000002220 ) ;
#33244 =( NAMED_UNIT ( * ) PLANE_ANGLE_UNIT ( ) SI_UNIT ( $, .RADIAN. ) );
#33245 = CARTESIAN_POINT ( 'NONE',  ( -149.9949999999999193, -6.826472737025115478, 4.959722759717900331 ) ) ;
#33246 = CARTESIAN_POINT ( 'NONE',  ( -131.2450000000000045, -4.716976649647093289, -6.492361379858945902 ) ) ;
#33247 = ORIENTED_EDGE ( 'NONE', *, *, #27221, .F. ) ;
#33248 = CARTESIAN_POINT ( 'NONE',  ( -87.44292637653380496, -1.166476076187852838E-15, -9.524999999999991473 ) ) ;
#33249 =( LENGTH_UNIT ( ) NAMED_UNIT ( * ) SI_UNIT ( .MILLI., .METRE. ) );
#33250 = TOROIDAL_SURFACE ( 'NONE', #1763, 17.00000000000000355, 1.000000000000000000 ) ;
#33251 = FILL_AREA_STYLE ('',( #23376 ) ) ;
#33252 = CARTESIAN_POINT ( 'NONE',  ( 0.000000000000000000, 43.00000000000000000, 0.000000000000000000 ) ) ;
#33253 = UNCERTAINTY_MEASURE_WITH_UNIT (LENGTH_MEASURE( 1.000000000000000082E-05 ), #49269, 'distance_accuracy_value', 'NONE');
#33254 = CARTESIAN_POINT ( 'NONE',  ( -182.2429263765338021, 5.598654528085804216, 7.705886871421366635 ) ) ;
#33255 =( LENGTH_UNIT ( ) NAMED_UNIT ( * ) SI_UNIT ( .MILLI., .METRE. ) );
#33256 = CARTESIAN_POINT ( 'NONE',  ( -62.84499999999998465, -7.632228543268599452, 2.479861379858951054 ) ) ;
#33257 = MECHANICAL_DESIGN_GEOMETRIC_PRESENTATION_REPRESENTATION (  '', ( #55748 ), #11901 ) ;
#33258 = DIRECTION ( 'NONE',  ( -1.000000000000000000, 0.000000000000000000, 0.000000000000000000 ) ) ;
#33259 = CARTESIAN_POINT ( 'NONE',  ( 21.75000000000001066, 22.24999999999998224, 3.750000000000000000 ) ) ;
#33260 = CYLINDRICAL_SURFACE ( 'NONE', #6211, 0.5000000000000004441 ) ;
#33261 = COLOUR_RGB ( '', 0.31764706, 0.68627451, 0.89019608) ;
#33262 = DIRECTION ( 'NONE',  ( 1.156482317317866302E-16, -1.000000000000000000, 0.000000000000000000 ) ) ;
#33263 = CARTESIAN_POINT ( 'NONE',  ( -75.35707362346617799, 5.598654528085804216, 7.705886871421366635 ) ) ;
#33264 = CARTESIAN_POINT ( 'NONE',  ( -99.44292637653380496, -1.166476076187852838E-15, -9.524999999999991473 ) ) ;
#33265 = APPLICATION_PROTOCOL_DEFINITION ( 'draft international standard', 'automotive_design', 1998, #63519 ) ;
#33266 =( BOUNDED_CURVE ( )  B_SPLINE_CURVE ( 2, ( #60495, #12307, #66495, #55930, #19327, #9149, #35534, #30565, #68579, #2774, #30924 ),
 .UNSPECIFIED., .F., .F. ) 
 B_SPLINE_CURVE_WITH_KNOTS ( ( 3, 2, 2, 2, 2, 3 ),
 ( 0.6086956521738987602, 0.6108695652173770085, 0.6130434782608551458, 0.6152173913043333942, 0.6173913043478115314, 0.6195652173912897798 ),
 .UNSPECIFIED. ) 
 CURVE ( )  GEOMETRIC_REPRESENTATION_ITEM ( )  RATIONAL_B_SPLINE_CURVE ( ( 1.000000000000322409, 0.9510565162948311224, 1.000000000000000000, 0.9510565162951535312, 1.000000000000000000, 0.9510565162951535312, 1.000000000000000000, 0.9510565162951535312, 1.000000000000000000, 0.9510565162954809360, 0.9999999999996725952 ) ) 
 REPRESENTATION_ITEM ( '' )  );
#33267 = CARTESIAN_POINT ( 'NONE',  ( -162.6570736234661751, 9.058813317711329915, 2.943386871421369566 ) ) ;
#33268 =( LENGTH_UNIT ( ) NAMED_UNIT ( * ) SI_UNIT ( .MILLI., .METRE. ) );
#33269 = CYLINDRICAL_SURFACE ( 'NONE', #7770, 1.000000000000000888 ) ;
#33270 = VECTOR ( 'NONE', #12938, 1000.000000000000000 ) ;
#33271 =( NAMED_UNIT ( * ) SI_UNIT ( $, .STERADIAN. ) SOLID_ANGLE_UNIT ( ) );
#33272 = ORIENTED_EDGE ( 'NONE', *, *, #31873, .F. ) ;
#33273 = EDGE_CURVE ( 'NONE', #28793, #47709, #47295, .T. ) ;
#33274 = SPHERICAL_SURFACE ( 'NONE', #59821, 0.2500000000000000000 ) ;
#33275 = AXIS2_PLACEMENT_3D ( 'NONE', #25429, #19807, #14522 ) ;
#33276 = ORIENTED_EDGE ( 'NONE', *, *, #2902, .F. ) ;
#33277 = SURFACE_SIDE_STYLE ('',( #32226 ) ) ;
#33279 = CARTESIAN_POINT ( 'NONE',  ( -6.826472737025120807, 125.1070736234661638, 4.959722759717906548 ) ) ;
#33278 = AXIS2_PLACEMENT_3D ( 'NONE', #19078, #56378, #13120 ) ;
#33280 = CARTESIAN_POINT ( 'NONE',  ( 24.75000000000000355, 37.00000000000000000, 4.000000000000000000 ) ) ;
#33281 = CARTESIAN_POINT ( 'NONE',  ( 6.826472737025121695, 138.6070736234661638, -4.959722759717905660 ) ) ;
#33282 = CARTESIAN_POINT ( 'NONE',  ( 34.99999999999999289, 99.99999999999998579, -7.500000000000000000 ) ) ;
#33283 = ORIENTED_EDGE ( 'NONE', *, *, #29702, .T. ) ;
#33284 = ORIENTED_EDGE ( 'NONE', *, *, #37126, .T. ) ;
#33285 = CARTESIAN_POINT ( 'NONE',  ( -4.041451884327380562, -1.417096231345237545, -7.000000000000003553 ) ) ;
#33286 = EDGE_CURVE ( 'NONE', #66441, #46816, #45882, .T. ) ;
#33287 = FILL_AREA_STYLE ('',( #43878 ) ) ;
#33288 = EDGE_LOOP ( 'NONE', ( #52784, #9507, #42279, #48491 ) ) ;
#33289 = DIRECTION ( 'NONE',  ( 1.000000000000000000, 0.000000000000000000, 0.000000000000000000 ) ) ;
#33290 = CARTESIAN_POINT ( 'NONE',  ( -119.6070736234661638, -8.102448949553174629, 5.886773742842742685 ) ) ;
#33291 = EDGE_CURVE ( 'NONE', #57684, #16642, #15389, .T. ) ;
#33292 = EDGE_CURVE ( 'NONE', #2723, #16561, #15717, .T. ) ;
#33293 = CARTESIAN_POINT ( 'NONE',  ( 7.632228543268608334, 134.3429263765337964, -2.479861379858951942 ) ) ;
#33294 = CARTESIAN_POINT ( 'NONE',  ( -93.74499999999999034, 4.716976649647094177, 6.492361379858945902 ) ) ;
#33295 = ORIENTED_EDGE ( 'NONE', *, *, #6321, .F. ) ;
#33296 = LINE ( 'NONE', #1901, #69325 ) ;
#33297 = EDGE_CURVE ( 'NONE', #4250, #54470, #65053, .T. ) ;
#33298 = SURFACE_SIDE_STYLE ('',( #28326 ) ) ;
#33299 = UNCERTAINTY_MEASURE_WITH_UNIT (LENGTH_MEASURE( 1.000000000000000082E-05 ), #65731, 'distance_accuracy_value', 'NONE');
#33300 = ORIENTED_EDGE ( 'NONE', *, *, #61045, .T. ) ;
#33301 = DIRECTION ( 'NONE',  ( -1.000000000000000000, 0.000000000000000000, -0.000000000000000000 ) ) ;
#33302 = LINE ( 'NONE', #65303, #15613 ) ;
#33303 =( GEOMETRIC_REPRESENTATION_CONTEXT ( 3 ) GLOBAL_UNCERTAINTY_ASSIGNED_CONTEXT ( ( #58683 ) ) GLOBAL_UNIT_ASSIGNED_CONTEXT ( ( #52363, #4830, #25579 ) ) REPRESENTATION_CONTEXT ( 'NONE', 'WORKASPACE' ) );
#33304 = EDGE_CURVE ( 'NONE', #22147, #25561, #20979, .T. ) ;
#33305 = CYLINDRICAL_SURFACE ( 'NONE', #59227, 0.2500000000000002220 ) ;
#33306 = ORIENTED_EDGE ( 'NONE', *, *, #21368, .T. ) ;
#33307 = CARTESIAN_POINT ( 'NONE',  ( -184.0000000000000000, 0.000000000000000000, 0.000000000000000000 ) ) ;
#33308 = ORIENTED_EDGE ( 'NONE', *, *, #42011, .T. ) ;
#33309 = FACE_OUTER_BOUND ( 'NONE', #68313, .T. ) ;
#33310 = COLOUR_RGB ( '', 0.09019608, 0.27058824, 0.51372549) ;
#33311 = LINE ( 'NONE', #854, #14453 ) ;
#33312 = FACE_OUTER_BOUND ( 'NONE', #1494, .T. ) ;
#33313 = CARTESIAN_POINT ( 'NONE',  ( 9.201091548649898755, 3.348923446466848475, 12.50000000000000000 ) ) ;
#33314 = CARTESIAN_POINT ( 'NONE',  ( -181.8570736234661638, -5.598654528085803328, -7.705886871421366635 ) ) ;
#33315 = FACE_OUTER_BOUND ( 'NONE', #14766, .T. ) ;
#33316 = CARTESIAN_POINT ( 'NONE',  ( -8.527945164174161263, 153.6178632149283487, 1.507062088730512617 ) ) ;
#33317 = EDGE_LOOP ( 'NONE', ( #55613, #57050, #10316, #50673 ) ) ;
#33318 = CARTESIAN_POINT ( 'NONE',  ( -79.99999999999998579, 50.00000000000000000, -6.999999999999988454 ) ) ;
#33319 = DIRECTION ( 'NONE',  ( -0.000000000000000000, -1.000000000000000000, -0.000000000000000000 ) ) ;
#33320 = CARTESIAN_POINT ( 'NONE',  ( -149.7570736234661979, -5.598654528085801552, 7.705886871421367523 ) ) ;
#33321 =( NAMED_UNIT ( * ) SI_UNIT ( $, .STERADIAN. ) SOLID_ANGLE_UNIT ( ) );
#33323 = VERTEX_POINT ( 'NONE', #37196 ) ;
#33322 = AXIS2_PLACEMENT_3D ( 'NONE', #38948, #32946, #33964 ) ;
#33324 = CARTESIAN_POINT ( 'NONE',  ( -156.3549999999999898, -4.716976649647093289, -6.492361379858945902 ) ) ;
#33325 = DIRECTION ( 'NONE',  ( -0.000000000000000000, -1.000000000000000000, -0.000000000000000000 ) ) ;
#33326 = CARTESIAN_POINT ( 'NONE',  ( -6.422934014168760974, 111.9999999999999858, 4.811085495980506721 ) ) ;
#33327 = CARTESIAN_POINT ( 'NONE',  ( -174.5949999999999989, 2.607480562269073321, 8.024999999999991473 ) ) ;
#33328 = CARTESIAN_POINT ( 'NONE',  ( -161.5449999999999875, -7.632228543268600340, -2.479861379858950166 ) ) ;
#33329 = ORIENTED_EDGE ( 'NONE', *, *, #3531, .T. ) ;
#33330 = SURFACE_SIDE_STYLE ('',( #38653 ) ) ;
#33331 = CARTESIAN_POINT ( 'NONE',  ( 45.00320036294371562, 10.00106678764790225, 3.045234739864684403 ) ) ;
#33332 = DIRECTION ( 'NONE',  ( -1.000000000000000000, -0.000000000000000000, -0.000000000000000000 ) ) ;
#33333 = CARTESIAN_POINT ( 'NONE',  ( -69.65499999999998693, -7.632228543268600340, -2.479861379858950166 ) ) ;
#33334 = DIRECTION ( 'NONE',  ( 0.000000000000000000, 0.000000000000000000, -1.000000000000000000 ) ) ;
#33336 = AXIS2_PLACEMENT_3D ( 'NONE', #38533, #26843, #64164 ) ;
#33335 = DIRECTION ( 'NONE',  ( -1.000000000000000000, -0.000000000000000000, -0.000000000000000000 ) ) ;
#33337 = CARTESIAN_POINT ( 'NONE',  ( -79.19499999999997897, 8.437984349512086979, -1.550032578732815448E-15 ) ) ;
#33338 = CARTESIAN_POINT ( 'NONE',  ( 0.000000000000000000, 134.5549999999999784, -9.525000000000000355 ) ) ;
#33339 = CARTESIAN_POINT ( 'NONE',  ( -7.632228543268607446, 126.5429263765337993, -2.479861379858953718 ) ) ;
#33340 = UNCERTAINTY_MEASURE_WITH_UNIT (LENGTH_MEASURE( 1.000000000000000082E-05 ), #4079, 'distance_accuracy_value', 'NONE');
#33341 =( NAMED_UNIT ( * ) SI_UNIT ( $, .STERADIAN. ) SOLID_ANGLE_UNIT ( ) );
#33342 = DIRECTION ( 'NONE',  ( -1.000000000000000000, -0.000000000000000000, -0.000000000000000000 ) ) ;
#33343 = ORIENTED_EDGE ( 'NONE', *, *, #25255, .T. ) ;
#33344 = SURFACE_STYLE_FILL_AREA ( #1263 ) ;
#33345 = DIRECTION ( 'NONE',  ( 0.000000000000000000, 1.000000000000000000, 0.000000000000000000 ) ) ;
#33346 = STYLED_ITEM ( 'NONE', ( #46690 ), #65115 ) ;
#33347 = CARTESIAN_POINT ( 'NONE',  ( 30.50000000000000711, 18.99999999999997868, 4.000000000000000000 ) ) ;
#33348 = MECHANICAL_DESIGN_GEOMETRIC_PRESENTATION_REPRESENTATION (  '', ( #32242 ), #44638 ) ;
#33349 = EDGE_CURVE ( 'NONE', #33822, #53938, #47774, .T. ) ;
#33350 = CARTESIAN_POINT ( 'NONE',  ( 44.99999999999998579, 119.9999999999999716, 9.500000000000000000 ) ) ;
#33351 = CIRCLE ( 'NONE', #16574, 3.500000000000003553 ) ;
#33352 = ORIENTED_EDGE ( 'NONE', *, *, #15691, .F. ) ;
#33353 = ORIENTED_EDGE ( 'NONE', *, *, #23202, .F. ) ;
#33354 = LINE ( 'NONE', #28746, #48773 ) ;
#33355 = ADVANCED_FACE ( 'NONE', ( #14668 ), #62489, .F. ) ;
#33356 = CARTESIAN_POINT ( 'NONE',  ( 21.02379604162863913, 110.4999999999999858, 9.500000000000000000 ) ) ;
#33357 = EDGE_CURVE ( 'NONE', #40163, #54309, #39394, .T. ) ;
#33358 = CARTESIAN_POINT ( 'NONE',  ( -70.25707362346616947, 5.598654528085800663, -7.705886871421367523 ) ) ;
#33359 = EDGE_LOOP ( 'NONE', ( #9618, #14454, #14367, #89 ) ) ;
#33360 = CARTESIAN_POINT ( 'NONE',  ( -115.7049999999999841, 2.607480562269072433, 8.024999999999991473 ) ) ;
#33361 = ORIENTED_EDGE ( 'NONE', *, *, #25816, .F. ) ;
#33362 = CARTESIAN_POINT ( 'NONE',  ( 60.00000000000000000, 110.4999999999999858, -10.00000000000000000 ) ) ;
#33363 = AXIS2_PLACEMENT_3D ( 'NONE', #1398, #1750, #60517 ) ;
#33364 = SURFACE_STYLE_USAGE ( .BOTH. , #11551 ) ;
#33365 = EDGE_LOOP ( 'NONE', ( #32793, #51191, #19806, #30082 ) ) ;
#33366 = CARTESIAN_POINT ( 'NONE',  ( -57.29292637653379217, 3.094860106618428031, -9.524999999999993250 ) ) ;
#33367 = CARTESIAN_POINT ( 'NONE',  ( -67.55707362346618083, -1.166476076187852838E-15, -9.524999999999991473 ) ) ;
#33368 = VERTEX_POINT ( 'NONE', #52994 ) ;
#33369 = EDGE_CURVE ( 'NONE', #246, #2194, #49785, .T. ) ;
#33370 = SURFACE_STYLE_FILL_AREA ( #44322 ) ;
#33371 = CARTESIAN_POINT ( 'NONE',  ( 3.094860106618431583, 159.0949999999999420, 9.525000000000000355 ) ) ;
#33372 = DIRECTION ( 'NONE',  ( -0.000000000000000000, -0.000000000000000000, -1.000000000000000000 ) ) ;
#33373 = ORIENTED_EDGE ( 'NONE', *, *, #65990, .F. ) ;
#33374 = VERTEX_POINT ( 'NONE', #42474 ) ;
#33375 = PRESENTATION_STYLE_ASSIGNMENT (( #64701 ) ) ;
#33376 =( LENGTH_UNIT ( ) NAMED_UNIT ( * ) SI_UNIT ( .MILLI., .METRE. ) );
#33377 = CARTESIAN_POINT ( 'NONE',  ( -152.6070736234661354, -8.102448949553174629, 5.886773742842742685 ) ) ;
#33378 = EDGE_CURVE ( 'NONE', #14708, #27627, #25538, .T. ) ;
#33379 = VERTEX_POINT ( 'NONE', #20632 ) ;
#33380 = CARTESIAN_POINT ( 'NONE',  ( -2.607480562269073765, 135.0929263765338249, -8.025000000000000355 ) ) ;
#33381 = DIRECTION ( 'NONE',  ( 0.000000000000000000, 0.000000000000000000, 1.000000000000000000 ) ) ;
#33382 = DIRECTION ( 'NONE',  ( 0.000000000000000000, -1.000000000000000000, 0.000000000000000000 ) ) ;
#33383 = CARTESIAN_POINT ( 'NONE',  ( -104.9929263765337879, 8.102448949553172852, -5.886773742842744461 ) ) ;
#33384 = CARTESIAN_POINT ( 'NONE',  ( -13.25000000000000355, 27.99999999999998934, 4.000000000000000000 ) ) ;
#33385 = ORIENTED_EDGE ( 'NONE', *, *, #44535, .F. ) ;
#33386 = ORIENTED_EDGE ( 'NONE', *, *, #56809, .F. ) ;
#33387 = SPHERICAL_SURFACE ( 'NONE', #33406, 0.2500000000000000000 ) ;
#33388 = CARTESIAN_POINT ( 'NONE',  ( 12.75000000000000533, 27.74999999999998224, 3.750000000000000000 ) ) ;
#33389 = CARTESIAN_POINT ( 'NONE',  ( -143.0050000000000239, 6.826472737025116366, 4.959722759717898555 ) ) ;
#33390 = SURFACE_SIDE_STYLE ('',( #66431 ) ) ;
#33391 =( NAMED_UNIT ( * ) PLANE_ANGLE_UNIT ( ) SI_UNIT ( $, .RADIAN. ) );
#33392 = UNCERTAINTY_MEASURE_WITH_UNIT (LENGTH_MEASURE( 1.000000000000000082E-05 ), #42824, 'distance_accuracy_value', 'NONE');
#33393 = VERTEX_POINT ( 'NONE', #20272 ) ;
#33394 = DIRECTION ( 'NONE',  ( -1.000000000000000000, 0.000000000000000000, 0.000000000000000000 ) ) ;
#33395 = CARTESIAN_POINT ( 'NONE',  ( -45.00000000000000000, 9.372904743120717086, -6.583929160757660881 ) ) ;
#33396 = EDGE_LOOP ( 'NONE', ( #42030, #55097 ) ) ;
#33397 = STYLED_ITEM ( 'NONE', ( #32254 ), #58687 ) ;
#33398 = ORIENTED_EDGE ( 'NONE', *, *, #29458, .F. ) ;
#33399 = CARTESIAN_POINT ( 'NONE',  ( -4.750000000000002665, 24.74999999999998579, 3.750000000000000000 ) ) ;
#33400 = SURFACE_SIDE_STYLE ('',( #17598 ) ) ;
#33401 = CARTESIAN_POINT ( 'NONE',  ( -51.95499999999996987, -7.632228543268599452, 2.479861379858951054 ) ) ;
#33402 = ORIENTED_EDGE ( 'NONE', *, *, #63392, .T. ) ;
#33403 = DIRECTION ( 'NONE',  ( -1.000000000000000000, 1.224646799147349509E-16, 0.000000000000000000 ) ) ;
#33404 = FACE_OUTER_BOUND ( 'NONE', #21986, .T. ) ;
#33406 = AXIS2_PLACEMENT_3D ( 'NONE', #43317, #16890, #54815 ) ;
#33405 = CARTESIAN_POINT ( 'NONE',  ( -48.50000000000000000, 14.49137674618942562, 7.500000000000000000 ) ) ;
#33407 = CARTESIAN_POINT ( 'NONE',  ( 23.21231517720797655, 117.9999999999999716, 7.500000000000000000 ) ) ;
#33408 = CARTESIAN_POINT ( 'NONE',  ( -128.3929263765338078, 8.102448949553176405, 5.886773742842740909 ) ) ;
#33409 = ORIENTED_EDGE ( 'NONE', *, *, #55351, .T. ) ;
#33410 = EDGE_CURVE ( 'NONE', #6607, #44763, #15040, .T. ) ;
#33411 = CARTESIAN_POINT ( 'NONE',  ( 5.000000000000000000, 6.123233995736766282E-16, 0.2499999999999941436 ) ) ;
#33412 = CARTESIAN_POINT ( 'NONE',  ( 19.49999999999997513, 8.000000000000000000, -4.000000000000000000 ) ) ;
#33413 = DIRECTION ( 'NONE',  ( 0.000000000000000000, 0.000000000000000000, 1.000000000000000000 ) ) ;
#33414 = SPHERICAL_SURFACE ( 'NONE', #53836, 0.2500000000000000000 ) ;
#33415 = CARTESIAN_POINT ( 'NONE',  ( -60.00000000000000000, -2.024042244987997205E-14, 11.50000000000003020 ) ) ;
#33416 = CARTESIAN_POINT ( 'NONE',  ( -113.3949999999999818, -6.826472737025113702, -4.959722759717900331 ) ) ;
#33417 = CARTESIAN_POINT ( 'NONE',  ( -5.598654528085806881, 110.8549999999999756, -7.705886871421374629 ) ) ;
#33418 = CARTESIAN_POINT ( 'NONE',  ( -74.24499999999999034, -4.716976649647093289, -6.492361379858945902 ) ) ;
#33419 = DIRECTION ( 'NONE',  ( -1.000000000000000000, 0.000000000000000000, 0.000000000000000000 ) ) ;
#33420 = FACE_OUTER_BOUND ( 'NONE', #54113, .T. ) ;
#33421 = DIRECTION ( 'NONE',  ( -1.000000000000000000, 1.224646799147349509E-16, 0.000000000000000000 ) ) ;
#33422 = UNCERTAINTY_MEASURE_WITH_UNIT (LENGTH_MEASURE( 1.000000000000000082E-05 ), #49212, 'distance_accuracy_value', 'NONE');
#33424 = CARTESIAN_POINT ( 'NONE',  ( 70.87837837837835764, 13.70805908423323949, 10.00000000000000000 ) ) ;
#33423 = APPLICATION_CONTEXT ( 'automotive_design' ) ;
#33425 = LINE ( 'NONE', #54856, #52165 ) ;
#33426 = ORIENTED_EDGE ( 'NONE', *, *, #38092, .T. ) ;
#33427 = CARTESIAN_POINT ( 'NONE',  ( -128.6929263765337907, 10.01517768586948698, -1.839758294383808571E-15 ) ) ;
#33428 = CARTESIAN_POINT ( 'NONE',  ( -139.0450000000000159, 7.632228543268600340, 2.479861379858949277 ) ) ;
#33429 = ADVANCED_FACE ( 'NONE', ( #69504 ), #33269, .T. ) ;
#33430 = EDGE_CURVE ( 'NONE', #5489, #59091, #18020, .T. ) ;
#33431 = CARTESIAN_POINT ( 'NONE',  ( 10.00000000000001954, 50.00000000000000000, 46.00000000000000000 ) ) ;
#33432 = ORIENTED_EDGE ( 'NONE', *, *, #32554, .F. ) ;
#33433 = ORIENTED_EDGE ( 'NONE', *, *, #58464, .T. ) ;
#33434 = DIRECTION ( 'NONE',  ( 0.000000000000000000, 0.000000000000000000, -1.000000000000000000 ) ) ;
#33435 = FACE_OUTER_BOUND ( 'NONE', #49646, .T. ) ;
#33436 = EDGE_CURVE ( 'NONE', #65805, #59038, #56964, .T. ) ;
#33437 =( GEOMETRIC_REPRESENTATION_CONTEXT ( 3 ) GLOBAL_UNCERTAINTY_ASSIGNED_CONTEXT ( ( #15034 ) ) GLOBAL_UNIT_ASSIGNED_CONTEXT ( ( #28009, #23134, #50553 ) ) REPRESENTATION_CONTEXT ( 'NONE', 'WORKASPACE' ) );
#33438 = DIRECTION ( 'NONE',  ( 0.000000000000000000, -1.000000000000000000, 0.000000000000000000 ) ) ;
#33439 = DIRECTION ( 'NONE',  ( 0.000000000000000000, 0.000000000000000000, -1.000000000000000000 ) ) ;
#33440 = CIRCLE ( 'NONE', #25590, 0.5000000000000004441 ) ;
#33441 = SPHERICAL_SURFACE ( 'NONE', #437, 1.000000000000000000 ) ;
#33442 = VECTOR ( 'NONE', #17915, 1000.000000000000000 ) ;
#33443 = DIRECTION ( 'NONE',  ( -0.000000000000000000, -0.000000000000000000, -1.000000000000000000 ) ) ;
#33444 = ORIENTED_EDGE ( 'NONE', *, *, #45998, .T. ) ;
#33445 = CARTESIAN_POINT ( 'NONE',  ( -142.1049999999999613, -6.826472737025113702, 4.959722759717902107 ) ) ;
#33446 = ORIENTED_EDGE ( 'NONE', *, *, #66493, .F. ) ;
#33447 = ORIENTED_EDGE ( 'NONE', *, *, #37640, .T. ) ;
#33448 = PLANE ( 'NONE',  #52639 ) ;
#33449 = CARTESIAN_POINT ( 'NONE',  ( 0.000000000000000000, 36.75000000000000000, 3.750000000000000000 ) ) ;
#33450 = EDGE_LOOP ( 'NONE', ( #33272, #772, #5165, #32945 ) ) ;
#33451 = EDGE_CURVE ( 'NONE', #18424, #56002, #1126, .T. ) ;
#33452 = MECHANICAL_DESIGN_GEOMETRIC_PRESENTATION_REPRESENTATION (  '', ( #15511 ), #1941 ) ;
#33453 = CARTESIAN_POINT ( 'NONE',  ( -57.58629378005873889, -7.761720733523186588, -0.7755720678490058972 ) ) ;
#33454 = DIRECTION ( 'NONE',  ( 1.000000000000000000, 0.000000000000000000, 0.000000000000000000 ) ) ;
#33455 = CARTESIAN_POINT ( 'NONE',  ( -8.102448949553181734, 127.8949999999999534, -5.886773742842749790 ) ) ;
#33456 =( NAMED_UNIT ( * ) PLANE_ANGLE_UNIT ( ) SI_UNIT ( $, .RADIAN. ) );
#33457 =( BOUNDED_CURVE ( )  B_SPLINE_CURVE ( 2, ( #9120, #42220, #15453, #36918, #8430, #30537, #53069, #22425, #32282, #4862, #58329 ),
 .UNSPECIFIED., .F., .F. ) 
 B_SPLINE_CURVE_WITH_KNOTS ( ( 3, 2, 2, 2, 2, 3 ),
 ( 0.09782608695651952291, 0.09999999999999774347, 0.1021739130434759502, 0.1043478260869541568, 0.1065217391304323635, 0.1086956521739105841 ),
 .UNSPECIFIED. ) 
 CURVE ( )  GEOMETRIC_REPRESENTATION_ITEM ( )  RATIONAL_B_SPLINE_CURVE ( ( 1.000000000000049960, 0.9510565162951035711, 1.000000000000000000, 0.9510565162951535312, 1.000000000000000000, 0.9510565162951535312, 1.000000000000000000, 0.9510565162951535312, 1.000000000000000000, 0.9510565162952088203, 0.9999999999999447109 ) ) 
 REPRESENTATION_ITEM ( '' )  );
#33458 = ORIENTED_EDGE ( 'NONE', *, *, #69336, .T. ) ;
#33459 = CARTESIAN_POINT ( 'NONE',  ( 8.046771365092977746, 72.00000000000001421, 6.349999999999997868 ) ) ;
#33460 = CARTESIAN_POINT ( 'NONE',  ( 3.094860106618431583, 127.2049999999999841, 9.525000000000000355 ) ) ;
#33461 = CARTESIAN_POINT ( 'NONE',  ( -53.60499999999998266, 6.826472737025113702, -4.959722759717902107 ) ) ;
#33462 = EDGE_CURVE ( 'NONE', #29481, #21095, #32221, .T. ) ;
#33463 = CARTESIAN_POINT ( 'NONE',  ( 41.84210526315787604, 107.2928455055531600, -4.000000000000000888 ) ) ;
#33464 = ORIENTED_EDGE ( 'NONE', *, *, #56199, .F. ) ;
#33465 = CARTESIAN_POINT ( 'NONE',  ( 8.102448949553181734, 157.5050000000000239, 5.886773742842750679 ) ) ;
#33466 = CARTESIAN_POINT ( 'NONE',  ( 0.000000000000000000, 149.9999999999999716, 0.000000000000000000 ) ) ;
#33467 = UNCERTAINTY_MEASURE_WITH_UNIT (LENGTH_MEASURE( 1.000000000000000082E-05 ), #55590, 'distance_accuracy_value', 'NONE');
#33468 = AXIS2_PLACEMENT_3D ( 'NONE', #8259, #24076, #8601 ) ;
#33469 = CARTESIAN_POINT ( 'NONE',  ( -79.99999999999998579, 50.00000000000000000, -12.00000000000000000 ) ) ;
#33470 = AXIS2_PLACEMENT_3D ( 'NONE', #23387, #815, #43853 ) ;
#33471 = CARTESIAN_POINT ( 'NONE',  ( 4.250000000000001776, 22.24999999999998579, 4.000000000000000000 ) ) ;
#33472 = ORIENTED_EDGE ( 'NONE', *, *, #14902, .T. ) ;
#33473 = SURFACE_SIDE_STYLE ('',( #61241 ) ) ;
#33474 = ORIENTED_EDGE ( 'NONE', *, *, #21944, .F. ) ;
#33475 = CARTESIAN_POINT ( 'NONE',  ( -34.31731514509471026, -10.02774732068182750, -3.508434557029131540 ) ) ;
#33476 = CARTESIAN_POINT ( 'NONE',  ( -171.2049999999999841, -2.607480562269071545, -8.024999999999991473 ) ) ;
#33477 = EDGE_LOOP ( 'NONE', ( #52943, #63422, #10581, #1907, #48715 ) ) ;
#33478 = UNCERTAINTY_MEASURE_WITH_UNIT (LENGTH_MEASURE( 1.000000000000000082E-05 ), #68518, 'distance_accuracy_value', 'NONE');
#33479 = DIRECTION ( 'NONE',  ( -1.000000000000000000, 0.000000000000000000, -0.000000000000000000 ) ) ;
#33480 = CARTESIAN_POINT ( 'NONE',  ( 28.00000000000002132, 43.00000000000000000, 90.00000000000000000 ) ) ;
#33481 = ORIENTED_EDGE ( 'NONE', *, *, #53747, .F. ) ;
#33482 = CARTESIAN_POINT ( 'NONE',  ( -45.90821385068745286, 9.419345871351781696, -3.356457195962587736 ) ) ;
#33483 = DIRECTION ( 'NONE',  ( 0.000000000000000000, 0.000000000000000000, 1.000000000000000000 ) ) ;
#33484 = CARTESIAN_POINT ( 'NONE',  ( -86.90499999999998693, 2.607480562269068880, -8.024999999999993250 ) ) ;
#33485 = ORIENTED_EDGE ( 'NONE', *, *, #9062, .F. ) ;
#33486 = DIRECTION ( 'NONE',  ( 1.000000000000000000, 0.000000000000000000, 0.000000000000000000 ) ) ;
#33487 = DIRECTION ( 'NONE',  ( 1.000000000000000000, 0.000000000000000000, 0.000000000000000000 ) ) ;
#33488 = DIRECTION ( 'NONE',  ( -0.000000000000000000, -0.000000000000000000, -1.000000000000000000 ) ) ;
#33489 = CARTESIAN_POINT ( 'NONE',  ( -53.90707362346615383, -3.094860106618429807, 9.524999999999991473 ) ) ;
#33490 = ADVANCED_FACE ( 'NONE', ( #21306 ), #25888, .T. ) ;
#33491 = CARTESIAN_POINT ( 'NONE',  ( -74.50000000000000000, 7.768687147774688384, -6.500000000000000888 ) ) ;
#33492 = ORIENTED_EDGE ( 'NONE', *, *, #55595, .F. ) ;
#33493 = AXIS2_PLACEMENT_3D ( 'NONE', #21179, #32099, #63745 ) ;
#33494 = DIRECTION ( 'NONE',  ( -1.000000000000000000, 0.000000000000000000, 0.000000000000000000 ) ) ;
#33495 = COLOUR_RGB ( '', 0.66274510, 0.83137255, 0.94901961) ;
#33496 = CARTESIAN_POINT ( 'NONE',  ( 0.000000000000000000, 130.4449999999999648, -9.525000000000000355 ) ) ;
#33497 = CARTESIAN_POINT ( 'NONE',  ( -108.7449999999999903, 4.716976649647094177, 6.492361379858945902 ) ) ;
#33498 = DIRECTION ( 'NONE',  ( 0.000000000000000000, 0.000000000000000000, -1.000000000000000000 ) ) ;
#33499 = PRODUCT_RELATED_PRODUCT_CATEGORY ( 'part', '', ( #30428 ) ) ;
#33501 = CARTESIAN_POINT ( 'NONE',  ( -17.50807934363836083, 11.19244030607554663, -4.328528619389988563 ) ) ;
#33500 = CARTESIAN_POINT ( 'NONE',  ( -34.31243252642629926, -10.02680648607947589, -3.499999999999429345 ) ) ;
#33502 = ADVANCED_FACE ( 'NONE', ( #16076 ), #59989, .T. ) ;
#33503 = CARTESIAN_POINT ( 'NONE',  ( -148.7929263765337566, -3.094860106618429807, 9.524999999999991473 ) ) ;
#33504 = EDGE_CURVE ( 'NONE', #40178, #52535, #14666, .T. ) ;
#33505 = PRESENTATION_STYLE_ASSIGNMENT (( #50057 ) ) ;
#33506 = CARTESIAN_POINT ( 'NONE',  ( -179.3950000000000102, -6.826472737025115478, -4.959722759717899443 ) ) ;
#33507 = STYLED_ITEM ( 'NONE', ( #43754 ), #67661 ) ;
#33508 = EDGE_CURVE ( 'NONE', #38783, #68819, #34891, .T. ) ;
#33509 = ADVANCED_FACE ( 'NONE', ( #43858 ), #64141, .F. ) ;
#33510 = DIRECTION ( 'NONE',  ( 0.000000000000000000, 1.000000000000000000, 0.000000000000000000 ) ) ;
#33511 = LINE ( 'NONE', #6769, #25911 ) ;
#33512 = ORIENTED_EDGE ( 'NONE', *, *, #15128, .F. ) ;
#33513 = CYLINDRICAL_SURFACE ( 'NONE', #35814, 0.2500000000000002220 ) ;
#33514 = FACE_OUTER_BOUND ( 'NONE', #46224, .T. ) ;
#33515 = ORIENTED_EDGE ( 'NONE', *, *, #35673, .T. ) ;
#33516 = CARTESIAN_POINT ( 'NONE',  ( -65.99292637653377369, 8.102448949553171076, -5.886773742842744461 ) ) ;
#33517 = CARTESIAN_POINT ( 'NONE',  ( -48.50000000000000000, 14.49137674618942384, -7.500000000000000000 ) ) ;
#33518 = DIRECTION ( 'NONE',  ( 0.000000000000000000, 0.000000000000000000, 1.000000000000000000 ) ) ;
#33519 = ADVANCED_FACE ( 'NONE', ( #50486 ), #39965, .T. ) ;
#33520 = AXIS2_PLACEMENT_3D ( 'NONE', #53492, #64735, #48600 ) ;
#33521 = PRESENTATION_STYLE_ASSIGNMENT (( #16683 ) ) ;
#33522 = PRESENTATION_STYLE_ASSIGNMENT (( #44131 ) ) ;
#33523 = CARTESIAN_POINT ( 'NONE',  ( -20.29261984882471381, 1.607755262496700421, 6.349999999999988098 ) ) ;
#33524 = EDGE_CURVE ( 'NONE', #69107, #29745, #30430, .T. ) ;
#33525 = FACE_BOUND ( 'NONE', #64871, .T. ) ;
#33526 = AXIS2_PLACEMENT_3D ( 'NONE', #57626, #25588, #62876 ) ;
#33527 = ORIENTED_EDGE ( 'NONE', *, *, #50524, .F. ) ;
#33528 = CARTESIAN_POINT ( 'NONE',  ( -169.2549999999999955, -4.716976649647092401, 6.492361379858946790 ) ) ;
#33529 = ORIENTED_EDGE ( 'NONE', *, *, #3257, .F. ) ;
#33530 = FILL_AREA_STYLE_COLOUR ( '', #59477 ) ;
#33531 =( NAMED_UNIT ( * ) PLANE_ANGLE_UNIT ( ) SI_UNIT ( $, .RADIAN. ) );
#33532 = AXIS2_PLACEMENT_3D ( 'NONE', #61619, #62668, #30298 ) ;
#33533 = CARTESIAN_POINT ( 'NONE',  ( -4.716976649647097730, 154.3570736234661922, -6.492361379858953896 ) ) ;
#33534 = ORIENTED_EDGE ( 'NONE', *, *, #17449, .F. ) ;
#33535 = SURFACE_STYLE_FILL_AREA ( #17045 ) ;
#33536 = CARTESIAN_POINT ( 'NONE',  ( -83.30499999999999261, 8.437984349512086979, -1.550032578732815448E-15 ) ) ;
#33537 =( BOUNDED_CURVE ( )  B_SPLINE_CURVE ( 2, ( #12646, #54522, #27425 ),
 .UNSPECIFIED., .F., .T. ) 
 B_SPLINE_CURVE_WITH_KNOTS ( ( 3, 3 ),
 ( 0.05767644037838164095, 0.05882352941176476058 ),
 .UNSPECIFIED. ) 
 CURVE ( )  GEOMETRIC_REPRESENTATION_ITEM ( )  RATIONAL_B_SPLINE_CURVE ( ( 0.9846338866368906650, 0.9904557693197236778, 1.000000000000000444 ) ) 
 REPRESENTATION_ITEM ( '' )  );
#33538 = UNCERTAINTY_MEASURE_WITH_UNIT (LENGTH_MEASURE( 1.000000000000000082E-05 ), #49740, 'distance_accuracy_value', 'NONE');
#33539 = DIRECTION ( 'NONE',  ( -1.000000000000000000, 1.387778780781444571E-14, 0.000000000000000000 ) ) ;
#33540 = AXIS2_PLACEMENT_3D ( 'NONE', #22704, #6493, #17108 ) ;
#33541 = COLOUR_RGB ( '', 0.72549020, 0.75294118, 0.79215686) ;
#33542 = DIRECTION ( 'NONE',  ( 1.000000000000000000, 0.000000000000000000, 0.000000000000000000 ) ) ;
#33543 = CARTESIAN_POINT ( 'NONE',  ( -169.4929263765338305, -8.102448949553174629, 5.886773742842742685 ) ) ;
#33544 = CARTESIAN_POINT ( 'NONE',  ( -114.1429263765338078, 5.598654528085800663, -7.705886871421367523 ) ) ;
#33545 = CYLINDRICAL_SURFACE ( 'NONE', #49711, 0.9999999999999974465 ) ;
#33546 = ORIENTED_EDGE ( 'NONE', *, *, #22185, .T. ) ;
#33547 = MECHANICAL_DESIGN_GEOMETRIC_PRESENTATION_REPRESENTATION (  '', ( #11092 ), #38119 ) ;
#33548 = CARTESIAN_POINT ( 'NONE',  ( -83.49999999999998579, -3.499999999999999556, 0.000000000000000000 ) ) ;
#33549 = DIRECTION ( 'NONE',  ( 0.000000000000000000, -1.000000000000000000, 0.000000000000000000 ) ) ;
#33550 = EDGE_CURVE ( 'NONE', #68105, #12632, #44880, .T. ) ;
#33551 = CARTESIAN_POINT ( 'NONE',  ( -61.19499999999997897, 8.437984349512085203, -1.550032578732815448E-15 ) ) ;
#33552 = EDGE_LOOP ( 'NONE', ( #5654, #52929, #21519, #67489 ) ) ;
#33553 =( NAMED_UNIT ( * ) SI_UNIT ( $, .STERADIAN. ) SOLID_ANGLE_UNIT ( ) );
#33554 = COLOUR_RGB ( '', 0.66274510, 0.83137255, 0.94901961) ;
#33555 = CARTESIAN_POINT ( 'NONE',  ( -49.04292637653379217, -9.058813317711329915, -2.943386871421370898 ) ) ;
#33556 = CARTESIAN_POINT ( 'NONE',  ( -45.00000000000000000, 9.675838479951684334, -6.195399861057250490 ) ) ;
#33557 = VERTEX_POINT ( 'NONE', #14581 ) ;
#33558 = CARTESIAN_POINT ( 'NONE',  ( -69.49999999999997158, 50.00000000000000000, 6.499999999999999112 ) ) ;
#33559 = ORIENTED_EDGE ( 'NONE', *, *, #36089, .T. ) ;
#33560 = DIRECTION ( 'NONE',  ( 0.000000000000000000, -1.000000000000000000, 0.000000000000000000 ) ) ;
#33561 = CARTESIAN_POINT ( 'NONE',  ( -111.3549999999999898, -4.716976649647093289, -6.492361379858945902 ) ) ;
#33562 = ORIENTED_EDGE ( 'NONE', *, *, #25271, .F. ) ;
#33563 = CARTESIAN_POINT ( 'NONE',  ( 21.50000000000000711, 22.24999999999998224, -3.750000000000000000 ) ) ;
#33564 =( LENGTH_UNIT ( ) NAMED_UNIT ( * ) SI_UNIT ( .MILLI., .METRE. ) );
#33565 = DIRECTION ( 'NONE',  ( 0.000000000000000000, 0.000000000000000000, 1.000000000000000000 ) ) ;
#33566 =( NAMED_UNIT ( * ) PLANE_ANGLE_UNIT ( ) SI_UNIT ( $, .RADIAN. ) );
#33567 = CARTESIAN_POINT ( 'NONE',  ( -150.3570736234661638, 5.598654528085804216, 7.705886871421366635 ) ) ;
#33568 = CARTESIAN_POINT ( 'NONE',  ( 2.000000000000023093, 50.00000000000000000, 65.00000000000000000 ) ) ;
#33569 = CARTESIAN_POINT ( 'NONE',  ( 8.102448949553179958, 129.3949999999999818, 5.886773742842750679 ) ) ;
#33570 = CARTESIAN_POINT ( 'NONE',  ( -87.50707362346614104, 8.102448949553176405, 5.886773742842740909 ) ) ;
#33571 = FILL_AREA_STYLE_COLOUR ( '', #67363 ) ;
#33572 = EDGE_LOOP ( 'NONE', ( #24290, #38688, #22108, #69196 ) ) ;
#33573 =( NAMED_UNIT ( * ) SI_UNIT ( $, .STERADIAN. ) SOLID_ANGLE_UNIT ( ) );
#33574 =( LENGTH_UNIT ( ) NAMED_UNIT ( * ) SI_UNIT ( .MILLI., .METRE. ) );
#33575 = AXIS2_PLACEMENT_3D ( 'NONE', #22329, #63840, #15686 ) ;
#33576 = PRESENTATION_STYLE_ASSIGNMENT (( #60990 ) ) ;
#33577 = CARTESIAN_POINT ( 'NONE',  ( -131.1550000000000011, 7.632228543268600340, 2.479861379858949277 ) ) ;
#33578 = FACE_OUTER_BOUND ( 'NONE', #45182, .T. ) ;
#33579 = CARTESIAN_POINT ( 'NONE',  ( 15.98999599679679839, 118.4999999999999716, 7.500000000000000000 ) ) ;
#33580 = FACE_OUTER_BOUND ( 'NONE', #53799, .T. ) ;
#33581 = CARTESIAN_POINT ( 'NONE',  ( -149.6949999999999648, -8.437984349512085203, 5.166775262442717831E-16 ) ) ;
#33582 = CIRCLE ( 'NONE', #42620, 13.49999999999999822 ) ;
#33583 = CARTESIAN_POINT ( 'NONE',  ( -126.1450000000000102, -4.716976649647092401, 6.492361379858946790 ) ) ;
#33584 = EDGE_LOOP ( 'NONE', ( #6467, #25351, #8454 ) ) ;
#33585 = PRESENTATION_STYLE_ASSIGNMENT (( #65595 ) ) ;
#33586 = TOROIDAL_SURFACE ( 'NONE', #50467, 17.50000000000000000, 0.5000000000000000000 ) ;
#33587 = SURFACE_SIDE_STYLE ('',( #18108 ) ) ;
#33588 = ADVANCED_FACE ( 'NONE', ( #51514 ), #47328, .F. ) ;
#33589 = DIRECTION ( 'NONE',  ( -1.000000000000000000, -0.000000000000000000, -0.000000000000000000 ) ) ;
#33590 = CARTESIAN_POINT ( 'NONE',  ( -181.3429263765338249, -9.058813317711329915, 2.943386871421371787 ) ) ;
#33591 = FILL_AREA_STYLE_COLOUR ( '', #34907 ) ;
#33592 = CARTESIAN_POINT ( 'NONE',  ( -60.59499999999997755, 2.607480562269073321, 8.024999999999991473 ) ) ;
#33593 = EDGE_CURVE ( 'NONE', #20287, #67877, #63112, .T. ) ;
#33594 = DIRECTION ( 'NONE',  ( 1.000000000000000000, 0.000000000000000000, 0.000000000000000000 ) ) ;
#33595 = LINE ( 'NONE', #44552, #45581 ) ;
#33596 = TOROIDAL_SURFACE ( 'NONE', #37062, 29.50000000000000000, 0.5000000000000000000 ) ;
#33597 = CARTESIAN_POINT ( 'NONE',  ( 71.49999999999998579, 64.07124727947029896, 7.000000000000000000 ) ) ;
#33598 = CARTESIAN_POINT ( 'NONE',  ( -99.74292637653380211, -5.598654528085803328, -7.705886871421366635 ) ) ;
#33599 = APPLICATION_PROTOCOL_DEFINITION ( 'draft international standard', 'automotive_design', 1998, #65785 ) ;
#33600 = STYLED_ITEM ( 'NONE', ( #34782 ), #19852 ) ;
#33601 = DIRECTION ( 'NONE',  ( -1.000000000000000000, -0.000000000000000000, -0.000000000000000000 ) ) ;
#33602 = FILL_AREA_STYLE ('',( #60330 ) ) ;
#33603 = CARTESIAN_POINT ( 'NONE',  ( -40.99999999999998579, 107.7459666924148394, 3.000000000000000444 ) ) ;
#33604 = AXIS2_PLACEMENT_3D ( 'NONE', #43577, #16821, #44950 ) ;
#33605 = ADVANCED_FACE ( 'NONE', ( #57490 ), #20189, .F. ) ;
#33606 = ORIENTED_EDGE ( 'NONE', *, *, #33823, .F. ) ;
#33607 = DIRECTION ( 'NONE',  ( 0.000000000000000000, 0.000000000000000000, -1.000000000000000000 ) ) ;
#33608 = LINE ( 'NONE', #29001, #52006 ) ;
#33609 = ORIENTED_EDGE ( 'NONE', *, *, #30467, .F. ) ;
#33610 = CARTESIAN_POINT ( 'NONE',  ( 0.000000000000000000, 2.500000000000000000, 0.000000000000000000 ) ) ;
#33611 = CARTESIAN_POINT ( 'NONE',  ( -7.632228543268607446, 124.6570736234661609, -2.479861379858953718 ) ) ;
#33612 = AXIS2_PLACEMENT_3D ( 'NONE', #14217, #35331, #35680 ) ;
#33613 = CARTESIAN_POINT ( 'NONE',  ( -23.71231517720798010, 117.4999999999999716, -9.500000000000000000 ) ) ;
#33614 = CARTESIAN_POINT ( 'NONE',  ( 6.826472737025119919, 138.0070736234661410, 4.959722759717908325 ) ) ;
#33615 = CARTESIAN_POINT ( 'NONE',  ( 68.00000000000000000, 2.776762340297168394E-15, 12.00000000000000000 ) ) ;
#33617 = EDGE_LOOP ( 'NONE', ( #5114, #64421, #32826, #37947 ) ) ;
#33616 = CIRCLE ( 'NONE', #42656, 2.000000000000001776 ) ;
#33618 = ORIENTED_EDGE ( 'NONE', *, *, #4, .F. ) ;
#33619 = CARTESIAN_POINT ( 'NONE',  ( -60.00000000000000000, -2.024042244987997205E-14, 12.00000000000000000 ) ) ;
#33620 = EDGE_CURVE ( 'NONE', #23940, #50938, #8961, .T. ) ;
#33621 = CARTESIAN_POINT ( 'NONE',  ( -93.50707362346618368, 8.102448949553176405, 5.886773742842740909 ) ) ;
#33622 = AXIS2_PLACEMENT_3D ( 'NONE', #25194, #63857, #20255 ) ;
#33623 = CIRCLE ( 'NONE', #27968, 0.2500000000000002220 ) ;
#33624 = DIRECTION ( 'NONE',  ( 0.000000000000000000, -1.000000000000000000, 0.000000000000000000 ) ) ;
#33625 = ADVANCED_FACE ( 'NONE', ( #26159 ), #36775, .F. ) ;
#33626 = CARTESIAN_POINT ( 'NONE',  ( -91.19499999999999318, 8.437984349512085203, -1.550032578732815448E-15 ) ) ;
#33628 = EDGE_LOOP ( 'NONE', ( #26460, #16471, #40494, #29878 ) ) ;
#33627 = VECTOR ( 'NONE', #55318, 1000.000000000000000 ) ;
#33629 = CIRCLE ( 'NONE', #5538, 14.49999999999999822 ) ;
#33630 = DIRECTION ( 'NONE',  ( 1.000000000000000000, 0.000000000000000000, 0.000000000000000000 ) ) ;
#33631 = SURFACE_SIDE_STYLE ('',( #60695 ) ) ;
#33632 = MECHANICAL_DESIGN_GEOMETRIC_PRESENTATION_REPRESENTATION (  '', ( #49422 ), #42677 ) ;
#33633 = ORIENTED_EDGE ( 'NONE', *, *, #4612, .T. ) ;
#33634 = LINE ( 'NONE', #27289, #53858 ) ;
#33635 = CARTESIAN_POINT ( 'NONE',  ( -75.48275862068965125, 63.99167409976912069, -41.30495168499704306 ) ) ;
#33636 = AXIS2_PLACEMENT_3D ( 'NONE', #47946, #69345, #29529 ) ;
#33637 = CARTESIAN_POINT ( 'NONE',  ( 6.898093598910793212, 2.361802048420730049, -6.052151411320861207 ) ) ;
#33638 = ORIENTED_EDGE ( 'NONE', *, *, #54702, .F. ) ;
#33639 = ORIENTED_EDGE ( 'NONE', *, *, #6321, .T. ) ;
#33640 = DIRECTION ( 'NONE',  ( -1.000000000000000000, 0.000000000000000000, 0.000000000000000000 ) ) ;
#33641 = CARTESIAN_POINT ( 'NONE',  ( -195.0000000000000000, 0.000000000000000000, 0.000000000000000000 ) ) ;
#33643 = STYLED_ITEM ( 'NONE', ( #55649 ), #15173 ) ;
#33642 =( LENGTH_UNIT ( ) NAMED_UNIT ( * ) SI_UNIT ( .MILLI., .METRE. ) );
#33644 = CARTESIAN_POINT ( 'NONE',  ( -177.8070736234661808, 10.01517768586948698, -1.839758294383808571E-15 ) ) ;
#33645 = CARTESIAN_POINT ( 'NONE',  ( -75.00000000000000000, 35.50862325381056905, 10.00000000000000000 ) ) ;
#33646 = TOROIDAL_SURFACE ( 'NONE', #21286, 1.000000000000000000, 0.5000000000000000000 ) ;
#33647 = DIRECTION ( 'NONE',  ( -0.000000000000000000, 1.000000000000000000, -0.000000000000000000 ) ) ;
#33648 = LINE ( 'NONE', #59680, #7046 ) ;
#33649 = CARTESIAN_POINT ( 'NONE',  ( -13.23915246117191025, 52.65078610323165265, -6.947530358905292580 ) ) ;
#33650 = ORIENTED_EDGE ( 'NONE', *, *, #35571, .F. ) ;
#33651 = AXIS2_PLACEMENT_3D ( 'NONE', #47759, #42455, #22338 ) ;
#33652 = CARTESIAN_POINT ( 'NONE',  ( 15.00000000000000000, 8.000000000000000000, 3.500000000000003997 ) ) ;
#33653 = SPHERICAL_SURFACE ( 'NONE', #42522, 0.5000000000000000000 ) ;
#33654 = DIRECTION ( 'NONE',  ( 1.000000000000000000, 0.000000000000000000, 0.000000000000000000 ) ) ;
#33655 = ORIENTED_EDGE ( 'NONE', *, *, #13731, .F. ) ;
#33656 = CARTESIAN_POINT ( 'NONE',  ( -163.2549999999999955, -4.716976649647092401, 6.492361379858946790 ) ) ;
#33657 = DIRECTION ( 'NONE',  ( -1.000000000000000000, -0.000000000000000000, -0.000000000000000000 ) ) ;
#33658 = CARTESIAN_POINT ( 'NONE',  ( -183.8592518627806953, -8.440169527594953536, -1.989286698146640164 ) ) ;
#33659 = EDGE_CURVE ( 'NONE', #66900, #5467, #19849, .T. ) ;
#33660 = CARTESIAN_POINT ( 'NONE',  ( -169.3449999999999989, 7.632228543268599452, -2.479861379858951942 ) ) ;
#33661 = CARTESIAN_POINT ( 'NONE',  ( -155.0949999999999704, -2.607480562269071545, -8.024999999999991473 ) ) ;
#33662 = CIRCLE ( 'NONE', #3284, 0.5000000000000004441 ) ;
#33663 = ORIENTED_EDGE ( 'NONE', *, *, #63536, .T. ) ;
#33664 = PRESENTATION_STYLE_ASSIGNMENT (( #22779 ) ) ;
#33665 = CARTESIAN_POINT ( 'NONE',  ( 44.88867800444037215, 10.61949827965496240, 3.673511479703632787 ) ) ;
#33666 = CARTESIAN_POINT ( 'NONE',  ( -6.826472737025120807, 150.9929263765338305, 4.959722759717906548 ) ) ;
#33667 = CARTESIAN_POINT ( 'NONE',  ( -70.10499999999998977, -6.826472737025115478, 4.959722759717900331 ) ) ;
#33668 = CARTESIAN_POINT ( 'NONE',  ( -36.73960380223706323, -12.13027782366804708, 3.018653417519900906 ) ) ;
#33669 = CARTESIAN_POINT ( 'NONE',  ( 39.74999999999999289, 18.99999999999997868, -3.750000000000000000 ) ) ;
#33670 = ADVANCED_FACE ( 'NONE', ( #54622 ), #21262, .T. ) ;
#33671 = CARTESIAN_POINT ( 'NONE',  ( -66.74499999999999034, 4.716976649647094177, 6.492361379858945902 ) ) ;
#33672 = CARTESIAN_POINT ( 'NONE',  ( 0.000000000000000000, 146.5549999999999784, -9.525000000000000355 ) ) ;
#33673 = CARTESIAN_POINT ( 'NONE',  ( -15.98999599679679839, 146.9999999999999716, 10.00000000000000000 ) ) ;
#33674 = EDGE_CURVE ( 'NONE', #11473, #26491, #20902, .T. ) ;
#33675 = CARTESIAN_POINT ( 'NONE',  ( 2.525713312988952630, 154.2507441751838542, 8.932758862731519756 ) ) ;
#33676 = VECTOR ( 'NONE', #21499, 1000.000000000000000 ) ;
#33677 = CYLINDRICAL_SURFACE ( 'NONE', #34855, 1.000000000000000888 ) ;
#33678 = ORIENTED_EDGE ( 'NONE', *, *, #6420, .F. ) ;
#33679 = EDGE_CURVE ( 'NONE', #57515, #17308, #23531, .T. ) ;
#33680 = COLOUR_RGB ( '', 0.09019608, 0.27058824, 0.51372549) ;
#33681 = CARTESIAN_POINT ( 'NONE',  ( 24.00000000000000000, 1.000000000000000000, 3.000000000000000000 ) ) ;
#33682 = DIRECTION ( 'NONE',  ( 0.000000000000000000, 0.000000000000000000, -1.000000000000000000 ) ) ;
#33683 = EDGE_CURVE ( 'NONE', #20924, #34097, #61672, .T. ) ;
#33684 = FACE_OUTER_BOUND ( 'NONE', #17916, .T. ) ;
#33685 = CARTESIAN_POINT ( 'NONE',  ( 34.99999999999999289, 99.99999999999998579, 7.000000000000000000 ) ) ;
#33686 = CARTESIAN_POINT ( 'NONE',  ( 22.99999999999995381, 0.000000000000000000, 32.00402776293825724 ) ) ;
#33687 = ORIENTED_EDGE ( 'NONE', *, *, #49595, .T. ) ;
#33688 = STYLED_ITEM ( 'NONE', ( #1341 ), #15523 ) ;
#33689 = EDGE_LOOP ( 'NONE', ( #7521, #31365, #62344, #18136 ) ) ;
#33690 = AXIS2_PLACEMENT_3D ( 'NONE', #28464, #2385, #11623 ) ;
#33691 = FILL_AREA_STYLE_COLOUR ( '', #38457 ) ;
#33692 = CARTESIAN_POINT ( 'NONE',  ( 0.9126302363882010660, 2.499999999999998224, 9.000000000000003553 ) ) ;
#33693 = DIRECTION ( 'NONE',  ( -0.000000000000000000, 1.000000000000000000, 1.224646799147353207E-16 ) ) ;
#33694 = VERTEX_POINT ( 'NONE', #43097 ) ;
#33695 = CARTESIAN_POINT ( 'NONE',  ( -112.4049999999999869, -2.607480562269069768, 8.024999999999991473 ) ) ;
#33696 = ORIENTED_EDGE ( 'NONE', *, *, #68101, .T. ) ;
#33697 = PRESENTATION_STYLE_ASSIGNMENT (( #18219 ) ) ;
#33698 = EDGE_LOOP ( 'NONE', ( #57868, #16270, #28950, #2330 ) ) ;
#33699 = SURFACE_STYLE_FILL_AREA ( #65717 ) ;
#33700 = CARTESIAN_POINT ( 'NONE',  ( -11.99999999999999822, -6.499999999999999112, 21.00000000000000000 ) ) ;
#33701 = EDGE_LOOP ( 'NONE', ( #10226, #59543 ) ) ;
#33702 = DIRECTION ( 'NONE',  ( 0.000000000000000000, 0.000000000000000000, 1.000000000000000000 ) ) ;
#33703 = PRESENTATION_STYLE_ASSIGNMENT (( #37666 ) ) ;
#33704 = ORIENTED_EDGE ( 'NONE', *, *, #29035, .T. ) ;
#33705 = ORIENTED_EDGE ( 'NONE', *, *, #66048, .T. ) ;
#33706 = CARTESIAN_POINT ( 'NONE',  ( -74.08841914795480932, 9.415459729490459395, -6.077763577362910397 ) ) ;
#33707 = EDGE_LOOP ( 'NONE', ( #18954, #6347, #4003, #39567 ) ) ;
#33708 = CARTESIAN_POINT ( 'NONE',  ( -4.716976649647097730, 138.2429263765338305, -6.492361379858953896 ) ) ;
#33709 = DIRECTION ( 'NONE',  ( 0.000000000000000000, 0.000000000000000000, -1.000000000000000000 ) ) ;
#33710 = DIRECTION ( 'NONE',  ( 0.000000000000000000, 0.000000000000000000, -1.000000000000000000 ) ) ;
#33711 = CARTESIAN_POINT ( 'NONE',  ( 5.000000000000000000, 6.123233995736766282E-16, 0.2500000000000011102 ) ) ;
#33712 = ORIENTED_EDGE ( 'NONE', *, *, #18916, .T. ) ;
#33713 = AXIS2_PLACEMENT_3D ( 'NONE', #66665, #53751, #18481 ) ;
#33714 = CARTESIAN_POINT ( 'NONE',  ( -11.00000000000000000, 8.000000000000000000, 4.000000000000000000 ) ) ;
#33715 = ORIENTED_EDGE ( 'NONE', *, *, #25038, .F. ) ;
#33716 = CARTESIAN_POINT ( 'NONE',  ( 62.24999999999998579, 33.74999999999999289, 4.000000000000000000 ) ) ;
#33717 = CARTESIAN_POINT ( 'NONE',  ( -60.00000000000000000, -2.024042244987997205E-14, -6.500000000000000000 ) ) ;
#33718 = SURFACE_STYLE_FILL_AREA ( #39051 ) ;
#33719 = CARTESIAN_POINT ( 'NONE',  ( -131.4549999999999841, 7.632228543268599452, -2.479861379858951942 ) ) ;
#33720 = CARTESIAN_POINT ( 'NONE',  ( 40.99999999999997868, 9.999999999999978684, 3.000000000000000000 ) ) ;
#33721 = AXIS2_PLACEMENT_3D ( 'NONE', #9841, #4529, #47515 ) ;
#33722 = FILL_AREA_STYLE ('',( #55879 ) ) ;
#33723 = ORIENTED_EDGE ( 'NONE', *, *, #66135, .F. ) ;
#33724 = CARTESIAN_POINT ( 'NONE',  ( -4.716976649647098618, 116.2570736234661553, 6.492361379858953008 ) ) ;
#33725 = CARTESIAN_POINT ( 'NONE',  ( 5.196152422706629359, 9.000000000000008882, 1.392304845413260272 ) ) ;
#33726 = CARTESIAN_POINT ( 'NONE',  ( -24.75000000000000355, 36.75000000000000000, 4.000000000000000000 ) ) ;
#33727 = ORIENTED_EDGE ( 'NONE', *, *, #57431, .F. ) ;
#33728 = ORIENTED_EDGE ( 'NONE', *, *, #63830, .F. ) ;
#33729 = CARTESIAN_POINT ( 'NONE',  ( 9.250000000000003553, 27.99999999999998934, 4.000000000000000000 ) ) ;
#33730 = CARTESIAN_POINT ( 'NONE',  ( -109.3429263765338106, -9.058813317711329915, 2.943386871421371787 ) ) ;
#33731 = ORIENTED_EDGE ( 'NONE', *, *, #51324, .T. ) ;
#33732 = DIRECTION ( 'NONE',  ( 1.000000000000000000, 0.000000000000000000, 0.000000000000000000 ) ) ;
#33733 = DIRECTION ( 'NONE',  ( 0.000000000000000000, 0.000000000000000000, -1.000000000000000000 ) ) ;
#33734 = SURFACE_STYLE_FILL_AREA ( #12267 ) ;
#33735 = AXIS2_PLACEMENT_3D ( 'NONE', #24255, #20006, #14063 ) ;
#33736 = EDGE_CURVE ( 'NONE', #6686, #29473, #32509, .T. ) ;
#33737 = AXIS2_PLACEMENT_3D ( 'NONE', #66460, #27756, #49260 ) ;
#33738 = PRESENTATION_STYLE_ASSIGNMENT (( #50973 ) ) ;
#33739 = FILL_AREA_STYLE ('',( #28442 ) ) ;
#33740 = CIRCLE ( 'NONE', #36030, 23.00000000000000000 ) ;
#33742 = EDGE_CURVE ( 'NONE', #63218, #62320, #29139, .T. ) ;
#33741 = VERTEX_POINT ( 'NONE', #5059 ) ;
#33743 = COLOUR_RGB ( '', 0.31764706, 0.68627451, 0.89019608) ;
#33744 = CARTESIAN_POINT ( 'NONE',  ( 57.74999999999998579, 30.74999999999999289, 3.750000000000000000 ) ) ;
#33745 = EDGE_CURVE ( 'NONE', #17724, #6296, #54278, .T. ) ;
#33746 = SURFACE_STYLE_USAGE ( .BOTH. , #44366 ) ;
#33747 = CARTESIAN_POINT ( 'NONE',  ( -10.39230484541327293, 3.364658241569156409E-15, 1.392304845413260939 ) ) ;
#33749 = SURFACE_STYLE_USAGE ( .BOTH. , #66100 ) ;
#33748 = CIRCLE ( 'NONE', #51758, 0.2500000000000002220 ) ;
#33750 = DIRECTION ( 'NONE',  ( 0.000000000000000000, 0.000000000000000000, -1.000000000000000000 ) ) ;
#33751 = EDGE_CURVE ( 'NONE', #48904, #37089, #37042, .T. ) ;
#33752 = EDGE_CURVE ( 'NONE', #49909, #60879, #5537, .T. ) ;
#33753 = CARTESIAN_POINT ( 'NONE',  ( -95.84499999999998465, -7.632228543268599452, 2.479861379858951054 ) ) ;
#33754 = CARTESIAN_POINT ( 'NONE',  ( 5.598654528085805993, 156.2450000000000045, 7.705886871421374629 ) ) ;
#33755 = CARTESIAN_POINT ( 'NONE',  ( -80.24499999999997613, -4.716976649647093289, -6.492361379858945902 ) ) ;
#33756 = EDGE_CURVE ( 'NONE', #1567, #27344, #49363, .T. ) ;
#33757 = CARTESIAN_POINT ( 'NONE',  ( 0.000000000000000000, 110.4999999999999858, 0.000000000000000000 ) ) ;
#33758 = PRESENTATION_LAYER_ASSIGNMENT (  '', '', ( #48425 ) ) ;
#33759 = ADVANCED_FACE ( 'NONE', ( #37481 ), #11723, .T. ) ;
#33760 = LINE ( 'NONE', #34111, #50801 ) ;
#33761 = SURFACE_SIDE_STYLE ('',( #980 ) ) ;
#33762 = SURFACE_STYLE_FILL_AREA ( #28466 ) ;
#33764 = ORIENTED_EDGE ( 'NONE', *, *, #25404, .T. ) ;
#33763 = AXIS2_PLACEMENT_3D ( 'NONE', #36533, #2787, #39806 ) ;
#33765 = EDGE_CURVE ( 'NONE', #41120, #38684, #26868, .T. ) ;
#33766 = CARTESIAN_POINT ( 'NONE',  ( -119.9929263765338021, 8.102448949553171076, -5.886773742842744461 ) ) ;
#33767 =( NAMED_UNIT ( * ) PLANE_ANGLE_UNIT ( ) SI_UNIT ( $, .RADIAN. ) );
#33768 = CARTESIAN_POINT ( 'NONE',  ( -133.3449999999999989, 7.632228543268599452, -2.479861379858951942 ) ) ;
#33769 = DIRECTION ( 'NONE',  ( -0.000000000000000000, -1.000000000000000000, -0.000000000000000000 ) ) ;
#33770 = COLOUR_RGB ( '', 0.31764706, 0.68627451, 0.89019608) ;
#33771 =( NAMED_UNIT ( * ) SI_UNIT ( $, .STERADIAN. ) SOLID_ANGLE_UNIT ( ) );
#33772 = ORIENTED_EDGE ( 'NONE', *, *, #2305, .F. ) ;
#33773 = ORIENTED_EDGE ( 'NONE', *, *, #67119, .T. ) ;
#33774 = PRESENTATION_LAYER_ASSIGNMENT (  '', '', ( #48440 ) ) ;
#33775 = CARTESIAN_POINT ( 'NONE',  ( 30.75000000000001066, 16.24999999999997513, -3.750000000000000000 ) ) ;
#33776 = MECHANICAL_DESIGN_GEOMETRIC_PRESENTATION_REPRESENTATION (  '', ( #67473 ), #9096 ) ;
#33777 = PRESENTATION_STYLE_ASSIGNMENT (( #39102 ) ) ;
#33778 = AXIS2_PLACEMENT_3D ( 'NONE', #40643, #67703, #57129 ) ;
#33779 = PRESENTATION_STYLE_ASSIGNMENT (( #11638 ) ) ;
#33780 = EDGE_LOOP ( 'NONE', ( #29232, #47828, #56458, #28780, #9203 ) ) ;
#33781 = CARTESIAN_POINT ( 'NONE',  ( -139.4049999999999727, -2.607480562269069768, 8.024999999999991473 ) ) ;
#33782 = ORIENTED_EDGE ( 'NONE', *, *, #40301, .F. ) ;
#33783 = ORIENTED_EDGE ( 'NONE', *, *, #28980, .T. ) ;
#33784 = DIRECTION ( 'NONE',  ( -0.000000000000000000, -0.000000000000000000, -1.000000000000000000 ) ) ;
#33785 = DIRECTION ( 'NONE',  ( 0.000000000000000000, -0.000000000000000000, -1.000000000000000000 ) ) ;
#33786 = ORIENTED_EDGE ( 'NONE', *, *, #58702, .F. ) ;
#33787 = COLOUR_RGB ( '', 0.08235294, 0.09019608, 0.10196078) ;
#33788 = CARTESIAN_POINT ( 'NONE',  ( -55.66437634316022098, -8.712199461619613672, -1.102180370744095139 ) ) ;
#33789 = CARTESIAN_POINT ( 'NONE',  ( 22.00000000000002132, 43.00000000000000000, 29.68999999999999417 ) ) ;
#33790 = CARTESIAN_POINT ( 'NONE',  ( 5.598654528085805993, 129.2450000000000045, 7.705886871421374629 ) ) ;
#33791 = SURFACE_STYLE_USAGE ( .BOTH. , #54557 ) ;
#33792 = PRESENTATION_LAYER_ASSIGNMENT (  '', '', ( #66376 ) ) ;
#33793 = EDGE_CURVE ( 'NONE', #11461, #27455, #66205, .T. ) ;
#33794 = CARTESIAN_POINT ( 'NONE',  ( -62.30499999999997840, 8.437984349512086979, -1.550032578732815448E-15 ) ) ;
#33795 = ORIENTED_EDGE ( 'NONE', *, *, #37565, .T. ) ;
#33796 = DIRECTION ( 'NONE',  ( -1.000000000000000000, -0.000000000000000000, -0.000000000000000000 ) ) ;
#33797 = CARTESIAN_POINT ( 'NONE',  ( 10.01517768586949408, 130.8049999999999784, 1.839758294383810543E-15 ) ) ;
#33798 = CARTESIAN_POINT ( 'NONE',  ( -56.30499999999999972, 8.437984349512086979, -1.550032578732815448E-15 ) ) ;
#33799 = CARTESIAN_POINT ( 'NONE',  ( 41.39002736484397360, 107.1345546009599445, -3.500000000000000000 ) ) ;
#33800 = VERTEX_POINT ( 'NONE', #31790 ) ;
#33801 = CARTESIAN_POINT ( 'NONE',  ( -1.166476076187854022E-15, 160.0550000000000068, 9.525000000000000355 ) ) ;
#33802 = CARTESIAN_POINT ( 'NONE',  ( 179.4361977533476136, 5.000000000000000000, 103.7004518695250823 ) ) ;
#33803 =( GEOMETRIC_REPRESENTATION_CONTEXT ( 3 ) GLOBAL_UNCERTAINTY_ASSIGNED_CONTEXT ( ( #41073 ) ) GLOBAL_UNIT_ASSIGNED_CONTEXT ( ( #38916, #55746, #50471 ) ) REPRESENTATION_CONTEXT ( 'NONE', 'WORKASPACE' ) );
#33804 = PLANE ( 'NONE',  #24349 ) ;
#33805 = DIRECTION ( 'NONE',  ( 0.000000000000000000, 0.000000000000000000, 1.000000000000000000 ) ) ;
#33806 = CARTESIAN_POINT ( 'NONE',  ( -22.50000000000000711, 33.99999999999999289, 4.000000000000000000 ) ) ;
#33807 = ORIENTED_EDGE ( 'NONE', *, *, #20186, .F. ) ;
#33808 = ORIENTED_EDGE ( 'NONE', *, *, #32467, .T. ) ;
#33809 = SURFACE_STYLE_FILL_AREA ( #28152 ) ;
#33811 = CARTESIAN_POINT ( 'NONE',  ( -160.5550000000000068, 0.000000000000000000, 8.024999999999991473 ) ) ;
#33810 = MECHANICAL_DESIGN_GEOMETRIC_PRESENTATION_REPRESENTATION (  '', ( #67505 ), #50643 ) ;
#33812 = VERTEX_POINT ( 'NONE', #32463 ) ;
#33813 = CARTESIAN_POINT ( 'NONE',  ( 22.99999999999996447, 0.000000000000000000, -29.00402776293825369 ) ) ;
#33814 = AXIS2_PLACEMENT_3D ( 'NONE', #64240, #53016, #53686 ) ;
#33815 = COLOUR_RGB ( '', 0.66274510, 0.83137255, 0.94901961) ;
#33816 = CARTESIAN_POINT ( 'NONE',  ( -183.9999999999999716, -8.313263101079598982, 1.518308302792259701 ) ) ;
#33817 = DIRECTION ( 'NONE',  ( 0.000000000000000000, 1.000000000000000000, -0.000000000000000000 ) ) ;
#33818 = ORIENTED_EDGE ( 'NONE', *, *, #53533, .T. ) ;
#33819 = ORIENTED_EDGE ( 'NONE', *, *, #15552, .F. ) ;
#33820 = CIRCLE ( 'NONE', #25922, 0.2500000000000002220 ) ;
#33821 = CARTESIAN_POINT ( 'NONE',  ( -80.90499999999995850, 2.607480562269068880, -8.024999999999993250 ) ) ;
#33822 = VERTEX_POINT ( 'NONE', #53596 ) ;
#33823 = EDGE_CURVE ( 'NONE', #33911, #8613, #22301, .T. ) ;
#33824 = DIRECTION ( 'NONE',  ( 1.000000000000000000, -0.000000000000000000, -0.000000000000000000 ) ) ;
#33825 = LINE ( 'NONE', #51409, #46621 ) ;
#33826 = EDGE_CURVE ( 'NONE', #44582, #48466, #27971, .T. ) ;
#33827 = PRESENTATION_LAYER_ASSIGNMENT (  '', '', ( #50718 ) ) ;
#33828 = CARTESIAN_POINT ( 'NONE',  ( -75.00000000000000000, 8.121151660576289899, -6.396433738442264705 ) ) ;
#33829 = ORIENTED_EDGE ( 'NONE', *, *, #11081, .T. ) ;
#33830 = PRESENTATION_STYLE_ASSIGNMENT (( #12365 ) ) ;
#33832 = DIRECTION ( 'NONE',  ( -1.000000000000000000, 0.000000000000000000, 0.000000000000000000 ) ) ;
#33831 = DIRECTION ( 'NONE',  ( 1.000000000000000000, 0.000000000000000000, -0.000000000000000000 ) ) ;
#33833 = CARTESIAN_POINT ( 'NONE',  ( -8.102448949553181734, 127.8949999999999534, -5.886773742842749790 ) ) ;
#33834 = CARTESIAN_POINT ( 'NONE',  ( -108.5949999999999847, 2.607480562269073321, 8.024999999999991473 ) ) ;
#33835 = MECHANICAL_DESIGN_GEOMETRIC_PRESENTATION_REPRESENTATION (  '', ( #47348 ), #52942 ) ;
#33836 = EDGE_CURVE ( 'NONE', #2790, #44704, #34778, .T. ) ;
#33838 = CARTESIAN_POINT ( 'NONE',  ( -17.51489521397122573, 11.19178930173965725, 4.333724509350330933 ) ) ;
#33837 = SURFACE_STYLE_USAGE ( .BOTH. , #54931 ) ;
#33839 = EDGE_CURVE ( 'NONE', #30495, #58318, #35907, .T. ) ;
#33840 = CARTESIAN_POINT ( 'NONE',  ( -155.3929263765337794, 8.102448949553176405, 5.886773742842740909 ) ) ;
#33841 = CARTESIAN_POINT ( 'NONE',  ( -170.6949999999999932, -8.437984349512085203, 5.166775262442717831E-16 ) ) ;
#33842 = CIRCLE ( 'NONE', #67554, 1.000000000000000888 ) ;
#33843 = FACE_OUTER_BOUND ( 'NONE', #55713, .T. ) ;
#33844 = VERTEX_POINT ( 'NONE', #2496 ) ;
#33845 = CARTESIAN_POINT ( 'NONE',  ( 60.00000000000000000, -2.024042244987997205E-14, -10.00000000000000000 ) ) ;
#33846 = ORIENTED_EDGE ( 'NONE', *, *, #25431, .F. ) ;
#33847 = AXIS2_PLACEMENT_3D ( 'NONE', #21140, #42645, #14149 ) ;
#33848 = CARTESIAN_POINT ( 'NONE',  ( -69.74292637653380211, -5.598654528085803328, -7.705886871421366635 ) ) ;
#33849 = CARTESIAN_POINT ( 'NONE',  ( -45.57140627820939471, 8.073499555448574228, 6.499999999999999112 ) ) ;
#33850 =( BOUNDED_CURVE ( )  B_SPLINE_CURVE ( 2, ( #64892, #49776, #65240, #39240, #12456, #33918, #38568, #55386, #16741, #49109, #59966 ),
 .UNSPECIFIED., .F., .F. ) 
 B_SPLINE_CURVE_WITH_KNOTS ( ( 3, 2, 2, 2, 2, 3 ),
 ( 0.9347826086956522174, 0.9369565217391304657, 0.9391304347826087140, 0.9413043478260869623, 0.9434782608695652106, 0.9456521739130434590 ),
 .UNSPECIFIED. ) 
 CURVE ( )  GEOMETRIC_REPRESENTATION_ITEM ( )  RATIONAL_B_SPLINE_CURVE ( ( 1.000000000000000000, 0.9510565162951535312, 1.000000000000000000, 0.9510565162951535312, 1.000000000000000000, 0.9510565162951535312, 1.000000000000000000, 0.9510565162951535312, 1.000000000000000000, 0.9510565162951535312, 1.000000000000000000 ) ) 
 REPRESENTATION_ITEM ( '' )  );
#33851 = DIRECTION ( 'NONE',  ( 0.000000000000000000, 0.000000000000000000, 1.000000000000000000 ) ) ;
#33852 = STYLED_ITEM ( 'NONE', ( #38169 ), #45950 ) ;
#33853 = CIRCLE ( 'NONE', #49604, 1.000000000000000000 ) ;
#33854 = CARTESIAN_POINT ( 'NONE',  ( 5.196152422706628471, 2.500000000000000000, -9.000000000000005329 ) ) ;
#33855 = CARTESIAN_POINT ( 'NONE',  ( -5.196152422706634688, -9.000000000000005329, 1.392304845413258052 ) ) ;
#33856 = COLOUR_RGB ( '', 0.66274510, 0.83137255, 0.94901961) ;
#33857 = VERTEX_POINT ( 'NONE', #61288 ) ;
#33858 = CARTESIAN_POINT ( 'NONE',  ( -166.1049999999999898, -6.826472737025113702, 4.959722759717902107 ) ) ;
#33859 = EDGE_LOOP ( 'NONE', ( #41272, #61124, #6387, #30549 ) ) ;
#33860 = SURFACE_STYLE_FILL_AREA ( #50078 ) ;
#33861 = SURFACE_STYLE_USAGE ( .BOTH. , #65891 ) ;
#33862 = DIRECTION ( 'NONE',  ( -0.000000000000000000, -1.000000000000000000, -0.000000000000000000 ) ) ;
#33863 = AXIS2_PLACEMENT_3D ( 'NONE', #14175, #61630, #13455 ) ;
#33864 = CARTESIAN_POINT ( 'NONE',  ( -8.437984349512095861, 148.8070736234661240, -5.166775262442723748E-16 ) ) ;
#33865 = EDGE_CURVE ( 'NONE', #37744, #17986, #44809, .T. ) ;
#33866 = AXIS2_PLACEMENT_3D ( 'NONE', #3638, #30051, #35354 ) ;
#33867 = ORIENTED_EDGE ( 'NONE', *, *, #40101, .F. ) ;
#33868 = DIRECTION ( 'NONE',  ( 1.000000000000000000, 0.000000000000000000, -1.300977106640435137E-16 ) ) ;
#33869 = CARTESIAN_POINT ( 'NONE',  ( -78.95499999999998408, -7.632228543268599452, 2.479861379858951054 ) ) ;
#33870 = CARTESIAN_POINT ( 'NONE',  ( -9.827790563157511022E-16, 122.5570736234661524, 8.025000000000000355 ) ) ;
#33871 = EDGE_CURVE ( 'NONE', #31257, #8740, #49369, .T. ) ;
#33872 = CARTESIAN_POINT ( 'NONE',  ( -9.058813317711337021, 129.1550000000000011, -2.943386871421374895 ) ) ;
#33873 = CIRCLE ( 'NONE', #67592, 10.49999999999999822 ) ;
#33874 =( NAMED_UNIT ( * ) PLANE_ANGLE_UNIT ( ) SI_UNIT ( $, .RADIAN. ) );
#33875 = CARTESIAN_POINT ( 'NONE',  ( 73.01088739851485343, 5.000000000000000000, 65.71817553072288831 ) ) ;
#33876 = CARTESIAN_POINT ( 'NONE',  ( -168.8929263765337794, -8.102448949553174629, -5.886773742842741797 ) ) ;
#33877 = CARTESIAN_POINT ( 'NONE',  ( -113.3929263765337936, 8.102448949553176405, 5.886773742842740909 ) ) ;
#33878 = CARTESIAN_POINT ( 'NONE',  ( 67.50000000000000000, 1.797044900979284448E-15, -11.50000000000000000 ) ) ;
#33879 = PRESENTATION_LAYER_ASSIGNMENT (  '', '', ( #58598 ) ) ;
#33880 = VERTEX_POINT ( 'NONE', #13440 ) ;
#33881 = LINE ( 'NONE', #17736, #21577 ) ;
#33882 = CARTESIAN_POINT ( 'NONE',  ( -58.49499999999998323, 6.826472737025113702, -4.959722759717902107 ) ) ;
#33883 = VERTEX_POINT ( 'NONE', #60255 ) ;
#33884 = CARTESIAN_POINT ( 'NONE',  ( 8.082903768654761123, -1.417096231345241097, 9.294316082458970795E-16 ) ) ;
#33885 = AXIS2_PLACEMENT_3D ( 'NONE', #50608, #45026, #2345 ) ;
#33886 = CARTESIAN_POINT ( 'NONE',  ( 22.00000000000002132, 43.00000000000000000, 90.00000000000000000 ) ) ;
#33887 = CARTESIAN_POINT ( 'NONE',  ( -45.00000000000000000, 9.289150624329689521, -6.641434857031669026 ) ) ;
#33888 = VERTEX_POINT ( 'NONE', #23313 ) ;
#33889 = CARTESIAN_POINT ( 'NONE',  ( -48.87409065588625623, -13.04242605562483703, 1.033469574933718604 ) ) ;
#33890 = CARTESIAN_POINT ( 'NONE',  ( -57.89499999999996760, 6.826472737025115478, 4.959722759717899443 ) ) ;
#33891 = CARTESIAN_POINT ( 'NONE',  ( -65.50000000000000000, -1.956686671034892874E-14, -6.500000000000000000 ) ) ;
#33892 = ORIENTED_EDGE ( 'NONE', *, *, #50796, .F. ) ;
#33893 = AXIS2_PLACEMENT_3D ( 'NONE', #28821, #38044, #43675 ) ;
#33894 = EDGE_CURVE ( 'NONE', #6686, #8720, #61612, .T. ) ;
#33895 = DIRECTION ( 'NONE',  ( 0.000000000000000000, 0.000000000000000000, -1.000000000000000000 ) ) ;
#33896 = CARTESIAN_POINT ( 'NONE',  ( -114.0549999999999926, -9.827790563157499189E-16, -8.024999999999991473 ) ) ;
#33897 = EDGE_LOOP ( 'NONE', ( #62644, #64357, #36260, #23234, #18463, #37495, #45186, #42276, #82, #19529, #28745, #45344, #29192, #48234, #21670, #44511, #49836, #46090, #43204, #37315, #64508, #12789, #14606, #56799, #55949, #52093, #25734, #44898, #65332, #8898, #59378, #34184, #28843, #33655 ) ) ;
#33898 = EDGE_CURVE ( 'NONE', #61448, #33800, #7485, .T. ) ;
#33899 = LINE ( 'NONE', #13845, #10372 ) ;
#33900 = CARTESIAN_POINT ( 'NONE',  ( -24.21231517720798010, 113.4999999999999858, 10.00000000000000000 ) ) ;
#33901 = DIRECTION ( 'NONE',  ( 0.000000000000000000, 0.000000000000000000, -1.000000000000000000 ) ) ;
#33902 = DIRECTION ( 'NONE',  ( 0.000000000000000000, 0.000000000000000000, 1.000000000000000000 ) ) ;
#33903 = CARTESIAN_POINT ( 'NONE',  ( -147.8070736234661524, 10.01517768586948698, -1.839758294383808571E-15 ) ) ;
#33904 =( GEOMETRIC_REPRESENTATION_CONTEXT ( 3 ) GLOBAL_UNCERTAINTY_ASSIGNED_CONTEXT ( ( #217 ) ) GLOBAL_UNIT_ASSIGNED_CONTEXT ( ( #32735, #53839, #11630 ) ) REPRESENTATION_CONTEXT ( 'NONE', 'WORKASPACE' ) );
#33905 = CARTESIAN_POINT ( 'NONE',  ( 48.75000000000000000, 22.24999999999998579, 3.750000000000000000 ) ) ;
#33906 = CARTESIAN_POINT ( 'NONE',  ( 9.058813317711338797, 129.8449999999999989, -2.943386871421372675 ) ) ;
#33907 = CARTESIAN_POINT ( 'NONE',  ( -84.20707362346614389, 3.094860106618433360, 9.524999999999991473 ) ) ;
#33908 = MECHANICAL_DESIGN_GEOMETRIC_PRESENTATION_REPRESENTATION (  '', ( #5825 ), #28304 ) ;
#33909 = EDGE_CURVE ( 'NONE', #29083, #9427, #24008, .T. ) ;
#33910 =( NAMED_UNIT ( * ) PLANE_ANGLE_UNIT ( ) SI_UNIT ( $, .RADIAN. ) );
#33911 = VERTEX_POINT ( 'NONE', #33855 ) ;
#33912 = CARTESIAN_POINT ( 'NONE',  ( 30.99999999999999289, 5.000000000000000000, -37.00402776293829277 ) ) ;
#33913 = EDGE_CURVE ( 'NONE', #25661, #64306, #44163, .T. ) ;
#33915 = SURFACE_STYLE_FILL_AREA ( #6840 ) ;
#33914 = CARTESIAN_POINT ( 'NONE',  ( 10.39230484541326582, 1.107695154586738839, 1.440973567693753677E-18 ) ) ;
#33916 = CARTESIAN_POINT ( 'NONE',  ( -135.0549999999999784, -9.827790563157499189E-16, -8.024999999999991473 ) ) ;
#33917 = DIRECTION ( 'NONE',  ( -0.000000000000000000, -1.000000000000000000, 0.000000000000000000 ) ) ;
#33918 = CARTESIAN_POINT ( 'NONE',  ( -55.19292637653379785, -10.01517768586948698, 6.132527647946031529E-16 ) ) ;
#33919 = CIRCLE ( 'NONE', #39591, 13.99999999999999822 ) ;
#33920 = CARTESIAN_POINT ( 'NONE',  ( -132.7450000000000045, 4.716976649647094177, 6.492361379858945902 ) ) ;
#33921 = EDGE_CURVE ( 'NONE', #22828, #64131, #11180, .T. ) ;
#33922 = CARTESIAN_POINT ( 'NONE',  ( -128.6949999999999932, -8.437984349512086979, 5.166775262442717831E-16 ) ) ;
#33923 = MECHANICAL_DESIGN_GEOMETRIC_PRESENTATION_REPRESENTATION (  '', ( #27171 ), #3557 ) ;
#33924 = CARTESIAN_POINT ( 'NONE',  ( 66.24999999999998579, 34.24999999999999289, 4.000000000000000000 ) ) ;
#33925 = ORIENTED_EDGE ( 'NONE', *, *, #6667, .F. ) ;
#33926 = DIRECTION ( 'NONE',  ( 0.000000000000000000, -1.000000000000000000, 0.000000000000000000 ) ) ;
#33927 = PRESENTATION_STYLE_ASSIGNMENT (( #23049 ) ) ;
#33928 = EDGE_CURVE ( 'NONE', #42069, #31871, #18395, .T. ) ;
#33929 = CARTESIAN_POINT ( 'NONE',  ( -181.0429263765338135, -9.058813317711329915, -2.943386871421370898 ) ) ;
#33930 = MECHANICAL_DESIGN_GEOMETRIC_PRESENTATION_REPRESENTATION (  '', ( #23790 ), #18169 ) ;
#33931 = CARTESIAN_POINT ( 'NONE',  ( -53.54499999999998039, -7.632228543268600340, -2.479861379858950166 ) ) ;
#33932 = COLOUR_RGB ( '', 0.66274510, 0.83137255, 0.94901961) ;
#33933 = CARTESIAN_POINT ( 'NONE',  ( 11.00000000000001776, 16.44305403005404287, 6.465863758942333782E-16 ) ) ;
#33934 = CARTESIAN_POINT ( 'NONE',  ( -103.2570736234661695, 5.598654528085800663, -7.705886871421367523 ) ) ;
#33935 = FILL_AREA_STYLE ('',( #38919 ) ) ;
#33936 = CARTESIAN_POINT ( 'NONE',  ( -54.73148258177910463, -9.107254030097815090, -2.000000000000000000 ) ) ;
#33937 =( LENGTH_UNIT ( ) NAMED_UNIT ( * ) SI_UNIT ( .MILLI., .METRE. ) );
#33938 = CARTESIAN_POINT ( 'NONE',  ( -96.59292637653379643, -3.094860106618431139, -9.524999999999991473 ) ) ;
#33939 = APPLICATION_PROTOCOL_DEFINITION ( 'draft international standard', 'automotive_design', 1998, #67111 ) ;
#33940 = CARTESIAN_POINT ( 'NONE',  ( -49.94031648296357417, -12.57106785925259551, 1.201245605581311882 ) ) ;
#33941 =( NAMED_UNIT ( * ) SI_UNIT ( $, .STERADIAN. ) SOLID_ANGLE_UNIT ( ) );
#33942 = CIRCLE ( 'NONE', #50780, 9.000000000000000000 ) ;
#33943 = CARTESIAN_POINT ( 'NONE',  ( 59.00000000000000000, 11.99999999999999822, 3.499999999999992895 ) ) ;
#33944 = PRESENTATION_STYLE_ASSIGNMENT (( #18128 ) ) ;
#33945 = CARTESIAN_POINT ( 'NONE',  ( -163.1929263765338192, -10.01517768586948698, 6.132527647946031529E-16 ) ) ;
#33946 = MECHANICAL_DESIGN_GEOMETRIC_PRESENTATION_REPRESENTATION (  '', ( #6992 ), #39615 ) ;
#33947 = DIRECTION ( 'NONE',  ( -0.000000000000000000, -0.000000000000000000, -1.000000000000000000 ) ) ;
#33948 = VERTEX_POINT ( 'NONE', #18727 ) ;
#33949 = SURFACE_SIDE_STYLE ('',( #23070 ) ) ;
#33950 = CARTESIAN_POINT ( 'NONE',  ( -75.48275862068965125, 63.99167409976912069, -41.30495168499704306 ) ) ;
#33951 = ORIENTED_EDGE ( 'NONE', *, *, #55130, .T. ) ;
#33952 = PRESENTATION_LAYER_ASSIGNMENT (  '', '', ( #9279 ) ) ;
#33953 = CARTESIAN_POINT ( 'NONE',  ( -2.607480562269075097, 128.4070736234661183, 8.025000000000000355 ) ) ;
#33954 = ADVANCED_FACE ( 'NONE', ( #1800, #50072 ), #60578, .F. ) ;
#33955 = MECHANICAL_DESIGN_GEOMETRIC_PRESENTATION_REPRESENTATION (  '', ( #8172 ), #10432 ) ;
#33956 = FILL_AREA_STYLE_COLOUR ( '', #28173 ) ;
#33957 = CARTESIAN_POINT ( 'NONE',  ( -74.50000000000001421, 36.50926243676796190, 10.00000000000000000 ) ) ;
#33958 = VECTOR ( 'NONE', #56832, 1000.000000000000000 ) ;
#33959 = SURFACE_STYLE_FILL_AREA ( #148 ) ;
#33960 = ORIENTED_EDGE ( 'NONE', *, *, #35437, .T. ) ;
#33961 = PLANE ( 'NONE',  #1718 ) ;
#33962 = CARTESIAN_POINT ( 'NONE',  ( 53.00000000000000000, 24.99999999999998579, 3.750000000000000000 ) ) ;
#33963 = VERTEX_POINT ( 'NONE', #34553 ) ;
#33964 = DIRECTION ( 'NONE',  ( 1.000000000000000000, 0.000000000000000000, 0.000000000000000000 ) ) ;
#33965 = SURFACE_STYLE_FILL_AREA ( #7930 ) ;
#33966 = AXIS2_PLACEMENT_3D ( 'NONE', #13037, #59843, #2057 ) ;
#33967 = PRESENTATION_LAYER_ASSIGNMENT (  '', '', ( #50854 ) ) ;
#33968 = CARTESIAN_POINT ( 'NONE',  ( 6.826472737025119919, 148.8929263765338078, 4.959722759717908325 ) ) ;
#33969 = CARTESIAN_POINT ( 'NONE',  ( -87.59499999999999886, 2.607480562269073321, 8.024999999999991473 ) ) ;
#33970 = VERTEX_POINT ( 'NONE', #45517 ) ;
#33971 = PRESENTATION_LAYER_ASSIGNMENT (  '', '', ( #55375 ) ) ;
#33972 = CARTESIAN_POINT ( 'NONE',  ( -5.000000000000000000, 0.000000000000000000, 7.500000000000000000 ) ) ;
#33973 = EDGE_CURVE ( 'NONE', #41992, #32584, #52054, .T. ) ;
#33974 = CARTESIAN_POINT ( 'NONE',  ( 45.50000000000000000, 9.639620389971918613, 6.500000000000000888 ) ) ;
#33975 =( NAMED_UNIT ( * ) PLANE_ANGLE_UNIT ( ) SI_UNIT ( $, .RADIAN. ) );
#33976 = UNCERTAINTY_MEASURE_WITH_UNIT (LENGTH_MEASURE( 1.000000000000000082E-05 ), #54648, 'distance_accuracy_value', 'NONE');
#33977 = VERTEX_POINT ( 'NONE', #51104 ) ;
#33978 = CARTESIAN_POINT ( 'NONE',  ( 8.437984349512095861, 161.1929263765338192, 1.550032578732817026E-15 ) ) ;
#33979 = EDGE_CURVE ( 'NONE', #30440, #19491, #7867, .T. ) ;
#33980 = EDGE_CURVE ( 'NONE', #3150, #64454, #69286, .T. ) ;
#33981 = MECHANICAL_DESIGN_GEOMETRIC_PRESENTATION_REPRESENTATION (  '', ( #68853 ), #34031 ) ;
#33982 = ORIENTED_EDGE ( 'NONE', *, *, #28062, .T. ) ;
#33983 = EDGE_CURVE ( 'NONE', #11216, #68346, #62661, .T. ) ;
#33984 = COLOUR_RGB ( '', 0.40784314, 0.44705882, 0.49803922) ;
#33985 = ORIENTED_EDGE ( 'NONE', *, *, #26292, .F. ) ;
#33986 = DIRECTION ( 'NONE',  ( 0.000000000000000000, 0.000000000000000000, -1.000000000000000000 ) ) ;
#33987 = DIRECTION ( 'NONE',  ( -1.000000000000000000, -0.000000000000000000, -0.000000000000000000 ) ) ;
#33988 = CARTESIAN_POINT ( 'NONE',  ( -179.4570736234661865, -9.058813317711329915, 2.943386871421371787 ) ) ;
#33989 = DIRECTION ( 'NONE',  ( -0.000000000000000000, -0.000000000000000000, 1.000000000000000000 ) ) ;
#33990 = CARTESIAN_POINT ( 'NONE',  ( 8.082903768654762899, -1.105959442090949618E-15, 7.500000000000000000 ) ) ;
#33991 = CARTESIAN_POINT ( 'NONE',  ( -110.0070736234661837, -8.102448949553172852, -5.886773742842741797 ) ) ;
#33992 = CIRCLE ( 'NONE', #16062, 0.5000000000000004441 ) ;
#33993 =( NAMED_UNIT ( * ) SI_UNIT ( $, .STERADIAN. ) SOLID_ANGLE_UNIT ( ) );
#33994 = AXIS2_PLACEMENT_3D ( 'NONE', #49473, #16456, #27966 ) ;
#33995 = DIRECTION ( 'NONE',  ( 0.000000000000000000, 0.000000000000000000, -1.000000000000000000 ) ) ;
#33996 = EDGE_LOOP ( 'NONE', ( #42437, #45682, #18724, #59494, #25826, #37924, #64370 ) ) ;
#33997 = CARTESIAN_POINT ( 'NONE',  ( 6.826472737025119919, 121.8929263765338220, 4.959722759717908325 ) ) ;
#33998 = EDGE_CURVE ( 'NONE', #67765, #33822, #31457, .T. ) ;
#33999 = FILL_AREA_STYLE ('',( #16817 ) ) ;
#34000 =( NAMED_UNIT ( * ) SI_UNIT ( $, .STERADIAN. ) SOLID_ANGLE_UNIT ( ) );
#34001 = ORIENTED_EDGE ( 'NONE', *, *, #16304, .F. ) ;
#34002 = CARTESIAN_POINT ( 'NONE',  ( -155.9049999999999443, 2.607480562269068880, -8.024999999999993250 ) ) ;
#34003 = DIRECTION ( 'NONE',  ( 9.376883653928687363E-17, 1.000000000000000000, 0.000000000000000000 ) ) ;
#34004 = CARTESIAN_POINT ( 'NONE',  ( -183.4562580486119430, -2.476980957186634136, -8.746383672357369576 ) ) ;
#34005 = CARTESIAN_POINT ( 'NONE',  ( -163.7950000000000159, 2.607480562269068880, -8.024999999999993250 ) ) ;
#34006 = CIRCLE ( 'NONE', #29487, 5.000000000000000000 ) ;
#34007 = CARTESIAN_POINT ( 'NONE',  ( -153.1450000000000102, -4.716976649647092401, 6.492361379858946790 ) ) ;
#34008 = ORIENTED_EDGE ( 'NONE', *, *, #6743, .T. ) ;
#34009 = DIRECTION ( 'NONE',  ( 0.000000000000000000, 0.000000000000000000, 1.000000000000000000 ) ) ;
#34010 = AXIS2_PLACEMENT_3D ( 'NONE', #12954, #23500, #56910 ) ;
#34011 = CARTESIAN_POINT ( 'NONE',  ( 44.30330429060720121, 9.767768096869062333, 3.048789874180130255 ) ) ;
#34012 = SURFACE_STYLE_FILL_AREA ( #52721 ) ;
#34013 = CARTESIAN_POINT ( 'NONE',  ( -74.00499999999996703, 6.826472737025116366, 4.959722759717898555 ) ) ;
#34014 = DIRECTION ( 'NONE',  ( 0.000000000000000000, -1.000000000000000000, 0.000000000000000000 ) ) ;
#34015 = AXIS2_PLACEMENT_3D ( 'NONE', #13832, #60959, #51462 ) ;
#34016 = SURFACE_SIDE_STYLE ('',( #22426 ) ) ;
#34017 = CARTESIAN_POINT ( 'NONE',  ( -70.34499999999998465, 7.632228543268599452, -2.479861379858951942 ) ) ;
#34018 = CARTESIAN_POINT ( 'NONE',  ( 5.598654528085809545, 143.2549999999999955, -7.705886871421373741 ) ) ;
#34019 = EDGE_CURVE ( 'NONE', #62248, #5399, #42728, .T. ) ;
#34020 = VECTOR ( 'NONE', #40150, 1000.000000000000000 ) ;
#34021 = CARTESIAN_POINT ( 'NONE',  ( -5.196152422706633800, -9.000000000000005329, 7.500000000000000000 ) ) ;
#34022 = CIRCLE ( 'NONE', #3659, 2.499999999999998668 ) ;
#34023 = CARTESIAN_POINT ( 'NONE',  ( -175.9429263765337907, 0.000000000000000000, 9.524999999999991473 ) ) ;
#34024 = EDGE_CURVE ( 'NONE', #1286, #66425, #56160, .T. ) ;
#34025 = UNCERTAINTY_MEASURE_WITH_UNIT (LENGTH_MEASURE( 1.000000000000000082E-05 ), #30271, 'distance_accuracy_value', 'NONE');
#34026 = VECTOR ( 'NONE', #11665, 1000.000000000000000 ) ;
#34027 =( NAMED_UNIT ( * ) PLANE_ANGLE_UNIT ( ) SI_UNIT ( $, .RADIAN. ) );
#34028 = DIRECTION ( 'NONE',  ( -0.000000000000000000, 0.000000000000000000, -1.000000000000000000 ) ) ;
#34029 = CARTESIAN_POINT ( 'NONE',  ( 0.000000000000000000, 114.4999999999999574, 0.000000000000000000 ) ) ;
#34030 = AXIS2_PLACEMENT_3D ( 'NONE', #30494, #61808, #14333 ) ;
#34031 =( GEOMETRIC_REPRESENTATION_CONTEXT ( 3 ) GLOBAL_UNCERTAINTY_ASSIGNED_CONTEXT ( ( #10294 ) ) GLOBAL_UNIT_ASSIGNED_CONTEXT ( ( #34192, #51068, #40530 ) ) REPRESENTATION_CONTEXT ( 'NONE', 'WORKASPACE' ) );
#34032 = LINE ( 'NONE', #1628, #4603 ) ;
#34033 = COLOUR_RGB ( '', 0.66274510, 0.83137255, 0.94901961) ;
#34034 =( NAMED_UNIT ( * ) PLANE_ANGLE_UNIT ( ) SI_UNIT ( $, .RADIAN. ) );
#34035 = CARTESIAN_POINT ( 'NONE',  ( 32.00000000000001421, 42.00000000000000000, 36.49999999999999289 ) ) ;
#34036 = ORIENTED_EDGE ( 'NONE', *, *, #46834, .T. ) ;
#34037 = EDGE_LOOP ( 'NONE', ( #66399, #24343, #18235, #52247 ) ) ;
#34038 = CARTESIAN_POINT ( 'NONE',  ( 0.000000000000000000, 13.00000000000000178, -36.49999999999999289 ) ) ;
#34039 = CARTESIAN_POINT ( 'NONE',  ( 36.00000000000002842, 5.000000000000000000, -29.00402776293825724 ) ) ;
#34040 = COLOUR_RGB ( '', 0.09019608, 0.27058824, 0.51372549) ;
#34041 = FILL_AREA_STYLE ('',( #39355 ) ) ;
#34042 = SURFACE_STYLE_FILL_AREA ( #50235 ) ;
#34043 = CARTESIAN_POINT ( 'NONE',  ( -12.74999999999999822, 4.336808689942018722E-16, 5.000000000000001776 ) ) ;
#34044 = ORIENTED_EDGE ( 'NONE', *, *, #40221, .F. ) ;
#34045 = CARTESIAN_POINT ( 'NONE',  ( -102.8049999999999784, -8.437984349512086979, 5.166775262442717831E-16 ) ) ;
#34046 = ORIENTED_EDGE ( 'NONE', *, *, #46692, .T. ) ;
#34047 = SURFACE_STYLE_FILL_AREA ( #66047 ) ;
#34048 = EDGE_LOOP ( 'NONE', ( #17865, #26911, #12214, #54800 ) ) ;
#34049 = CARTESIAN_POINT ( 'NONE',  ( -56.99292637653380211, 8.102448949553172852, -5.886773742842744461 ) ) ;
#34050 = DIRECTION ( 'NONE',  ( -0.000000000000000000, -0.000000000000000000, -1.000000000000000000 ) ) ;
#34051 = ORIENTED_EDGE ( 'NONE', *, *, #17948, .F. ) ;
#34052 = EDGE_CURVE ( 'NONE', #52470, #34254, #59194, .T. ) ;
#34053 = AXIS2_PLACEMENT_3D ( 'NONE', #21066, #69596, #53437 ) ;
#34054 = AXIS2_PLACEMENT_3D ( 'NONE', #40294, #30055, #3281 ) ;
#34055 = CARTESIAN_POINT ( 'NONE',  ( -17.75000000000000355, -3.000000000000000000, 20.00000000000000000 ) ) ;
#34056 = EDGE_LOOP ( 'NONE', ( #67257, #62072, #1985, #38048 ) ) ;
#34057 = EDGE_LOOP ( 'NONE', ( #28150, #53898, #7145 ) ) ;
#34058 = AXIS2_PLACEMENT_3D ( 'NONE', #42363, #6, #63418 ) ;
#34059 = SURFACE_STYLE_USAGE ( .BOTH. , #12590 ) ;
#34060 = DIRECTION ( 'NONE',  ( 0.000000000000000000, 0.000000000000000000, 1.000000000000000000 ) ) ;
#34061 = CARTESIAN_POINT ( 'NONE',  ( 44.99999999999998579, 119.9999999999999716, -7.500000000000000000 ) ) ;
#34062 = EDGE_CURVE ( 'NONE', #6066, #37003, #1010, .T. ) ;
#34063 = DIRECTION ( 'NONE',  ( 0.000000000000000000, 0.000000000000000000, 1.000000000000000000 ) ) ;
#34064 = ORIENTED_EDGE ( 'NONE', *, *, #40198, .F. ) ;
#34065 = CARTESIAN_POINT ( 'NONE',  ( 2.607480562269076430, 137.7929263765338135, -8.025000000000000355 ) ) ;
#34066 = DIRECTION ( 'NONE',  ( 1.000000000000000000, -0.000000000000000000, -0.000000000000000000 ) ) ;
#34067 = CARTESIAN_POINT ( 'NONE',  ( -195.0000000000000000, 0.000000000000000000, 5.499999999999985789 ) ) ;
#34068 = DIRECTION ( 'NONE',  ( 1.000000000000000000, 0.000000000000000000, 0.000000000000000000 ) ) ;
#34069 = EDGE_CURVE ( 'NONE', #52109, #42774, #1068, .T. ) ;
#34070 = CARTESIAN_POINT ( 'NONE',  ( 22.50000000000000711, 34.24999999999999289, 4.000000000000000000 ) ) ;
#34071 = VECTOR ( 'NONE', #48709, 1000.000000000000000 ) ;
#34072 = ORIENTED_EDGE ( 'NONE', *, *, #8515, .F. ) ;
#34073 = ORIENTED_EDGE ( 'NONE', *, *, #18816, .T. ) ;
#34074 = FILL_AREA_STYLE ('',( #18604 ) ) ;
#34075 = CARTESIAN_POINT ( 'NONE',  ( -13.23915246117191025, 52.65078610323165265, 6.947530358905294356 ) ) ;
#34076 = DIRECTION ( 'NONE',  ( 0.000000000000000000, 0.000000000000000000, 1.000000000000000000 ) ) ;
#34077 = CARTESIAN_POINT ( 'NONE',  ( -128.7549999999999955, 4.716976649647091513, -6.492361379858946790 ) ) ;
#34078 = AXIS2_PLACEMENT_3D ( 'NONE', #31652, #58065, #63326 ) ;
#34079 = DIRECTION ( 'NONE',  ( 0.000000000000000000, 1.000000000000000000, 0.000000000000000000 ) ) ;
#34080 = ORIENTED_EDGE ( 'NONE', *, *, #50753, .T. ) ;
#34081 = FILL_AREA_STYLE_COLOUR ( '', #18308 ) ;
#34082 = MECHANICAL_DESIGN_GEOMETRIC_PRESENTATION_REPRESENTATION (  '', ( #42029 ), #10600 ) ;
#34083 = EDGE_LOOP ( 'NONE', ( #2620, #46136, #24272, #57317 ) ) ;
#34084 = ORIENTED_EDGE ( 'NONE', *, *, #14463, .T. ) ;
#34085 = DIRECTION ( 'NONE',  ( -1.000000000000000000, -9.811390859391773608E-17, -0.000000000000000000 ) ) ;
#34086 = STYLED_ITEM ( 'NONE', ( #36715 ), #6209 ) ;
#34087 = CARTESIAN_POINT ( 'NONE',  ( -20.77811424250900174, 115.1386898118646656, 10.00000000000000000 ) ) ;
#34088 = ADVANCED_FACE ( 'NONE', ( #46560 ), #19768, .T. ) ;
#34089 = AXIS2_PLACEMENT_3D ( 'NONE', #18270, #28440, #34095 ) ;
#34090 = ORIENTED_EDGE ( 'NONE', *, *, #12000, .F. ) ;
#34091 = LINE ( 'NONE', #17917, #10145 ) ;
#34092 = CARTESIAN_POINT ( 'NONE',  ( 0.000000000000000000, 0.000000000000000000, 0.000000000000000000 ) ) ;
#34093 = DIRECTION ( 'NONE',  ( -0.000000000000000000, -0.000000000000000000, -1.000000000000000000 ) ) ;
#34094 = CARTESIAN_POINT ( 'NONE',  ( 2.755511676787084419, 7.000000000000007105, 0.5168645644872258416 ) ) ;
#34095 = DIRECTION ( 'NONE',  ( 0.000000000000000000, 0.000000000000000000, 1.000000000000000000 ) ) ;
#34096 = CARTESIAN_POINT ( 'NONE',  ( -177.3570736234661638, 5.598654528085804216, 7.705886871421366635 ) ) ;
#34097 = VERTEX_POINT ( 'NONE', #57408 ) ;
#34098 = COLOUR_RGB ( '', 0.31764706, 0.68627451, 0.89019608) ;
#34099 = SPHERICAL_SURFACE ( 'NONE', #40348, 0.5000000000000000000 ) ;
#34100 = AXIS2_PLACEMENT_3D ( 'NONE', #6183, #5132, #38238 ) ;
#34101 = LINE ( 'NONE', #33411, #42721 ) ;
#34102 =( LENGTH_UNIT ( ) NAMED_UNIT ( * ) SI_UNIT ( .MILLI., .METRE. ) );
#34103 = CARTESIAN_POINT ( 'NONE',  ( -60.39042638714564504, -8.499999999999994671, 1.000000000000000000 ) ) ;
#34104 = DIRECTION ( 'NONE',  ( -1.000000000000000000, -0.000000000000000000, -0.000000000000000000 ) ) ;
#34105 = DIRECTION ( 'NONE',  ( 0.000000000000000000, 0.000000000000000000, 1.000000000000000000 ) ) ;
#34106 = CARTESIAN_POINT ( 'NONE',  ( -99.89499999999998181, 6.826472737025115478, 4.959722759717899443 ) ) ;
#34107 = CARTESIAN_POINT ( 'NONE',  ( 9.058813317711338797, 121.9549999999999841, -2.943386871421372675 ) ) ;
#34108 = CARTESIAN_POINT ( 'NONE',  ( -74.84499999999998465, -7.632228543268599452, 2.479861379858951054 ) ) ;
#34109 = STYLED_ITEM ( 'NONE', ( #63638 ), #61675 ) ;
#34110 = DIRECTION ( 'NONE',  ( 0.000000000000000000, 0.000000000000000000, 1.000000000000000000 ) ) ;
#34111 = CARTESIAN_POINT ( 'NONE',  ( 3.851859888774471706E-31, -8.500000000000000000, 24.00000000000000000 ) ) ;
#34112 = UNCERTAINTY_MEASURE_WITH_UNIT (LENGTH_MEASURE( 1.000000000000000082E-05 ), #56750, 'distance_accuracy_value', 'NONE');
#34113 = FILL_AREA_STYLE_COLOUR ( '', #26931 ) ;
#34114 = AXIS2_PLACEMENT_3D ( 'NONE', #64098, #36730, #5341 ) ;
#34115 = SURFACE_STYLE_USAGE ( .BOTH. , #34798 ) ;
#34116 = VERTEX_POINT ( 'NONE', #57768 ) ;
#34117 = COLOUR_RGB ( '', 0.08235294, 0.09019608, 0.10196078) ;
#34118 = CARTESIAN_POINT ( 'NONE',  ( -127.7929263765337993, -3.094860106618429807, 9.524999999999991473 ) ) ;
#34119 = CARTESIAN_POINT ( 'NONE',  ( -136.1949999999999363, 8.437984349512085203, -1.550032578732815448E-15 ) ) ;
#34120 =( NAMED_UNIT ( * ) SI_UNIT ( $, .STERADIAN. ) SOLID_ANGLE_UNIT ( ) );
#34121 = DIRECTION ( 'NONE',  ( 0.000000000000000000, 1.000000000000000000, 0.000000000000000000 ) ) ;
#34122 = CARTESIAN_POINT ( 'NONE',  ( -127.5570736234661950, -1.166476076187852838E-15, -9.524999999999991473 ) ) ;
#34123 = ORIENTED_EDGE ( 'NONE', *, *, #20567, .T. ) ;
#34124 = EDGE_LOOP ( 'NONE', ( #60589, #24677, #5093, #33818 ) ) ;
#34125 = AXIS2_PLACEMENT_3D ( 'NONE', #11842, #22755, #60029 ) ;
#34126 = DIRECTION ( 'NONE',  ( -1.000000000000000000, 0.000000000000000000, 0.000000000000000000 ) ) ;
#34127 = SURFACE_STYLE_FILL_AREA ( #59823 ) ;
#34128 = CIRCLE ( 'NONE', #17299, 8.000000000000000000 ) ;
#34129 = AXIS2_PLACEMENT_3D ( 'NONE', #12121, #51081, #7798 ) ;
#34130 = FILL_AREA_STYLE ('',( #12663 ) ) ;
#34131 = CARTESIAN_POINT ( 'NONE',  ( -131.1570736234661751, -9.058813317711329915, -2.943386871421370898 ) ) ;
#34132 = CARTESIAN_POINT ( 'NONE',  ( -6.413663052920317575, -2.891209729714697030, 1.212104147520903391E-15 ) ) ;
#34133 = DIRECTION ( 'NONE',  ( 0.000000000000000000, -0.000000000000000000, 1.000000000000000000 ) ) ;
#34134 = ORIENTED_EDGE ( 'NONE', *, *, #19996, .T. ) ;
#34135 = CARTESIAN_POINT ( 'NONE',  ( -138.9549999999999841, -7.632228543268599452, 2.479861379858951054 ) ) ;
#34136 = ORIENTED_EDGE ( 'NONE', *, *, #40616, .F. ) ;
#34137 = CIRCLE ( 'NONE', #12791, 29.50000000000000000 ) ;
#34138 = ORIENTED_EDGE ( 'NONE', *, *, #59182, .T. ) ;
#34139 = CARTESIAN_POINT ( 'NONE',  ( -48.00000000000000000, 99.99999999999992895, 7.000000000000000000 ) ) ;
#34140 = CARTESIAN_POINT ( 'NONE',  ( 16.00000000000001776, 43.00000000000000000, 29.68999999999999417 ) ) ;
#34141 = VERTEX_POINT ( 'NONE', #9594 ) ;
#34142 = EDGE_CURVE ( 'NONE', #57180, #29481, #10093, .T. ) ;
#34143 = CIRCLE ( 'NONE', #38665, 0.5000000000000004441 ) ;
#34144 = CYLINDRICAL_SURFACE ( 'NONE', #36097, 0.2500000000000002220 ) ;
#34145 = DIRECTION ( 'NONE',  ( 0.000000000000000000, -1.000000000000000000, 0.000000000000000000 ) ) ;
#34146 = CARTESIAN_POINT ( 'NONE',  ( 5.598654528085809545, 127.1449999999999818, -7.705886871421373741 ) ) ;
#34147 = SURFACE_SIDE_STYLE ('',( #7429 ) ) ;
#34148 = CIRCLE ( 'NONE', #42095, 0.5000000000000004441 ) ;
#34149 = ORIENTED_EDGE ( 'NONE', *, *, #48996, .F. ) ;
#34150 = AXIS2_PLACEMENT_3D ( 'NONE', #64173, #47012, #26189 ) ;
#34151 = PRESENTATION_STYLE_ASSIGNMENT (( #18985 ) ) ;
#34152 = CARTESIAN_POINT ( 'NONE',  ( -9.058813317711337021, 138.1550000000000011, -2.943386871421374895 ) ) ;
#34153 = CARTESIAN_POINT ( 'NONE',  ( -57.80499999999998550, -8.437984349512086979, 5.166775262442717831E-16 ) ) ;
#34154 = CARTESIAN_POINT ( 'NONE',  ( 41.13907225104257037, 107.8972693614197169, -3.376186789259871812 ) ) ;
#34155 = EDGE_LOOP ( 'NONE', ( #3843, #54943, #61616, #62511 ) ) ;
#34156 = CARTESIAN_POINT ( 'NONE',  ( 8.102448949553183510, 161.1049999999999613, -5.886773742842746238 ) ) ;
#34157 = CARTESIAN_POINT ( 'NONE',  ( 8.319377385370872346, -3.000000000000000888, -12.50000000000000000 ) ) ;
#34158 = UNCERTAINTY_MEASURE_WITH_UNIT (LENGTH_MEASURE( 1.000000000000000082E-05 ), #46903, 'distance_accuracy_value', 'NONE');
#34159 = EDGE_CURVE ( 'NONE', #53011, #37678, #13485, .T. ) ;
#34160 = CARTESIAN_POINT ( 'NONE',  ( -87.74292637653380211, -5.598654528085803328, -7.705886871421366635 ) ) ;
#34161 = CIRCLE ( 'NONE', #66695, 1.000000000000000888 ) ;
#34162 = SURFACE_STYLE_USAGE ( .BOTH. , #12690 ) ;
#34163 = EDGE_CURVE ( 'NONE', #67977, #56670, #4465, .T. ) ;
#34164 = DIRECTION ( 'NONE',  ( 0.000000000000000000, -1.000000000000000000, 0.000000000000000000 ) ) ;
#34165 = EDGE_LOOP ( 'NONE', ( #57605, #59820, #8160, #17963 ) ) ;
#34166 = EDGE_CURVE ( 'NONE', #61370, #41269, #38064, .T. ) ;
#34167 = CARTESIAN_POINT ( 'NONE',  ( 60.00000000000000000, -2.024042244987997205E-14, -7.000000000000000000 ) ) ;
#34168 = ORIENTED_EDGE ( 'NONE', *, *, #30117, .T. ) ;
#34169 =( NAMED_UNIT ( * ) PLANE_ANGLE_UNIT ( ) SI_UNIT ( $, .RADIAN. ) );
#34170 = AXIS2_PLACEMENT_3D ( 'NONE', #2221, #35361, #45930 ) ;
#34171 =( GEOMETRIC_REPRESENTATION_CONTEXT ( 3 ) GLOBAL_UNCERTAINTY_ASSIGNED_CONTEXT ( ( #68562 ) ) GLOBAL_UNIT_ASSIGNED_CONTEXT ( ( #51975, #57949, #68150 ) ) REPRESENTATION_CONTEXT ( 'NONE', 'WORKASPACE' ) );
#34172 = CARTESIAN_POINT ( 'NONE',  ( -121.7070736234669397, -3.094860106631069918, -9.524999999990811261 ) ) ;
#34173 = DIRECTION ( 'NONE',  ( 1.000000000000000000, 0.000000000000000000, 0.000000000000000000 ) ) ;
#34174 = CARTESIAN_POINT ( 'NONE',  ( -166.7049999999999557, 2.607480562269073321, 8.024999999999991473 ) ) ;
#34176 = ORIENTED_EDGE ( 'NONE', *, *, #69259, .T. ) ;
#34175 = ADVANCED_FACE ( 'NONE', ( #42654 ), #31705, .T. ) ;
#34177 = PRESENTATION_STYLE_ASSIGNMENT (( #28872 ) ) ;
#34178 = UNCERTAINTY_MEASURE_WITH_UNIT (LENGTH_MEASURE( 1.000000000000000082E-05 ), #19106, 'distance_accuracy_value', 'NONE');
#34179 = EDGE_CURVE ( 'NONE', #56168, #23696, #18478, .T. ) ;
#34180 = CARTESIAN_POINT ( 'NONE',  ( -65.99999999999998579, 50.00000000000000000, -10.49999999999999822 ) ) ;
#34181 = SURFACE_STYLE_FILL_AREA ( #28161 ) ;
#34182 = CARTESIAN_POINT ( 'NONE',  ( 57.74999999999998579, 30.74999999999999289, -4.000000000000000000 ) ) ;
#34183 = ORIENTED_EDGE ( 'NONE', *, *, #51331, .F. ) ;
#34184 = ORIENTED_EDGE ( 'NONE', *, *, #9889, .T. ) ;
#34185 =( NAMED_UNIT ( * ) SI_UNIT ( $, .STERADIAN. ) SOLID_ANGLE_UNIT ( ) );
#34186 = CARTESIAN_POINT ( 'NONE',  ( -45.91025672304794369, 9.422403540771759012, -3.407313310066902190 ) ) ;
#34187 = CARTESIAN_POINT ( 'NONE',  ( -75.95499999999998408, -7.632228543268599452, 2.479861379858951054 ) ) ;
#34188 = VERTEX_POINT ( 'NONE', #64764 ) ;
#34189 = DIRECTION ( 'NONE',  ( 0.000000000000000000, 1.000000000000000000, 0.000000000000000000 ) ) ;
#34190 = AXIS2_PLACEMENT_3D ( 'NONE', #2252, #39302, #61061 ) ;
#34191 =( BOUNDED_CURVE ( )  B_SPLINE_CURVE ( 2, ( #676, #1735, #22205 ),
 .UNSPECIFIED., .F., .F. ) 
 B_SPLINE_CURVE_WITH_KNOTS ( ( 3, 3 ),
 ( 0.8235294117647057321, 0.8246765007980889628 ),
 .UNSPECIFIED. ) 
 CURVE ( )  GEOMETRIC_REPRESENTATION_ITEM ( )  RATIONAL_B_SPLINE_CURVE ( ( 1.000000000000000888, 0.9904557693197235668, 0.9846338866368905540 ) ) 
 REPRESENTATION_ITEM ( '' )  );
#34192 =( LENGTH_UNIT ( ) NAMED_UNIT ( * ) SI_UNIT ( .MILLI., .METRE. ) );
#34193 = CARTESIAN_POINT ( 'NONE',  ( 44.99999999999977973, 149.4999999999999716, -9.500000000000000000 ) ) ;
#34194 = PRESENTATION_LAYER_ASSIGNMENT (  '', '', ( #1536 ) ) ;
#34195 = CIRCLE ( 'NONE', #12837, 0.2500000000000002220 ) ;
#34196 = ORIENTED_EDGE ( 'NONE', *, *, #3147, .F. ) ;
#34198 = DIRECTION ( 'NONE',  ( 0.000000000000000000, -1.000000000000000000, 0.000000000000000000 ) ) ;
#34197 = CYLINDRICAL_SURFACE ( 'NONE', #23341, 0.5000000000000004441 ) ;
#34199 = AXIS2_PLACEMENT_3D ( 'NONE', #38848, #39182, #15722 ) ;
#34200 = CARTESIAN_POINT ( 'NONE',  ( -5.598654528085808657, 134.6449999999999818, 7.705886871421373741 ) ) ;
#34201 = CARTESIAN_POINT ( 'NONE',  ( -107.9949999999999761, -6.826472737025115478, 4.959722759717900331 ) ) ;
#34202 = DIRECTION ( 'NONE',  ( 0.000000000000000000, 0.000000000000000000, 1.000000000000000000 ) ) ;
#34203 = VECTOR ( 'NONE', #34278, 1000.000000000000000 ) ;
#34205 = CARTESIAN_POINT ( 'NONE',  ( -195.0000000000000000, 1.166476076187852838E-15, -9.524999999999991473 ) ) ;
#34204 = CARTESIAN_POINT ( 'NONE',  ( -23.21231517720797655, 117.4999999999999716, -9.500000000000000000 ) ) ;
#34206 = AXIS2_PLACEMENT_3D ( 'NONE', #66793, #50268, #65745 ) ;
#34207 = CARTESIAN_POINT ( 'NONE',  ( -150.5929263765337964, -3.094860106618431139, -9.524999999999991473 ) ) ;
#34208 = CARTESIAN_POINT ( 'NONE',  ( -164.5449999999999875, -7.632228543268600340, -2.479861379858950166 ) ) ;
#34209 = CIRCLE ( 'NONE', #40975, 0.2500000000000002220 ) ;
#34210 = DIRECTION ( 'NONE',  ( -0.000000000000000000, -0.000000000000000000, -1.000000000000000000 ) ) ;
#34212 =( NAMED_UNIT ( * ) SI_UNIT ( $, .STERADIAN. ) SOLID_ANGLE_UNIT ( ) );
#34211 = COLOUR_RGB ( '', 0.31764706, 0.68627451, 0.89019608) ;
#34213 = VERTEX_POINT ( 'NONE', #20824 ) ;
#34214 = CARTESIAN_POINT ( 'NONE',  ( 15.98999599679679839, 117.4999999999999716, -10.00000000000000000 ) ) ;
#34215 = EDGE_LOOP ( 'NONE', ( #31197, #33183, #46387, #12842 ) ) ;
#34216 = CARTESIAN_POINT ( 'NONE',  ( -64.49292637653380211, -8.102448949553172852, 5.886773742842742685 ) ) ;
#34217 = LINE ( 'NONE', #50397, #54006 ) ;
#34218 = CARTESIAN_POINT ( 'NONE',  ( 44.70258591656318714, 9.999999999999980460, -3.296040418704463182 ) ) ;
#34219 = AXIS2_PLACEMENT_3D ( 'NONE', #29762, #67057, #2633 ) ;
#34220 = CARTESIAN_POINT ( 'NONE',  ( -8.437984349512095861, 142.8070736234661808, -5.166775262442723748E-16 ) ) ;
#34221 = ORIENTED_EDGE ( 'NONE', *, *, #31682, .F. ) ;
#34222 = CARTESIAN_POINT ( 'NONE',  ( -170.9049999999999727, 2.607480562269069324, -8.024999999999993250 ) ) ;
#34223 =( GEOMETRIC_REPRESENTATION_CONTEXT ( 3 ) GLOBAL_UNCERTAINTY_ASSIGNED_CONTEXT ( ( #24286 ) ) GLOBAL_UNIT_ASSIGNED_CONTEXT ( ( #62426, #68762, #30054 ) ) REPRESENTATION_CONTEXT ( 'NONE', 'WORKASPACE' ) );
#34224 = ORIENTED_EDGE ( 'NONE', *, *, #25336, .F. ) ;
#34225 =( NAMED_UNIT ( * ) SI_UNIT ( $, .STERADIAN. ) SOLID_ANGLE_UNIT ( ) );
#34226 = FILL_AREA_STYLE_COLOUR ( '', #64606 ) ;
#34227 = EDGE_CURVE ( 'NONE', #1278, #48365, #42329, .T. ) ;
#34228 = DIRECTION ( 'NONE',  ( 0.000000000000000000, 0.000000000000000000, 1.000000000000000000 ) ) ;
#34229 = FACE_OUTER_BOUND ( 'NONE', #62981, .T. ) ;
#34230 = CARTESIAN_POINT ( 'NONE',  ( 7.632228543268608334, 156.4570736234661581, -2.479861379858951942 ) ) ;
#34231 = COLOUR_RGB ( '', 0.08235294, 0.09019608, 0.10196078) ;
#34232 = EDGE_CURVE ( 'NONE', #53882, #58067, #21147, .T. ) ;
#34233 = ORIENTED_EDGE ( 'NONE', *, *, #42809, .T. ) ;
#34234 = CARTESIAN_POINT ( 'NONE',  ( 21.02379604162863913, 114.4999999999999574, -10.00000000000000000 ) ) ;
#34235 = CARTESIAN_POINT ( 'NONE',  ( -88.40499999999997272, -2.607480562269069768, 8.024999999999991473 ) ) ;
#34236 = COLOUR_RGB ( '', 0.31764706, 0.68627451, 0.89019608) ;
#34237 = CARTESIAN_POINT ( 'NONE',  ( -7.632228543268607446, 121.6570736234661609, -2.479861379858953718 ) ) ;
#34238 = CARTESIAN_POINT ( 'NONE',  ( -10.01517768586949231, 132.3049999999999500, -6.132527647946036459E-16 ) ) ;
#34239 = UNCERTAINTY_MEASURE_WITH_UNIT (LENGTH_MEASURE( 1.000000000000000082E-05 ), #24472, 'distance_accuracy_value', 'NONE');
#34240 = CARTESIAN_POINT ( 'NONE',  ( -13.25000000000000355, 28.24999999999998934, -3.750000000000000000 ) ) ;
#34241 = CARTESIAN_POINT ( 'NONE',  ( -126.7429263765338163, -5.598654528085803328, -7.705886871421366635 ) ) ;
#34242 = LINE ( 'NONE', #56026, #37704 ) ;
#34243 = ADVANCED_FACE ( 'NONE', ( #43012 ), #54542, .T. ) ;
#34244 = FILL_AREA_STYLE_COLOUR ( '', #66532 ) ;
#34245 = ORIENTED_EDGE ( 'NONE', *, *, #52288, .T. ) ;
#34246 =( NAMED_UNIT ( * ) PLANE_ANGLE_UNIT ( ) SI_UNIT ( $, .RADIAN. ) );
#34247 = SURFACE_STYLE_FILL_AREA ( #66960 ) ;
#34248 = CARTESIAN_POINT ( 'NONE',  ( -50.69499999999998607, -8.437984349512085203, 5.166775262442717831E-16 ) ) ;
#34249 = VERTEX_POINT ( 'NONE', #29176 ) ;
#34250 = SURFACE_STYLE_FILL_AREA ( #13470 ) ;
#34251 = CARTESIAN_POINT ( 'NONE',  ( -45.00000000000000000, 9.656580361551753811, -6.242521039668959659 ) ) ;
#34252 = EDGE_CURVE ( 'NONE', #52169, #5042, #15725, .T. ) ;
#34253 = DIRECTION ( 'NONE',  ( 0.000000000000000000, 1.000000000000000000, -0.000000000000000000 ) ) ;
#34254 = VERTEX_POINT ( 'NONE', #22542 ) ;
#34255 = CARTESIAN_POINT ( 'NONE',  ( -53.84499999999997755, -7.632228543268599452, 2.479861379858951054 ) ) ;
#34256 = ORIENTED_EDGE ( 'NONE', *, *, #2997, .F. ) ;
#34257 = AXIS2_PLACEMENT_3D ( 'NONE', #67148, #18936, #61850 ) ;
#34258 = CARTESIAN_POINT ( 'NONE',  ( -75.00000000000000000, 8.707403661853380328, 5.727618941855547874 ) ) ;
#34259 = CARTESIAN_POINT ( 'NONE',  ( -104.3049999999999784, 8.437984349512085203, -1.550032578732815448E-15 ) ) ;
#34260 = ORIENTED_EDGE ( 'NONE', *, *, #13756, .F. ) ;
#34261 = DIRECTION ( 'NONE',  ( 0.000000000000000000, 0.000000000000000000, 1.000000000000000000 ) ) ;
#34262 = DIRECTION ( 'NONE',  ( 0.000000000000000000, 0.000000000000000000, 1.000000000000000000 ) ) ;
#34263 = PRESENTATION_LAYER_ASSIGNMENT (  '', '', ( #54484 ) ) ;
#34264 = VECTOR ( 'NONE', #39090, 1000.000000000000000 ) ;
#34265 = CARTESIAN_POINT ( 'NONE',  ( -150.0570736234661808, 0.000000000000000000, 9.524999999999991473 ) ) ;
#34266 = COLOUR_RGB ( '', 0.40784314, 0.44705882, 0.49803922) ;
#34267 = LINE ( 'NONE', #45206, #55322 ) ;
#34268 = CARTESIAN_POINT ( 'NONE',  ( 8.102448949553179958, 138.3949999999999818, 5.886773742842750679 ) ) ;
#34269 = CARTESIAN_POINT ( 'NONE',  ( -84.35707362346617799, 5.598654528085804216, 7.705886871421366635 ) ) ;
#34270 = DIRECTION ( 'NONE',  ( 0.000000000000000000, 0.000000000000000000, -1.000000000000000000 ) ) ;
#34271 = SPHERICAL_SURFACE ( 'NONE', #66461, 0.5000000000000000000 ) ;
#34272 = VERTEX_POINT ( 'NONE', #55228 ) ;
#34273 = DIRECTION ( 'NONE',  ( 2.168404344971007882E-16, 0.000000000000000000, 1.000000000000000000 ) ) ;
#34275 = FACE_OUTER_BOUND ( 'NONE', #32585, .T. ) ;
#34274 = DIRECTION ( 'NONE',  ( 0.000000000000000000, 1.000000000000000000, 0.000000000000000000 ) ) ;
#34276 = CIRCLE ( 'NONE', #27516, 0.5000000000000004441 ) ;
#34277 = CARTESIAN_POINT ( 'NONE',  ( -132.0549999999999784, -9.827790563157499189E-16, -8.024999999999991473 ) ) ;
#34278 = DIRECTION ( 'NONE',  ( -0.000000000000000000, 1.000000000000000000, -0.000000000000000000 ) ) ;
#34279 = CARTESIAN_POINT ( 'NONE',  ( -139.6449999999999818, 4.716976649647091513, -6.492361379858946790 ) ) ;
#34280 = CARTESIAN_POINT ( 'NONE',  ( -127.3449999999999847, 7.632228543268599452, -2.479861379858951942 ) ) ;
#34281 = CARTESIAN_POINT ( 'NONE',  ( -36.37589283219813296, -10.39236702006417268, 4.075234830157013377 ) ) ;
#34282 = ORIENTED_EDGE ( 'NONE', *, *, #21255, .F. ) ;
#34283 = CIRCLE ( 'NONE', #15200, 0.5000000000000004441 ) ;
#34284 =( BOUNDED_CURVE ( )  B_SPLINE_CURVE ( 2, ( #22016, #32539, #33934, #38918, #43519, #16754, #54004, #38223, #1873, #55034, #55397 ),
 .UNSPECIFIED., .F., .F. ) 
 B_SPLINE_CURVE_WITH_KNOTS ( ( 3, 2, 2, 2, 2, 3 ),
 ( 0.5760869565217255905, 0.5782608695652037278, 0.5804347826086819762, 0.5826086956521601135, 0.5847826086956383618, 0.5869565217391166101 ),
 .UNSPECIFIED. ) 
 CURVE ( )  GEOMETRIC_REPRESENTATION_ITEM ( )  RATIONAL_B_SPLINE_CURVE ( ( 1.000000000000304867, 0.9510565162948485529, 1.000000000000000000, 0.9510565162951535312, 1.000000000000000000, 0.9510565162951535312, 1.000000000000000000, 0.9510565162951535312, 1.000000000000000000, 0.9510565162954659479, 0.9999999999996875832 ) ) 
 REPRESENTATION_ITEM ( '' )  );
#34285 = ADVANCED_FACE ( 'NONE', ( #50662 ), #6354, .T. ) ;
#34286 = CYLINDRICAL_SURFACE ( 'NONE', #56070, 0.2500000000000002220 ) ;
#34287 = DIRECTION ( 'NONE',  ( -1.000000000000000000, 0.000000000000000000, 0.000000000000000000 ) ) ;
#34288 = DIRECTION ( 'NONE',  ( 1.000000000000000000, 0.000000000000000000, -1.300977106640434891E-16 ) ) ;
#34289 = CIRCLE ( 'NONE', #29806, 0.5000000000000004441 ) ;
#34290 = CARTESIAN_POINT ( 'NONE',  ( -180.8929263765338362, -8.102448949553172852, -5.886773742842741797 ) ) ;
#34291 =( NAMED_UNIT ( * ) PLANE_ANGLE_UNIT ( ) SI_UNIT ( $, .RADIAN. ) );
#34292 = CARTESIAN_POINT ( 'NONE',  ( 27.00000000000001776, 15.00000000000000000, 34.49999999999999289 ) ) ;
#34293 = B_SPLINE_CURVE_WITH_KNOTS ( 'NONE', 3,
 ( #62485, #24843, #35767, #24160 ),
 .UNSPECIFIED., .F., .F.,
 ( 4, 4 ),
 ( 6.735063895479954530E-16, 0.001113530544794672211 ),
 .UNSPECIFIED. ) ;
#34294 = CARTESIAN_POINT ( 'NONE',  ( 0.000000000000000000, 30.74999999999999289, 3.750000000000000000 ) ) ;
#34295 = DIRECTION ( 'NONE',  ( 1.000000000000000000, 0.000000000000000000, 0.000000000000000000 ) ) ;
#34296 = DIRECTION ( 'NONE',  ( 1.000000000000000000, 0.000000000000000000, 0.000000000000000000 ) ) ;
#34297 = CARTESIAN_POINT ( 'NONE',  ( -95.84292637653379643, 9.058813317711329915, -2.943386871421373119 ) ) ;
#34298 = APPLICATION_PROTOCOL_DEFINITION ( 'draft international standard', 'automotive_design', 1998, #37069 ) ;
#34299 = SURFACE_SIDE_STYLE ('',( #61363 ) ) ;
#34300 = AXIS2_PLACEMENT_3D ( 'NONE', #5342, #10987, #6390 ) ;
#34301 = CARTESIAN_POINT ( 'NONE',  ( 0.000000000000000000, 0.000000000000000000, 42.50000000000000000 ) ) ;
#34302 = CIRCLE ( 'NONE', #43357, 0.5000000000000004441 ) ;
#34303 = CARTESIAN_POINT ( 'NONE',  ( 0.000000000000000000, -2.500000000000000000, -3.499999999999997780 ) ) ;
#34304 = SURFACE_SIDE_STYLE ('',( #34635 ) ) ;
#34305 = CARTESIAN_POINT ( 'NONE',  ( -41.01786561352938065, 107.7208547478748528, 3.150777047984529844 ) ) ;
#34306 = EDGE_CURVE ( 'NONE', #2782, #43549, #55000, .T. ) ;
#34307 = MECHANICAL_DESIGN_GEOMETRIC_PRESENTATION_REPRESENTATION (  '', ( #44457 ), #46718 ) ;
#34308 = DIRECTION ( 'NONE',  ( -0.000000000000000000, -0.000000000000000000, 1.000000000000000000 ) ) ;
#34309 = EDGE_CURVE ( 'NONE', #1545, #56168, #26059, .T. ) ;
#34310 = ORIENTED_EDGE ( 'NONE', *, *, #22888, .F. ) ;
#34311 = CARTESIAN_POINT ( 'NONE',  ( 4.041451884327375232, 2.500000000000000000, -7.000000000000002665 ) ) ;
#34313 = ORIENTED_EDGE ( 'NONE', *, *, #12952, .T. ) ;
#34312 = AXIS2_PLACEMENT_3D ( 'NONE', #21238, #4350, #32159 ) ;
#34314 = CARTESIAN_POINT ( 'NONE',  ( -64.19292637653380496, -10.01517768586948698, 6.132527647946031529E-16 ) ) ;
#34315 = PRESENTATION_LAYER_ASSIGNMENT (  '', '', ( #60119 ) ) ;
#34316 = CARTESIAN_POINT ( 'NONE',  ( 4.716976649647099507, 120.7570736234661553, -6.492361379858953008 ) ) ;
#34317 = EDGE_CURVE ( 'NONE', #14638, #3378, #14609, .T. ) ;
#34318 = CARTESIAN_POINT ( 'NONE',  ( -23.21231517720798010, 117.9999999999999716, -10.00000000000000000 ) ) ;
#34319 = CARTESIAN_POINT ( 'NONE',  ( 75.00000000000000000, 19.83714805418753002, -6.873786395979923469 ) ) ;
#34320 = DIRECTION ( 'NONE',  ( 0.000000000000000000, 1.000000000000000000, 0.000000000000000000 ) ) ;
#34321 = VERTEX_POINT ( 'NONE', #55587 ) ;
#34322 = CARTESIAN_POINT ( 'NONE',  ( -93.59292637653493330, -3.094860106637388864, -9.524999999986219379 ) ) ;
#34323 = COLOUR_RGB ( '', 0.40784314, 0.44705882, 0.49803922) ;
#34324 = DIRECTION ( 'NONE',  ( 0.07898106964430656740, 0.9968761159932768567, 0.000000000000000000 ) ) ;
#34325 = DIRECTION ( 'NONE',  ( 0.000000000000000000, 0.000000000000000000, 1.000000000000000000 ) ) ;
#34326 = CARTESIAN_POINT ( 'NONE',  ( 7.000000000000017764, 42.74314482547740113, 27.71473342867655987 ) ) ;
#34327 = CIRCLE ( 'NONE', #66925, 3.500000000000003553 ) ;
#34328 = EDGE_CURVE ( 'NONE', #44609, #33108, #65157, .T. ) ;
#34329 = CARTESIAN_POINT ( 'NONE',  ( -79.19499999999997897, 8.437984349512085203, -1.550032578732815448E-15 ) ) ;
#34330 = EDGE_LOOP ( 'NONE', ( #49083, #48133, #14090 ) ) ;
#34331 = VECTOR ( 'NONE', #3835, 1000.000000000000000 ) ;
#34332 = DIRECTION ( 'NONE',  ( 1.000000000000000000, -0.000000000000000000, 0.000000000000000000 ) ) ;
#34333 = CYLINDRICAL_SURFACE ( 'NONE', #50862, 0.5000000000000000000 ) ;
#34334 = AXIS2_PLACEMENT_3D ( 'NONE', #15628, #5719, #15987 ) ;
#34335 = EDGE_CURVE ( 'NONE', #23161, #20703, #50321, .T. ) ;
#34336 = EDGE_LOOP ( 'NONE', ( #6782, #49995, #51552, #16232 ) ) ;
#34337 = PRESENTATION_STYLE_ASSIGNMENT (( #56476 ) ) ;
#34338 = CARTESIAN_POINT ( 'NONE',  ( -15.98999599679679839, 147.4999999999999716, -9.500000000000000000 ) ) ;
#34339 = ORIENTED_EDGE ( 'NONE', *, *, #60350, .T. ) ;
#34340 = FILL_AREA_STYLE_COLOUR ( '', #35298 ) ;
#34341 = ORIENTED_EDGE ( 'NONE', *, *, #18194, .T. ) ;
#34342 = CARTESIAN_POINT ( 'NONE',  ( 93.00000000000000000, 0.9999999999999991118, 0.000000000000000000 ) ) ;
#34343 = FILL_AREA_STYLE ('',( #45635 ) ) ;
#34344 = CARTESIAN_POINT ( 'NONE',  ( -75.48275862068965125, 36.00832590023089352, -9.500000000000001776 ) ) ;
#34345 = CARTESIAN_POINT ( 'NONE',  ( -182.6070736234661638, -8.102448949553172852, 5.886773742842742685 ) ) ;
#34346 = DIRECTION ( 'NONE',  ( 0.000000000000000000, 0.000000000000000000, 1.000000000000000000 ) ) ;
#34347 = CARTESIAN_POINT ( 'NONE',  ( -3.094860106618434248, 113.7949999999999875, 9.525000000000000355 ) ) ;
#34348 = CARTESIAN_POINT ( 'NONE',  ( -114.9570736234661723, 9.058813317711329915, -2.943386871421373119 ) ) ;
#34349 = VECTOR ( 'NONE', #64560, 1000.000000000000000 ) ;
#34350 = CARTESIAN_POINT ( 'NONE',  ( -74.50000000000001421, 1.735173206890468129E-14, 9.500000000000000000 ) ) ;
#34351 = CARTESIAN_POINT ( 'NONE',  ( -85.25707362346616947, 5.598654528085800663, -7.705886871421367523 ) ) ;
#34352 = ORIENTED_EDGE ( 'NONE', *, *, #30467, .T. ) ;
#34353 = CARTESIAN_POINT ( 'NONE',  ( 0.4644257559287154891, 42.85561152959480324, 45.52242327283500600 ) ) ;
#34354 = DIRECTION ( 'NONE',  ( 1.000000000000000000, 0.000000000000000000, 0.000000000000000000 ) ) ;
#34355 = CARTESIAN_POINT ( 'NONE',  ( -4.500000000000002665, 21.99999999999998579, 4.000000000000000000 ) ) ;
#34357 = DIRECTION ( 'NONE',  ( 0.000000000000000000, -1.000000000000000000, 0.000000000000000000 ) ) ;
#34356 = VECTOR ( 'NONE', #15547, 1000.000000000000000 ) ;
#34358 = EDGE_LOOP ( 'NONE', ( #60498, #60013, #43135, #26102 ) ) ;
#34359 = CARTESIAN_POINT ( 'NONE',  ( -155.0050000000000239, 6.826472737025116366, 4.959722759717898555 ) ) ;
#34360 = DIRECTION ( 'NONE',  ( -1.000000000000000000, 0.000000000000000000, 0.000000000000000000 ) ) ;
#34361 = CARTESIAN_POINT ( 'NONE',  ( -183.6416822935978530, -6.162375212911135769, -6.406072214693263156 ) ) ;
#34362 = CARTESIAN_POINT ( 'NONE',  ( -169.0449999999999875, 7.632228543268600340, 2.479861379858949277 ) ) ;
#34363 = CIRCLE ( 'NONE', #18650, 7.500000000000007105 ) ;
#34364 = CARTESIAN_POINT ( 'NONE',  ( -159.5949999999999989, 2.607480562269072433, 8.024999999999991473 ) ) ;
#34365 = ORIENTED_EDGE ( 'NONE', *, *, #64011, .F. ) ;
#34366 = EDGE_CURVE ( 'NONE', #59038, #55900, #33266, .T. ) ;
#34367 = DIRECTION ( 'NONE',  ( 1.000000000000000000, 8.881784197001252323E-16, 0.000000000000000000 ) ) ;
#34368 = FACE_BOUND ( 'NONE', #47440, .T. ) ;
#34369 = CARTESIAN_POINT ( 'NONE',  ( -77.15499999999998693, 7.632228543268600340, 2.479861379858949277 ) ) ;
#34370 = CARTESIAN_POINT ( 'NONE',  ( -37.13402269541712286, -12.35322054092467425, 1.284749433650013373 ) ) ;
#34371 =( NAMED_UNIT ( * ) PLANE_ANGLE_UNIT ( ) SI_UNIT ( $, .RADIAN. ) );
#34372 = CIRCLE ( 'NONE', #65862, 0.2500000000000002220 ) ;
#34373 = CARTESIAN_POINT ( 'NONE',  ( -71.24499999999999034, -4.716976649647093289, -6.492361379858945902 ) ) ;
#34374 = CARTESIAN_POINT ( 'NONE',  ( -1.166476076187854022E-15, 145.0549999999999784, 9.525000000000000355 ) ) ;
#34375 = CARTESIAN_POINT ( 'NONE',  ( 27.99999999999998934, 5.000000000000000000, -37.00402776293828566 ) ) ;
#34376 = VECTOR ( 'NONE', #57088, 1000.000000000000000 ) ;
#34377 = CARTESIAN_POINT ( 'NONE',  ( 29.00000000000002842, 42.00000000000000000, 80.00402776293826435 ) ) ;
#34378 = AXIS2_PLACEMENT_3D ( 'NONE', #54796, #22824, #65720 ) ;
#34379 = EDGE_CURVE ( 'NONE', #35471, #16364, #35171, .T. ) ;
#34380 = B_SPLINE_CURVE_WITH_KNOTS ( 'NONE', 3,
 ( #55093, #49853, #28708, #50196, #29408, #2639 ),
 .UNSPECIFIED., .F., .F.,
 ( 4, 2, 4 ),
 ( 0.005386537104126977275, 0.008060814333094818568, 0.01073509156206266073 ),
 .UNSPECIFIED. ) ;
#34381 = CARTESIAN_POINT ( 'NONE',  ( 0.000000000000000000, 0.000000000000000000, 0.7500000000000000000 ) ) ;
#34382 = DIRECTION ( 'NONE',  ( 7.080503983578803083E-17, 1.000000000000000000, -0.000000000000000000 ) ) ;
#34383 = EDGE_CURVE ( 'NONE', #63907, #10734, #18917, .T. ) ;
#34384 = EDGE_CURVE ( 'NONE', #65503, #39245, #64009, .T. ) ;
#34385 = CARTESIAN_POINT ( 'NONE',  ( 3.000000000000002665, 38.70020753820971748, -89.00000000000000000 ) ) ;
#34386 = VERTEX_POINT ( 'NONE', #52068 ) ;
#34387 = ORIENTED_EDGE ( 'NONE', *, *, #49723, .T. ) ;
#34388 = FILL_AREA_STYLE_COLOUR ( '', #44305 ) ;
#34389 = CARTESIAN_POINT ( 'NONE',  ( -133.5570736234661808, -1.166476076187852838E-15, -9.524999999999991473 ) ) ;
#34390 = COLOUR_RGB ( '', 0.09019608, 0.27058824, 0.51372549) ;
#34391 = EDGE_CURVE ( 'NONE', #44875, #53696, #14396, .T. ) ;
#34392 = DIRECTION ( 'NONE',  ( 0.000000000000000000, 0.000000000000000000, 1.000000000000000000 ) ) ;
#34393 = LINE ( 'NONE', #29081, #38656 ) ;
#34394 = EDGE_CURVE ( 'NONE', #66538, #29534, #12319, .T. ) ;
#34395 = EDGE_LOOP ( 'NONE', ( #66907, #25076, #12400, #57640, #23172, #52115 ) ) ;
#34396 = ORIENTED_EDGE ( 'NONE', *, *, #31606, .T. ) ;
#34397 = AXIS2_PLACEMENT_3D ( 'NONE', #49931, #38369, #23508 ) ;
#34398 = VERTEX_POINT ( 'NONE', #57675 ) ;
#34399 = CARTESIAN_POINT ( 'NONE',  ( 0.000000000000000000, 113.5549999999999926, -9.525000000000000355 ) ) ;
#34400 = CARTESIAN_POINT ( 'NONE',  ( -20.12916642283592950, 109.9999999999999858, 10.05319148936170137 ) ) ;
#34401 = ORIENTED_EDGE ( 'NONE', *, *, #57909, .T. ) ;
#34402 = COLOUR_RGB ( '', 0.31764706, 0.68627451, 0.89019608) ;
#34403 = LINE ( 'NONE', #35794, #147 ) ;
#34404 = CARTESIAN_POINT ( 'NONE',  ( -122.0949999999999847, -2.607480562269071545, -8.024999999999991473 ) ) ;
#34405 = VERTEX_POINT ( 'NONE', #40137 ) ;
#34406 = EDGE_LOOP ( 'NONE', ( #67816, #13468, #15750, #66317 ) ) ;
#34407 = CARTESIAN_POINT ( 'NONE',  ( -74.08452722063037754, 9.430195807687216103, -6.000000000000000000 ) ) ;
#34408 =( LENGTH_UNIT ( ) NAMED_UNIT ( * ) SI_UNIT ( .MILLI., .METRE. ) );
#34409 = CARTESIAN_POINT ( 'NONE',  ( -10.67256264059687787, -11.73548369089732724, 2.509972884434803930 ) ) ;
#34410 = VERTEX_POINT ( 'NONE', #62927 ) ;
#34411 = CARTESIAN_POINT ( 'NONE',  ( -4.716976649647097730, 144.2429263765338305, -6.492361379858953896 ) ) ;
#34412 = FACE_OUTER_BOUND ( 'NONE', #63419, .T. ) ;
#34413 = FACE_OUTER_BOUND ( 'NONE', #8029, .T. ) ;
#34414 = AXIS2_PLACEMENT_3D ( 'NONE', #55427, #7250, #51204 ) ;
#34415 = CARTESIAN_POINT ( 'NONE',  ( -44.99999999999977973, 146.9999999999999716, -9.500000000000000000 ) ) ;
#34416 = VERTEX_POINT ( 'NONE', #62245 ) ;
#34417 = CARTESIAN_POINT ( 'NONE',  ( 98.00000000000000000, 16.00000000000000000, 0.000000000000000000 ) ) ;
#34418 = EDGE_LOOP ( 'NONE', ( #65460, #31224, #69468, #32658, #43243 ) ) ;
#34419 = CARTESIAN_POINT ( 'NONE',  ( 0.000000000000000000, 154.9999999999999716, 0.000000000000000000 ) ) ;
#34420 = CARTESIAN_POINT ( 'NONE',  ( -20.57648123223228609, 114.5810881445910070, 10.27659574468085246 ) ) ;
#34421 = CARTESIAN_POINT ( 'NONE',  ( -44.99999999999998579, 119.9999999999999716, 10.00000000000000000 ) ) ;
#34422 = CARTESIAN_POINT ( 'NONE',  ( -132.0549999999999784, -9.827790563157499189E-16, -8.024999999999991473 ) ) ;
#34423 = CARTESIAN_POINT ( 'NONE',  ( -25.00000000000000355, 37.00000000000000000, 3.750000000000000000 ) ) ;
#34424 = ADVANCED_FACE ( 'NONE', ( #13356 ), #4165, .T. ) ;
#34425 = LINE ( 'NONE', #44683, #134 ) ;
#34426 = ORIENTED_EDGE ( 'NONE', *, *, #38670, .F. ) ;
#34427 = CARTESIAN_POINT ( 'NONE',  ( -195.0000000000000000, 0.000000000000000000, 0.000000000000000000 ) ) ;
#34428 = DIRECTION ( 'NONE',  ( 0.000000000000000000, -0.6691306063588591257, -0.7431448254773933559 ) ) ;
#34429 = CARTESIAN_POINT ( 'NONE',  ( -45.00000000000000000, 9.519990751839808141, -6.451194676399504502 ) ) ;
#34430 = VERTEX_POINT ( 'NONE', #3823 ) ;
#34431 = ORIENTED_EDGE ( 'NONE', *, *, #5614, .T. ) ;
#34432 = LINE ( 'NONE', #40094, #48610 ) ;
#34433 = DIRECTION ( 'NONE',  ( 0.000000000000000000, 0.000000000000000000, 1.000000000000000000 ) ) ;
#34434 = CARTESIAN_POINT ( 'NONE',  ( -51.05707362346617373, 0.000000000000000000, 9.524999999999991473 ) ) ;
#34435 = FACE_OUTER_BOUND ( 'NONE', #32666, .T. ) ;
#34436 = EDGE_LOOP ( 'NONE', ( #47895, #47984, #7329, #31015, #42290, #66940 ) ) ;
#34437 =( NAMED_UNIT ( * ) SI_UNIT ( $, .STERADIAN. ) SOLID_ANGLE_UNIT ( ) );
#34438 = SURFACE_STYLE_FILL_AREA ( #55894 ) ;
#34439 = CARTESIAN_POINT ( 'NONE',  ( -91.64292637653380780, -5.598654528085801552, 7.705886871421367523 ) ) ;
#34440 = CARTESIAN_POINT ( 'NONE',  ( -34.99999999999992895, 113.4999999999999858, -7.000000000000000000 ) ) ;
#34441 = CARTESIAN_POINT ( 'NONE',  ( 0.000000000000000000, 130.0570736234661524, -8.025000000000000355 ) ) ;
#34442 = PRESENTATION_STYLE_ASSIGNMENT (( #28804 ) ) ;
#34443 = EDGE_LOOP ( 'NONE', ( #24802, #56121, #33819, #56101 ) ) ;
#34444 = DIRECTION ( 'NONE',  ( 9.376883653928687363E-17, 1.000000000000000000, 0.000000000000000000 ) ) ;
#34445 = CARTESIAN_POINT ( 'NONE',  ( 6.826472737025121695, 117.6070736234661638, -4.959722759717905660 ) ) ;
#34446 = CARTESIAN_POINT ( 'NONE',  ( -100.1049999999999898, -6.826472737025115478, 4.959722759717900331 ) ) ;
#34447 = CARTESIAN_POINT ( 'NONE',  ( -54.50000000000002132, -1.956686671034893189E-14, -12.00000000000000000 ) ) ;
#34448 = SURFACE_SIDE_STYLE ('',( #56601 ) ) ;
#34449 = DIRECTION ( 'NONE',  ( 1.000000000000000000, 0.000000000000000000, 0.000000000000000000 ) ) ;
#34450 = CARTESIAN_POINT ( 'NONE',  ( -99.59499999999998465, 2.607480562269072433, 8.024999999999991473 ) ) ;
#34451 = CARTESIAN_POINT ( 'NONE',  ( 8.102448949553183510, 116.1049999999999756, -5.886773742842746238 ) ) ;
#34452 = STYLED_ITEM ( 'NONE', ( #21532 ), #3590 ) ;
#34453 = CARTESIAN_POINT ( 'NONE',  ( -81.89499999999999602, 6.826472737025116366, 4.959722759717898555 ) ) ;
#34454 = EDGE_CURVE ( 'NONE', #28212, #40785, #57281, .T. ) ;
#34455 = CYLINDRICAL_SURFACE ( 'NONE', #431, 1.000000000000000888 ) ;
#34456 = PRESENTATION_LAYER_ASSIGNMENT (  '', '', ( #35627 ) ) ;
#34457 =( NAMED_UNIT ( * ) SI_UNIT ( $, .STERADIAN. ) SOLID_ANGLE_UNIT ( ) );
#34458 = FACE_OUTER_BOUND ( 'NONE', #69057, .T. ) ;
#34459 = PRESENTATION_STYLE_ASSIGNMENT (( #34115 ) ) ;
#34460 = ORIENTED_EDGE ( 'NONE', *, *, #16638, .F. ) ;
#34461 = EDGE_CURVE ( 'NONE', #36214, #67765, #61528, .T. ) ;
#34462 = CARTESIAN_POINT ( 'NONE',  ( -116.0929263765337822, 3.094860106618433360, 9.524999999999991473 ) ) ;
#34463 = CARTESIAN_POINT ( 'NONE',  ( -142.3449999999999989, 7.632228543268599452, -2.479861379858951942 ) ) ;
#34464 = CARTESIAN_POINT ( 'NONE',  ( 32.00000000000000711, 42.00000000000000000, -45.00000000000000000 ) ) ;
#34465 = CIRCLE ( 'NONE', #65951, 0.2500000000000002220 ) ;
#34466 = EDGE_CURVE ( 'NONE', #40838, #61112, #6758, .T. ) ;
#34467 = DIRECTION ( 'NONE',  ( 0.000000000000000000, 1.000000000000000000, -0.000000000000000000 ) ) ;
#34468 = FACE_OUTER_BOUND ( 'NONE', #41389, .T. ) ;
#34469 = CARTESIAN_POINT ( 'NONE',  ( -173.6929263765337907, 10.01517768586948698, -1.839758294383808966E-15 ) ) ;
#34470 = ORIENTED_EDGE ( 'NONE', *, *, #4330, .F. ) ;
#34471 = VERTEX_POINT ( 'NONE', #25637 ) ;
#34472 = DIRECTION ( 'NONE',  ( 0.000000000000000000, -1.000000000000000000, 0.000000000000000000 ) ) ;
#34473 = CYLINDRICAL_SURFACE ( 'NONE', #43217, 0.5000000000000004441 ) ;
#34474 = AXIS2_PLACEMENT_3D ( 'NONE', #26599, #48121, #10794 ) ;
#34475 =( NAMED_UNIT ( * ) PLANE_ANGLE_UNIT ( ) SI_UNIT ( $, .RADIAN. ) );
#34476 = CARTESIAN_POINT ( 'NONE',  ( -130.7070736234668402, -3.094860106629389040, -9.524999999992031618 ) ) ;
#34477 = LINE ( 'NONE', #50663, #54412 ) ;
#34478 = DIRECTION ( 'NONE',  ( 0.000000000000000000, 0.000000000000000000, -1.000000000000000000 ) ) ;
#34479 = EDGE_CURVE ( 'NONE', #34864, #23185, #34816, .T. ) ;
#34480 = ORIENTED_EDGE ( 'NONE', *, *, #44972, .F. ) ;
#34481 = CARTESIAN_POINT ( 'NONE',  ( -130.4050000000000011, -2.607480562269069768, 8.024999999999991473 ) ) ;
#34482 = ORIENTED_EDGE ( 'NONE', *, *, #13711, .F. ) ;
#34483 = EDGE_LOOP ( 'NONE', ( #41678, #25981 ) ) ;
#34484 = CARTESIAN_POINT ( 'NONE',  ( -73.94292637653379074, 0.000000000000000000, 9.524999999999991473 ) ) ;
#34485 =( NAMED_UNIT ( * ) PLANE_ANGLE_UNIT ( ) SI_UNIT ( $, .RADIAN. ) );
#34486 = ORIENTED_EDGE ( 'NONE', *, *, #37221, .F. ) ;
#34487 = DIRECTION ( 'NONE',  ( 0.000000000000000000, 0.000000000000000000, -1.000000000000000000 ) ) ;
#34488 =( NAMED_UNIT ( * ) PLANE_ANGLE_UNIT ( ) SI_UNIT ( $, .RADIAN. ) );
#34489 = CARTESIAN_POINT ( 'NONE',  ( 0.000000000000000000, 142.4449999999999932, -9.525000000000000355 ) ) ;
#34490 =( NAMED_UNIT ( * ) PLANE_ANGLE_UNIT ( ) SI_UNIT ( $, .RADIAN. ) );
#34491 = ORIENTED_EDGE ( 'NONE', *, *, #45078, .T. ) ;
#34492 =( NAMED_UNIT ( * ) PLANE_ANGLE_UNIT ( ) SI_UNIT ( $, .RADIAN. ) );
#34493 = CARTESIAN_POINT ( 'NONE',  ( 3.094860106618431583, 142.2049999999999557, 9.525000000000000355 ) ) ;
#34494 = DIRECTION ( 'NONE',  ( 1.000000000000000000, 0.000000000000000000, 0.000000000000000000 ) ) ;
#34495 = CARTESIAN_POINT ( 'NONE',  ( 30.99999999999999289, 5.000000000000000000, -37.00402776293829277 ) ) ;
#34496 = PRODUCT_DEFINITION_SHAPE ( 'NONE', 'NONE',  #69701 ) ;
#34497 = ORIENTED_EDGE ( 'NONE', *, *, #23142, .T. ) ;
#34498 = CARTESIAN_POINT ( 'NONE',  ( -8.102448949553181734, 159.6050000000000182, 5.886773742842747126 ) ) ;
#34499 = CARTESIAN_POINT ( 'NONE',  ( -8.082903768654762899, 3.516382302766490365E-15, 7.500000000000000000 ) ) ;
#34500 = CARTESIAN_POINT ( 'NONE',  ( -87.89292637653377938, -8.102448949553174629, -5.886773742842741797 ) ) ;
#34501 = PRESENTATION_LAYER_ASSIGNMENT (  '', '', ( #69317 ) ) ;
#34502 = DIRECTION ( 'NONE',  ( 0.000000000000000000, 1.000000000000000000, -0.000000000000000000 ) ) ;
#34503 = CIRCLE ( 'NONE', #57000, 20.42000000000000526 ) ;
#34504 = ORIENTED_EDGE ( 'NONE', *, *, #162, .T. ) ;
#34505 =( LENGTH_UNIT ( ) NAMED_UNIT ( * ) SI_UNIT ( .MILLI., .METRE. ) );
#34506 = EDGE_LOOP ( 'NONE', ( #43358, #29406, #8782, #25082 ) ) ;
#34507 = CARTESIAN_POINT ( 'NONE',  ( -37.74999999999999289, 0.000000000000000000, -5.100000000000000533 ) ) ;
#34508 = FACE_BOUND ( 'NONE', #69320, .T. ) ;
#34509 = DIRECTION ( 'NONE',  ( -1.000000000000000000, -0.000000000000000000, -0.000000000000000000 ) ) ;
#34510 = CARTESIAN_POINT ( 'NONE',  ( -163.2549999999999955, -4.716976649647092401, 6.492361379858946790 ) ) ;
#34511 = ORIENTED_EDGE ( 'NONE', *, *, #59710, .T. ) ;
#34512 = ADVANCED_FACE ( 'NONE', ( #8096 ), #35868, .T. ) ;
#34513 = DIRECTION ( 'NONE',  ( 1.000000000000000000, 0.000000000000000000, 0.000000000000000000 ) ) ;
#34514 = CARTESIAN_POINT ( 'NONE',  ( -15.48999599679679662, 146.9999999999999716, 9.500000000000000000 ) ) ;
#34515 = CARTESIAN_POINT ( 'NONE',  ( 45.00000000000000000, 10.58011009419028881, -6.521986687992749943 ) ) ;
#34516 = ORIENTED_EDGE ( 'NONE', *, *, #18289, .T. ) ;
#34517 = VERTEX_POINT ( 'NONE', #48190 ) ;
#34518 = CIRCLE ( 'NONE', #16583, 19.99999999999998934 ) ;
#34519 = DIRECTION ( 'NONE',  ( -1.000000000000000000, -0.000000000000000000, -0.000000000000000000 ) ) ;
#34520 = CARTESIAN_POINT ( 'NONE',  ( -78.80500000000000682, -8.437984349512085203, 5.166775262442717831E-16 ) ) ;
#34521 = ORIENTED_EDGE ( 'NONE', *, *, #42798, .T. ) ;
#34522 =( NAMED_UNIT ( * ) SI_UNIT ( $, .STERADIAN. ) SOLID_ANGLE_UNIT ( ) );
#34523 = CARTESIAN_POINT ( 'NONE',  ( -64.40707362346617515, 3.094860106618428031, -9.524999999999993250 ) ) ;
#34524 = CARTESIAN_POINT ( 'NONE',  ( -150.8070736234661808, 10.01517768586948698, -1.839758294383808966E-15 ) ) ;
#34525 = CARTESIAN_POINT ( 'NONE',  ( -75.00000000000000000, 7.768687147774687496, -6.500000000000000888 ) ) ;
#34526 = VERTEX_POINT ( 'NONE', #59365 ) ;
#34527 = CARTESIAN_POINT ( 'NONE',  ( -7.511572993685801073E-16, 7.000000000000000888, 0.000000000000000000 ) ) ;
#34529 = CARTESIAN_POINT ( 'NONE',  ( 30.75000000000001066, 16.24999999999997513, -3.750000000000000000 ) ) ;
#34528 = CARTESIAN_POINT ( 'NONE',  ( -52.70707362346615099, -3.094860106618431139, -9.524999999999991473 ) ) ;
#34530 = CARTESIAN_POINT ( 'NONE',  ( 0.000000000000000000, 136.4449999999999932, -9.525000000000000355 ) ) ;
#34531 = CARTESIAN_POINT ( 'NONE',  ( -103.1950000000000074, 8.437984349512085203, -1.550032578732815448E-15 ) ) ;
#34532 = EDGE_CURVE ( 'NONE', #44642, #49404, #42924, .T. ) ;
#34533 = CARTESIAN_POINT ( 'NONE',  ( 54.50000000000002132, 1.797044900979284448E-15, -12.00000000000000000 ) ) ;
#34535 = CARTESIAN_POINT ( 'NONE',  ( -19.82863456809962344, 11.92953265915295624, 1.308243074720540022 ) ) ;
#34534 = DIRECTION ( 'NONE',  ( 0.000000000000000000, 1.000000000000000000, 0.000000000000000000 ) ) ;
#34536 = CARTESIAN_POINT ( 'NONE',  ( -144.5929263765337964, -3.094860106618431139, -9.524999999999991473 ) ) ;
#34537 =( NAMED_UNIT ( * ) SI_UNIT ( $, .STERADIAN. ) SOLID_ANGLE_UNIT ( ) );
#34538 = CARTESIAN_POINT ( 'NONE',  ( -165.7450000000000045, 4.716976649647094177, 6.492361379858945902 ) ) ;
#34539 =( GEOMETRIC_REPRESENTATION_CONTEXT ( 3 ) GLOBAL_UNCERTAINTY_ASSIGNED_CONTEXT ( ( #3082 ) ) GLOBAL_UNIT_ASSIGNED_CONTEXT ( ( #5851, #57968, #15756 ) ) REPRESENTATION_CONTEXT ( 'NONE', 'WORKASPACE' ) );
#34540 = TOROIDAL_SURFACE ( 'NONE', #53628, 0.5000000000000000000, 0.2500000000000000000 ) ;
#34541 = EDGE_CURVE ( 'NONE', #66756, #5601, #39391, .T. ) ;
#34542 = AXIS2_PLACEMENT_3D ( 'NONE', #60116, #66427, #66074 ) ;
#34543 = DIRECTION ( 'NONE',  ( -1.000000000000000000, -0.000000000000000000, -0.000000000000000000 ) ) ;
#34544 = DIRECTION ( 'NONE',  ( 0.000000000000000000, 0.000000000000000000, -1.000000000000000000 ) ) ;
#34545 = ORIENTED_EDGE ( 'NONE', *, *, #67393, .T. ) ;
#34546 = DIRECTION ( 'NONE',  ( 1.000000000000000000, 0.000000000000000000, 0.000000000000000000 ) ) ;
#34547 = VERTEX_POINT ( 'NONE', #20374 ) ;
#34548 = ADVANCED_FACE ( 'NONE', ( #58707 ), #48538, .F. ) ;
#34549 = SURFACE_STYLE_USAGE ( .BOTH. , #30289 ) ;
#34550 = ADVANCED_FACE ( 'NONE', ( #42247 ), #53761, .T. ) ;
#34551 = DIRECTION ( 'NONE',  ( 1.982541115402069054E-16, 0.000000000000000000, -1.000000000000000000 ) ) ;
#34552 = CARTESIAN_POINT ( 'NONE',  ( 2.607480562269118174, 147.9070736234661467, -8.024999999999970157 ) ) ;
#34553 = CARTESIAN_POINT ( 'NONE',  ( 108.3664351561509278, 14.00000000000000000, 18.43563588791581154 ) ) ;
#34554 = AXIS2_PLACEMENT_3D ( 'NONE', #34976, #67332, #51496 ) ;
#34555 = CARTESIAN_POINT ( 'NONE',  ( -6.826472737025120807, 142.5070736234661410, -4.959722759717907437 ) ) ;
#34556 = EDGE_CURVE ( 'NONE', #69397, #43530, #46120, .T. ) ;
#34557 = ORIENTED_EDGE ( 'NONE', *, *, #58090, .F. ) ;
#34558 = CARTESIAN_POINT ( 'NONE',  ( -162.9549999999999841, -7.632228543268599452, 2.479861379858951054 ) ) ;
#34559 = ORIENTED_EDGE ( 'NONE', *, *, #69029, .F. ) ;
#34560 = CARTESIAN_POINT ( 'NONE',  ( -19.89974874213240597, 115.4999999999999574, -10.00000000000000000 ) ) ;
#34561 = LINE ( 'NONE', #7148, #55563 ) ;
#34562 =( NAMED_UNIT ( * ) PLANE_ANGLE_UNIT ( ) SI_UNIT ( $, .RADIAN. ) );
#34563 = DIRECTION ( 'NONE',  ( 0.000000000000000000, 1.000000000000000000, 0.000000000000000000 ) ) ;
#34564 = CARTESIAN_POINT ( 'NONE',  ( 0.000000000000000000, 112.4449999999999932, -9.525000000000000355 ) ) ;
#34565 = VERTEX_POINT ( 'NONE', #17871 ) ;
#34566 = DIRECTION ( 'NONE',  ( 1.156482317317873451E-16, -1.000000000000000000, -0.000000000000000000 ) ) ;
#34567 = CARTESIAN_POINT ( 'NONE',  ( -82.40499999999998693, -2.607480562269069768, 8.024999999999991473 ) ) ;
#34568 = CARTESIAN_POINT ( 'NONE',  ( -195.0000000000000000, 1.166476076187852838E-15, -9.524999999999991473 ) ) ;
#34569 = CARTESIAN_POINT ( 'NONE',  ( 8.102448949553183510, 128.1049999999999898, -5.886773742842746238 ) ) ;
#34570 =( NAMED_UNIT ( * ) SI_UNIT ( $, .STERADIAN. ) SOLID_ANGLE_UNIT ( ) );
#34571 =( LENGTH_UNIT ( ) NAMED_UNIT ( * ) SI_UNIT ( .MILLI., .METRE. ) );
#34572 = CARTESIAN_POINT ( 'NONE',  ( 20.56347600517836938, 115.3187862480272372, 10.00000000000000000 ) ) ;
#34573 = CARTESIAN_POINT ( 'NONE',  ( 71.50000000000000000, 35.92875272052971525, -7.500000000000000000 ) ) ;
#34574 = VERTEX_POINT ( 'NONE', #6593 ) ;
#34575 = FACE_OUTER_BOUND ( 'NONE', #30844, .T. ) ;
#34576 = CARTESIAN_POINT ( 'NONE',  ( -54.29499999999998749, -2.607480562269069768, 8.024999999999991473 ) ) ;
#34577 = ORIENTED_EDGE ( 'NONE', *, *, #18955, .F. ) ;
#34578 =( BOUNDED_CURVE ( )  B_SPLINE_CURVE ( 2, ( #56504, #45308, #29422, #66728, #18545, #40032, #8340, #13237, #2655, #61761, #13590 ),
 .UNSPECIFIED., .F., .F. ) 
 B_SPLINE_CURVE_WITH_KNOTS ( ( 3, 2, 2, 2, 2, 3 ),
 ( 0.4456521739130328563, 0.4478260869565111046, 0.4499999999999892975, 0.4521739130434675458, 0.4543478260869457386, 0.4565217391304239314 ),
 .UNSPECIFIED. ) 
 CURVE ( )  GEOMETRIC_REPRESENTATION_ITEM ( )  RATIONAL_B_SPLINE_CURVE ( ( 1.000000000000238698, 0.9510565162949148332, 1.000000000000000000, 0.9510565162951535312, 1.000000000000000000, 0.9510565162951535312, 1.000000000000000000, 0.9510565162951535312, 1.000000000000000000, 0.9510565162953972251, 0.9999999999997563060 ) ) 
 REPRESENTATION_ITEM ( '' )  );
#34579 = CARTESIAN_POINT ( 'NONE',  ( -69.99999999999998579, 50.00000000000000000, -12.00000000000000000 ) ) ;
#34580 = CARTESIAN_POINT ( 'NONE',  ( 82.09357085539566867, 0.000000000000000000, -37.00402776293823592 ) ) ;
#34581 = LINE ( 'NONE', #66613, #27399 ) ;
#34582 = PRESENTATION_LAYER_ASSIGNMENT (  '', '', ( #6459 ) ) ;
#34583 = CARTESIAN_POINT ( 'NONE',  ( 16.75000000000000711, 27.99999999999998224, 4.000000000000000000 ) ) ;
#34584 = VERTEX_POINT ( 'NONE', #11895 ) ;
#34585 = CARTESIAN_POINT ( 'NONE',  ( -50.54499999999998039, -7.632228543268600340, -2.479861379858950166 ) ) ;
#34586 = ORIENTED_EDGE ( 'NONE', *, *, #36440, .F. ) ;
#34587 = MECHANICAL_DESIGN_GEOMETRIC_PRESENTATION_REPRESENTATION (  '', ( #39104 ), #60392 ) ;
#34588 = PRESENTATION_LAYER_ASSIGNMENT (  '', '', ( #4236 ) ) ;
#34589 = CARTESIAN_POINT ( 'NONE',  ( -75.00000000000000000, 8.700918745341546412, 5.871692373102170848 ) ) ;
#34590 = CARTESIAN_POINT ( 'NONE',  ( -104.6050000000000040, 6.826472737025113702, -4.959722759717902107 ) ) ;
#34591 = EDGE_LOOP ( 'NONE', ( #10265, #9860, #2075, #47107 ) ) ;
#34592 = DIRECTION ( 'NONE',  ( 0.000000000000000000, 1.000000000000000000, 1.156482317317871478E-16 ) ) ;
#34593 = FACE_OUTER_BOUND ( 'NONE', #49247, .T. ) ;
#34594 = DIRECTION ( 'NONE',  ( -1.000000000000000000, 0.000000000000000000, 0.000000000000000000 ) ) ;
#34595 = AXIS2_PLACEMENT_3D ( 'NONE', #10077, #57565, #52319 ) ;
#34596 = CARTESIAN_POINT ( 'NONE',  ( -139.2570736234661695, 5.598654528085800663, -7.705886871421367523 ) ) ;
#34597 = SURFACE_STYLE_USAGE ( .BOTH. , #13142 ) ;
#34598 = CARTESIAN_POINT ( 'NONE',  ( -1.166476076187854022E-15, 143.9449999999999932, 9.525000000000000355 ) ) ;
#34599 = CARTESIAN_POINT ( 'NONE',  ( -80.45707362346617231, -9.058813317711329915, 2.943386871421371787 ) ) ;
#34600 = CARTESIAN_POINT ( 'NONE',  ( -95.54292637653379927, 9.058813317711329915, 2.943386871421369566 ) ) ;
#34601 = PRESENTATION_LAYER_ASSIGNMENT (  '', '', ( #9927 ) ) ;
#34603 = DIRECTION ( 'NONE',  ( 0.000000000000000000, 1.000000000000000000, 0.000000000000000000 ) ) ;
#34602 = CARTESIAN_POINT ( 'NONE',  ( 4.716976649647096842, 119.8570736234661638, 6.492361379858953896 ) ) ;
#34604 = CARTESIAN_POINT ( 'NONE',  ( -123.3549999999999898, -4.716976649647093289, -6.492361379858945902 ) ) ;
#34605 = FACE_OUTER_BOUND ( 'NONE', #4274, .T. ) ;
#34606 = DIRECTION ( 'NONE',  ( -0.000000000000000000, -1.000000000000000000, 0.000000000000000000 ) ) ;
#34607 = CARTESIAN_POINT ( 'NONE',  ( -8.102448949553181734, 113.4949999999999619, 5.886773742842747126 ) ) ;
#34608 = CARTESIAN_POINT ( 'NONE',  ( -135.2950000000000159, -2.607480562269069768, 8.024999999999991473 ) ) ;
#34609 = ADVANCED_FACE ( 'NONE', ( #39356 ), #5639, .F. ) ;
#34610 = CARTESIAN_POINT ( 'NONE',  ( -122.6949999999999790, -8.437984349512086979, 5.166775262442717831E-16 ) ) ;
#34611 = CARTESIAN_POINT ( 'NONE',  ( 19.00000000000000000, 8.000000000000000000, 3.500000000000003997 ) ) ;
#34612 = ORIENTED_EDGE ( 'NONE', *, *, #49261, .F. ) ;
#34613 = ADVANCED_FACE ( 'NONE', ( #55133 ), #18213, .F. ) ;
#34615 = EDGE_CURVE ( 'NONE', #42104, #63360, #1956, .T. ) ;
#34614 = FILL_AREA_STYLE ('',( #7891 ) ) ;
#34616 = CARTESIAN_POINT ( 'NONE',  ( -121.0429263765337993, -9.058813317711329915, -2.943386871421370898 ) ) ;
#34617 = CARTESIAN_POINT ( 'NONE',  ( -177.7429263765338021, -5.598654528085803328, -7.705886871421366635 ) ) ;
#34618 = PRESENTATION_STYLE_ASSIGNMENT (( #28983 ) ) ;
#34619 = CARTESIAN_POINT ( 'NONE',  ( -48.89499999999999602, 6.826472737025116366, 4.959722759717898555 ) ) ;
#34620 = EDGE_CURVE ( 'NONE', #49461, #1044, #68592, .T. ) ;
#34621 = ADVANCED_FACE ( 'NONE', ( #59736 ), #49202, .T. ) ;
#34622 = DIRECTION ( 'NONE',  ( 1.000000000000000000, 0.000000000000000000, -1.300977106640434891E-16 ) ) ;
#34623 = DIRECTION ( 'NONE',  ( 1.000000000000000000, -0.000000000000000000, 0.000000000000000000 ) ) ;
#34624 = ADVANCED_BREP_SHAPE_REPRESENTATION ( '', ( #50492, #42840 ), #53979 ) ;
#34625 = EDGE_CURVE ( 'NONE', #63373, #54365, #31439, .T. ) ;
#34626 = AXIS2_PLACEMENT_3D ( 'NONE', #54879, #23577, #59834 ) ;
#34627 = DIRECTION ( 'NONE',  ( 1.000000000000000000, 0.000000000000000000, 0.000000000000000000 ) ) ;
#34628 = DIRECTION ( 'NONE',  ( 1.000000000000000000, 0.000000000000000000, 0.000000000000000000 ) ) ;
#34629 = CARTESIAN_POINT ( 'NONE',  ( -97.79292637653381348, -3.094860106618429807, 9.524999999999991473 ) ) ;
#34630 = PRODUCT_CONTEXT ( 'NONE', #51410, 'mechanical' ) ;
#34631 = COLOUR_RGB ( '', 0.08235294, 0.09019608, 0.10196078) ;
#34632 = SURFACE_STYLE_USAGE ( .BOTH. , #34299 ) ;
#34633 = DIRECTION ( 'NONE',  ( 1.000000000000000000, -0.000000000000000000, 0.000000000000000000 ) ) ;
#34634 = ADVANCED_FACE ( 'NONE', ( #3647 ), #10019, .T. ) ;
#34635 = SURFACE_STYLE_FILL_AREA ( #33602 ) ;
#34636 = CIRCLE ( 'NONE', #42519, 0.5000000000000004441 ) ;
#34637 = AXIS2_PLACEMENT_3D ( 'NONE', #105, #32897, #54333 ) ;
#34638 = EDGE_LOOP ( 'NONE', ( #7291, #7687, #31919, #48319 ) ) ;
#34639 = DIRECTION ( 'NONE',  ( 1.000000000000000000, -0.000000000000000000, 0.000000000000000000 ) ) ;
#34640 = DIRECTION ( 'NONE',  ( -0.000000000000000000, 1.000000000000000000, -0.000000000000000000 ) ) ;
#34641 = ORIENTED_EDGE ( 'NONE', *, *, #13990, .F. ) ;
#34642 = CARTESIAN_POINT ( 'NONE',  ( 0.000000000000000000, 0.000000000000000000, 0.7500000000000000000 ) ) ;
#34643 = MECHANICAL_DESIGN_GEOMETRIC_PRESENTATION_REPRESENTATION (  '', ( #29004 ), #6511 ) ;
#34644 = CARTESIAN_POINT ( 'NONE',  ( 4.716976649647099507, 126.7570736234661695, -6.492361379858953008 ) ) ;
#34645 = AXIS2_PLACEMENT_3D ( 'NONE', #68871, #41814, #63231 ) ;
#34646 =( NAMED_UNIT ( * ) SI_UNIT ( $, .STERADIAN. ) SOLID_ANGLE_UNIT ( ) );
#34647 = DIRECTION ( 'NONE',  ( 1.000000000000000000, -0.000000000000000000, 0.000000000000000000 ) ) ;
#34648 = VERTEX_POINT ( 'NONE', #4342 ) ;
#34649 = FILL_AREA_STYLE_COLOUR ( '', #7354 ) ;
#34650 = DIRECTION ( 'NONE',  ( 1.000000000000000000, -0.000000000000000000, 0.000000000000000000 ) ) ;
#34651 = FILL_AREA_STYLE ('',( #18824 ) ) ;
#34652 = SPHERICAL_SURFACE ( 'NONE', #51961, 0.2500000000000000000 ) ;
#34653 = CARTESIAN_POINT ( 'NONE',  ( -80.24499999999997613, -4.716976649647093289, -6.492361379858945902 ) ) ;
#34654 = ORIENTED_EDGE ( 'NONE', *, *, #56396, .T. ) ;
#34655 = EDGE_CURVE ( 'NONE', #67791, #38837, #4012, .T. ) ;
#34656 =( LENGTH_UNIT ( ) NAMED_UNIT ( * ) SI_UNIT ( .MILLI., .METRE. ) );
#34657 = CYLINDRICAL_SURFACE ( 'NONE', #8355, 17.99999999999999645 ) ;
#34658 = AXIS2_PLACEMENT_3D ( 'NONE', #5276, #37359, #10240 ) ;
#34659 = UNCERTAINTY_MEASURE_WITH_UNIT (LENGTH_MEASURE( 1.000000000000000082E-05 ), #17556, 'distance_accuracy_value', 'NONE');
#34660 = ORIENTED_EDGE ( 'NONE', *, *, #26819, .T. ) ;
#34661 = CARTESIAN_POINT ( 'NONE',  ( -76.34292637653379643, -9.058813317711329915, 2.943386871421371787 ) ) ;
#34662 =( LENGTH_UNIT ( ) NAMED_UNIT ( * ) SI_UNIT ( .MILLI., .METRE. ) );
#34663 = CONICAL_SURFACE ( 'NONE', #896, 5.500000000000005329, 0.7853981633974309595 ) ;
#34664 = CARTESIAN_POINT ( 'NONE',  ( -2.448909842207114274, 50.66868219381804295, -7.156559940361793437 ) ) ;
#34665 = VERTEX_POINT ( 'NONE', #42074 ) ;
#34666 = FACE_OUTER_BOUND ( 'NONE', #33317, .T. ) ;
#34667 = ORIENTED_EDGE ( 'NONE', *, *, #21544, .T. ) ;
#34669 = CARTESIAN_POINT ( 'NONE',  ( -136.9429263765338192, 0.000000000000000000, 9.524999999999991473 ) ) ;
#34668 =( GEOMETRIC_REPRESENTATION_CONTEXT ( 3 ) GLOBAL_UNCERTAINTY_ASSIGNED_CONTEXT ( ( #52600 ) ) GLOBAL_UNIT_ASSIGNED_CONTEXT ( ( #22081, #44621, #43581 ) ) REPRESENTATION_CONTEXT ( 'NONE', 'WORKASPACE' ) );
#34670 = DIRECTION ( 'NONE',  ( 1.000000000000000000, 0.000000000000000000, 0.000000000000000000 ) ) ;
#34671 = CARTESIAN_POINT ( 'NONE',  ( 27.99999999999999645, 5.000000000000000000, -72.00402776293822171 ) ) ;
#34672 = CIRCLE ( 'NONE', #31311, 4.999999999999997335 ) ;
#34673 = CARTESIAN_POINT ( 'NONE',  ( -177.0570736234661808, 0.000000000000000000, 9.524999999999991473 ) ) ;
#34674 = CARTESIAN_POINT ( 'NONE',  ( -11.54296011127659050, 55.11956624581093678, -6.687176662279907369 ) ) ;
#34675 = CARTESIAN_POINT ( 'NONE',  ( 8.102448949553179958, 117.3949999999999818, 5.886773742842750679 ) ) ;
#34676 = COLOUR_RGB ( '', 0.40784314, 0.44705882, 0.49803922) ;
#34677 =( BOUNDED_SURFACE ( )  B_SPLINE_SURFACE ( 3, 2, ( 
 ( #38021, #38378, #630 ),
 ( #53798, #64368, #22150 ),
 ( #27736, #59409, #32344 ),
 ( #69312, #16217, #26381 ),
 ( #43646, #5600, #27046 ),
 ( #11242, #280, #65039 ),
 ( #944, #11589, #4928 ),
 ( #33061, #48227, #6306 ) ),
 .UNSPECIFIED., .F., .F., .F. ) 
 B_SPLINE_SURFACE_WITH_KNOTS ( ( 4, 2, 2, 4 ),
 ( 3, 3 ),
 ( 0.0005765750791842491792, 0.001029553238931483865, 0.001482531398678718334, 0.002388487718173187488 ),
 ( 0.000000000000000000, 1.000000000000000000 ),
 .UNSPECIFIED. ) 
 GEOMETRIC_REPRESENTATION_ITEM ( )  RATIONAL_B_SPLINE_SURFACE ( (
 ( 1.000000000000000000, 0.8885233166386380388, 1.000000000000000000),
 ( 1.000000000000000000, 0.8885760224879465374, 1.000000000000000000),
 ( 1.000000000000000000, 0.8838232350071849597, 1.000000000000000000),
 ( 1.000000000000000000, 0.8662144792540281690, 1.000000000000000000),
 ( 1.000000000000000000, 0.8532605865699290915, 1.000000000000000000),
 ( 1.000000000000000000, 0.8046051514202448018, 1.000000000000000000),
 ( 1.000000000000000000, 0.7601637718248979159, 1.000000000000000000),
 ( 1.000000000000000000, 0.7071067811865546782, 1.000000000000000000) ) ) 
 REPRESENTATION_ITEM ( '' )  SURFACE ( )  );
#34678 = CARTESIAN_POINT ( 'NONE',  ( -108.8070736234661666, 10.01517768586948698, -1.839758294383808571E-15 ) ) ;
#34679 = SURFACE_STYLE_FILL_AREA ( #44607 ) ;
#34680 = CARTESIAN_POINT ( 'NONE',  ( 16.00000000000001776, 15.00000000000000000, 29.68999999999999417 ) ) ;
#34681 = ORIENTED_EDGE ( 'NONE', *, *, #25746, .F. ) ;
#34682 = CARTESIAN_POINT ( 'NONE',  ( 0.000000000000000000, 1.408343819019453020E-15, -10.99999999999995381 ) ) ;
#34683 = CARTESIAN_POINT ( 'NONE',  ( 44.91886116991580735, 9.999999999999980460, -3.201362207699240514 ) ) ;
#34684 = DIRECTION ( 'NONE',  ( 0.000000000000000000, 1.000000000000000000, 0.000000000000000000 ) ) ;
#34685 = CARTESIAN_POINT ( 'NONE',  ( -148.8549999999999898, 4.716976649647094177, 6.492361379858945902 ) ) ;
#34686 = ADVANCED_FACE ( 'NONE', ( #57502 ), #36060, .T. ) ;
#34687 =( NAMED_UNIT ( * ) PLANE_ANGLE_UNIT ( ) SI_UNIT ( $, .RADIAN. ) );
#34688 = CARTESIAN_POINT ( 'NONE',  ( 28.00000000000002842, 38.00000000000000711, 90.00000000000000000 ) ) ;
#34689 = CARTESIAN_POINT ( 'NONE',  ( -166.4950000000000045, 6.826472737025113702, -4.959722759717902107 ) ) ;
#34690 = CIRCLE ( 'NONE', #5449, 0.5000000000000004441 ) ;
#34691 = CARTESIAN_POINT ( 'NONE',  ( -159.8950000000000102, 6.826472737025115478, 4.959722759717899443 ) ) ;
#34692 = EDGE_LOOP ( 'NONE', ( #54639, #46229 ) ) ;
#34693 = ADVANCED_FACE ( 'NONE', ( #47338 ), #1728, .F. ) ;
#34694 = CARTESIAN_POINT ( 'NONE',  ( 48.74999999999999289, 24.74999999999998579, 4.000000000000000000 ) ) ;
#34695 = DIRECTION ( 'NONE',  ( -1.000000000000000000, -0.000000000000000000, -0.000000000000000000 ) ) ;
#34696 = CARTESIAN_POINT ( 'NONE',  ( -70.25499999999998124, -4.716976649647092401, 6.492361379858946790 ) ) ;
#34697 = CARTESIAN_POINT ( 'NONE',  ( -34.68069995552857421, -10.68067889009693872, 2.165721509536973954 ) ) ;
#34699 = CARTESIAN_POINT ( 'NONE',  ( -167.5429263765338135, 9.058813317711329915, 2.943386871421369566 ) ) ;
#34698 = AXIS2_PLACEMENT_3D ( 'NONE', #63599, #31930, #42532 ) ;
#34700 = CARTESIAN_POINT ( 'NONE',  ( -72.59499999999998465, 2.607480562269072433, 8.024999999999991473 ) ) ;
#34701 = CARTESIAN_POINT ( 'NONE',  ( -3.094860106618432471, 149.7049999999999272, -9.525000000000000355 ) ) ;
#34702 = DIRECTION ( 'NONE',  ( -0.000000000000000000, -1.000000000000000000, -0.000000000000000000 ) ) ;
#34703 = ADVANCED_FACE ( 'NONE', ( #4083 ), #28121, .F. ) ;
#34704 = UNCERTAINTY_MEASURE_WITH_UNIT (LENGTH_MEASURE( 1.000000000000000082E-05 ), #46340, 'distance_accuracy_value', 'NONE');
#34705 = FACE_OUTER_BOUND ( 'NONE', #11532, .T. ) ;
#34706 =( NAMED_UNIT ( * ) SI_UNIT ( $, .STERADIAN. ) SOLID_ANGLE_UNIT ( ) );
#34707 = EDGE_CURVE ( 'NONE', #33857, #16450, #50658, .T. ) ;
#34708 = SURFACE_STYLE_FILL_AREA ( #19919 ) ;
#34709 = DIRECTION ( 'NONE',  ( 0.000000000000000000, 0.000000000000000000, -1.000000000000000000 ) ) ;
#34710 = AXIS2_PLACEMENT_3D ( 'NONE', #34694, #18542, #30106 ) ;
#34711 = CARTESIAN_POINT ( 'NONE',  ( -9.827790563157511022E-16, 116.5570736234661666, 8.025000000000000355 ) ) ;
#34712 = ORIENTED_EDGE ( 'NONE', *, *, #52356, .T. ) ;
#34713 = AXIS2_PLACEMENT_3D ( 'NONE', #2314, #50931, #23840 ) ;
#34714 = ORIENTED_EDGE ( 'NONE', *, *, #61104, .T. ) ;
#34715 =( NAMED_UNIT ( * ) PLANE_ANGLE_UNIT ( ) SI_UNIT ( $, .RADIAN. ) );
#34716 = AXIS2_PLACEMENT_3D ( 'NONE', #63197, #30120, #68138 ) ;
#34717 = LINE ( 'NONE', #64762, #7981 ) ;
#34718 = CARTESIAN_POINT ( 'NONE',  ( -44.99999999999999289, 9.585601099689366578, 6.373959028214387423 ) ) ;
#34719 = DIRECTION ( 'NONE',  ( 0.000000000000000000, -1.224646799147353454E-16, 1.000000000000000000 ) ) ;
#34720 = EDGE_LOOP ( 'NONE', ( #11479, #38852, #47297, #5305 ) ) ;
#34721 = ORIENTED_EDGE ( 'NONE', *, *, #28980, .F. ) ;
#34722 = DIRECTION ( 'NONE',  ( -1.000000000000000000, 0.000000000000000000, 0.000000000000000000 ) ) ;
#34723 = CYLINDRICAL_SURFACE ( 'NONE', #55601, 0.2500000000000002220 ) ;
#34724 = EDGE_LOOP ( 'NONE', ( #32977, #52379, #2537, #28525 ) ) ;
#34725 = CARTESIAN_POINT ( 'NONE',  ( -145.7929263765342967, -3.094860106610362926, 9.525000000005851675 ) ) ;
#34726 = ORIENTED_EDGE ( 'NONE', *, *, #9867, .T. ) ;
#34727 = AXIS2_PLACEMENT_3D ( 'NONE', #29691, #3975, #67672 ) ;
#34728 = B_SPLINE_CURVE_WITH_KNOTS ( 'NONE', 3,
 ( #48805, #22369, #44572, #1888, #23077, #60000 ),
 .UNSPECIFIED., .F., .F.,
 ( 4, 2, 4 ),
 ( 0.000000000000000000, 0.0004110251708232767233, 0.0008220503416465534466 ),
 .UNSPECIFIED. ) ;
#34729 = FACE_OUTER_BOUND ( 'NONE', #21454, .T. ) ;
#34730 = CARTESIAN_POINT ( 'NONE',  ( -107.8449999999999989, -7.632228543268599452, 2.479861379858951054 ) ) ;
#34731 = VERTEX_POINT ( 'NONE', #12309 ) ;
#34732 = VECTOR ( 'NONE', #2991, 1000.000000000000000 ) ;
#34733 = ADVANCED_FACE ( 'NONE', ( #52334 ), #47708, .F. ) ;
#34734 = EDGE_LOOP ( 'NONE', ( #46734, #37158, #29638, #29320 ) ) ;
#34735 =( REPRESENTATION_RELATIONSHIP ('NONE','NONE', #5102, #21747 ) REPRESENTATION_RELATIONSHIP_WITH_TRANSFORMATION ( #14575 )SHAPE_REPRESENTATION_RELATIONSHIP( ) );
#34736 = CARTESIAN_POINT ( 'NONE',  ( -1.751052283315748914, 110.4999999999999432, -9.372962259333457169 ) ) ;
#34737 = CARTESIAN_POINT ( 'NONE',  ( -10.25964068305781041, -11.89358858517478446, -1.623775006699102130 ) ) ;
#34738 = FACE_OUTER_BOUND ( 'NONE', #45512, .T. ) ;
#34739 = ORIENTED_EDGE ( 'NONE', *, *, #30097, .F. ) ;
#34740 = CARTESIAN_POINT ( 'NONE',  ( -4.716976649647098618, 142.1429263765338078, 6.492361379858953008 ) ) ;
#34741 =( NAMED_UNIT ( * ) PLANE_ANGLE_UNIT ( ) SI_UNIT ( $, .RADIAN. ) );
#34742 =( NAMED_UNIT ( * ) SI_UNIT ( $, .STERADIAN. ) SOLID_ANGLE_UNIT ( ) );
#34743 = VECTOR ( 'NONE', #18456, 1000.000000000000000 ) ;
#34744 = CARTESIAN_POINT ( 'NONE',  ( 6.999798566743339556, 49.77026365512251971, 12.50000000000000000 ) ) ;
#34745 = ORIENTED_EDGE ( 'NONE', *, *, #55340, .F. ) ;
#34746 = LINE ( 'NONE', #45366, #54257 ) ;
#34747 = VERTEX_POINT ( 'NONE', #37208 ) ;
#34748 = PRESENTATION_STYLE_ASSIGNMENT (( #66788 ) ) ;
#34749 = CARTESIAN_POINT ( 'NONE',  ( 74.49999999999998579, 119.9999999999997584, 10.00000000000000000 ) ) ;
#34750 = DIRECTION ( 'NONE',  ( 0.000000000000000000, 0.000000000000000000, -1.000000000000000000 ) ) ;
#34751 = DIRECTION ( 'NONE',  ( 1.000000000000000000, 0.000000000000000000, 0.000000000000000000 ) ) ;
#34752 = CARTESIAN_POINT ( 'NONE',  ( -134.6050000000000182, 6.826472737025113702, -4.959722759717902107 ) ) ;
#34753 = DIRECTION ( 'NONE',  ( 1.000000000000000000, -0.000000000000000000, -0.000000000000000000 ) ) ;
#34754 =( GEOMETRIC_REPRESENTATION_CONTEXT ( 3 ) GLOBAL_UNCERTAINTY_ASSIGNED_CONTEXT ( ( #4449 ) ) GLOBAL_UNIT_ASSIGNED_CONTEXT ( ( #34662, #51214, #35023 ) ) REPRESENTATION_CONTEXT ( 'NONE', 'WORKASPACE' ) );
#34755 = PRESENTATION_LAYER_ASSIGNMENT (  '', '', ( #53843 ) ) ;
#34756 = FILL_AREA_STYLE_COLOUR ( '', #31634 ) ;
#34757 = VERTEX_POINT ( 'NONE', #58270 ) ;
#34758 = FACE_OUTER_BOUND ( 'NONE', #65184, .T. ) ;
#34759 = EDGE_CURVE ( 'NONE', #30491, #22486, #20556, .T. ) ;
#34760 = FACE_OUTER_BOUND ( 'NONE', #17895, .T. ) ;
#34761 = CARTESIAN_POINT ( 'NONE',  ( -157.1929263765337907, -10.01517768586948698, 6.132527647946031529E-16 ) ) ;
#34762 = CYLINDRICAL_SURFACE ( 'NONE', #69667, 0.5000000000000004441 ) ;
#34763 = ORIENTED_EDGE ( 'NONE', *, *, #462, .T. ) ;
#34764 = ORIENTED_EDGE ( 'NONE', *, *, #26578, .F. ) ;
#34765 = AXIS2_PLACEMENT_3D ( 'NONE', #46614, #46955, #20152 ) ;
#34766 = CARTESIAN_POINT ( 'NONE',  ( -30.83411394072454925, -7.922994316747240084, -1.304230133214211662 ) ) ;
#34767 = DIRECTION ( 'NONE',  ( 0.000000000000000000, 1.000000000000000000, 0.000000000000000000 ) ) ;
#34768 = EDGE_CURVE ( 'NONE', #35517, #40833, #10445, .T. ) ;
#34769 = FACE_OUTER_BOUND ( 'NONE', #2913, .T. ) ;
#34770 = VERTEX_POINT ( 'NONE', #31877 ) ;
#34771 = CARTESIAN_POINT ( 'NONE',  ( -123.2070736234669255, 3.094860106630802576, 9.524999999991006661 ) ) ;
#34772 =( NAMED_UNIT ( * ) SI_UNIT ( $, .STERADIAN. ) SOLID_ANGLE_UNIT ( ) );
#34773 = EDGE_CURVE ( 'NONE', #12077, #63927, #26585, .T. ) ;
#34774 = PRESENTATION_STYLE_ASSIGNMENT (( #13315 ) ) ;
#34775 =( GEOMETRIC_REPRESENTATION_CONTEXT ( 3 ) GLOBAL_UNCERTAINTY_ASSIGNED_CONTEXT ( ( #46998 ) ) GLOBAL_UNIT_ASSIGNED_CONTEXT ( ( #45069, #62574, #34120 ) ) REPRESENTATION_CONTEXT ( 'NONE', 'WORKASPACE' ) );
#34776 = CARTESIAN_POINT ( 'NONE',  ( -58.55707362346616662, -1.166476076187852838E-15, -9.524999999999991473 ) ) ;
#34777 = DIRECTION ( 'NONE',  ( -1.000000000000000000, 0.000000000000000000, -4.625929269271509580E-16 ) ) ;
#34778 = CIRCLE ( 'NONE', #4426, 0.2500000000000002220 ) ;
#34779 = CARTESIAN_POINT ( 'NONE',  ( -74.99999999999998579, 50.00000000000000000, -41.30495168499704306 ) ) ;
#34780 = MECHANICAL_DESIGN_GEOMETRIC_PRESENTATION_REPRESENTATION (  '', ( #65100 ), #13436 ) ;
#34781 = ORIENTED_EDGE ( 'NONE', *, *, #59955, .F. ) ;
#34782 = PRESENTATION_STYLE_ASSIGNMENT (( #30182 ) ) ;
#34783 = ADVANCED_FACE ( 'NONE', ( #31169 ), #25902, .T. ) ;
#34784 = CARTESIAN_POINT ( 'NONE',  ( 71.50000000000000000, 14.49137674618942562, 9.500000000000000000 ) ) ;
#34785 = AXIS2_PLACEMENT_3D ( 'NONE', #25434, #3586, #67657 ) ;
#34786 = SURFACE_SIDE_STYLE ('',( #50979 ) ) ;
#34787 = CARTESIAN_POINT ( 'NONE',  ( -97.55499999999999261, 0.000000000000000000, 8.024999999999991473 ) ) ;
#34788 = DIRECTION ( 'NONE',  ( 2.478176394252586564E-16, 0.000000000000000000, 1.000000000000000000 ) ) ;
#34789 = CIRCLE ( 'NONE', #66212, 3.100000000000001865 ) ;
#34790 = ADVANCED_FACE ( 'NONE', ( #42485 ), #16447, .F. ) ;
#34791 = CARTESIAN_POINT ( 'NONE',  ( -97.64499999999999602, 4.716976649647091513, -6.492361379858946790 ) ) ;
#34792 = CARTESIAN_POINT ( 'NONE',  ( -5.598654528085808657, 114.7549999999999812, 7.705886871421373741 ) ) ;
#34793 = CARTESIAN_POINT ( 'NONE',  ( -79.19499999999997897, 8.437984349512085203, -1.550032578732815448E-15 ) ) ;
#34794 = DIRECTION ( 'NONE',  ( 0.000000000000000000, -1.000000000000000000, 0.000000000000000000 ) ) ;
#34795 = ADVANCED_FACE ( 'NONE', ( #20647 ), #39275, .F. ) ;
#34796 = UNCERTAINTY_MEASURE_WITH_UNIT (LENGTH_MEASURE( 1.000000000000000082E-05 ), #67458, 'distance_accuracy_value', 'NONE');
#34797 = AXIS2_PLACEMENT_3D ( 'NONE', #60832, #45059, #66474 ) ;
#34798 = SURFACE_SIDE_STYLE ('',( #33762 ) ) ;
#34799 = ORIENTED_EDGE ( 'NONE', *, *, #49489, .F. ) ;
#34800 = CARTESIAN_POINT ( 'NONE',  ( -118.3429263765338106, -9.058813317711329915, 2.943386871421371787 ) ) ;
#34801 = EDGE_CURVE ( 'NONE', #54030, #15520, #34728, .T. ) ;
#34802 = CARTESIAN_POINT ( 'NONE',  ( -135.7450000000000045, 4.716976649647094177, 6.492361379858945902 ) ) ;
#34803 = SURFACE_STYLE_FILL_AREA ( #40127 ) ;
#34804 = VECTOR ( 'NONE', #11610, 1000.000000000000000 ) ;
#34805 = CARTESIAN_POINT ( 'NONE',  ( 0.000000000000000000, 0.000000000000000000, 7.500000000000000000 ) ) ;
#34806 = SURFACE_STYLE_FILL_AREA ( #3089 ) ;
#34807 = CARTESIAN_POINT ( 'NONE',  ( 48.50000000000000000, 14.49137674618942562, -9.500000000000000000 ) ) ;
#34808 = ORIENTED_EDGE ( 'NONE', *, *, #51965, .F. ) ;
#34809 = ORIENTED_EDGE ( 'NONE', *, *, #45868, .F. ) ;
#34810 = VECTOR ( 'NONE', #60290, 1000.000000000000000 ) ;
#34811 = COLOUR_RGB ( '', 0.40784314, 0.44705882, 0.49803922) ;
#34812 = DIRECTION ( 'NONE',  ( -0.000000000000000000, 1.000000000000000000, 0.000000000000000000 ) ) ;
#34813 = DIRECTION ( 'NONE',  ( -1.000000000000000000, 0.000000000000000000, 0.000000000000000000 ) ) ;
#34814 = CIRCLE ( 'NONE', #60611, 0.5000000000000004441 ) ;
#34815 = CYLINDRICAL_SURFACE ( 'NONE', #66406, 0.5000000000000004441 ) ;
#34816 = LINE ( 'NONE', #56270, #12375 ) ;
#34817 = CYLINDRICAL_SURFACE ( 'NONE', #18483, 9.524999999999991473 ) ;
#34818 = ORIENTED_EDGE ( 'NONE', *, *, #51951, .F. ) ;
#34819 = CARTESIAN_POINT ( 'NONE',  ( -132.2049999999999841, -2.607480562269071545, -8.024999999999991473 ) ) ;
#34820 = ORIENTED_EDGE ( 'NONE', *, *, #3890, .T. ) ;
#34821 = CARTESIAN_POINT ( 'NONE',  ( -123.6570736234661751, 9.058813317711329915, 2.943386871421369566 ) ) ;
#34822 = ORIENTED_EDGE ( 'NONE', *, *, #49489, .T. ) ;
#34823 = DIRECTION ( 'NONE',  ( 0.000000000000000000, 0.000000000000000000, 1.000000000000000000 ) ) ;
#34824 =( NAMED_UNIT ( * ) SI_UNIT ( $, .STERADIAN. ) SOLID_ANGLE_UNIT ( ) );
#34825 = VERTEX_POINT ( 'NONE', #17799 ) ;
#34826 = STYLED_ITEM ( 'NONE', ( #54154 ), #11347 ) ;
#34827 = DIRECTION ( 'NONE',  ( -0.000000000000000000, -1.000000000000000000, -0.000000000000000000 ) ) ;
#34828 = CARTESIAN_POINT ( 'NONE',  ( 23.50000000000001776, 15.00000000000000000, -29.68999999999999417 ) ) ;
#34829 = COLOUR_RGB ( '', 0.31764706, 0.68627451, 0.89019608) ;
#34830 = CARTESIAN_POINT ( 'NONE',  ( 8.102448949553183510, 144.9950000000000045, -5.886773742842746238 ) ) ;
#34831 = LINE ( 'NONE', #14411, #30643 ) ;
#34832 = ORIENTED_EDGE ( 'NONE', *, *, #57503, .F. ) ;
#34833 = CARTESIAN_POINT ( 'NONE',  ( -74.50000000000000000, -1.856352308976905642E-14, -6.999999999999999112 ) ) ;
#34834 = CARTESIAN_POINT ( 'NONE',  ( -10.01517768586949408, 141.3050000000000068, -6.132527647946036459E-16 ) ) ;
#34835 = CARTESIAN_POINT ( 'NONE',  ( -47.75499999999999545, 4.716976649647091513, -6.492361379858946790 ) ) ;
#34836 = CIRCLE ( 'NONE', #42781, 0.5000000000000004441 ) ;
#34837 = DIRECTION ( 'NONE',  ( -0.000000000000000000, -0.000000000000000000, -1.000000000000000000 ) ) ;
#34838 = VERTEX_POINT ( 'NONE', #65629 ) ;
#34839 = CARTESIAN_POINT ( 'NONE',  ( 2.607480562269071989, 115.5929263765337964, 8.025000000000002132 ) ) ;
#34840 = CARTESIAN_POINT ( 'NONE',  ( 0.000000000000000000, 1.999999999999998668, 5.000000000000000000 ) ) ;
#34841 = UNCERTAINTY_MEASURE_WITH_UNIT (LENGTH_MEASURE( 1.000000000000000082E-05 ), #5003, 'distance_accuracy_value', 'NONE');
#34842 =( GEOMETRIC_REPRESENTATION_CONTEXT ( 3 ) GLOBAL_UNCERTAINTY_ASSIGNED_CONTEXT ( ( #15887 ) ) GLOBAL_UNIT_ASSIGNED_CONTEXT ( ( #33268, #55045, #32926 ) ) REPRESENTATION_CONTEXT ( 'NONE', 'WORKASPACE' ) );
#34843 = DIRECTION ( 'NONE',  ( 0.000000000000000000, 1.000000000000000000, 0.000000000000000000 ) ) ;
#34844 = ORIENTED_EDGE ( 'NONE', *, *, #42250, .T. ) ;
#34845 = AXIS2_PLACEMENT_3D ( 'NONE', #5268, #48939, #27745 ) ;
#34846 = CARTESIAN_POINT ( 'NONE',  ( 0.000000000000000000, 2.500000000000000000, 0.000000000000000000 ) ) ;
#34847 = EDGE_LOOP ( 'NONE', ( #12018, #21311, #30327, #19432 ) ) ;
#34848 = FACE_OUTER_BOUND ( 'NONE', #48823, .T. ) ;
#34849 = AXIS2_PLACEMENT_3D ( 'NONE', #27419, #17612, #49962 ) ;
#34850 = CARTESIAN_POINT ( 'NONE',  ( -122.6070736234661780, -8.102448949553174629, 5.886773742842742685 ) ) ;
#34851 = DIRECTION ( 'NONE',  ( -1.000000000000000000, 0.000000000000000000, 0.000000000000000000 ) ) ;
#34852 = CARTESIAN_POINT ( 'NONE',  ( -166.4049999999999727, -2.607480562269069768, 8.024999999999991473 ) ) ;
#34853 = ORIENTED_EDGE ( 'NONE', *, *, #12602, .F. ) ;
#34854 = UNCERTAINTY_MEASURE_WITH_UNIT (LENGTH_MEASURE( 1.000000000000000082E-05 ), #64770, 'distance_accuracy_value', 'NONE');
#34855 = AXIS2_PLACEMENT_3D ( 'NONE', #55826, #55120, #55484 ) ;
#34856 =( GEOMETRIC_REPRESENTATION_CONTEXT ( 3 ) GLOBAL_UNCERTAINTY_ASSIGNED_CONTEXT ( ( #50148 ) ) GLOBAL_UNIT_ASSIGNED_CONTEXT ( ( #17944, #33767, #32729 ) ) REPRESENTATION_CONTEXT ( 'NONE', 'WORKASPACE' ) );
#34857 = EDGE_CURVE ( 'NONE', #69477, #39066, #43870, .T. ) ;
#34858 = DIRECTION ( 'NONE',  ( 0.000000000000000000, 0.000000000000000000, -1.000000000000000000 ) ) ;
#34859 = CARTESIAN_POINT ( 'NONE',  ( -17.75000000000000711, 31.24999999999999289, 4.000000000000000000 ) ) ;
#34860 = FACE_OUTER_BOUND ( 'NONE', #30881, .T. ) ;
#34861 = VERTEX_POINT ( 'NONE', #33613 ) ;
#34862 = CIRCLE ( 'NONE', #4512, 0.4999999999999994449 ) ;
#34863 = ADVANCED_FACE ( 'NONE', ( #12852 ), #27956, .T. ) ;
#34864 = VERTEX_POINT ( 'NONE', #1192 ) ;
#34865 = DIRECTION ( 'NONE',  ( 0.000000000000000000, 0.000000000000000000, 1.000000000000000000 ) ) ;
#34867 = EDGE_CURVE ( 'NONE', #64812, #31792, #55416, .T. ) ;
#34866 = CARTESIAN_POINT ( 'NONE',  ( -11.00000000000000000, 8.000000000000000000, 3.500000000000003997 ) ) ;
#34868 = CARTESIAN_POINT ( 'NONE',  ( -77.75499999999999545, 4.716976649647091513, -6.492361379858946790 ) ) ;
#34869 = EDGE_LOOP ( 'NONE', ( #51042, #57950, #18622 ) ) ;
#34870 = CARTESIAN_POINT ( 'NONE',  ( 39.49999999999999289, 18.74999999999997868, 4.000000000000000000 ) ) ;
#34871 = EDGE_CURVE ( 'NONE', #23185, #2421, #66312, .T. ) ;
#34872 = STYLED_ITEM ( 'NONE', ( #30909 ), #59600 ) ;
#34873 = CARTESIAN_POINT ( 'NONE',  ( -63.20707362346617231, 3.094860106618433360, 9.524999999999991473 ) ) ;
#34874 = CARTESIAN_POINT ( 'NONE',  ( -150.9570736234661581, 9.058813317711329915, -2.943386871421373119 ) ) ;
#34875 = FACE_OUTER_BOUND ( 'NONE', #56825, .T. ) ;
#34876 = ORIENTED_EDGE ( 'NONE', *, *, #29203, .F. ) ;
#34877 = PLANE ( 'NONE',  #12408 ) ;
#34879 = DIRECTION ( 'NONE',  ( 1.000000000000000000, 0.000000000000000000, 4.625929269271509580E-16 ) ) ;
#34878 = DIRECTION ( 'NONE',  ( 0.000000000000000000, 1.000000000000000000, 0.000000000000000000 ) ) ;
#34880 = EDGE_CURVE ( 'NONE', #5601, #54750, #41758, .T. ) ;
#34881 = CARTESIAN_POINT ( 'NONE',  ( 8.102448949553183510, 141.9950000000000045, -5.886773742842746238 ) ) ;
#34882 = CARTESIAN_POINT ( 'NONE',  ( -104.2449999999999903, -4.716976649647093289, -6.492361379858945902 ) ) ;
#34883 = AXIS2_PLACEMENT_3D ( 'NONE', #43096, #16684, #16351 ) ;
#34884 = DIRECTION ( 'NONE',  ( -0.000000000000000000, 0.000000000000000000, 1.000000000000000000 ) ) ;
#34885 = AXIS2_PLACEMENT_3D ( 'NONE', #19278, #24909, #46423 ) ;
#34886 = DIRECTION ( 'NONE',  ( -0.7071067811865352493, 0.000000000000000000, -0.7071067811865597852 ) ) ;
#34887 = COLOUR_RGB ( '', 0.09019608, 0.27058824, 0.51372549) ;
#34888 = UNCERTAINTY_MEASURE_WITH_UNIT (LENGTH_MEASURE( 1.000000000000000082E-05 ), #21575, 'distance_accuracy_value', 'NONE');
#34890 = CARTESIAN_POINT ( 'NONE',  ( -19.67620707751459008, 11.86859602145972836, 1.777522113161904782 ) ) ;
#34889 = CARTESIAN_POINT ( 'NONE',  ( -96.80707362346618083, 10.01517768586948698, -1.839758294383808966E-15 ) ) ;
#34891 = CIRCLE ( 'NONE', #53957, 0.5000000000000004441 ) ;
#34892 = CARTESIAN_POINT ( 'NONE',  ( -141.7429263765338021, -5.598654528085803328, -7.705886871421366635 ) ) ;
#34893 = FILL_AREA_STYLE_COLOUR ( '', #38263 ) ;
#34894 = CARTESIAN_POINT ( 'NONE',  ( -162.1449999999999818, -4.716976649647092401, 6.492361379858946790 ) ) ;
#34895 = TOROIDAL_SURFACE ( 'NONE', #24782, 10.50000000000000533, 0.5000000000000000000 ) ;
#34896 = EDGE_CURVE ( 'NONE', #11361, #63620, #32936, .T. ) ;
#34897 = CARTESIAN_POINT ( 'NONE',  ( 0.000000000000000000, 0.000000000000000000, 0.2499999999999924227 ) ) ;
#34898 = ORIENTED_EDGE ( 'NONE', *, *, #68149, .F. ) ;
#34899 = DIRECTION ( 'NONE',  ( 0.000000000000000000, -1.000000000000000000, 0.000000000000000000 ) ) ;
#34900 = ORIENTED_EDGE ( 'NONE', *, *, #30083, .F. ) ;
#34901 = EDGE_CURVE ( 'NONE', #41057, #24214, #1555, .T. ) ;
#34902 =( NAMED_UNIT ( * ) SI_UNIT ( $, .STERADIAN. ) SOLID_ANGLE_UNIT ( ) );
#34903 =( GEOMETRIC_REPRESENTATION_CONTEXT ( 3 ) GLOBAL_UNCERTAINTY_ASSIGNED_CONTEXT ( ( #45912 ) ) GLOBAL_UNIT_ASSIGNED_CONTEXT ( ( #48097, #65956, #60327 ) ) REPRESENTATION_CONTEXT ( 'NONE', 'WORKASPACE' ) );
#34904 = SURFACE_STYLE_FILL_AREA ( #28910 ) ;
#34905 = DIRECTION ( 'NONE',  ( -1.000000000000000000, 0.000000000000000000, 0.000000000000000000 ) ) ;
#34906 = DIRECTION ( 'NONE',  ( -5.782411586589351722E-16, 1.000000000000000000, 0.000000000000000000 ) ) ;
#34907 = COLOUR_RGB ( '', 0.31764706, 0.68627451, 0.89019608) ;
#34908 = CARTESIAN_POINT ( 'NONE',  ( 29.00000000000000000, 0.000000000000000000, 3.902931319921305165E-16 ) ) ;
#34909 = ORIENTED_EDGE ( 'NONE', *, *, #1051, .T. ) ;
#34910 = CARTESIAN_POINT ( 'NONE',  ( -158.3049999999999500, 8.437984349512086979, -1.550032578732815448E-15 ) ) ;
#34911 = ORIENTED_EDGE ( 'NONE', *, *, #9666, .F. ) ;
#34912 = CARTESIAN_POINT ( 'NONE',  ( 6.422934014168398598, 153.0000000000000000, 4.811085495980990778 ) ) ;
#34913 = DIRECTION ( 'NONE',  ( 1.000000000000000000, 1.387778780781444571E-14, -0.000000000000000000 ) ) ;
#34914 = ORIENTED_EDGE ( 'NONE', *, *, #54271, .F. ) ;
#34915 = AXIS2_PLACEMENT_3D ( 'NONE', #36927, #10851, #572 ) ;
#34916 = PRESENTATION_STYLE_ASSIGNMENT (( #51114 ) ) ;
#34917 = DIRECTION ( 'NONE',  ( 0.000000000000000000, 0.000000000000000000, 1.000000000000000000 ) ) ;
#34918 = CARTESIAN_POINT ( 'NONE',  ( 8.102448949553183510, 114.9949999999999903, -5.886773742842746238 ) ) ;
#34919 = ORIENTED_EDGE ( 'NONE', *, *, #50920, .T. ) ;
#34920 = STYLED_ITEM ( 'NONE', ( #3194 ), #45092 ) ;
#34921 = DIRECTION ( 'NONE',  ( 0.000000000000000000, 0.000000000000000000, -1.000000000000000000 ) ) ;
#34922 = LINE ( 'NONE', #39540, #45168 ) ;
#34923 = AXIS2_PLACEMENT_3D ( 'NONE', #48602, #68635, #9566 ) ;
#34924 = CARTESIAN_POINT ( 'NONE',  ( -72.50499999999998124, -6.826472737025113702, -4.959722759717900331 ) ) ;
#34925 = DIRECTION ( 'NONE',  ( 0.000000000000000000, 0.000000000000000000, 1.000000000000000000 ) ) ;
#34926 = CARTESIAN_POINT ( 'NONE',  ( 3.094860106618435136, 137.4050000000000296, -9.525000000000000355 ) ) ;
#34927 = UNCERTAINTY_MEASURE_WITH_UNIT (LENGTH_MEASURE( 1.000000000000000082E-05 ), #38990, 'distance_accuracy_value', 'NONE');
#34928 = CYLINDRICAL_SURFACE ( 'NONE', #3734, 0.5000000000000004441 ) ;
#34929 = CYLINDRICAL_SURFACE ( 'NONE', #27604, 4.999999999999997335 ) ;
#34930 = CIRCLE ( 'NONE', #55137, 5.000000000000000000 ) ;
#34931 = PRESENTATION_STYLE_ASSIGNMENT (( #67291 ) ) ;
#34932 = ADVANCED_FACE ( 'NONE', ( #6190 ), #65278, .F. ) ;
#34933 = COLOUR_RGB ( '', 0.09019608, 0.27058824, 0.51372549) ;
#34934 = CYLINDRICAL_SURFACE ( 'NONE', #14931, 0.5000000000000004441 ) ;
#34935 = ORIENTED_EDGE ( 'NONE', *, *, #61507, .T. ) ;
#34936 = SURFACE_SIDE_STYLE ('',( #14186 ) ) ;
#34937 = CARTESIAN_POINT ( 'NONE',  ( -49.64499999999999602, 4.716976649647091513, -6.492361379858946790 ) ) ;
#34939 = EDGE_LOOP ( 'NONE', ( #34176, #55516, #50782, #30395 ) ) ;
#34938 = COLOUR_RGB ( '', 0.31764706, 0.68627451, 0.89019608) ;
#34940 = CARTESIAN_POINT ( 'NONE',  ( 0.000000000000000000, 2.299999999999999822, -10.00000000000000000 ) ) ;
#34941 = VECTOR ( 'NONE', #224, 1000.000000000000000 ) ;
#34942 = SURFACE_STYLE_USAGE ( .BOTH. , #29670 ) ;
#34943 = DIRECTION ( 'NONE',  ( -0.000000000000000000, -1.000000000000000000, -0.000000000000000000 ) ) ;
#34944 = PLANE ( 'NONE',  #5992 ) ;
#34945 = ORIENTED_EDGE ( 'NONE', *, *, #12568, .F. ) ;
#34946 = CARTESIAN_POINT ( 'NONE',  ( -51.54855153546065338, -10.14125325047201187, 4.285873052701354879 ) ) ;
#34947 = CARTESIAN_POINT ( 'NONE',  ( -55.34499999999997755, 7.632228543268599452, -2.479861379858951942 ) ) ;
#34948 = FILL_AREA_STYLE_COLOUR ( '', #26531 ) ;
#34949 = VECTOR ( 'NONE', #36146, 1000.000000000000000 ) ;
#34950 = ORIENTED_EDGE ( 'NONE', *, *, #12701, .F. ) ;
#34952 = EDGE_CURVE ( 'NONE', #10613, #37052, #51895, .T. ) ;
#34951 =( LENGTH_UNIT ( ) NAMED_UNIT ( * ) SI_UNIT ( .MILLI., .METRE. ) );
#34953 = CARTESIAN_POINT ( 'NONE',  ( -108.0549999999999784, -9.827790563157499189E-16, -8.024999999999991473 ) ) ;
#34954 = ORIENTED_EDGE ( 'NONE', *, *, #29056, .F. ) ;
#34955 = CARTESIAN_POINT ( 'NONE',  ( 0.000000000000000000, 109.9999999999999858, -9.525000000000000355 ) ) ;
#34956 = CARTESIAN_POINT ( 'NONE',  ( -143.3070736234661240, -10.01517768586948698, 6.132527647946031529E-16 ) ) ;
#34957 = CYLINDRICAL_SURFACE ( 'NONE', #64257, 0.5000000000000004441 ) ;
#34958 = AXIS2_PLACEMENT_3D ( 'NONE', #62487, #14306, #35769 ) ;
#34959 = CARTESIAN_POINT ( 'NONE',  ( 0.000000000000000000, 139.4449999999999932, -9.525000000000000355 ) ) ;
#34960 = CARTESIAN_POINT ( 'NONE',  ( -85.40707362346616094, 3.094860106618428031, -9.524999999999993250 ) ) ;
#34961 = CARTESIAN_POINT ( 'NONE',  ( -95.24292637653381632, 5.598654528085804216, 7.705886871421366635 ) ) ;
#34962 = CARTESIAN_POINT ( 'NONE',  ( 6.000000000000017764, 26.00000000000000355, -20.50000000000000355 ) ) ;
#34963 = PRESENTATION_LAYER_ASSIGNMENT (  '', '', ( #49440 ) ) ;
#34964 = AXIS2_PLACEMENT_3D ( 'NONE', #8500, #52798, #56673 ) ;
#34965 = CYLINDRICAL_SURFACE ( 'NONE', #27881, 13.99999999999999822 ) ;
#34966 = EDGE_CURVE ( 'NONE', #10826, #63373, #51527, .T. ) ;
#34967 = CARTESIAN_POINT ( 'NONE',  ( -121.7049999999999841, 2.607480562269073321, 8.024999999999991473 ) ) ;
#34968 = FILL_AREA_STYLE ('',( #8932 ) ) ;
#34969 = PRESENTATION_STYLE_ASSIGNMENT (( #51491 ) ) ;
#34970 = CARTESIAN_POINT ( 'NONE',  ( -135.7450000000000045, 4.716976649647094177, 6.492361379858945902 ) ) ;
#34971 = CARTESIAN_POINT ( 'NONE',  ( -115.7949999999999875, 2.607480562269069324, -8.024999999999993250 ) ) ;
#34972 = VECTOR ( 'NONE', #22896, 1000.000000000000000 ) ;
#34973 = CARTESIAN_POINT ( 'NONE',  ( -5.000000000000000000, 0.000000000000000000, 1.000000000000000000 ) ) ;
#34974 = ORIENTED_EDGE ( 'NONE', *, *, #56948, .F. ) ;
#34975 = DIRECTION ( 'NONE',  ( 2.312964634635740689E-15, -1.000000000000000000, 0.000000000000000000 ) ) ;
#34976 = CARTESIAN_POINT ( 'NONE',  ( 0.000000000000000000, 0.000000000000000000, 0.000000000000000000 ) ) ;
#34977 = PRESENTATION_STYLE_ASSIGNMENT (( #3260 ) ) ;
#34978 = CARTESIAN_POINT ( 'NONE',  ( -175.0429263765338135, -9.058813317711329915, -2.943386871421370898 ) ) ;
#34979 =( BOUNDED_CURVE ( )  B_SPLINE_CURVE ( 2, ( #47718, #41710, #63134, #58547, #14972, #31449, #10709, #36455, #20568, #26527, #9697 ),
 .UNSPECIFIED., .F., .F. ) 
 B_SPLINE_CURVE_WITH_KNOTS ( ( 3, 2, 2, 2, 2, 3 ),
 ( 0.6176470588235297710, 0.6235294117647062206, 0.6294117647058826703, 0.6352941176470590090, 0.6411764705882355697, 0.6470588235294120194 ),
 .UNSPECIFIED. ) 
 CURVE ( )  GEOMETRIC_REPRESENTATION_ITEM ( )  RATIONAL_B_SPLINE_CURVE ( ( 0.9999999999999972244, 0.9510565162951563067, 1.000000000000000000, 0.9510565162951535312, 1.000000000000000000, 0.9510565162951535312, 1.000000000000000000, 0.9510565162951535312, 1.000000000000000000, 0.9510565162951516438, 1.000000000000001776 ) ) 
 REPRESENTATION_ITEM ( '' )  );
#34980 = FILL_AREA_STYLE ('',( #41682 ) ) ;
#34981 = DIRECTION ( 'NONE',  ( -0.000000000000000000, -0.000000000000000000, 1.000000000000000000 ) ) ;
#34982 = VECTOR ( 'NONE', #59520, 1000.000000000000000 ) ;
#34983 = LINE ( 'NONE', #45587, #68051 ) ;
#34984 = TOROIDAL_SURFACE ( 'NONE', #4648, 1.000000000000000000, 0.5000000000000000000 ) ;
#34985 = DIRECTION ( 'NONE',  ( 0.000000000000000000, -1.000000000000000000, 0.000000000000000000 ) ) ;
#34986 = FACE_OUTER_BOUND ( 'NONE', #31375, .T. ) ;
#34987 = ORIENTED_EDGE ( 'NONE', *, *, #3056, .T. ) ;
#34988 = VECTOR ( 'NONE', #40658, 1000.000000000000000 ) ;
#34989 = CARTESIAN_POINT ( 'NONE',  ( -85.04292637653381348, -9.058813317711329915, -2.943386871421370898 ) ) ;
#34990 = CONICAL_SURFACE ( 'NONE', #62, 4.000000000000000000, 0.7853981633974482790 ) ;
#34991 = DIRECTION ( 'NONE',  ( -0.000000000000000000, 1.000000000000000000, 0.000000000000000000 ) ) ;
#34992 = DIRECTION ( 'NONE',  ( 0.000000000000000000, 0.000000000000000000, 1.000000000000000000 ) ) ;
#34993 = CARTESIAN_POINT ( 'NONE',  ( -163.7929263765340693, -3.094860106613926298, 9.525000000003263523 ) ) ;
#34994 = VECTOR ( 'NONE', #45910, 1000.000000000000000 ) ;
#34995 = DIRECTION ( 'NONE',  ( 0.000000000000000000, 1.000000000000000000, 0.000000000000000000 ) ) ;
#34996 = ORIENTED_EDGE ( 'NONE', *, *, #51635, .F. ) ;
#34997 = VECTOR ( 'NONE', #65847, 1000.000000000000000 ) ;
#34998 = DIRECTION ( 'NONE',  ( -0.9994052928406508274, -0.03448275862069643399, -0.000000000000000000 ) ) ;
#34999 = SURFACE_STYLE_FILL_AREA ( #49200 ) ;
#35000 = CARTESIAN_POINT ( 'NONE',  ( -4.750000000000002665, 24.99999999999998579, -3.750000000000000000 ) ) ;
#35001 = EDGE_LOOP ( 'NONE', ( #39114, #66434, #57482, #11059 ) ) ;
#35002 = CARTESIAN_POINT ( 'NONE',  ( -63.59292637653378222, -3.094860106618431139, -9.524999999999991473 ) ) ;
#35003 =( BOUNDED_CURVE ( )  B_SPLINE_CURVE ( 2, ( #44994, #67104, #51622, #46027, #19237, #45685, #18223, #13987, #66762, #62508, #35455 ),
 .UNSPECIFIED., .F., .F. ) 
 B_SPLINE_CURVE_WITH_KNOTS ( ( 3, 2, 2, 2, 2, 3 ),
 ( 0.8586956521739130821, 0.8608695652173913304, 0.8630434782608695787, 0.8652173913043478271, 0.8673913043478260754, 0.8695652173913043237 ),
 .UNSPECIFIED. ) 
 CURVE ( )  GEOMETRIC_REPRESENTATION_ITEM ( )  RATIONAL_B_SPLINE_CURVE ( ( 1.000000000000000000, 0.9510565162951535312, 1.000000000000000000, 0.9510565162951535312, 1.000000000000000000, 0.9510565162951535312, 1.000000000000000000, 0.9510565162951535312, 1.000000000000000000, 0.9510565162951535312, 1.000000000000000000 ) ) 
 REPRESENTATION_ITEM ( '' )  );
#35004 = CARTESIAN_POINT ( 'NONE',  ( 2.607480562269071989, 137.7070736234661013, 8.025000000000002132 ) ) ;
#35005 = VECTOR ( 'NONE', #8734, 1000.000000000000000 ) ;
#35006 = FACE_OUTER_BOUND ( 'NONE', #29182, .T. ) ;
#35007 = ORIENTED_EDGE ( 'NONE', *, *, #53544, .T. ) ;
#35008 = CARTESIAN_POINT ( 'NONE',  ( 34.99999999999992895, 113.4999999999999858, -7.000000000000000000 ) ) ;
#35009 = DIRECTION ( 'NONE',  ( -1.000000000000000000, 0.000000000000000000, 0.000000000000000000 ) ) ;
#35010 = CARTESIAN_POINT ( 'NONE',  ( 68.99999999999998579, 1.000000000000008438, -4.000000000000000000 ) ) ;
#35011 = SURFACE_SIDE_STYLE ('',( #33965 ) ) ;
#35012 = EDGE_CURVE ( 'NONE', #55787, #1416, #24778, .T. ) ;
#35013 = MECHANICAL_DESIGN_GEOMETRIC_PRESENTATION_REPRESENTATION (  '', ( #53004 ), #33904 ) ;
#35014 = CARTESIAN_POINT ( 'NONE',  ( -71.90707362346616094, -3.094860106618429807, 9.524999999999991473 ) ) ;
#35015 = CARTESIAN_POINT ( 'NONE',  ( -82.79499999999998749, 2.607480562269068880, -8.024999999999993250 ) ) ;
#35016 = EDGE_LOOP ( 'NONE', ( #5761, #59907, #5929, #48064 ) ) ;
#35017 = EDGE_CURVE ( 'NONE', #30753, #53491, #2224, .T. ) ;
#35018 = PLANE ( 'NONE',  #7539 ) ;
#35019 = MECHANICAL_DESIGN_GEOMETRIC_PRESENTATION_REPRESENTATION (  '', ( #41788 ), #13730 ) ;
#35020 = FILL_AREA_STYLE ('',( #30074 ) ) ;
#35021 = VERTEX_POINT ( 'NONE', #23755 ) ;
#35022 = CARTESIAN_POINT ( 'NONE',  ( -75.74292637653380211, -5.598654528085803328, -7.705886871421366635 ) ) ;
#35023 =( NAMED_UNIT ( * ) SI_UNIT ( $, .STERADIAN. ) SOLID_ANGLE_UNIT ( ) );
#35024 = AXIS2_PLACEMENT_3D ( 'NONE', #23844, #45349, #19242 ) ;
#35025 = EDGE_CURVE ( 'NONE', #40048, #52271, #21480, .T. ) ;
#35026 = ADVANCED_FACE ( 'NONE', ( #35712 ), #47390, .F. ) ;
#35027 = VERTEX_POINT ( 'NONE', #56821 ) ;
#35028 = AXIS2_PLACEMENT_3D ( 'NONE', #26586, #41791, #16089 ) ;
#35029 = ADVANCED_FACE ( 'NONE', ( #67360 ), #61377, .F. ) ;
#35030 = ORIENTED_EDGE ( 'NONE', *, *, #11599, .T. ) ;
#35031 = PRESENTATION_STYLE_ASSIGNMENT (( #17823 ) ) ;
#35032 = FACE_OUTER_BOUND ( 'NONE', #5061, .T. ) ;
#35033 = DIRECTION ( 'NONE',  ( -1.000000000000000000, 0.000000000000000000, 0.000000000000000000 ) ) ;
#35034 = CARTESIAN_POINT ( 'NONE',  ( -168.3570736234661922, 5.598654528085804216, 7.705886871421366635 ) ) ;
#35035 = EDGE_CURVE ( 'NONE', #59308, #58413, #68699, .T. ) ;
#35036 = CARTESIAN_POINT ( 'NONE',  ( -3.094860106618432471, 112.5949999999999847, -9.525000000000000355 ) ) ;
#35037 = CARTESIAN_POINT ( 'NONE',  ( -112.7070736234661581, -3.094860106618431139, -9.524999999999991473 ) ) ;
#35038 = VECTOR ( 'NONE', #67706, 1000.000000000000000 ) ;
#35039 = PRESENTATION_STYLE_ASSIGNMENT (( #60713 ) ) ;
#35040 = EDGE_CURVE ( 'NONE', #57704, #8462, #28215, .T. ) ;
#35041 = CARTESIAN_POINT ( 'NONE',  ( -133.5570736234661808, -1.166476076187852838E-15, -9.524999999999991473 ) ) ;
#35042 = ORIENTED_EDGE ( 'NONE', *, *, #57166, .F. ) ;
#35043 = CIRCLE ( 'NONE', #24944, 6.000000000000005329 ) ;
#35044 = DIRECTION ( 'NONE',  ( 1.000000000000000000, 0.000000000000000000, 0.000000000000000000 ) ) ;
#35045 = DIRECTION ( 'NONE',  ( -1.000000000000000000, 0.000000000000000000, 0.000000000000000000 ) ) ;
#35046 = DIRECTION ( 'NONE',  ( -1.000000000000000000, 0.000000000000000000, 0.000000000000000000 ) ) ;
#35047 = CIRCLE ( 'NONE', #24947, 0.2500000000000002220 ) ;
#35048 = CARTESIAN_POINT ( 'NONE',  ( -147.5049999999999955, -6.826472737025115478, -4.959722759717899443 ) ) ;
#35049 = SURFACE_STYLE_USAGE ( .BOTH. , #57910 ) ;
#35050 = CARTESIAN_POINT ( 'NONE',  ( -147.5929263765342796, -3.094860106626229346, -9.524999999994326672 ) ) ;
#35051 = VECTOR ( 'NONE', #35483, 1000.000000000000000 ) ;
#35052 = CARTESIAN_POINT ( 'NONE',  ( -166.7950000000000159, 2.607480562269068880, -8.024999999999993250 ) ) ;
#35053 = CARTESIAN_POINT ( 'NONE',  ( -147.5949999999999704, 2.607480562269072433, 8.024999999999991473 ) ) ;
#35054 = ORIENTED_EDGE ( 'NONE', *, *, #22393, .T. ) ;
#35055 = COLOUR_RGB ( '', 0.72549020, 0.75294118, 0.79215686) ;
#35056 = CYLINDRICAL_SURFACE ( 'NONE', #6477, 8.000000000000014211 ) ;
#35057 = CARTESIAN_POINT ( 'NONE',  ( 36.00000000000002842, 0.000000000000000000, 77.00402776293825013 ) ) ;
#35058 = CARTESIAN_POINT ( 'NONE',  ( -62.30499999999997840, 8.437984349512085203, -1.550032578732815448E-15 ) ) ;
#35059 = DIRECTION ( 'NONE',  ( -1.000000000000000000, 0.000000000000000000, -0.000000000000000000 ) ) ;
#35060 = DIRECTION ( 'NONE',  ( 1.000000000000000000, -0.000000000000000000, -0.000000000000000000 ) ) ;
#35061 = CARTESIAN_POINT ( 'NONE',  ( -58.94499999999998607, -9.827790563157499189E-16, -8.024999999999991473 ) ) ;
#35062 = CARTESIAN_POINT ( 'NONE',  ( -9.058813317711337021, 150.1549999999999727, -2.943386871421374895 ) ) ;
#35063 = DIRECTION ( 'NONE',  ( -0.000000000000000000, 0.000000000000000000, 1.000000000000000000 ) ) ;
#35064 = COLOUR_RGB ( '', 0.08235294, 0.09019608, 0.10196078) ;
#35065 = FILL_AREA_STYLE_COLOUR ( '', #27843 ) ;
#35066 = DIRECTION ( 'NONE',  ( 1.000000000000000000, 0.000000000000000000, 0.000000000000000000 ) ) ;
#35067 = DIRECTION ( 'NONE',  ( -1.000000000000000000, 0.000000000000000000, 0.000000000000000000 ) ) ;
#35068 = VECTOR ( 'NONE', #49270, 1000.000000000000000 ) ;
#35069 = DIRECTION ( 'NONE',  ( 0.000000000000000000, 1.000000000000000000, -0.000000000000000000 ) ) ;
#35070 = DIRECTION ( 'NONE',  ( 0.000000000000000000, 0.000000000000000000, -1.000000000000000000 ) ) ;
#35071 =( GEOMETRIC_REPRESENTATION_CONTEXT ( 3 ) GLOBAL_UNCERTAINTY_ASSIGNED_CONTEXT ( ( #10376 ) ) GLOBAL_UNIT_ASSIGNED_CONTEXT ( ( #14979, #25156, #5082 ) ) REPRESENTATION_CONTEXT ( 'NONE', 'WORKASPACE' ) );
#35072 =( NAMED_UNIT ( * ) PLANE_ANGLE_UNIT ( ) SI_UNIT ( $, .RADIAN. ) );
#35073 = CIRCLE ( 'NONE', #49703, 0.5000000000000004441 ) ;
#35074 = DIRECTION ( 'NONE',  ( 0.000000000000000000, 0.000000000000000000, 1.000000000000000000 ) ) ;
#35075 = ORIENTED_EDGE ( 'NONE', *, *, #55112, .F. ) ;
#35076 = ORIENTED_EDGE ( 'NONE', *, *, #29879, .T. ) ;
#35077 = DIRECTION ( 'NONE',  ( 0.000000000000000000, 0.000000000000000000, 1.000000000000000000 ) ) ;
#35078 =( GEOMETRIC_REPRESENTATION_CONTEXT ( 3 ) GLOBAL_UNCERTAINTY_ASSIGNED_CONTEXT ( ( #65828 ) ) GLOBAL_UNIT_ASSIGNED_CONTEXT ( ( #41809, #68866, #52350 ) ) REPRESENTATION_CONTEXT ( 'NONE', 'WORKASPACE' ) );
#35079 =( NAMED_UNIT ( * ) PLANE_ANGLE_UNIT ( ) SI_UNIT ( $, .RADIAN. ) );
#35080 = MECHANICAL_DESIGN_GEOMETRIC_PRESENTATION_REPRESENTATION (  '', ( #38508 ), #3560 ) ;
#35081 = DIRECTION ( 'NONE',  ( 0.000000000000000000, 0.000000000000000000, -1.000000000000000000 ) ) ;
#35082 = EDGE_LOOP ( 'NONE', ( #32345, #53481, #55700, #67359 ) ) ;
#35083 = EDGE_LOOP ( 'NONE', ( #41605, #43162, #40093 ) ) ;
#35084 = DIRECTION ( 'NONE',  ( 0.000000000000000000, 0.000000000000000000, 1.000000000000000000 ) ) ;
#35085 = VERTEX_POINT ( 'NONE', #48041 ) ;
#35086 = CARTESIAN_POINT ( 'NONE',  ( -5.598654528085806881, 113.8549999999999898, -7.705886871421374629 ) ) ;
#35087 = LINE ( 'NONE', #13988, #42319 ) ;
#35088 = ORIENTED_EDGE ( 'NONE', *, *, #51381, .F. ) ;
#35089 = CIRCLE ( 'NONE', #58694, 17.00000000000000000 ) ;
#35090 = ADVANCED_FACE ( 'NONE', ( #26520, #26173 ), #21234, .T. ) ;
#35091 = CARTESIAN_POINT ( 'NONE',  ( -82.55707362346618083, -1.166476076187852838E-15, -9.524999999999991473 ) ) ;
#35092 = CYLINDRICAL_SURFACE ( 'NONE', #35024, 9.524999999999991473 ) ;
#35093 = CARTESIAN_POINT ( 'NONE',  ( -110.5449999999999875, -7.632228543268600340, -2.479861379858950166 ) ) ;
#35094 = ORIENTED_EDGE ( 'NONE', *, *, #45772, .F. ) ;
#35095 = EDGE_CURVE ( 'NONE', #51912, #23284, #6224, .T. ) ;
#35096 =( BOUNDED_CURVE ( )  B_SPLINE_CURVE ( 2, ( #22295, #43794, #50775, #12775, #13121, #66601, #66954, #50093, #60600, #2148, #1823 ),
 .UNSPECIFIED., .F., .F. ) 
 B_SPLINE_CURVE_WITH_KNOTS ( ( 3, 2, 2, 2, 2, 3 ),
 ( 0.4999999999999882316, 0.5021739130434664800, 0.5043478260869446173, 0.5065217391304228656, 0.5086956521739010029, 0.5108695652173793622 ),
 .UNSPECIFIED. ) 
 CURVE ( )  GEOMETRIC_REPRESENTATION_ITEM ( )  RATIONAL_B_SPLINE_CURVE ( ( 1.000000000000264899, 0.9510565162948886320, 1.000000000000000000, 0.9510565162951535312, 1.000000000000000000, 0.9510565162951535312, 1.000000000000000000, 0.9510565162951535312, 1.000000000000000000, 0.9510565162954235374, 0.9999999999997299938 ) ) 
 REPRESENTATION_ITEM ( '' )  );
#35097 = PRESENTATION_LAYER_ASSIGNMENT (  '', '', ( #36310 ) ) ;
#35098 = CARTESIAN_POINT ( 'NONE',  ( -10.39230484541326938, 2.500000000000000000, -1.734723475976807094E-15 ) ) ;
#35099 = CARTESIAN_POINT ( 'NONE',  ( -53.84292637653378932, 9.058813317711329915, -2.943386871421373119 ) ) ;
#35100 = CARTESIAN_POINT ( 'NONE',  ( -11.23735010877653728, -11.53731097901733804, -3.308824629120899363 ) ) ;
#35101 = CARTESIAN_POINT ( 'NONE',  ( -18.00000000000000711, 31.24999999999999289, -3.750000000000000000 ) ) ;
#35102 = ORIENTED_EDGE ( 'NONE', *, *, #53552, .T. ) ;
#35103 = CARTESIAN_POINT ( 'NONE',  ( 2.607480562269071989, 145.5929263765338249, 8.025000000000002132 ) ) ;
#35104 = CARTESIAN_POINT ( 'NONE',  ( -54.07000006678288884, -9.448433432976491630, -2.594157102514922375 ) ) ;
#35105 = VECTOR ( 'NONE', #10983, 1000.000000000000000 ) ;
#35106 = DIRECTION ( 'NONE',  ( 1.000000000000000000, -0.000000000000000000, -1.300977106640434891E-16 ) ) ;
#35107 = DIRECTION ( 'NONE',  ( 0.000000000000000000, 0.000000000000000000, 1.000000000000000000 ) ) ;
#35108 = VERTEX_POINT ( 'NONE', #10704 ) ;
#35109 = CARTESIAN_POINT ( 'NONE',  ( 48.00000000000000000, 99.99999999999992895, 9.500000000000000000 ) ) ;
#35110 = EDGE_CURVE ( 'NONE', #37037, #40236, #41705, .T. ) ;
#35111 = ORIENTED_EDGE ( 'NONE', *, *, #37222, .F. ) ;
#35112 = DIRECTION ( 'NONE',  ( -0.000000000000000000, -0.000000000000000000, -1.000000000000000000 ) ) ;
#35113 = SURFACE_STYLE_FILL_AREA ( #34074 ) ;
#35114 = FACE_OUTER_BOUND ( 'NONE', #25343, .T. ) ;
#35115 = FACE_OUTER_BOUND ( 'NONE', #45091, .T. ) ;
#35117 = CARTESIAN_POINT ( 'NONE',  ( -137.4549999999999841, 7.632228543268599452, -2.479861379858951942 ) ) ;
#35116 = CONICAL_SURFACE ( 'NONE', #21656, 5.000000000000004441, 0.7853981633974579379 ) ;
#35118 = LINE ( 'NONE', #18918, #59700 ) ;
#35119 = ORIENTED_EDGE ( 'NONE', *, *, #35156, .T. ) ;
#35120 = FILL_AREA_STYLE_COLOUR ( '', #64687 ) ;
#35121 = AXIS2_PLACEMENT_3D ( 'NONE', #62607, #52448, #20402 ) ;
#35122 = EDGE_CURVE ( 'NONE', #40785, #34213, #36787, .T. ) ;
#35123 = CARTESIAN_POINT ( 'NONE',  ( -74.86954670510183973, 36.13097948458331388, 9.842709678231122084 ) ) ;
#35124 = DIRECTION ( 'NONE',  ( -1.000000000000000000, 0.000000000000000000, 0.000000000000000000 ) ) ;
#35125 = ORIENTED_EDGE ( 'NONE', *, *, #12701, .T. ) ;
#35126 = CIRCLE ( 'NONE', #4790, 8.500000000000007105 ) ;
#35127 = ORIENTED_EDGE ( 'NONE', *, *, #11278, .F. ) ;
#35128 = CARTESIAN_POINT ( 'NONE',  ( -32.13196390538205094, -8.494561555450525603, -2.203021938113412848 ) ) ;
#35129 = SURFACE_STYLE_FILL_AREA ( #56224 ) ;
#35130 = EDGE_LOOP ( 'NONE', ( #50868, #65625, #32176, #25516 ) ) ;
#35131 = FILL_AREA_STYLE_COLOUR ( '', #26968 ) ;
#35132 = CARTESIAN_POINT ( 'NONE',  ( -182.3049999999999500, 8.437984349512085203, -1.550032578732815448E-15 ) ) ;
#35133 = CARTESIAN_POINT ( 'NONE',  ( -9.984889265949528081, 1.515110734050472807, 0.7056644834263087196 ) ) ;
#35134 = AXIS2_PLACEMENT_3D ( 'NONE', #47889, #59063, #15491 ) ;
#35135 = CARTESIAN_POINT ( 'NONE',  ( -15.48999599679679662, 117.9999999999999716, -9.500000000000000000 ) ) ;
#35136 = CARTESIAN_POINT ( 'NONE',  ( -54.65707362346616804, 9.058813317711329915, 2.943386871421369566 ) ) ;
#35137 = CARTESIAN_POINT ( 'NONE',  ( -175.3449999999999989, 7.632228543268599452, -2.479861379858951942 ) ) ;
#35138 = DIRECTION ( 'NONE',  ( -0.000000000000000000, -0.000000000000000000, 1.000000000000000000 ) ) ;
#35139 = ORIENTED_EDGE ( 'NONE', *, *, #51054, .F. ) ;
#35140 = VECTOR ( 'NONE', #63737, 1000.000000000000000 ) ;
#35141 = CARTESIAN_POINT ( 'NONE',  ( -160.8570736234661922, -5.598654528085803328, -7.705886871421366635 ) ) ;
#35142 = DIRECTION ( 'NONE',  ( 0.000000000000000000, -0.000000000000000000, -1.000000000000000000 ) ) ;
#35143 =( NAMED_UNIT ( * ) SI_UNIT ( $, .STERADIAN. ) SOLID_ANGLE_UNIT ( ) );
#35144 = CARTESIAN_POINT ( 'NONE',  ( -89.90499999999998693, 2.607480562269068880, -8.024999999999993250 ) ) ;
#35145 = CARTESIAN_POINT ( 'NONE',  ( 3.021204673494646276, 154.5000000000000568, -9.043681037409140089 ) ) ;
#35146 = DIRECTION ( 'NONE',  ( 1.224646799147353207E-16, 1.000000000000000000, -0.000000000000000000 ) ) ;
#35147 = COLOUR_RGB ( '', 0.40784314, 0.44705882, 0.49803922) ;
#35148 = AXIS2_PLACEMENT_3D ( 'NONE', #64382, #49251, #32703 ) ;
#35149 = CARTESIAN_POINT ( 'NONE',  ( -102.4449999999999932, 0.000000000000000000, 8.024999999999991473 ) ) ;
#35150 = CARTESIAN_POINT ( 'NONE',  ( -10.01517768586949231, 120.3049999999999784, -6.132527647946036459E-16 ) ) ;
#35151 = CARTESIAN_POINT ( 'NONE',  ( -64.94499999999999318, -9.827790563157499189E-16, -8.024999999999991473 ) ) ;
#35152 = MECHANICAL_DESIGN_GEOMETRIC_PRESENTATION_REPRESENTATION (  '', ( #48701 ), #26148 ) ;
#35153 = FILL_AREA_STYLE ('',( #61189 ) ) ;
#35154 = CARTESIAN_POINT ( 'NONE',  ( -56.90707362346616804, -3.094860106618429807, 9.524999999999991473 ) ) ;
#35155 = CARTESIAN_POINT ( 'NONE',  ( 179.4098300562505415, 0.000000000000000000, 0.000000000000000000 ) ) ;
#35156 = EDGE_CURVE ( 'NONE', #65484, #58922, #43179, .T. ) ;
#35157 = TOROIDAL_SURFACE ( 'NONE', #18394, 16.50000000000000000, 0.5000000000000000000 ) ;
#35158 = DIRECTION ( 'NONE',  ( 1.000000000000000000, 0.000000000000000000, 0.000000000000000000 ) ) ;
#35159 = ORIENTED_EDGE ( 'NONE', *, *, #31392, .F. ) ;
#35160 = CARTESIAN_POINT ( 'NONE',  ( -111.1429263765338078, 5.598654528085800663, -7.705886871421367523 ) ) ;
#35161 = CARTESIAN_POINT ( 'NONE',  ( -129.8949999999999818, 6.826472737025116366, 4.959722759717898555 ) ) ;
#35162 = DIRECTION ( 'NONE',  ( 1.000000000000000000, 0.000000000000000000, 0.000000000000000000 ) ) ;
#35164 = DIRECTION ( 'NONE',  ( 0.000000000000000000, 1.000000000000000000, 0.000000000000000000 ) ) ;
#35163 = DIRECTION ( 'NONE',  ( -1.000000000000000000, 0.000000000000000000, 0.000000000000000000 ) ) ;
#35165 = CYLINDRICAL_SURFACE ( 'NONE', #21565, 3.000000000000000444 ) ;
#35166 = EDGE_LOOP ( 'NONE', ( #20832, #37372, #59093, #45758 ) ) ;
#35167 = VERTEX_POINT ( 'NONE', #53609 ) ;
#35168 = AXIS2_PLACEMENT_3D ( 'NONE', #10013, #52928, #4717 ) ;
#35169 = DIRECTION ( 'NONE',  ( 1.000000000000000000, 0.000000000000000000, -3.932039878880752229E-15 ) ) ;
#35170 = DIRECTION ( 'NONE',  ( -0.000000000000000000, -0.000000000000000000, -1.000000000000000000 ) ) ;
#35171 = LINE ( 'NONE', #20016, #68543 ) ;
#35172 = CARTESIAN_POINT ( 'NONE',  ( -8.082903768654762899, 3.463586619550771876E-15, 1.082903768654759125 ) ) ;
#35173 = CARTESIAN_POINT ( 'NONE',  ( -127.5570736234661950, -1.166476076187852838E-15, -9.524999999999991473 ) ) ;
#35174 = ORIENTED_EDGE ( 'NONE', *, *, #1440, .F. ) ;
#35175 = CARTESIAN_POINT ( 'NONE',  ( -128.0049999999999670, 6.826472737025115478, 4.959722759717899443 ) ) ;
#35177 = EDGE_CURVE ( 'NONE', #67453, #32736, #14967, .T. ) ;
#35176 = ORIENTED_EDGE ( 'NONE', *, *, #67691, .F. ) ;
#35178 = CYLINDRICAL_SURFACE ( 'NONE', #20771, 12.50000000000000178 ) ;
#35179 = CARTESIAN_POINT ( 'NONE',  ( -120.9570736234661865, 9.058813317711329915, -2.943386871421373119 ) ) ;
#35180 = EDGE_CURVE ( 'NONE', #26367, #48229, #21597, .T. ) ;
#35181 = ORIENTED_EDGE ( 'NONE', *, *, #46091, .F. ) ;
#35182 = CYLINDRICAL_SURFACE ( 'NONE', #12215, 0.2500000000000002220 ) ;
#35183 = DIRECTION ( 'NONE',  ( 1.000000000000000000, 7.709882115452468306E-16, -0.000000000000000000 ) ) ;
#35184 = VERTEX_POINT ( 'NONE', #58541 ) ;
#35185 = CIRCLE ( 'NONE', #48690, 0.2500000000000002220 ) ;
#35186 = DIRECTION ( 'NONE',  ( -0.7071067811865549002, 8.659560562355022838E-17, 0.7071067811865401342 ) ) ;
#35187 = CARTESIAN_POINT ( 'NONE',  ( -9.058813317711337021, 143.0449999999999875, -2.943386871421374895 ) ) ;
#35188 =( GEOMETRIC_REPRESENTATION_CONTEXT ( 3 ) GLOBAL_UNCERTAINTY_ASSIGNED_CONTEXT ( ( #28462 ) ) GLOBAL_UNIT_ASSIGNED_CONTEXT ( ( #2439, #28518, #29209 ) ) REPRESENTATION_CONTEXT ( 'NONE', 'WORKASPACE' ) );
#35189 = VERTEX_POINT ( 'NONE', #10374 ) ;
#35190 = CARTESIAN_POINT ( 'NONE',  ( -22.25000000000000711, 33.99999999999999289, 3.750000000000000000 ) ) ;
#35192 = EDGE_CURVE ( 'NONE', #27775, #65805, #42759, .T. ) ;
#35191 = CARTESIAN_POINT ( 'NONE',  ( 0.000000000000000000, 137.5549999999999784, -9.525000000000000355 ) ) ;
#35193 = LINE ( 'NONE', #56651, #17098 ) ;
#35194 = DIRECTION ( 'NONE',  ( 0.000000000000000000, 0.000000000000000000, 1.000000000000000000 ) ) ;
#35195 = VERTEX_POINT ( 'NONE', #4345 ) ;
#35196 = CARTESIAN_POINT ( 'NONE',  ( 6.826472737025119919, 115.8929263765338220, 4.959722759717908325 ) ) ;
#35197 = LINE ( 'NONE', #24980, #62573 ) ;
#35198 = SURFACE_STYLE_FILL_AREA ( #40503 ) ;
#35199 = MECHANICAL_DESIGN_GEOMETRIC_PRESENTATION_REPRESENTATION (  '', ( #38606 ), #10552 ) ;
#35200 = VECTOR ( 'NONE', #35861, 1000.000000000000000 ) ;
#35201 = DIRECTION ( 'NONE',  ( -0.000000000000000000, 0.000000000000000000, 1.000000000000000000 ) ) ;
#35202 = DIRECTION ( 'NONE',  ( 0.000000000000000000, 0.000000000000000000, 1.000000000000000000 ) ) ;
#35203 = ORIENTED_EDGE ( 'NONE', *, *, #32637, .F. ) ;
#35204 = LINE ( 'NONE', #30239, #17256 ) ;
#35205 = EDGE_CURVE ( 'NONE', #67406, #53491, #65314, .T. ) ;
#35206 = ORIENTED_EDGE ( 'NONE', *, *, #30172, .T. ) ;
#35207 = DIRECTION ( 'NONE',  ( 0.000000000000000000, -0.000000000000000000, 1.000000000000000000 ) ) ;
#35208 = CARTESIAN_POINT ( 'NONE',  ( -122.3070736234661808, -10.01517768586948698, 6.132527647946031529E-16 ) ) ;
#35209 = CARTESIAN_POINT ( 'NONE',  ( 6.062177826491071286, -3.500000000000002220, 0.000000000000000000 ) ) ;
#35210 = CARTESIAN_POINT ( 'NONE',  ( -165.8050000000000068, -8.437984349512085203, 5.166775262442717831E-16 ) ) ;
#35211 = ORIENTED_EDGE ( 'NONE', *, *, #47839, .F. ) ;
#35212 =( NAMED_UNIT ( * ) PLANE_ANGLE_UNIT ( ) SI_UNIT ( $, .RADIAN. ) );
#35213 = B_SPLINE_CURVE_WITH_KNOTS ( 'NONE', 3,
 ( #33150, #54908, #6736, #5686, #37434, #49324 ),
 .UNSPECIFIED., .F., .F.,
 ( 4, 2, 4 ),
 ( 0.000000000000000000, 0.0003110656624534448192, 0.0006221313249068896383 ),
 .UNSPECIFIED. ) ;
#35214 =( GEOMETRIC_REPRESENTATION_CONTEXT ( 3 ) GLOBAL_UNCERTAINTY_ASSIGNED_CONTEXT ( ( #56023 ) ) GLOBAL_UNIT_ASSIGNED_CONTEXT ( ( #14360, #35830, #3781 ) ) REPRESENTATION_CONTEXT ( 'NONE', 'WORKASPACE' ) );
#35215 = DIRECTION ( 'NONE',  ( -0.000000000000000000, -1.000000000000000000, -0.000000000000000000 ) ) ;
#35216 = EDGE_CURVE ( 'NONE', #19853, #56811, #25828, .T. ) ;
#35217 = CARTESIAN_POINT ( 'NONE',  ( -54.08595089178545123, -9.512283121613346992, 3.449313401996987327 ) ) ;
#35218 =( NAMED_UNIT ( * ) SI_UNIT ( $, .STERADIAN. ) SOLID_ANGLE_UNIT ( ) );
#35219 = DIRECTION ( 'NONE',  ( 0.000000000000000000, 0.000000000000000000, -1.000000000000000000 ) ) ;
#35220 = ORIENTED_EDGE ( 'NONE', *, *, #48408, .F. ) ;
#35221 = DIRECTION ( 'NONE',  ( -0.000000000000000000, -1.000000000000000000, -0.000000000000000000 ) ) ;
#35222 = EDGE_LOOP ( 'NONE', ( #6637, #12670, #56179, #44453 ) ) ;
#35223 = DIRECTION ( 'NONE',  ( 1.300977106640434891E-16, -0.000000000000000000, 1.000000000000000000 ) ) ;
#35224 = CARTESIAN_POINT ( 'NONE',  ( -6.062177826491069510, 2.500000000000000000, 3.499999999999999556 ) ) ;
#35225 = CARTESIAN_POINT ( 'NONE',  ( -72.05499999999997840, -9.827790563157499189E-16, -8.024999999999991473 ) ) ;
#35226 = ORIENTED_EDGE ( 'NONE', *, *, #61863, .F. ) ;
#35227 = AXIS2_PLACEMENT_3D ( 'NONE', #16859, #11204, #6270 ) ;
#35228 = DIRECTION ( 'NONE',  ( -1.000000000000000000, -0.000000000000000000, -0.000000000000000000 ) ) ;
#35229 = AXIS2_PLACEMENT_3D ( 'NONE', #23321, #6443, #27869 ) ;
#35230 = LINE ( 'NONE', #40888, #48178 ) ;
#35231 = FACE_OUTER_BOUND ( 'NONE', #27635, .T. ) ;
#35232 = ORIENTED_EDGE ( 'NONE', *, *, #66159, .F. ) ;
#35233 =( NAMED_UNIT ( * ) PLANE_ANGLE_UNIT ( ) SI_UNIT ( $, .RADIAN. ) );
#35235 = DIRECTION ( 'NONE',  ( 1.000000000000000000, 0.000000000000000000, 0.000000000000000000 ) ) ;
#35234 = CARTESIAN_POINT ( 'NONE',  ( -34.99999999999992895, 109.9999999999999858, 9.500000000000000000 ) ) ;
#35236 = AXIS2_PLACEMENT_3D ( 'NONE', #31085, #27174, #411 ) ;
#35237 = CARTESIAN_POINT ( 'NONE',  ( 3.094860106618435136, 136.2949999999999875, -9.525000000000000355 ) ) ;
#35238 = CARTESIAN_POINT ( 'NONE',  ( -100.6449999999999818, 4.716976649647091513, -6.492361379858946790 ) ) ;
#35239 = CARTESIAN_POINT ( 'NONE',  ( 1.000000000000000000, 43.00000000000000000, 45.61250543006183733 ) ) ;
#35240 = COLOUR_RGB ( '', 0.08235294, 0.09019608, 0.10196078) ;
#35241 = EDGE_CURVE ( 'NONE', #47060, #58906, #42077, .T. ) ;
#35243 = CARTESIAN_POINT ( 'NONE',  ( -183.2510368117331154, 0.000000000000000000, 8.774999999999991473 ) ) ;
#35242 = LINE ( 'NONE', #61595, #24491 ) ;
#35244 = CARTESIAN_POINT ( 'NONE',  ( -146.9929263765338021, 8.102448949553171076, -5.886773742842744461 ) ) ;
#35245 = MECHANICAL_DESIGN_GEOMETRIC_PRESENTATION_REPRESENTATION (  '', ( #19469 ), #32990 ) ;
#35246 = DIRECTION ( 'NONE',  ( 1.000000000000000000, 0.000000000000000000, 0.000000000000000000 ) ) ;
#35247 = CARTESIAN_POINT ( 'NONE',  ( -164.6949999999999648, -8.437984349512085203, 5.166775262442717831E-16 ) ) ;
#35248 = CIRCLE ( 'NONE', #39798, 12.50000000000001066 ) ;
#35249 = AXIS2_PLACEMENT_3D ( 'NONE', #12562, #23150, #55488 ) ;
#35250 = CYLINDRICAL_SURFACE ( 'NONE', #14615, 0.5000000000000004441 ) ;
#35251 =( LENGTH_UNIT ( ) NAMED_UNIT ( * ) SI_UNIT ( .MILLI., .METRE. ) );
#35252 = ORIENTED_EDGE ( 'NONE', *, *, #40775, .F. ) ;
#35253 = DIRECTION ( 'NONE',  ( -0.000000000000000000, -0.000000000000000000, 1.000000000000000000 ) ) ;
#35255 = EDGE_LOOP ( 'NONE', ( #41002, #27538, #65555, #18174 ) ) ;
#35254 = CIRCLE ( 'NONE', #62208, 1.000000000000000000 ) ;
#35256 = CONICAL_SURFACE ( 'NONE', #64485, 8.524999999999977263, 0.7853981633974552734 ) ;
#35257 = VECTOR ( 'NONE', #62774, 1000.000000000000000 ) ;
#35258 = EDGE_CURVE ( 'NONE', #1595, #58900, #22639, .T. ) ;
#35259 = CARTESIAN_POINT ( 'NONE',  ( -184.0000000000000000, 0.000000000000000000, 8.024999999999991473 ) ) ;
#35260 = CARTESIAN_POINT ( 'NONE',  ( -45.00000000000000711, 7.952411872162973516, 6.456960098914690249 ) ) ;
#35261 = CARTESIAN_POINT ( 'NONE',  ( -173.6070736234661638, -8.102448949553174629, 5.886773742842742685 ) ) ;
#35262 = CARTESIAN_POINT ( 'NONE',  ( -2.607480562268989832, 142.2070736234661297, -8.025000000000060751 ) ) ;
#35263 = ORIENTED_EDGE ( 'NONE', *, *, #24758, .F. ) ;
#35264 = CARTESIAN_POINT ( 'NONE',  ( -157.7049999999999557, 2.607480562269072433, 8.024999999999991473 ) ) ;
#35265 = ADVANCED_FACE ( 'NONE', ( #64850, #44148 ), #60271, .T. ) ;
#35266 = PRESENTATION_LAYER_ASSIGNMENT (  '', '', ( #65586 ) ) ;
#35267 = EDGE_CURVE ( 'NONE', #47926, #46046, #37294, .T. ) ;
#35268 = VERTEX_POINT ( 'NONE', #48729 ) ;
#35269 = FILL_AREA_STYLE ('',( #24014 ) ) ;
#35270 = CARTESIAN_POINT ( 'NONE',  ( 27.99999999999998224, 5.000000000000000000, 72.00402776293822171 ) ) ;
#35271 = VERTEX_POINT ( 'NONE', #23327 ) ;
#35272 = COLOUR_RGB ( '', 0.08235294, 0.09019608, 0.10196078) ;
#35273 = CARTESIAN_POINT ( 'NONE',  ( 0.000000000000000000, 114.4999999999999574, 22.50000000000000000 ) ) ;
#35274 = CARTESIAN_POINT ( 'NONE',  ( 6.826472737025119919, 159.0070736234661695, 4.959722759717908325 ) ) ;
#35275 = AXIS2_PLACEMENT_3D ( 'NONE', #3864, #62971, #25348 ) ;
#35276 = ORIENTED_EDGE ( 'NONE', *, *, #31608, .T. ) ;
#35277 = SURFACE_SIDE_STYLE ('',( #24022 ) ) ;
#35279 = EDGE_CURVE ( 'NONE', #58710, #42429, #49729, .T. ) ;
#35278 = CARTESIAN_POINT ( 'NONE',  ( -3.094860106618432471, 113.7049999999999699, -9.525000000000000355 ) ) ;
#35280 = CARTESIAN_POINT ( 'NONE',  ( -72.65499999999998693, -7.632228543268600340, -2.479861379858950166 ) ) ;
#35281 = SURFACE_SIDE_STYLE ('',( #46576 ) ) ;
#35282 = ORIENTED_EDGE ( 'NONE', *, *, #33410, .F. ) ;
#35283 = CARTESIAN_POINT ( 'NONE',  ( 0.000000000000000000, 137.5549999999999784, -9.525000000000000355 ) ) ;
#35284 =( NAMED_UNIT ( * ) PLANE_ANGLE_UNIT ( ) SI_UNIT ( $, .RADIAN. ) );
#35285 = DIRECTION ( 'NONE',  ( 0.000000000000000000, 1.000000000000000000, 0.000000000000000000 ) ) ;
#35286 = EDGE_CURVE ( 'NONE', #53126, #19860, #50319, .T. ) ;
#35287 = SPHERICAL_SURFACE ( 'NONE', #56346, 1.000000000000000000 ) ;
#35288 = PRESENTATION_LAYER_ASSIGNMENT (  '', '', ( #24028 ) ) ;
#35289 =( NAMED_UNIT ( * ) PLANE_ANGLE_UNIT ( ) SI_UNIT ( $, .RADIAN. ) );
#35290 = CARTESIAN_POINT ( 'NONE',  ( -18.25000000000000711, 33.74999999999999289, 4.000000000000000000 ) ) ;
#35291 = ORIENTED_EDGE ( 'NONE', *, *, #38244, .T. ) ;
#35293 =( NAMED_UNIT ( * ) PLANE_ANGLE_UNIT ( ) SI_UNIT ( $, .RADIAN. ) );
#35292 = AXIS2_PLACEMENT_3D ( 'NONE', #44599, #29759, #6910 ) ;
#35294 = SURFACE_STYLE_USAGE ( .BOTH. , #61313 ) ;
#35295 = CARTESIAN_POINT ( 'NONE',  ( -50.54499999999998039, -7.632228543268600340, -2.479861379858950166 ) ) ;
#35296 = ORIENTED_EDGE ( 'NONE', *, *, #11718, .T. ) ;
#35297 = PRESENTATION_STYLE_ASSIGNMENT (( #65911 ) ) ;
#35298 = COLOUR_RGB ( '', 0.66274510, 0.83137255, 0.94901961) ;
#35299 = LINE ( 'NONE', #45189, #41411 ) ;
#35300 = DIRECTION ( 'NONE',  ( -0.000000000000000000, -0.000000000000000000, -1.000000000000000000 ) ) ;
#35301 = SPHERICAL_SURFACE ( 'NONE', #59918, 1.000000000000000000 ) ;
#35302 = ORIENTED_EDGE ( 'NONE', *, *, #50611, .T. ) ;
#35303 = CARTESIAN_POINT ( 'NONE',  ( -58.04499999999998749, 7.632228543268600340, 2.479861379858949277 ) ) ;
#35304 = VERTEX_POINT ( 'NONE', #32851 ) ;
#35305 = STYLED_ITEM ( 'NONE', ( #42330 ), #30399 ) ;
#35306 = CARTESIAN_POINT ( 'NONE',  ( 4.000000000000002665, 38.93969262078591242, -89.65797985667433068 ) ) ;
#35307 = CARTESIAN_POINT ( 'NONE',  ( -102.0549999999999926, -9.827790563157499189E-16, -8.024999999999991473 ) ) ;
#35308 = ORIENTED_EDGE ( 'NONE', *, *, #66953, .T. ) ;
#35309 = ADVANCED_FACE ( 'NONE', ( #27188 ), #5794, .F. ) ;
#35310 = CARTESIAN_POINT ( 'NONE',  ( 0.000000000000000000, -2.500000000000000000, 0.000000000000000000 ) ) ;
#35311 = SURFACE_STYLE_USAGE ( .BOTH. , #40250 ) ;
#35312 = CARTESIAN_POINT ( 'NONE',  ( -136.8570736234661638, -5.598654528085803328, -7.705886871421366635 ) ) ;
#35313 =( GEOMETRIC_REPRESENTATION_CONTEXT ( 3 ) GLOBAL_UNCERTAINTY_ASSIGNED_CONTEXT ( ( #51545 ) ) GLOBAL_UNIT_ASSIGNED_CONTEXT ( ( #11998, #5319, #10626 ) ) REPRESENTATION_CONTEXT ( 'NONE', 'WORKASPACE' ) );
#35314 = EDGE_CURVE ( 'NONE', #40876, #51672, #6112, .T. ) ;
#35315 = CARTESIAN_POINT ( 'NONE',  ( 0.000000000000000000, 0.000000000000000000, -4.000000000000000000 ) ) ;
#35316 = CARTESIAN_POINT ( 'NONE',  ( 8.102448949553179958, 141.3949999999999818, 5.886773742842750679 ) ) ;
#35317 = CARTESIAN_POINT ( 'NONE',  ( -72.50707362346616947, 8.102448949553176405, 5.886773742842740909 ) ) ;
#35318 = COLOUR_RGB ( '', 0.66274510, 0.83137255, 0.94901961) ;
#35319 = MECHANICAL_DESIGN_GEOMETRIC_PRESENTATION_REPRESENTATION (  '', ( #30774 ), #64488 ) ;
#35320 = CARTESIAN_POINT ( 'NONE',  ( -72.44292637653379074, -1.166476076187852838E-15, -9.524999999999991473 ) ) ;
#35321 = CARTESIAN_POINT ( 'NONE',  ( 11.00000000000001776, 26.00000000000000355, 27.49999999999999645 ) ) ;
#35322 = DIRECTION ( 'NONE',  ( 0.000000000000000000, 0.000000000000000000, -1.000000000000000000 ) ) ;
#35323 = CARTESIAN_POINT ( 'NONE',  ( 8.437984349512095861, 120.3070736234661382, 1.550032578732816828E-15 ) ) ;
#35324 = AXIS2_PLACEMENT_3D ( 'NONE', #47925, #19736, #69326 ) ;
#35325 = CARTESIAN_POINT ( 'NONE',  ( -123.9549999999999841, -7.632228543268599452, 2.479861379858951054 ) ) ;
#35326 = CARTESIAN_POINT ( 'NONE',  ( 23.85435327029094665, 24.60286873851424261, -27.21019326824331230 ) ) ;
#35327 = CARTESIAN_POINT ( 'NONE',  ( 5.598654528085805993, 111.2449999999999761, 7.705886871421374629 ) ) ;
#35328 = CARTESIAN_POINT ( 'NONE',  ( -137.3950000000000102, -6.826472737025115478, -4.959722759717899443 ) ) ;
#35329 = CIRCLE ( 'NONE', #39876, 3.000000000000000444 ) ;
#35330 = CARTESIAN_POINT ( 'NONE',  ( -118.0450000000000017, 7.632228543268600340, 2.479861379858949277 ) ) ;
#35331 = DIRECTION ( 'NONE',  ( 0.000000000000000000, 0.000000000000000000, 1.000000000000000000 ) ) ;
#35332 = ORIENTED_EDGE ( 'NONE', *, *, #22847, .F. ) ;
#35333 = CARTESIAN_POINT ( 'NONE',  ( -146.7570736234661695, -5.598654528085801552, 7.705886871421367523 ) ) ;
#35334 = FACE_OUTER_BOUND ( 'NONE', #4123, .T. ) ;
#35335 = CARTESIAN_POINT ( 'NONE',  ( -121.1929263765337907, -10.01517768586948698, 6.132527647946031529E-16 ) ) ;
#35336 = CARTESIAN_POINT ( 'NONE',  ( -168.1429263765338078, 5.598654528085800663, -7.705886871421367523 ) ) ;
#35337 = CARTESIAN_POINT ( 'NONE',  ( -49.79499999999998039, 2.607480562269068880, -8.024999999999993250 ) ) ;
#35338 =( GEOMETRIC_REPRESENTATION_CONTEXT ( 3 ) GLOBAL_UNCERTAINTY_ASSIGNED_CONTEXT ( ( #51038 ) ) GLOBAL_UNIT_ASSIGNED_CONTEXT ( ( #55225, #22902, #60847 ) ) REPRESENTATION_CONTEXT ( 'NONE', 'WORKASPACE' ) );
#35339 =( NAMED_UNIT ( * ) SI_UNIT ( $, .STERADIAN. ) SOLID_ANGLE_UNIT ( ) );
#35340 = EDGE_CURVE ( 'NONE', #48195, #30995, #34922, .T. ) ;
#35341 = COLOUR_RGB ( '', 0.08235294, 0.09019608, 0.10196078) ;
#35342 = DIRECTION ( 'NONE',  ( 0.000000000000000000, 1.000000000000000000, -0.000000000000000000 ) ) ;
#35343 = CARTESIAN_POINT ( 'NONE',  ( 22.00000000000000355, 43.00000000000000000, -90.00000000000000000 ) ) ;
#35344 = ORIENTED_EDGE ( 'NONE', *, *, #13979, .F. ) ;
#35345 = CARTESIAN_POINT ( 'NONE',  ( -87.29292637653381348, 3.094860106618428031, -9.524999999999993250 ) ) ;
#35346 = ITEM_DEFINED_TRANSFORMATION ( 'NONE', 'NONE', #21390,  #42840 ) ;
#35347 = AXIS2_PLACEMENT_3D ( 'NONE', #20199, #52253, #36058 ) ;
#35348 = DIRECTION ( 'NONE',  ( 1.000000000000000000, 0.000000000000000000, 0.000000000000000000 ) ) ;
#35349 =( LENGTH_UNIT ( ) NAMED_UNIT ( * ) SI_UNIT ( .MILLI., .METRE. ) );
#35350 = ADVANCED_FACE ( 'NONE', ( #8554 ), #2866, .T. ) ;
#35351 = STYLED_ITEM ( 'NONE', ( #51336 ), #31604 ) ;
#35352 = CARTESIAN_POINT ( 'NONE',  ( -179.8429263765338249, 9.058813317711329915, -2.943386871421373119 ) ) ;
#35353 = DIRECTION ( 'NONE',  ( 0.000000000000000000, -0.000000000000000000, 1.000000000000000000 ) ) ;
#35354 = DIRECTION ( 'NONE',  ( 0.000000000000000000, 0.000000000000000000, 1.000000000000000000 ) ) ;
#35355 = EDGE_CURVE ( 'NONE', #30255, #1355, #31673, .T. ) ;
#35356 = ORIENTED_EDGE ( 'NONE', *, *, #63543, .F. ) ;
#35357 = CARTESIAN_POINT ( 'NONE',  ( 5.885195493260862776, 3.806542393196805651, -4.285986713106759716E-16 ) ) ;
#35358 = DIRECTION ( 'NONE',  ( -1.000000000000000000, 7.709882115452468306E-16, 0.000000000000000000 ) ) ;
#35359 = CARTESIAN_POINT ( 'NONE',  ( 31.00000000000000711, 42.00000000000000000, -36.50000000000000000 ) ) ;
#35360 = ORIENTED_EDGE ( 'NONE', *, *, #35205, .F. ) ;
#35361 = DIRECTION ( 'NONE',  ( 1.000000000000000000, 0.000000000000000000, 0.000000000000000000 ) ) ;
#35362 = CYLINDRICAL_SURFACE ( 'NONE', #29716, 1.000000000000000888 ) ;
#35363 = CARTESIAN_POINT ( 'NONE',  ( 4.716976649647096842, 128.8570736234661638, 6.492361379858953896 ) ) ;
#35364 = VECTOR ( 'NONE', #1696, 1000.000000000000000 ) ;
#35365 = MECHANICAL_DESIGN_GEOMETRIC_PRESENTATION_REPRESENTATION (  '', ( #22919 ), #1554 ) ;
#35366 = VERTEX_POINT ( 'NONE', #56370 ) ;
#35367 = CARTESIAN_POINT ( 'NONE',  ( 60.00000000000000000, 1.797044900979284448E-15, 6.999999999999988454 ) ) ;
#35368 = CARTESIAN_POINT ( 'NONE',  ( -107.6049999999999756, 6.826472737025113702, -4.959722759717902107 ) ) ;
#35369 = SURFACE_SIDE_STYLE ('',( #44907 ) ) ;
#35370 = SURFACE_STYLE_USAGE ( .BOTH. , #44574 ) ;
#35371 = ORIENTED_EDGE ( 'NONE', *, *, #66901, .F. ) ;
#35372 = CARTESIAN_POINT ( 'NONE',  ( 10.00000000000000533, 50.00000000000000000, -46.00000000000000000 ) ) ;
#35373 = EDGE_CURVE ( 'NONE', #68534, #69071, #60944, .T. ) ;
#35374 = CYLINDRICAL_SURFACE ( 'NONE', #22625, 0.2500000000000002220 ) ;
#35375 = DIRECTION ( 'NONE',  ( -1.000000000000000000, 0.000000000000000000, 0.000000000000000000 ) ) ;
#35376 = CIRCLE ( 'NONE', #5037, 10.50000000000000178 ) ;
#35377 = AXIS2_PLACEMENT_3D ( 'NONE', #26259, #31177, #10103 ) ;
#35378 = CARTESIAN_POINT ( 'NONE',  ( -9.250000000000003553, 27.74999999999998934, -3.750000000000000000 ) ) ;
#35379 = CARTESIAN_POINT ( 'NONE',  ( -78.59499999999999886, 2.607480562269073321, 8.024999999999991473 ) ) ;
#35380 = ORIENTED_EDGE ( 'NONE', *, *, #18682, .T. ) ;
#35381 = CARTESIAN_POINT ( 'NONE',  ( -24.75000000000000355, 36.75000000000000000, -3.000000000000000000 ) ) ;
#35382 = CARTESIAN_POINT ( 'NONE',  ( 57.49999999999998579, 30.99999999999999289, 3.750000000000000000 ) ) ;
#35383 = UNCERTAINTY_MEASURE_WITH_UNIT (LENGTH_MEASURE( 1.000000000000000082E-05 ), #51450, 'distance_accuracy_value', 'NONE');
#35384 = ORIENTED_EDGE ( 'NONE', *, *, #667, .F. ) ;
#35385 = CARTESIAN_POINT ( 'NONE',  ( -75.44292637653379074, -1.166476076187852838E-15, -9.524999999999991473 ) ) ;
#35386 = CARTESIAN_POINT ( 'NONE',  ( -5.000000000000000000, 0.000000000000000000, 0.2500000000000011102 ) ) ;
#35387 = AXIS2_PLACEMENT_3D ( 'NONE', #4207, #14817, #4572 ) ;
#35388 = CARTESIAN_POINT ( 'NONE',  ( 44.99999999999998579, 119.9999999999999716, -9.500000000000000000 ) ) ;
#35389 = AXIS2_PLACEMENT_3D ( 'NONE', #54451, #7571, #13181 ) ;
#35390 = FACE_OUTER_BOUND ( 'NONE', #17065, .T. ) ;
#35391 = EDGE_LOOP ( 'NONE', ( #5691, #22617, #32692, #13914 ) ) ;
#35392 = ORIENTED_EDGE ( 'NONE', *, *, #10768, .T. ) ;
#35393 = DIRECTION ( 'NONE',  ( 1.000000000000000000, 0.000000000000000000, 0.000000000000000000 ) ) ;
#35394 = CARTESIAN_POINT ( 'NONE',  ( -41.49999999999998579, 106.9282032302754999, -3.500000000000000000 ) ) ;
#35395 = CARTESIAN_POINT ( 'NONE',  ( 3.728455551739337626, -1.573594397639262343, 6.999999999999999112 ) ) ;
#35396 = CARTESIAN_POINT ( 'NONE',  ( -174.3570736234661638, 5.598654528085804216, 7.705886871421366635 ) ) ;
#35397 = CARTESIAN_POINT ( 'NONE',  ( -12.94269599874522214, 56.39257344741367461, 6.552927311739624727 ) ) ;
#35398 = CARTESIAN_POINT ( 'NONE',  ( -5.598654528085808657, 116.6449999999999818, 7.705886871421373741 ) ) ;
#35399 =( GEOMETRIC_REPRESENTATION_CONTEXT ( 3 ) GLOBAL_UNCERTAINTY_ASSIGNED_CONTEXT ( ( #39778 ) ) GLOBAL_UNIT_ASSIGNED_CONTEXT ( ( #12068, #22994, #65894 ) ) REPRESENTATION_CONTEXT ( 'NONE', 'WORKASPACE' ) );
#35400 = CARTESIAN_POINT ( 'NONE',  ( -111.2070736234661865, 3.094860106618433360, 9.524999999999991473 ) ) ;
#35401 = CARTESIAN_POINT ( 'NONE',  ( -83.49999999999998579, 4.336808689942018722E-16, 24.00000000000000000 ) ) ;
#35402 = PRESENTATION_LAYER_ASSIGNMENT (  '', '', ( #48888 ) ) ;
#35403 = ORIENTED_EDGE ( 'NONE', *, *, #17131, .F. ) ;
#35404 =( BOUNDED_CURVE ( )  B_SPLINE_CURVE ( 2, ( #5533, #15794, #54086, #59347, #33339, #44289, #37973, #10509, #10845, #27337, #49529 ),
 .UNSPECIFIED., .F., .F. ) 
 B_SPLINE_CURVE_WITH_KNOTS ( ( 3, 2, 2, 2, 2, 3 ),
 ( 0.2941176470588235392, 0.2999999999999999889, 0.3058823529411764941, 0.3117647058823529438, 0.3176470588235293935, 0.3235294117647058987 ),
 .UNSPECIFIED. ) 
 CURVE ( )  GEOMETRIC_REPRESENTATION_ITEM ( )  RATIONAL_B_SPLINE_CURVE ( ( 1.000000000000000000, 0.9510565162951535312, 1.000000000000000000, 0.9510565162951535312, 1.000000000000000000, 0.9510565162951535312, 1.000000000000000000, 0.9510565162951535312, 1.000000000000000000, 0.9510565162951535312, 1.000000000000000000 ) ) 
 REPRESENTATION_ITEM ( '' )  );
#35405 = SURFACE_STYLE_USAGE ( .BOTH. , #52632 ) ;
#35406 = LINE ( 'NONE', #51932, #51193 ) ;
#35408 = FILL_AREA_STYLE ('',( #3331 ) ) ;
#35407 = CARTESIAN_POINT ( 'NONE',  ( 5.196152422706629359, 9.000000000000008882, 1.392304845413260272 ) ) ;
#35409 = CARTESIAN_POINT ( 'NONE',  ( -152.7549999999999955, 4.716976649647091513, -6.492361379858946790 ) ) ;
#35410 = DIRECTION ( 'NONE',  ( 1.000000000000000000, -0.000000000000000000, -0.000000000000000000 ) ) ;
#35411 = CARTESIAN_POINT ( 'NONE',  ( -7.971148328998627797, 111.3190071099407845, -3.524084523217378973 ) ) ;
#35412 = CARTESIAN_POINT ( 'NONE',  ( -161.9950000000000045, -6.826472737025115478, 4.959722759717900331 ) ) ;
#35413 = CARTESIAN_POINT ( 'NONE',  ( -146.3950000000000102, -6.826472737025113702, -4.959722759717900331 ) ) ;
#35414 = ORIENTED_EDGE ( 'NONE', *, *, #44036, .F. ) ;
#35415 = AXIS2_PLACEMENT_3D ( 'NONE', #36000, #24716, #42365 ) ;
#35416 = CARTESIAN_POINT ( 'NONE',  ( -10.39230484541327293, 3.364658241569156409E-15, 1.392304845413260939 ) ) ;
#35417 = CIRCLE ( 'NONE', #16359, 0.5000000000000004441 ) ;
#35418 = CARTESIAN_POINT ( 'NONE',  ( 26.00000000000001066, 21.99999999999998224, 3.750000000000000000 ) ) ;
#35419 = FACE_OUTER_BOUND ( 'NONE', #5266, .T. ) ;
#35420 = CARTESIAN_POINT ( 'NONE',  ( -63.95499999999998408, -7.632228543268599452, 2.479861379858951054 ) ) ;
#35421 = DIRECTION ( 'NONE',  ( 1.000000000000000000, -0.000000000000000000, 0.000000000000000000 ) ) ;
#35422 =( NAMED_UNIT ( * ) SI_UNIT ( $, .STERADIAN. ) SOLID_ANGLE_UNIT ( ) );
#35423 = COLOUR_RGB ( '', 0.09019608, 0.27058824, 0.51372549) ;
#35424 = CARTESIAN_POINT ( 'NONE',  ( -61.79499999999998039, 2.607480562269069324, -8.024999999999993250 ) ) ;
#35425 = CARTESIAN_POINT ( 'NONE',  ( -9.058813317711337021, 153.1549999999999727, -2.943386871421374895 ) ) ;
#35426 = CARTESIAN_POINT ( 'NONE',  ( -143.6070736234661354, -8.102448949553174629, 5.886773742842742685 ) ) ;
#35427 = EDGE_CURVE ( 'NONE', #6580, #38434, #10350, .T. ) ;
#35428 = AXIS2_PLACEMENT_3D ( 'NONE', #6970, #28393, #60761 ) ;
#35429 = CIRCLE ( 'NONE', #55654, 0.5000000000000004441 ) ;
#35430 = CARTESIAN_POINT ( 'NONE',  ( 24.21231517720798010, 113.4999999999999858, -7.500000000000000000 ) ) ;
#35431 = UNCERTAINTY_MEASURE_WITH_UNIT (LENGTH_MEASURE( 1.000000000000000082E-05 ), #35504, 'distance_accuracy_value', 'NONE');
#35432 =( BOUNDED_CURVE ( )  B_SPLINE_CURVE ( 3, ( #34326, #13544, #39987, #45264 ),
 .UNSPECIFIED., .F., .F. ) 
 B_SPLINE_CURVE_WITH_KNOTS ( ( 4, 4 ),
 ( 4.712388980384687898, 5.445427266222307772 ),
 .UNSPECIFIED. ) 
 CURVE ( )  GEOMETRIC_REPRESENTATION_ITEM ( )  RATIONAL_B_SPLINE_CURVE ( ( 1.000000000000000000, 0.9557202843314677176, 0.9557202843314677176, 1.000000000000000000 ) ) 
 REPRESENTATION_ITEM ( '' )  );
#35433 = CARTESIAN_POINT ( 'NONE',  ( 1.000000000000000888, 43.00000000000000000, -45.61250543006183733 ) ) ;
#35434 = DIRECTION ( 'NONE',  ( 1.000000000000000000, -1.189524669241239115E-16, -0.000000000000000000 ) ) ;
#35435 = AXIS2_PLACEMENT_3D ( 'NONE', #17718, #66222, #2129 ) ;
#35436 = PLANE ( 'NONE',  #42876 ) ;
#35437 = EDGE_CURVE ( 'NONE', #65858, #22750, #52190, .T. ) ;
#35438 = ADVANCED_FACE ( 'NONE', ( #16191 ), #8075, .T. ) ;
#35439 = STYLED_ITEM ( 'NONE', ( #59493 ), #57848 ) ;
#35440 = CARTESIAN_POINT ( 'NONE',  ( 26.00000000000001776, 14.00000000000000000, -34.49999999999999289 ) ) ;
#35441 = ORIENTED_EDGE ( 'NONE', *, *, #29173, .F. ) ;
#35442 = VERTEX_POINT ( 'NONE', #923 ) ;
#35443 = DIRECTION ( 'NONE',  ( 1.000000000000000000, 0.000000000000000000, 0.000000000000000000 ) ) ;
#35444 = ADVANCED_FACE ( 'NONE', ( #21425 ), #6611, .F. ) ;
#35446 =( LENGTH_UNIT ( ) NAMED_UNIT ( * ) SI_UNIT ( .MILLI., .METRE. ) );
#35445 = AXIS2_PLACEMENT_3D ( 'NONE', #15922, #53528, #69026 ) ;
#35447 = EDGE_CURVE ( 'NONE', #2934, #25731, #42921, .T. ) ;
#35448 = AXIS2_PLACEMENT_3D ( 'NONE', #8262, #40634, #14941 ) ;
#35449 = SPHERICAL_SURFACE ( 'NONE', #60880, 0.2500000000000000000 ) ;
#35450 = ORIENTED_EDGE ( 'NONE', *, *, #359, .F. ) ;
#35451 = ORIENTED_EDGE ( 'NONE', *, *, #25327, .T. ) ;
#35452 = FACE_OUTER_BOUND ( 'NONE', #57453, .T. ) ;
#35453 = ADVANCED_FACE ( 'NONE', ( #53775 ), #16877, .F. ) ;
#35454 = ORIENTED_EDGE ( 'NONE', *, *, #495, .F. ) ;
#35455 = CARTESIAN_POINT ( 'NONE',  ( -64.94292637653380496, 0.000000000000000000, 9.524999999999991473 ) ) ;
#35456 = DIRECTION ( 'NONE',  ( 0.000000000000000000, 0.000000000000000000, -1.000000000000000000 ) ) ;
#35457 = ORIENTED_EDGE ( 'NONE', *, *, #29790, .T. ) ;
#35458 = DIRECTION ( 'NONE',  ( 1.000000000000000000, 0.000000000000000000, 0.000000000000000000 ) ) ;
#35459 = DIRECTION ( 'NONE',  ( 0.000000000000000000, 0.000000000000000000, 1.000000000000000000 ) ) ;
#35460 = CARTESIAN_POINT ( 'NONE',  ( -112.0449999999999875, 7.632228543268600340, 2.479861379858949277 ) ) ;
#35461 = ORIENTED_EDGE ( 'NONE', *, *, #28305, .F. ) ;
#35462 = DIRECTION ( 'NONE',  ( 0.000000000000000000, -0.8090169943749472292, -0.5877852522924733591 ) ) ;
#35463 = CARTESIAN_POINT ( 'NONE',  ( 23.21231517720798010, 1.797044900979284448E-15, -9.500000000000000000 ) ) ;
#35464 = DIRECTION ( 'NONE',  ( -1.000000000000000000, -7.080503983578803083E-17, 0.000000000000000000 ) ) ;
#35465 = ORIENTED_EDGE ( 'NONE', *, *, #31927, .F. ) ;
#35466 = CARTESIAN_POINT ( 'NONE',  ( -7.632228543268608334, 147.8429263765338249, 2.479861379858952830 ) ) ;
#35467 = VECTOR ( 'NONE', #12608, 999.9999999999998863 ) ;
#35468 =( NAMED_UNIT ( * ) PLANE_ANGLE_UNIT ( ) SI_UNIT ( $, .RADIAN. ) );
#35469 = VERTEX_POINT ( 'NONE', #23493 ) ;
#35470 = CARTESIAN_POINT ( 'NONE',  ( -23.71231517720798010, 112.9999999999999858, -7.500000000000000000 ) ) ;
#35471 = VERTEX_POINT ( 'NONE', #18588 ) ;
#35472 = CARTESIAN_POINT ( 'NONE',  ( 57.74999999999998579, 30.74999999999999289, -4.000000000000000000 ) ) ;
#35473 = CARTESIAN_POINT ( 'NONE',  ( -20.54906699372407530, 114.6596276111864654, 10.28538896680104209 ) ) ;
#35474 = CARTESIAN_POINT ( 'NONE',  ( -67.49999999999998579, -1.929132118054077781E-14, 12.00000000000000000 ) ) ;
#35475 = CARTESIAN_POINT ( 'NONE',  ( -125.9049999999999869, 2.607480562269068880, -8.024999999999993250 ) ) ;
#35476 = CARTESIAN_POINT ( 'NONE',  ( 30.25000000000000711, 18.99999999999997868, -3.750000000000000000 ) ) ;
#35477 = CARTESIAN_POINT ( 'NONE',  ( 8.437984349512095861, 141.3070736234661808, 1.550032578732816828E-15 ) ) ;
#35478 = DIRECTION ( 'NONE',  ( 0.000000000000000000, 0.000000000000000000, 1.000000000000000000 ) ) ;
#35479 = DIRECTION ( 'NONE',  ( 0.000000000000000000, 0.000000000000000000, 1.000000000000000000 ) ) ;
#35480 = CARTESIAN_POINT ( 'NONE',  ( -4.250000000000001776, 21.74999999999998579, -3.750000000000000000 ) ) ;
#35481 = ORIENTED_EDGE ( 'NONE', *, *, #52543, .F. ) ;
#35482 = EDGE_LOOP ( 'NONE', ( #31145, #50581, #14723, #67949, #2153, #53464, #65102, #35871, #20510, #59729 ) ) ;
#35483 = DIRECTION ( 'NONE',  ( -0.000000000000000000, -0.000000000000000000, -1.000000000000000000 ) ) ;
#35484 = CARTESIAN_POINT ( 'NONE',  ( -32.56443198604022626, -8.762778093175665362, -2.499999999999996891 ) ) ;
#35485 = CARTESIAN_POINT ( 'NONE',  ( 4.750000000000002665, 24.74999999999998579, 3.750000000000000000 ) ) ;
#35486 = DIRECTION ( 'NONE',  ( 0.000000000000000000, 0.000000000000000000, 1.000000000000000000 ) ) ;
#35487 = ORIENTED_EDGE ( 'NONE', *, *, #17449, .T. ) ;
#35488 = DIRECTION ( 'NONE',  ( 0.000000000000000000, 1.000000000000000000, 0.000000000000000000 ) ) ;
#35489 = CARTESIAN_POINT ( 'NONE',  ( -176.9050000000000011, 2.607480562269068880, -8.024999999999993250 ) ) ;
#35490 = PRESENTATION_STYLE_ASSIGNMENT (( #62206 ) ) ;
#35491 = VECTOR ( 'NONE', #19713, 1000.000000000000000 ) ;
#35492 = CARTESIAN_POINT ( 'NONE',  ( -56.15707362346616804, -9.058813317711329915, -2.943386871421370898 ) ) ;
#35493 = AXIS2_PLACEMENT_3D ( 'NONE', #48670, #59157, #16978 ) ;
#35494 = CARTESIAN_POINT ( 'NONE',  ( -175.4949999999999761, 6.826472737025113702, -4.959722759717902107 ) ) ;
#35495 = CARTESIAN_POINT ( 'NONE',  ( 41.72781494893835230, 107.4000720140338387, 3.999999999999999112 ) ) ;
#35496 = CIRCLE ( 'NONE', #61334, 1.000000000000000888 ) ;
#35497 = ORIENTED_EDGE ( 'NONE', *, *, #35216, .F. ) ;
#35498 = DIRECTION ( 'NONE',  ( -1.000000000000000000, -0.000000000000000000, -0.000000000000000000 ) ) ;
#35499 =( NAMED_UNIT ( * ) PLANE_ANGLE_UNIT ( ) SI_UNIT ( $, .RADIAN. ) );
#35500 =( GEOMETRIC_REPRESENTATION_CONTEXT ( 3 ) GLOBAL_UNCERTAINTY_ASSIGNED_CONTEXT ( ( #69378 ) ) GLOBAL_UNIT_ASSIGNED_CONTEXT ( ( #7476, #11711, #54938 ) ) REPRESENTATION_CONTEXT ( 'NONE', 'WORKASPACE' ) );
#35501 = FILL_AREA_STYLE ('',( #55904 ) ) ;
#35502 = CARTESIAN_POINT ( 'NONE',  ( -89.30499999999999261, 8.437984349512085203, -1.550032578732815448E-15 ) ) ;
#35503 = CARTESIAN_POINT ( 'NONE',  ( 9.158309064922752540, 154.5000000000000568, -2.653638227437481678 ) ) ;
#35504 =( LENGTH_UNIT ( ) NAMED_UNIT ( * ) SI_UNIT ( .MILLI., .METRE. ) );
#35505 =( NAMED_UNIT ( * ) PLANE_ANGLE_UNIT ( ) SI_UNIT ( $, .RADIAN. ) );
#35506 = CARTESIAN_POINT ( 'NONE',  ( -93.89499999999996760, 6.826472737025115478, 4.959722759717899443 ) ) ;
#35507 = CARTESIAN_POINT ( 'NONE',  ( -5.598654528085806881, 128.8549999999999898, -7.705886871421374629 ) ) ;
#35508 = CARTESIAN_POINT ( 'NONE',  ( -67.64499999999998181, 4.716976649647091513, -6.492361379858946790 ) ) ;
#35509 = CARTESIAN_POINT ( 'NONE',  ( 18.25000000000000711, 33.74999999999999289, 3.750000000000000000 ) ) ;
#35510 = ADVANCED_FACE ( 'NONE', ( #51284 ), #65362, .T. ) ;
#35511 = FACE_OUTER_BOUND ( 'NONE', #36568, .T. ) ;
#35512 = B_SPLINE_CURVE_WITH_KNOTS ( 'NONE', 3,
 ( #11497, #48838, #532, #22061 ),
 .UNSPECIFIED., .F., .F.,
 ( 4, 4 ),
 ( -4.672407068502317808E-06, 0.0001893522667583549335 ),
 .UNSPECIFIED. ) ;
#35513 = UNCERTAINTY_MEASURE_WITH_UNIT (LENGTH_MEASURE( 1.000000000000000082E-05 ), #8407, 'distance_accuracy_value', 'NONE');
#35514 = ADVANCED_FACE ( 'NONE', ( #44665 ), #28407, .T. ) ;
#35515 = CIRCLE ( 'NONE', #41164, 5.000000000000004441 ) ;
#35516 = CARTESIAN_POINT ( 'NONE',  ( 4.000000000000002665, 38.70020753820971748, -89.00000000000000000 ) ) ;
#35517 = VERTEX_POINT ( 'NONE', #66058 ) ;
#35518 = CARTESIAN_POINT ( 'NONE',  ( -110.8429263765337964, 9.058813317711329915, -2.943386871421373119 ) ) ;
#35519 = CARTESIAN_POINT ( 'NONE',  ( -126.4450000000000074, 0.000000000000000000, 8.024999999999991473 ) ) ;
#35520 = DIRECTION ( 'NONE',  ( 0.9544448354272550006, -0.2817348470284508077, -0.09828800586081520851 ) ) ;
#35521 = EDGE_CURVE ( 'NONE', #149, #51718, #17891, .T. ) ;
#35522 = AXIS2_PLACEMENT_3D ( 'NONE', #33313, #32589, #17824 ) ;
#35523 = CARTESIAN_POINT ( 'NONE',  ( 21.50000000000001066, 24.99999999999998579, 3.750000000000000000 ) ) ;
#35524 = EDGE_CURVE ( 'NONE', #17063, #20808, #7663, .T. ) ;
#35526 = CARTESIAN_POINT ( 'NONE',  ( 57.00000000000000000, 0.000000000000000000, 60.00402776293825724 ) ) ;
#35525 = CARTESIAN_POINT ( 'NONE',  ( 8.437984349512095861, 135.3070736234661524, 1.550032578732816828E-15 ) ) ;
#35527 = VECTOR ( 'NONE', #55338, 1000.000000000000000 ) ;
#35528 = DIRECTION ( 'NONE',  ( 1.000000000000000000, 8.881784197001252323E-16, 0.000000000000000000 ) ) ;
#35529 = ORIENTED_EDGE ( 'NONE', *, *, #49747, .T. ) ;
#35530 = VERTEX_POINT ( 'NONE', #55518 ) ;
#35531 = CARTESIAN_POINT ( 'NONE',  ( -44.50000000000000000, 9.499999999999980460, 3.000000000000000000 ) ) ;
#35532 =( BOUNDED_CURVE ( )  B_SPLINE_CURVE ( 2, ( #1506, #61336, #29687, #13490, #7199, #13145, #34600, #56056, #34961, #50122, #7872 ),
 .UNSPECIFIED., .F., .F. ) 
 B_SPLINE_CURVE_WITH_KNOTS ( ( 3, 2, 2, 2, 2, 3 ),
 ( 0.6413043478260718189, 0.6434782608695499562, 0.6456521739130283155, 0.6478260869565064528, 0.6499999999999847011, 0.6521739130434628384 ),
 .UNSPECIFIED. ) 
 CURVE ( )  GEOMETRIC_REPRESENTATION_ITEM ( )  RATIONAL_B_SPLINE_CURVE ( ( 1.000000000000339950, 0.9510565162948135809, 1.000000000000000000, 0.9510565162951535312, 1.000000000000000000, 0.9510565162951535312, 1.000000000000000000, 0.9510565162951535312, 1.000000000000000000, 0.9510565162955009200, 0.9999999999996526112 ) ) 
 REPRESENTATION_ITEM ( '' )  );
#35533 = ADVANCED_FACE ( 'NONE', ( #45005 ), #12591, .T. ) ;
#35534 = CARTESIAN_POINT ( 'NONE',  ( -98.15707362346617515, -9.058813317711329915, -2.943386871421370898 ) ) ;
#35535 = DIRECTION ( 'NONE',  ( 1.000000000000000000, 0.000000000000000000, 0.000000000000000000 ) ) ;
#35536 = CARTESIAN_POINT ( 'NONE',  ( -126.5070736234661979, 8.102448949553176405, 5.886773742842740909 ) ) ;
#35537 = ORIENTED_EDGE ( 'NONE', *, *, #23333, .F. ) ;
#35538 = CARTESIAN_POINT ( 'NONE',  ( -132.6550000000000011, -7.632228543268600340, -2.479861379858950166 ) ) ;
#35539 = ORIENTED_EDGE ( 'NONE', *, *, #20001, .F. ) ;
#35540 = CARTESIAN_POINT ( 'NONE',  ( 67.50000000000000000, 1.797044900979284448E-15, -12.00000000000000000 ) ) ;
#35541 = VECTOR ( 'NONE', #23841, 1000.000000000000000 ) ;
#35542 = CARTESIAN_POINT ( 'NONE',  ( -118.8570736234661780, -5.598654528085803328, -7.705886871421366635 ) ) ;
#35543 = ORIENTED_EDGE ( 'NONE', *, *, #39352, .F. ) ;
#35544 = CYLINDRICAL_SURFACE ( 'NONE', #44871, 4.999999999999990230 ) ;
#35545 = DIRECTION ( 'NONE',  ( 0.000000000000000000, 1.000000000000000000, 0.000000000000000000 ) ) ;
#35546 = ORIENTED_EDGE ( 'NONE', *, *, #14538, .T. ) ;
#35547 = AXIS2_PLACEMENT_3D ( 'NONE', #1836, #25768, #62695 ) ;
#35548 = DIRECTION ( 'NONE',  ( -1.189524669241239115E-16, -1.000000000000000000, -0.000000000000000000 ) ) ;
#35549 = CARTESIAN_POINT ( 'NONE',  ( -5.598654528085806881, 139.7449999999999761, -7.705886871421374629 ) ) ;
#35550 = CARTESIAN_POINT ( 'NONE',  ( 57.24999999999999289, 28.24999999999998934, -4.000000000000000000 ) ) ;
#35551 = EDGE_LOOP ( 'NONE', ( #52021, #55892, #28065, #56135 ) ) ;
#35552 = CARTESIAN_POINT ( 'NONE',  ( 27.99999999999998934, 0.000000000000000000, -37.00402776293828566 ) ) ;
#35553 = CARTESIAN_POINT ( 'NONE',  ( 5.598654528085805993, 136.3550000000000182, 7.705886871421374629 ) ) ;
#35554 = CARTESIAN_POINT ( 'NONE',  ( -48.65499999999997272, -7.632228543268600340, -2.479861379858950166 ) ) ;
#35555 = CYLINDRICAL_SURFACE ( 'NONE', #48792, 0.5000000000000004441 ) ;
#35556 = EDGE_LOOP ( 'NONE', ( #37594, #40335, #56524, #14325 ) ) ;
#35557 = CARTESIAN_POINT ( 'NONE',  ( -2.607480562269075097, 115.2929263765338135, 8.025000000000000355 ) ) ;
#35558 = UNCERTAINTY_MEASURE_WITH_UNIT (LENGTH_MEASURE( 1.000000000000000082E-05 ), #503, 'distance_accuracy_value', 'NONE');
#35559 = SURFACE_STYLE_FILL_AREA ( #14099 ) ;
#35560 = CARTESIAN_POINT ( 'NONE',  ( 72.00000000000000000, 14.49137674618942562, -9.500000000000000000 ) ) ;
#35561 = DIRECTION ( 'NONE',  ( -1.000000000000000000, 0.000000000000000000, 0.000000000000000000 ) ) ;
#35562 = EDGE_LOOP ( 'NONE', ( #65914, #29807, #53805, #56913 ) ) ;
#35563 = CARTESIAN_POINT ( 'NONE',  ( -4.792168507806670696, -9.000000000000005329, 1.190312887963161259 ) ) ;
#35564 = VERTEX_POINT ( 'NONE', #8020 ) ;
#35565 = DIRECTION ( 'NONE',  ( -1.000000000000000000, 0.000000000000000000, -0.000000000000000000 ) ) ;
#35566 = DIRECTION ( 'NONE',  ( -1.000000000000000000, -0.000000000000000000, -0.000000000000000000 ) ) ;
#35567 = CARTESIAN_POINT ( 'NONE',  ( -153.0550000000000068, -9.827790563157499189E-16, -8.024999999999991473 ) ) ;
#35568 = ORIENTED_EDGE ( 'NONE', *, *, #4174, .F. ) ;
#35569 = CARTESIAN_POINT ( 'NONE',  ( -70.87837837837835764, 13.70805908423324126, -9.500000000000000000 ) ) ;
#35570 = UNCERTAINTY_MEASURE_WITH_UNIT (LENGTH_MEASURE( 1.000000000000000082E-05 ), #7978, 'distance_accuracy_value', 'NONE');
#35571 = EDGE_CURVE ( 'NONE', #62679, #49132, #46326, .T. ) ;
#35572 = CYLINDRICAL_SURFACE ( 'NONE', #43164, 0.5000000000000004441 ) ;
#35573 = DIRECTION ( 'NONE',  ( 1.000000000000000000, 0.000000000000000000, 0.000000000000000000 ) ) ;
#35574 = CARTESIAN_POINT ( 'NONE',  ( 72.49999999999998579, 63.67479433117734544, 10.00000000000000000 ) ) ;
#35575 = DIRECTION ( 'NONE',  ( -1.000000000000000000, 0.000000000000000000, 0.000000000000000000 ) ) ;
#35576 = ORIENTED_EDGE ( 'NONE', *, *, #3623, .T. ) ;
#35577 = DIRECTION ( 'NONE',  ( 0.000000000000000000, 0.000000000000000000, 1.000000000000000000 ) ) ;
#35578 = ORIENTED_EDGE ( 'NONE', *, *, #29702, .F. ) ;
#35579 = DIRECTION ( 'NONE',  ( 0.000000000000000000, 0.000000000000000000, 1.000000000000000000 ) ) ;
#35580 =( LENGTH_UNIT ( ) NAMED_UNIT ( * ) SI_UNIT ( .MILLI., .METRE. ) );
#35581 = CARTESIAN_POINT ( 'NONE',  ( -77.00499999999999545, 6.826472737025116366, 4.959722759717898555 ) ) ;
#35582 = ORIENTED_EDGE ( 'NONE', *, *, #40221, .T. ) ;
#35584 = STYLED_ITEM ( 'NONE', ( #22829 ), #3109 ) ;
#35583 = CARTESIAN_POINT ( 'NONE',  ( -61.55707362346617373, -1.166476076187852838E-15, -9.524999999999991473 ) ) ;
#35585 = DIRECTION ( 'NONE',  ( 0.000000000000000000, -1.000000000000000000, 0.000000000000000000 ) ) ;
#35586 = SPHERICAL_SURFACE ( 'NONE', #43252, 0.2500000000000000000 ) ;
#35587 = EDGE_LOOP ( 'NONE', ( #26780, #36183, #38598, #36233 ) ) ;
#35588 = CARTESIAN_POINT ( 'NONE',  ( -75.00000000000000000, 8.545765431912627719, -5.556277950132133547 ) ) ;
#35589 = FILL_AREA_STYLE_COLOUR ( '', #67451 ) ;
#35591 =( NAMED_UNIT ( * ) PLANE_ANGLE_UNIT ( ) SI_UNIT ( $, .RADIAN. ) );
#35590 = CARTESIAN_POINT ( 'NONE',  ( -184.0000000000000000, 0.000000000000000000, 0.000000000000000000 ) ) ;
#35592 = EDGE_CURVE ( 'NONE', #25953, #51005, #47279, .T. ) ;
#35593 = PRESENTATION_LAYER_ASSIGNMENT (  '', '', ( #24324 ) ) ;
#35594 = EDGE_CURVE ( 'NONE', #64619, #43539, #11691, .T. ) ;
#35595 = CARTESIAN_POINT ( 'NONE',  ( 10.01517768586949231, 138.6949999999999932, 1.839758294383810543E-15 ) ) ;
#35596 = CARTESIAN_POINT ( 'NONE',  ( -98.39499999999999602, -6.826472737025115478, -4.959722759717899443 ) ) ;
#35597 = DIRECTION ( 'NONE',  ( 1.000000000000000000, 0.000000000000000000, 0.000000000000000000 ) ) ;
#35598 = DIRECTION ( 'NONE',  ( -0.000000000000000000, 0.000000000000000000, -1.000000000000000000 ) ) ;
#35599 = UNCERTAINTY_MEASURE_WITH_UNIT (LENGTH_MEASURE( 1.000000000000000082E-05 ), #3811, 'distance_accuracy_value', 'NONE');
#35600 = ADVANCED_FACE ( 'NONE', ( #57242 ), #3745, .T. ) ;
#35601 = PLANE ( 'NONE',  #10069 ) ;
#35602 = ORIENTED_EDGE ( 'NONE', *, *, #54671, .T. ) ;
#35603 = CARTESIAN_POINT ( 'NONE',  ( -145.0429263765338135, -9.058813317711329915, -2.943386871421370898 ) ) ;
#35604 = PRESENTATION_STYLE_ASSIGNMENT (( #24661 ) ) ;
#35605 = CARTESIAN_POINT ( 'NONE',  ( -153.7450000000000045, 4.716976649647094177, 6.492361379858945902 ) ) ;
#35606 = EDGE_CURVE ( 'NONE', #3817, #42106, #39594, .T. ) ;
#35607 = DIRECTION ( 'NONE',  ( 1.000000000000000000, 0.000000000000000000, 0.000000000000000000 ) ) ;
#35608 = CARTESIAN_POINT ( 'NONE',  ( 48.49999999999999289, 24.74999999999998579, 3.750000000000000000 ) ) ;
#35609 = ORIENTED_EDGE ( 'NONE', *, *, #43501, .F. ) ;
#35610 = CARTESIAN_POINT ( 'NONE',  ( 48.50000000000000000, 14.49137674618942562, 7.000000000000000000 ) ) ;
#35611 = ORIENTED_EDGE ( 'NONE', *, *, #24200, .T. ) ;
#35612 = B_SPLINE_CURVE_WITH_KNOTS ( 'NONE', 3,
 ( #7277, #8325, #45290, #18524, #29404, #61070, #39309, #24462, #51565 ),
 .UNSPECIFIED., .F., .F.,
 ( 4, 2, 1, 2, 4 ),
 ( 0.007659788818331629730, 0.009746199297478887538, 0.01078940453705251601, 0.01131100715683933111, 0.01183260977662614448 ),
 .UNSPECIFIED. ) ;
#35613 = SURFACE_STYLE_FILL_AREA ( #29263 ) ;
#35614 = ADVANCED_FACE ( 'NONE', ( #30146 ), #67681, .T. ) ;
#35615 = FILL_AREA_STYLE ('',( #19417 ) ) ;
#35616 = CARTESIAN_POINT ( 'NONE',  ( -45.66562050014668728, 8.455502173247500863, 6.462386104487610083 ) ) ;
#35617 = CARTESIAN_POINT ( 'NONE',  ( -172.8570736234661922, -5.598654528085803328, -7.705886871421366635 ) ) ;
#35618 = DIRECTION ( 'NONE',  ( -1.000000000000000000, -7.709882115452469292E-16, 0.000000000000000000 ) ) ;
#35619 = AXIS2_PLACEMENT_3D ( 'NONE', #35922, #56680, #19377 ) ;
#35620 = EDGE_LOOP ( 'NONE', ( #66894, #66618, #687 ) ) ;
#35621 = CARTESIAN_POINT ( 'NONE',  ( -159.3549999999999898, -4.716976649647093289, -6.492361379858945902 ) ) ;
#35622 = CIRCLE ( 'NONE', #28863, 13.49999999999999822 ) ;
#35623 = VERTEX_POINT ( 'NONE', #4447 ) ;
#35624 = CARTESIAN_POINT ( 'NONE',  ( -20.99060317843563794, 114.7782486714346533, -10.00000000000000178 ) ) ;
#35625 = CYLINDRICAL_SURFACE ( 'NONE', #38833, 0.5000000000000004441 ) ;
#35626 = ORIENTED_EDGE ( 'NONE', *, *, #13164, .F. ) ;
#35627 = STYLED_ITEM ( 'NONE', ( #60015 ), #50379 ) ;
#35628 = SURFACE_STYLE_USAGE ( .BOTH. , #2858 ) ;
#35629 = DIRECTION ( 'NONE',  ( 0.9418169057949938860, 0.000000000000000000, -0.3361263392814427542 ) ) ;
#35630 = CARTESIAN_POINT ( 'NONE',  ( 3.094860106618431583, 111.0949999999999704, 9.525000000000000355 ) ) ;
#35631 = EDGE_LOOP ( 'NONE', ( #32697, #36417, #18877, #63388 ) ) ;
#35632 = CARTESIAN_POINT ( 'NONE',  ( 0.000000000000000000, 0.000000000000000000, 52.50000000000000000 ) ) ;
#35633 = CARTESIAN_POINT ( 'NONE',  ( 9.058813317711338797, 112.9549999999999841, -2.943386871421372675 ) ) ;
#35634 = CARTESIAN_POINT ( 'NONE',  ( -75.80499999999997840, -8.437984349512086979, 5.166775262442717831E-16 ) ) ;
#35635 = ORIENTED_EDGE ( 'NONE', *, *, #66373, .T. ) ;
#35636 = CARTESIAN_POINT ( 'NONE',  ( -5.598654528085806881, 134.8549999999999898, -7.705886871421374629 ) ) ;
#35637 = UNCERTAINTY_MEASURE_WITH_UNIT (LENGTH_MEASURE( 1.000000000000000082E-05 ), #55967, 'distance_accuracy_value', 'NONE');
#35638 = CARTESIAN_POINT ( 'NONE',  ( -23.21231517720797655, 117.4999999999999716, 7.000000000000000000 ) ) ;
#35639 = CIRCLE ( 'NONE', #40128, 15.00000000000000000 ) ;
#35640 = CARTESIAN_POINT ( 'NONE',  ( -41.40613950039011826, 107.1008216811760718, 3.493724300021677553 ) ) ;
#35641 = CARTESIAN_POINT ( 'NONE',  ( 3.000000000000002665, 42.00000000000000000, -80.00402776293826435 ) ) ;
#35642 = EDGE_LOOP ( 'NONE', ( #30155, #18599, #40083, #44233 ) ) ;
#35643 = CARTESIAN_POINT ( 'NONE',  ( 74.99999999999998579, 50.00000000000000000, -7.000000000000000000 ) ) ;
#35644 = CARTESIAN_POINT ( 'NONE',  ( -6.413663052920317575, -2.499999999999997780, -2.891209729714699250 ) ) ;
#35645 = CARTESIAN_POINT ( 'NONE',  ( -55.79499999999998039, 2.607480562269068880, -8.024999999999993250 ) ) ;
#35646 = EDGE_LOOP ( 'NONE', ( #922, #38779, #28852, #65269 ) ) ;
#35647 = LINE ( 'NONE', #57797, #26113 ) ;
#35648 = EDGE_CURVE ( 'NONE', #13986, #8875, #62036, .T. ) ;
#35649 = DIRECTION ( 'NONE',  ( -0.000000000000000000, -0.000000000000000000, -1.000000000000000000 ) ) ;
#35650 = DIRECTION ( 'NONE',  ( 0.000000000000000000, -1.000000000000000000, 0.000000000000000000 ) ) ;
#35651 = ORIENTED_EDGE ( 'NONE', *, *, #850, .F. ) ;
#35652 = SURFACE_SIDE_STYLE ('',( #25428 ) ) ;
#35653 = EDGE_LOOP ( 'NONE', ( #13023, #55813, #58945, #52306 ) ) ;
#35654 = FACE_OUTER_BOUND ( 'NONE', #50168, .T. ) ;
#35655 = CARTESIAN_POINT ( 'NONE',  ( -105.5049999999999812, -6.826472737025115478, -4.959722759717899443 ) ) ;
#35656 = ORIENTED_EDGE ( 'NONE', *, *, #54933, .T. ) ;
#35657 = DIRECTION ( 'NONE',  ( -1.000000000000000000, -0.000000000000000000, -0.000000000000000000 ) ) ;
#35658 = DIRECTION ( 'NONE',  ( -0.000000000000000000, -0.000000000000000000, -1.000000000000000000 ) ) ;
#35659 = CARTESIAN_POINT ( 'NONE',  ( -138.2070736234661865, 3.094860106618433360, 9.524999999999991473 ) ) ;
#35660 = SURFACE_STYLE_FILL_AREA ( #69401 ) ;
#35661 = CARTESIAN_POINT ( 'NONE',  ( 3.094860106618435136, 142.2950000000000159, -9.525000000000000355 ) ) ;
#35662 = CARTESIAN_POINT ( 'NONE',  ( -78.35707362346616378, 5.598654528085804216, 7.705886871421366635 ) ) ;
#35663 = PRODUCT_DEFINITION ( 'UNKNOWN', '', #25901, #16431 ) ;
#35664 = EDGE_CURVE ( 'NONE', #7106, #37864, #28597, .T. ) ;
#35666 = ADVANCED_FACE ( 'NONE', ( #65907 ), #55702, .F. ) ;
#35665 =( NAMED_UNIT ( * ) PLANE_ANGLE_UNIT ( ) SI_UNIT ( $, .RADIAN. ) );
#35667 = ORIENTED_EDGE ( 'NONE', *, *, #23047, .T. ) ;
#35668 = CARTESIAN_POINT ( 'NONE',  ( -19.83771012782007048, -11.93314589359951761, -1.305473525340978380 ) ) ;
#35669 = AXIS2_PLACEMENT_3D ( 'NONE', #5164, #47814, #10470 ) ;
#35671 = CARTESIAN_POINT ( 'NONE',  ( -7.766025168014157209, 1.733974831985841458, 0.5488498361408482573 ) ) ;
#35670 = DIRECTION ( 'NONE',  ( 1.000000000000000000, -0.000000000000000000, -1.300977106640434891E-16 ) ) ;
#35672 = AXIS2_PLACEMENT_3D ( 'NONE', #56932, #29844, #41136 ) ;
#35673 = EDGE_CURVE ( 'NONE', #7860, #44595, #33881, .T. ) ;
#35674 = CARTESIAN_POINT ( 'NONE',  ( -123.2049999999999699, -2.607480562269071545, -8.024999999999991473 ) ) ;
#35675 = EDGE_CURVE ( 'NONE', #58449, #57125, #2155, .T. ) ;
#35676 = PRESENTATION_LAYER_ASSIGNMENT (  '', '', ( #8695 ) ) ;
#35677 =( LENGTH_UNIT ( ) NAMED_UNIT ( * ) SI_UNIT ( .MILLI., .METRE. ) );
#35678 = CARTESIAN_POINT ( 'NONE',  ( -121.6449999999999960, 4.716976649647091513, -6.492361379858946790 ) ) ;
#35679 = CARTESIAN_POINT ( 'NONE',  ( -119.0949999999999847, -2.607480562269071545, -8.024999999999991473 ) ) ;
#35680 = DIRECTION ( 'NONE',  ( 1.000000000000000000, 0.000000000000000000, 0.000000000000000000 ) ) ;
#35681 = VERTEX_POINT ( 'NONE', #53375 ) ;
#35682 =( NAMED_UNIT ( * ) SI_UNIT ( $, .STERADIAN. ) SOLID_ANGLE_UNIT ( ) );
#35683 = EDGE_CURVE ( 'NONE', #9536, #63831, #5158, .T. ) ;
#35684 = CARTESIAN_POINT ( 'NONE',  ( -15.98999599679679839, 117.9999999999999716, 7.000000000000000000 ) ) ;
#35685 = CARTESIAN_POINT ( 'NONE',  ( -169.0429263765338135, -9.058813317711329915, -2.943386871421370898 ) ) ;
#35686 =( LENGTH_UNIT ( ) NAMED_UNIT ( * ) SI_UNIT ( .MILLI., .METRE. ) );
#35687 = CARTESIAN_POINT ( 'NONE',  ( -182.3950000000000102, -6.826472737025115478, -4.959722759717899443 ) ) ;
#35688 =( GEOMETRIC_REPRESENTATION_CONTEXT ( 3 ) GLOBAL_UNCERTAINTY_ASSIGNED_CONTEXT ( ( #7988 ) ) GLOBAL_UNIT_ASSIGNED_CONTEXT ( ( #17776, #60647, #39599 ) ) REPRESENTATION_CONTEXT ( 'NONE', 'WORKASPACE' ) );
#35689 = EDGE_CURVE ( 'NONE', #62302, #21323, #11743, .T. ) ;
#35690 = AXIS2_PLACEMENT_3D ( 'NONE', #60776, #12596, #33381 ) ;
#35691 = CARTESIAN_POINT ( 'NONE',  ( -15.98999599679679839, 146.4999999999999716, 7.500000000000000000 ) ) ;
#35692 = CARTESIAN_POINT ( 'NONE',  ( -1.744870598150811469, -7.000000000000001776, 0.2069669095365348765 ) ) ;
#35693 = ORIENTED_EDGE ( 'NONE', *, *, #45859, .F. ) ;
#35694 = CARTESIAN_POINT ( 'NONE',  ( -84.29292637653381348, 3.094860106618428031, -9.524999999999993250 ) ) ;
#35695 = DIRECTION ( 'NONE',  ( 1.000000000000000000, 0.000000000000000000, 0.000000000000000000 ) ) ;
#35696 =( REPRESENTATION_RELATIONSHIP ('NONE','NONE', #5102, #38844 ) REPRESENTATION_RELATIONSHIP_WITH_TRANSFORMATION ( #31084 )SHAPE_REPRESENTATION_RELATIONSHIP( ) );
#35697 = CARTESIAN_POINT ( 'NONE',  ( -11.99999999999999822, -6.499999999999999112, 21.00000000000000000 ) ) ;
#35698 = CARTESIAN_POINT ( 'NONE',  ( 2.607480562269051116, 122.7070736234661439, 8.025000000000016342 ) ) ;
#35699 = FILL_AREA_STYLE ('',( #68064 ) ) ;
#35700 = CARTESIAN_POINT ( 'NONE',  ( 26.00000000000001776, 42.00000000000000000, -29.68999999999999417 ) ) ;
#35701 = ORIENTED_EDGE ( 'NONE', *, *, #722, .F. ) ;
#35702 = CARTESIAN_POINT ( 'NONE',  ( -135.5929263765344217, -3.094860106628851248, -9.524999999992420641 ) ) ;
#35703 = DIRECTION ( 'NONE',  ( -1.000000000000000000, 0.000000000000000000, 0.000000000000000000 ) ) ;
#35704 = SURFACE_STYLE_FILL_AREA ( #30746 ) ;
#35705 = EDGE_LOOP ( 'NONE', ( #31329, #36033, #35252, #28233 ) ) ;
#35706 = FACE_OUTER_BOUND ( 'NONE', #56424, .T. ) ;
#35707 = EDGE_CURVE ( 'NONE', #45578, #65484, #60885, .T. ) ;
#35708 =( LENGTH_UNIT ( ) NAMED_UNIT ( * ) SI_UNIT ( .MILLI., .METRE. ) );
#35709 = CARTESIAN_POINT ( 'NONE',  ( -7.632228543268607446, 136.6570736234661467, -2.479861379858953718 ) ) ;
#35710 = FILL_AREA_STYLE ('',( #19859 ) ) ;
#35711 = ORIENTED_EDGE ( 'NONE', *, *, #2660, .F. ) ;
#35712 = FACE_OUTER_BOUND ( 'NONE', #45125, .T. ) ;
#35713 = CARTESIAN_POINT ( 'NONE',  ( -104.9049999999999869, 2.607480562269069324, -8.024999999999993250 ) ) ;
#35714 = SURFACE_STYLE_FILL_AREA ( #52601 ) ;
#35715 = AXIS2_PLACEMENT_3D ( 'NONE', #37147, #32173, #48390 ) ;
#35716 = VERTEX_POINT ( 'NONE', #28231 ) ;
#35717 = AXIS2_PLACEMENT_3D ( 'NONE', #69149, #47753, #52969 ) ;
#35718 = FACE_OUTER_BOUND ( 'NONE', #38994, .T. ) ;
#35719 =( NAMED_UNIT ( * ) PLANE_ANGLE_UNIT ( ) SI_UNIT ( $, .RADIAN. ) );
#35720 = AXIS2_PLACEMENT_3D ( 'NONE', #40359, #57204, #45666 ) ;
#35721 = CARTESIAN_POINT ( 'NONE',  ( -85.04499999999998749, 7.632228543268600340, 2.479861379858949277 ) ) ;
#35722 = EDGE_LOOP ( 'NONE', ( #15596, #51060, #45342, #68700 ) ) ;
#35724 = DIRECTION ( 'NONE',  ( -0.000000000000000000, -0.000000000000000000, 1.000000000000000000 ) ) ;
#35723 =( BOUNDED_CURVE ( )  B_SPLINE_CURVE ( 2, ( #55555, #66450, #8423, #8058, #23885, #50628, #55899, #40435, #34096, #29140, #29510 ),
 .UNSPECIFIED., .F., .F. ) 
 B_SPLINE_CURVE_WITH_KNOTS ( ( 3, 2, 2, 2, 2, 3 ),
 ( 0.03260869565217317662, 0.03478260869565139024, 0.03695652173912960387, 0.03913043478260781749, 0.04130434782608602418, 0.04347826086956423780 ),
 .UNSPECIFIED. ) 
 CURVE ( )  GEOMETRIC_REPRESENTATION_ITEM ( )  RATIONAL_B_SPLINE_CURVE ( ( 1.000000000000016653, 0.9510565162951370999, 1.000000000000000000, 0.9510565162951535312, 1.000000000000000000, 0.9510565162951535312, 1.000000000000000000, 0.9510565162951535312, 1.000000000000000000, 0.9510565162951755136, 0.9999999999999780176 ) ) 
 REPRESENTATION_ITEM ( '' )  );
#35725 =( NAMED_UNIT ( * ) PLANE_ANGLE_UNIT ( ) SI_UNIT ( $, .RADIAN. ) );
#35726 = CARTESIAN_POINT ( 'NONE',  ( 75.00000000000000000, 20.36037961002804053, 10.00000000000000000 ) ) ;
#35727 = VERTEX_POINT ( 'NONE', #64251 ) ;
#35728 = CIRCLE ( 'NONE', #23362, 0.5000000000000004441 ) ;
#35729 = VECTOR ( 'NONE', #3313, 1000.000000000000000 ) ;
#35730 = LINE ( 'NONE', #45955, #37083 ) ;
#35731 = CARTESIAN_POINT ( 'NONE',  ( -48.00000000000000000, 99.99999999999992895, -7.500000000000000000 ) ) ;
#35732 = ORIENTED_EDGE ( 'NONE', *, *, #25415, .F. ) ;
#35733 = CARTESIAN_POINT ( 'NONE',  ( 68.99999999999998579, 1.000000000000008438, 4.000000000000000000 ) ) ;
#35734 = EDGE_LOOP ( 'NONE', ( #31458, #23033, #46968, #41698 ) ) ;
#35735 = FACE_OUTER_BOUND ( 'NONE', #34939, .T. ) ;
#35736 = CARTESIAN_POINT ( 'NONE',  ( -9.827790563157511022E-16, 127.4429263765338192, 8.025000000000000355 ) ) ;
#35737 = DIRECTION ( 'NONE',  ( 0.000000000000000000, 0.000000000000000000, -1.000000000000000000 ) ) ;
#35738 = CARTESIAN_POINT ( 'NONE',  ( -173.4570736234661865, -9.058813317711329915, 2.943386871421371787 ) ) ;
#35739 = CARTESIAN_POINT ( 'NONE',  ( 34.99999999999992895, 110.4999999999999858, 9.500000000000000000 ) ) ;
#35740 = CARTESIAN_POINT ( 'NONE',  ( 3.094860106618435136, 118.2949999999999875, -9.525000000000000355 ) ) ;
#35741 = CARTESIAN_POINT ( 'NONE',  ( -106.5570736234661666, -1.166476076187852838E-15, -9.524999999999991473 ) ) ;
#35742 = EDGE_CURVE ( 'NONE', #33844, #17336, #18209, .T. ) ;
#35743 = CARTESIAN_POINT ( 'NONE',  ( -183.3519149756361912, 1.436423777000723276E-13, -9.173085024363883733 ) ) ;
#35744 = CARTESIAN_POINT ( 'NONE',  ( -64.70707362346617231, -3.094860106618431139, -9.524999999999991473 ) ) ;
#35745 = ORIENTED_EDGE ( 'NONE', *, *, #3691, .T. ) ;
#35746 = CARTESIAN_POINT ( 'NONE',  ( -107.2429263765338021, 5.598654528085804216, 7.705886871421366635 ) ) ;
#35747 = CARTESIAN_POINT ( 'NONE',  ( -81.44292637653380496, -1.166476076187852838E-15, -9.524999999999991473 ) ) ;
#35749 = CARTESIAN_POINT ( 'NONE',  ( 74.99999999999998579, 119.9999999999997584, -9.500000000000000000 ) ) ;
#35748 = FACE_OUTER_BOUND ( 'NONE', #66668, .T. ) ;
#35750 = SURFACE_STYLE_FILL_AREA ( #24821 ) ;
#35751 = EDGE_CURVE ( 'NONE', #49404, #10212, #36227, .T. ) ;
#35752 = CARTESIAN_POINT ( 'NONE',  ( -153.9550000000000125, -7.632228543268599452, 2.479861379858951054 ) ) ;
#35753 = CARTESIAN_POINT ( 'NONE',  ( 0.000000000000000000, 42.00000000000000000, -75.00000000000001421 ) ) ;
#35754 = CARTESIAN_POINT ( 'NONE',  ( -155.9949999999999761, -6.826472737025115478, 4.959722759717900331 ) ) ;
#35755 = CARTESIAN_POINT ( 'NONE',  ( -143.6949999999999932, -8.437984349512086979, 5.166775262442717831E-16 ) ) ;
#35756 = EDGE_LOOP ( 'NONE', ( #53788, #34431, #44172, #6885 ) ) ;
#35757 = CARTESIAN_POINT ( 'NONE',  ( -181.5570736234661808, -1.166476076187852838E-15, -9.524999999999991473 ) ) ;
#35758 =( LENGTH_UNIT ( ) NAMED_UNIT ( * ) SI_UNIT ( .MILLI., .METRE. ) );
#35759 = CARTESIAN_POINT ( 'NONE',  ( -68.30499999999997840, 8.437984349512085203, -1.550032578732815448E-15 ) ) ;
#35760 = CARTESIAN_POINT ( 'NONE',  ( -13.50000000000000533, 30.74999999999999289, -3.750000000000000000 ) ) ;
#35761 = AXIS2_PLACEMENT_3D ( 'NONE', #52537, #15593, #38800 ) ;
#35762 =( GEOMETRIC_REPRESENTATION_CONTEXT ( 3 ) GLOBAL_UNCERTAINTY_ASSIGNED_CONTEXT ( ( #21302 ) ) GLOBAL_UNIT_ASSIGNED_CONTEXT ( ( #23714, #24394, #2553 ) ) REPRESENTATION_CONTEXT ( 'NONE', 'WORKASPACE' ) );
#35763 = EDGE_CURVE ( 'NONE', #17310, #16969, #1332, .T. ) ;
#35764 = CARTESIAN_POINT ( 'NONE',  ( -62.84499999999998465, -7.632228543268599452, 2.479861379858951054 ) ) ;
#35765 = CARTESIAN_POINT ( 'NONE',  ( 8.102448949553181734, 160.5049999999999386, 5.886773742842750679 ) ) ;
#35766 = DIRECTION ( 'NONE',  ( 1.000000000000000000, 0.000000000000000000, 0.000000000000000000 ) ) ;
#35767 = CARTESIAN_POINT ( 'NONE',  ( -0.3711768842070180541, 154.5000000000000284, -9.524999999999986144 ) ) ;
#35768 = CARTESIAN_POINT ( 'NONE',  ( 0.000000000000000000, 0.000000000000000000, 0.000000000000000000 ) ) ;
#35769 = DIRECTION ( 'NONE',  ( 0.000000000000000000, 0.000000000000000000, -1.000000000000000000 ) ) ;
#35770 = CARTESIAN_POINT ( 'NONE',  ( -0.7252983342185689297, 110.8245556577202962, 9.200444342279737953 ) ) ;
#35771 = AXIS2_PLACEMENT_3D ( 'NONE', #48941, #53489, #10917 ) ;
#35772 = SURFACE_STYLE_USAGE ( .BOTH. , #14312 ) ;
#35773 = ADVANCED_FACE ( 'NONE', ( #40587 ), #3217, .F. ) ;
#35774 = CARTESIAN_POINT ( 'NONE',  ( 44.25000000000000000, 21.74999999999998579, -3.750000000000000000 ) ) ;
#35775 = CARTESIAN_POINT ( 'NONE',  ( 11.00000000000001776, -3.148064030671221758, 29.68999999999999417 ) ) ;
#35776 = VERTEX_POINT ( 'NONE', #41289 ) ;
#35777 = EDGE_LOOP ( 'NONE', ( #7267, #46065, #10090, #33001 ) ) ;
#35778 = CARTESIAN_POINT ( 'NONE',  ( -61.40707362346617515, 3.094860106618428031, -9.524999999999993250 ) ) ;
#35779 = ADVANCED_FACE ( 'NONE', ( #2526 ), #66605, .T. ) ;
#35780 = CARTESIAN_POINT ( 'NONE',  ( 4.041451884327375232, -1.417096231345241097, -7.000000000000002665 ) ) ;
#35781 = AXIS2_PLACEMENT_3D ( 'NONE', #43340, #64387, #59425 ) ;
#35782 = SURFACE_STYLE_FILL_AREA ( #24860 ) ;
#35783 = CARTESIAN_POINT ( 'NONE',  ( 75.00000000000000000, -2.215169945516535778E-14, 6.999999999999999112 ) ) ;
#35784 = SURFACE_SIDE_STYLE ('',( #9763 ) ) ;
#35785 = ORIENTED_EDGE ( 'NONE', *, *, #26138, .T. ) ;
#35787 = EDGE_LOOP ( 'NONE', ( #58612, #31134, #28032, #1744, #42168, #37581, #53958, #27964, #40845, #53090, #3986, #41165, #30429, #6047, #11812, #61814 ) ) ;
#35786 = AXIS2_PLACEMENT_3D ( 'NONE', #36566, #68528, #67226 ) ;
#35788 = FACE_OUTER_BOUND ( 'NONE', #65382, .T. ) ;
#35789 = ORIENTED_EDGE ( 'NONE', *, *, #23293, .T. ) ;
#35790 = CARTESIAN_POINT ( 'NONE',  ( -1.166476076187854022E-15, 115.0549999999999926, 9.525000000000000355 ) ) ;
#35791 = CARTESIAN_POINT ( 'NONE',  ( 5.249999999999997335, 6.429395695523601195E-16, 0.000000000000000000 ) ) ;
#35792 = ORIENTED_EDGE ( 'NONE', *, *, #54671, .F. ) ;
#35793 = AXIS2_PLACEMENT_3D ( 'NONE', #40216, #3924, #14491 ) ;
#35794 = CARTESIAN_POINT ( 'NONE',  ( 53.25000000000005684, 1.231653667943533289E-13, 4.000000000000000000 ) ) ;
#35795 = CARTESIAN_POINT ( 'NONE',  ( -109.1949999999999648, 8.437984349512085203, -1.550032578732815448E-15 ) ) ;
#35796 = ORIENTED_EDGE ( 'NONE', *, *, #41201, .F. ) ;
#35797 =( GEOMETRIC_REPRESENTATION_CONTEXT ( 3 ) GLOBAL_UNCERTAINTY_ASSIGNED_CONTEXT ( ( #44085 ) ) GLOBAL_UNIT_ASSIGNED_CONTEXT ( ( #48135, #37938, #69218 ) ) REPRESENTATION_CONTEXT ( 'NONE', 'WORKASPACE' ) );
#35798 = DIRECTION ( 'NONE',  ( 1.000000000000000000, 0.000000000000000000, -0.000000000000000000 ) ) ;
#35799 = CARTESIAN_POINT ( 'NONE',  ( -16.72057948583355369, 65.79671608775228719, -5.561181121879805289 ) ) ;
#35800 = EDGE_LOOP ( 'NONE', ( #19372, #20639, #62749, #39038 ) ) ;
#35801 = CARTESIAN_POINT ( 'NONE',  ( 4.716976649647099507, 140.6429263765338078, -6.492361379858953008 ) ) ;
#35802 =( BOUNDED_CURVE ( )  B_SPLINE_CURVE ( 2, ( #21862, #32745, #38066, #54543, #39105, #997, #22544, #44401, #49632, #6011, #65455 ),
 .UNSPECIFIED., .F., .F. ) 
 B_SPLINE_CURVE_WITH_KNOTS ( ( 3, 2, 2, 2, 2, 3 ),
 ( 0.9565217391304348116, 0.9586956521739130599, 0.9608695652173913082, 0.9630434782608695565, 0.9652173913043478048, 0.9673913043478260532 ),
 .UNSPECIFIED. ) 
 CURVE ( )  GEOMETRIC_REPRESENTATION_ITEM ( )  RATIONAL_B_SPLINE_CURVE ( ( 1.000000000000000000, 0.9510565162951535312, 1.000000000000000000, 0.9510565162951535312, 1.000000000000000000, 0.9510565162951535312, 1.000000000000000000, 0.9510565162951535312, 1.000000000000000000, 0.9510565162951535312, 1.000000000000000000 ) ) 
 REPRESENTATION_ITEM ( '' )  );
#35803 = DIRECTION ( 'NONE',  ( 0.000000000000000000, -1.000000000000000000, 0.000000000000000000 ) ) ;
#35804 = STYLED_ITEM ( 'NONE', ( #59263 ), #51078 ) ;
#35805 = FACE_OUTER_BOUND ( 'NONE', #19723, .T. ) ;
#35806 = DIRECTION ( 'NONE',  ( 1.000000000000000000, 0.000000000000000000, 0.000000000000000000 ) ) ;
#35807 = EDGE_LOOP ( 'NONE', ( #40146, #67184, #44614, #14096, #6234 ) ) ;
#35808 = EDGE_CURVE ( 'NONE', #66756, #11552, #35989, .T. ) ;
#35809 = SURFACE_STYLE_FILL_AREA ( #14341 ) ;
#35810 = VERTEX_POINT ( 'NONE', #14513 ) ;
#35811 = FILL_AREA_STYLE ('',( #9087 ) ) ;
#35812 = CARTESIAN_POINT ( 'NONE',  ( -141.2929263765343535, 3.094860106609420125, -9.525000000006537348 ) ) ;
#35814 = AXIS2_PLACEMENT_3D ( 'NONE', #27854, #1078, #22618 ) ;
#35813 = CYLINDRICAL_SURFACE ( 'NONE', #32144, 0.2500000000000002220 ) ;
#35815 = CARTESIAN_POINT ( 'NONE',  ( -127.5550000000000068, 0.000000000000000000, 8.024999999999991473 ) ) ;
#35816 = DIRECTION ( 'NONE',  ( 1.000000000000000000, -0.000000000000000000, 0.000000000000000000 ) ) ;
#35817 = CARTESIAN_POINT ( 'NONE',  ( -45.00000000000000000, 0.000000000000000000, 0.000000000000000000 ) ) ;
#35818 = CARTESIAN_POINT ( 'NONE',  ( -125.0929263765345780, 3.094860106630937135, 9.524999999990908961 ) ) ;
#35819 = DIRECTION ( 'NONE',  ( -1.000000000000000000, 0.000000000000000000, 0.000000000000000000 ) ) ;
#35820 = CARTESIAN_POINT ( 'NONE',  ( 0.000000000000000000, 0.000000000000000000, 0.7500000000000000000 ) ) ;
#35821 = EDGE_LOOP ( 'NONE', ( #522, #35865, #4239, #21609, #25337, #4605, #41784, #48295, #68352, #22753, #41870, #826, #38640, #63235, #40098, #47890 ) ) ;
#35822 = CIRCLE ( 'NONE', #3230, 0.2500000000000002220 ) ;
#35823 = ORIENTED_EDGE ( 'NONE', *, *, #53659, .F. ) ;
#35824 = DIRECTION ( 'NONE',  ( 0.000000000000000000, 0.000000000000000000, -1.000000000000000000 ) ) ;
#35825 = CARTESIAN_POINT ( 'NONE',  ( -74.50000000000000000, 7.768687147774688384, -6.999999999999999112 ) ) ;
#35826 = VERTEX_POINT ( 'NONE', #18422 ) ;
#35827 =( NAMED_UNIT ( * ) PLANE_ANGLE_UNIT ( ) SI_UNIT ( $, .RADIAN. ) );
#35828 = ADVANCED_FACE ( 'NONE', ( #66959 ), #61312, .T. ) ;
#35829 = CARTESIAN_POINT ( 'NONE',  ( -175.5549999999999784, 0.000000000000000000, 8.024999999999991473 ) ) ;
#35830 =( NAMED_UNIT ( * ) PLANE_ANGLE_UNIT ( ) SI_UNIT ( $, .RADIAN. ) );
#35831 = FILL_AREA_STYLE ('',( #8417 ) ) ;
#35832 = CARTESIAN_POINT ( 'NONE',  ( -53.45707362346615810, -9.058813317711329915, 2.943386871421371787 ) ) ;
#35833 = ADVANCED_FACE ( 'NONE', ( #46587 ), #62685, .T. ) ;
#35834 = CARTESIAN_POINT ( 'NONE',  ( -181.3449999999999989, 7.632228543268599452, -2.479861379858951942 ) ) ;
#35835 =( BOUNDED_CURVE ( )  B_SPLINE_CURVE ( 2, ( #44583, #55782, #27975, #7589, #39291, #55071, #6895, #50516, #49480, #17143, #60694 ),
 .UNSPECIFIED., .F., .F. ) 
 B_SPLINE_CURVE_WITH_KNOTS ( ( 3, 2, 2, 2, 2, 3 ),
 ( 0.2352941176470587370, 0.2411764705882352144, 0.2470588235294116919, 0.2529411764705881693, 0.2588235294117646745, 0.2647058823529411242 ),
 .UNSPECIFIED. ) 
 CURVE ( )  GEOMETRIC_REPRESENTATION_ITEM ( )  RATIONAL_B_SPLINE_CURVE ( ( 1.000000000000000666, 0.9510565162951529761, 1.000000000000000000, 0.9510565162951535312, 1.000000000000000000, 0.9510565162951535312, 1.000000000000000000, 0.9510565162951535312, 1.000000000000000000, 0.9510565162951539753, 0.9999999999999995559 ) ) 
 REPRESENTATION_ITEM ( '' )  );
#35836 = PRESENTATION_STYLE_ASSIGNMENT (( #5435 ) ) ;
#35837 = ORIENTED_EDGE ( 'NONE', *, *, #50316, .F. ) ;
#35838 = CARTESIAN_POINT ( 'NONE',  ( 82.09357085539578236, 5.000000000000000000, 32.00402776293825724 ) ) ;
#35839 = ADVANCED_FACE ( 'NONE', ( #64091 ), #25420, .T. ) ;
#35841 = FACE_OUTER_BOUND ( 'NONE', #24800, .T. ) ;
#35840 = MECHANICAL_DESIGN_GEOMETRIC_PRESENTATION_REPRESENTATION (  '', ( #15626 ), #5463 ) ;
#35842 = CARTESIAN_POINT ( 'NONE',  ( -90.35499999999998977, -4.716976649647093289, -6.492361379858945902 ) ) ;
#35843 = DIRECTION ( 'NONE',  ( 7.080503983578803083E-17, -1.000000000000000000, 0.000000000000000000 ) ) ;
#35844 = CARTESIAN_POINT ( 'NONE',  ( 57.00000000000000000, 0.9999999999999991118, 80.00402776293826435 ) ) ;
#35845 = EDGE_CURVE ( 'NONE', #40883, #61513, #1384, .T. ) ;
#35846 = CARTESIAN_POINT ( 'NONE',  ( -90.59499999999999886, 2.607480562269072433, 8.024999999999991473 ) ) ;
#35847 = CARTESIAN_POINT ( 'NONE',  ( -8.102448949553181734, 123.6049999999999756, 5.886773742842747126 ) ) ;
#35848 = CARTESIAN_POINT ( 'NONE',  ( -70.64499999999998181, 4.716976649647091513, -6.492361379858946790 ) ) ;
#35849 = CARTESIAN_POINT ( 'NONE',  ( -75.00000000000000000, 9.119539144243724138, -6.744166081069411511 ) ) ;
#35850 = COLOUR_RGB ( '', 0.09019608, 0.27058824, 0.51372549) ;
#35851 = CARTESIAN_POINT ( 'NONE',  ( -55.70707362346616520, -3.094860106618431139, -9.524999999999991473 ) ) ;
#35852 = DIRECTION ( 'NONE',  ( 0.000000000000000000, 0.000000000000000000, 1.000000000000000000 ) ) ;
#35853 = CIRCLE ( 'NONE', #5481, 5.000000000000000000 ) ;
#35854 = FACE_OUTER_BOUND ( 'NONE', #9851, .T. ) ;
#35855 = VERTEX_POINT ( 'NONE', #41633 ) ;
#35856 = CARTESIAN_POINT ( 'NONE',  ( -118.9429263765338050, 0.000000000000000000, 9.524999999999991473 ) ) ;
#35857 = CARTESIAN_POINT ( 'NONE',  ( -128.6950000000000216, -8.437984349512085203, 5.166775262442717831E-16 ) ) ;
#35858 = CARTESIAN_POINT ( 'NONE',  ( -4.716976649647098618, 146.2570736234661410, 6.492361379858953008 ) ) ;
#35859 = AXIS2_PLACEMENT_3D ( 'NONE', #68222, #35520, #58023 ) ;
#35860 =( NAMED_UNIT ( * ) SI_UNIT ( $, .STERADIAN. ) SOLID_ANGLE_UNIT ( ) );
#35861 = DIRECTION ( 'NONE',  ( -1.000000000000000000, -0.000000000000000000, -0.000000000000000000 ) ) ;
#35862 = CARTESIAN_POINT ( 'NONE',  ( -71.50000000000000000, 35.92875272052971525, 7.500000000000000000 ) ) ;
#35863 = ORIENTED_EDGE ( 'NONE', *, *, #67253, .F. ) ;
#35864 = COLOUR_RGB ( '', 0.08235294, 0.09019608, 0.10196078) ;
#35865 = ORIENTED_EDGE ( 'NONE', *, *, #47063, .T. ) ;
#35866 = DIRECTION ( 'NONE',  ( 0.000000000000000000, 0.000000000000000000, 1.000000000000000000 ) ) ;
#35867 = CARTESIAN_POINT ( 'NONE',  ( -15.48999599679679662, 117.9999999999999716, 9.500000000000000000 ) ) ;
#35868 = CYLINDRICAL_SURFACE ( 'NONE', #51722, 0.5000000000000004441 ) ;
#35869 = TOROIDAL_SURFACE ( 'NONE', #5504, 1.000000000000000000, 0.5000000000000000000 ) ;
#35870 = CARTESIAN_POINT ( 'NONE',  ( 82.09357085539566867, 5.000000000000000000, -37.00402776293823592 ) ) ;
#35871 = ORIENTED_EDGE ( 'NONE', *, *, #34454, .T. ) ;
#35872 = CARTESIAN_POINT ( 'NONE',  ( -136.2549999999999955, -4.716976649647092401, 6.492361379858946790 ) ) ;
#35873 = ORIENTED_EDGE ( 'NONE', *, *, #24223, .F. ) ;
#35874 = DIRECTION ( 'NONE',  ( -0.000000000000000000, -0.000000000000000000, 1.000000000000000000 ) ) ;
#35875 = CARTESIAN_POINT ( 'NONE',  ( -125.9070736234661751, -3.094860106618429807, 9.524999999999991473 ) ) ;
#35876 = VERTEX_POINT ( 'NONE', #31038 ) ;
#35877 = PLANE ( 'NONE',  #61623 ) ;
#35878 = PLANE ( 'NONE',  #60178 ) ;
#35879 = EDGE_LOOP ( 'NONE', ( #54529, #40733, #69147, #55607 ) ) ;
#35880 = CIRCLE ( 'NONE', #5517, 0.5000000000000000000 ) ;
#35882 = CARTESIAN_POINT ( 'NONE',  ( -7.794228634059948035, -2.500000000000000000, 4.499999999999999112 ) ) ;
#35881 = CIRCLE ( 'NONE', #38175, 0.5000000000000004441 ) ;
#35883 = CARTESIAN_POINT ( 'NONE',  ( 10.01517768586949231, 138.6949999999999932, 1.839758294383810543E-15 ) ) ;
#35884 = ORIENTED_EDGE ( 'NONE', *, *, #5911, .T. ) ;
#35885 = FILL_AREA_STYLE ('',( #14413 ) ) ;
#35886 = CARTESIAN_POINT ( 'NONE',  ( 5.598654528085809545, 146.2549999999999955, -7.705886871421373741 ) ) ;
#35887 = DIRECTION ( 'NONE',  ( 0.000000000000000000, 1.000000000000000000, 0.000000000000000000 ) ) ;
#35888 = COLOUR_RGB ( '', 0.31764706, 0.68627451, 0.89019608) ;
#35889 =( LENGTH_UNIT ( ) NAMED_UNIT ( * ) SI_UNIT ( .MILLI., .METRE. ) );
#35890 = ORIENTED_EDGE ( 'NONE', *, *, #69104, .T. ) ;
#35891 = CARTESIAN_POINT ( 'NONE',  ( -4.716976649647098618, 121.1429263765338220, 6.492361379858953008 ) ) ;
#35892 =( NAMED_UNIT ( * ) PLANE_ANGLE_UNIT ( ) SI_UNIT ( $, .RADIAN. ) );
#35893 = PRESENTATION_STYLE_ASSIGNMENT (( #14797 ) ) ;
#35894 = CARTESIAN_POINT ( 'NONE',  ( -98.69292637653380496, 10.01517768586948698, -1.839758294383808966E-15 ) ) ;
#35895 = CARTESIAN_POINT ( 'NONE',  ( 15.48999599679679662, 118.4999999999999716, 7.000000000000000000 ) ) ;
#35896 = VERTEX_POINT ( 'NONE', #4277 ) ;
#35897 = EDGE_CURVE ( 'NONE', #35826, #60834, #18852, .T. ) ;
#35898 = AXIS2_PLACEMENT_3D ( 'NONE', #50210, #12902, #34367 ) ;
#35899 = CARTESIAN_POINT ( 'NONE',  ( -2.244403820859648846, -9.000000000000005329, 0.2663676893020989755 ) ) ;
#35900 = ORIENTED_EDGE ( 'NONE', *, *, #58572, .T. ) ;
#35901 = CARTESIAN_POINT ( 'NONE',  ( -60.89292637653380780, -8.102448949553172852, -5.886773742842741797 ) ) ;
#35902 = AXIS2_PLACEMENT_3D ( 'NONE', #60360, #17816, #43214 ) ;
#35903 = CARTESIAN_POINT ( 'NONE',  ( -23.71231517720798010, 117.4999999999999716, 7.000000000000000000 ) ) ;
#35904 = DIRECTION ( 'NONE',  ( 1.000000000000000000, -0.000000000000000000, -1.300977106640434891E-16 ) ) ;
#35905 = CARTESIAN_POINT ( 'NONE',  ( -148.4050000000000296, -2.607480562269069768, 8.024999999999991473 ) ) ;
#35906 = ORIENTED_EDGE ( 'NONE', *, *, #41649, .T. ) ;
#35907 = CIRCLE ( 'NONE', #16841, 6.999999999999997335 ) ;
#35908 = B_SPLINE_CURVE_WITH_KNOTS ( 'NONE', 3,
 ( #52045, #68556, #47856, #14750, #47493, #19663, #35849, #15460, #52730, #4147, #20712, #30191 ),
 .UNSPECIFIED., .F., .F.,
 ( 4, 2, 2, 2, 2, 4 ),
 ( 0.000000000000000000, 0.0002999083533514613608, 0.0005998167067029227216, 0.001199633413405845443, 0.001799450120108768165, 0.002399266826811690886 ),
 .UNSPECIFIED. ) ;
#35909 = AXIS2_PLACEMENT_3D ( 'NONE', #30696, #8581, #3965 ) ;
#35910 = ADVANCED_FACE ( 'NONE', ( #58140 ), #31763, .T. ) ;
#35911 =( GEOMETRIC_REPRESENTATION_CONTEXT ( 3 ) GLOBAL_UNCERTAINTY_ASSIGNED_CONTEXT ( ( #41918 ) ) GLOBAL_UNIT_ASSIGNED_CONTEXT ( ( #63468, #42413, #10010 ) ) REPRESENTATION_CONTEXT ( 'NONE', 'WORKASPACE' ) );
#35912 = EDGE_CURVE ( 'NONE', #51279, #49320, #6747, .T. ) ;
#35913 = PRESENTATION_LAYER_ASSIGNMENT (  '', '', ( #69588 ) ) ;
#35914 = CARTESIAN_POINT ( 'NONE',  ( 7.749999999999993783, 9.491012693391979898E-16, 0.000000000000000000 ) ) ;
#35915 = LINE ( 'NONE', #57717, #31437 ) ;
#35916 = LINE ( 'NONE', #52114, #10779 ) ;
#35917 = ORIENTED_EDGE ( 'NONE', *, *, #12783, .F. ) ;
#35918 = VECTOR ( 'NONE', #68137, 1000.000000000000000 ) ;
#35919 = EDGE_CURVE ( 'NONE', #68848, #4324, #53216, .T. ) ;
#35920 = ORIENTED_EDGE ( 'NONE', *, *, #10355, .F. ) ;
#35921 = CARTESIAN_POINT ( 'NONE',  ( 44.99999999999977263, 147.4999999999999716, 9.500000000000000000 ) ) ;
#35922 = CARTESIAN_POINT ( 'NONE',  ( -71.50000000000000000, 14.49137674618942562, 10.00000000000000000 ) ) ;
#35923 = CARTESIAN_POINT ( 'NONE',  ( -67.40499999999997272, -2.607480562269069768, 8.024999999999991473 ) ) ;
#35924 = VERTEX_POINT ( 'NONE', #44766 ) ;
#35925 = EDGE_CURVE ( 'NONE', #33393, #25339, #54900, .T. ) ;
#35926 = CARTESIAN_POINT ( 'NONE',  ( 74.99999999999998579, 50.00000000000000000, -7.000000000000000000 ) ) ;
#35927 = ADVANCED_FACE ( 'NONE', ( #6727 ), #54207, .T. ) ;
#35928 = PRESENTATION_LAYER_ASSIGNMENT (  '', '', ( #66224 ) ) ;
#35929 = ADVANCED_FACE ( 'NONE', ( #48663 ), #43402, .T. ) ;
#35930 = DIRECTION ( 'NONE',  ( -0.000000000000000000, 1.000000000000000000, 0.000000000000000000 ) ) ;
#35931 = PRESENTATION_LAYER_ASSIGNMENT (  '', '', ( #66226 ) ) ;
#35932 = ORIENTED_EDGE ( 'NONE', *, *, #34069, .F. ) ;
#35933 = ADVANCED_FACE ( 'NONE', ( #27128 ), #7092, .T. ) ;
#35934 = CARTESIAN_POINT ( 'NONE',  ( 39.74999999999999289, 0.000000000000000000, 4.000000000000000000 ) ) ;
#35935 = LINE ( 'NONE', #57381, #15815 ) ;
#35936 = SURFACE_SIDE_STYLE ('',( #14458 ) ) ;
#35937 = MECHANICAL_DESIGN_GEOMETRIC_PRESENTATION_REPRESENTATION (  '', ( #28037 ), #66233 ) ;
#35939 = PLANE ( 'NONE',  #22448 ) ;
#35938 = CARTESIAN_POINT ( 'NONE',  ( 57.00000000000000000, 16.00000000000000000, 72.50402776293826435 ) ) ;
#35940 = CARTESIAN_POINT ( 'NONE',  ( 10.01517768586949231, 147.6949999999999932, 1.839758294383810543E-15 ) ) ;
#35941 = CARTESIAN_POINT ( 'NONE',  ( -97.94499999999999318, -9.827790563157499189E-16, -8.024999999999991473 ) ) ;
#35942 = CARTESIAN_POINT ( 'NONE',  ( 4.000000000000030198, 38.93969262078591242, 89.65797985667433068 ) ) ;
#35943 = CARTESIAN_POINT ( 'NONE',  ( -72.00000000000000000, 13.41640786499872284, -7.500000000000000000 ) ) ;
#35944 = CARTESIAN_POINT ( 'NONE',  ( -72.44292637653379074, -1.166476076187852838E-15, -9.524999999999991473 ) ) ;
#35946 = ORIENTED_EDGE ( 'NONE', *, *, #11505, .T. ) ;
#35945 = VECTOR ( 'NONE', #58423, 1000.000000000000000 ) ;
#35947 = CARTESIAN_POINT ( 'NONE',  ( -139.0429263765338135, -9.058813317711329915, -2.943386871421370898 ) ) ;
#35948 =( NAMED_UNIT ( * ) PLANE_ANGLE_UNIT ( ) SI_UNIT ( $, .RADIAN. ) );
#35949 = CARTESIAN_POINT ( 'NONE',  ( -158.9950000000000045, -6.826472737025115478, 4.959722759717900331 ) ) ;
#35950 = CARTESIAN_POINT ( 'NONE',  ( -9.250000000000003553, 27.74999999999998934, 4.000000000000000000 ) ) ;
#35951 = CYLINDRICAL_SURFACE ( 'NONE', #31914, 9.524999999999991473 ) ;
#35952 = VECTOR ( 'NONE', #43691, 1000.000000000000000 ) ;
#35953 = CARTESIAN_POINT ( 'NONE',  ( 1.227708416145219032E-15, 154.9999999999999716, -10.02499999999997904 ) ) ;
#35954 = VERTEX_POINT ( 'NONE', #12016 ) ;
#35955 = CARTESIAN_POINT ( 'NONE',  ( -18.00000000000000711, 33.99999999999999289, 4.000000000000000000 ) ) ;
#35956 = VERTEX_POINT ( 'NONE', #16970 ) ;
#35957 = AXIS2_PLACEMENT_3D ( 'NONE', #57053, #63020, #30293 ) ;
#35958 = DIRECTION ( 'NONE',  ( 0.000000000000000000, 0.000000000000000000, 1.000000000000000000 ) ) ;
#35959 = ADVANCED_FACE ( 'NONE', ( #1032 ), #63205, .F. ) ;
#35960 = AXIS2_PLACEMENT_3D ( 'NONE', #29966, #3906, #31001 ) ;
#35961 = CARTESIAN_POINT ( 'NONE',  ( -144.1429263765338078, 5.598654528085800663, -7.705886871421367523 ) ) ;
#35962 = CARTESIAN_POINT ( 'NONE',  ( 71.74137931034479720, 63.10081643261027295, -9.500000000000000000 ) ) ;
#35963 = CIRCLE ( 'NONE', #41604, 0.5000000000000004441 ) ;
#35964 = CARTESIAN_POINT ( 'NONE',  ( -59.62102754835381546, -7.580807888618323886, -0.06943374021246458139 ) ) ;
#35965 = ORIENTED_EDGE ( 'NONE', *, *, #16037, .T. ) ;
#35966 = CARTESIAN_POINT ( 'NONE',  ( -163.2549999999999955, -4.716976649647092401, 6.492361379858946790 ) ) ;
#35967 = VERTEX_POINT ( 'NONE', #17669 ) ;
#35968 = CYLINDRICAL_SURFACE ( 'NONE', #49267, 0.5000000000000004441 ) ;
#35969 = CARTESIAN_POINT ( 'NONE',  ( 44.99999999999977973, 146.9999999999999716, -9.500000000000000000 ) ) ;
#35970 = EDGE_LOOP ( 'NONE', ( #31994, #63131, #25575, #4432 ) ) ;
#35971 = AXIS2_PLACEMENT_3D ( 'NONE', #36045, #30738, #20544 ) ;
#35972 = VECTOR ( 'NONE', #54843, 1000.000000000000000 ) ;
#35973 = CARTESIAN_POINT ( 'NONE',  ( 1.000000000000000888, 43.00000000000000000, 74.38749456993816978 ) ) ;
#35974 = CARTESIAN_POINT ( 'NONE',  ( -10.01517768586949231, 110.1949999999999648, -6.132527647946036459E-16 ) ) ;
#35975 = AXIS2_PLACEMENT_3D ( 'NONE', #13001, #39089, #60158 ) ;
#35976 = COLOUR_RGB ( '', 0.66274510, 0.83137255, 0.94901961) ;
#35977 = ORIENTED_EDGE ( 'NONE', *, *, #22332, .T. ) ;
#35978 = CARTESIAN_POINT ( 'NONE',  ( -58.34292637653379643, -9.058813317711329915, 2.943386871421371787 ) ) ;
#35979 = CARTESIAN_POINT ( 'NONE',  ( 8.102448949553179958, 121.5049999999999670, 5.886773742842750679 ) ) ;
#35980 = CARTESIAN_POINT ( 'NONE',  ( -72.05499999999997840, -9.827790563157499189E-16, -8.024999999999991473 ) ) ;
#35981 = CARTESIAN_POINT ( 'NONE',  ( 48.25000000000000000, 22.24999999999998579, 4.000000000000000000 ) ) ;
#35982 = VERTEX_POINT ( 'NONE', #46501 ) ;
#35983 = CARTESIAN_POINT ( 'NONE',  ( -9.058813317711338797, 138.4549999999999841, 2.943386871421373563 ) ) ;
#35984 =( NAMED_UNIT ( * ) SI_UNIT ( $, .STERADIAN. ) SOLID_ANGLE_UNIT ( ) );
#35985 = PRESENTATION_STYLE_ASSIGNMENT (( #4994 ) ) ;
#35986 = EDGE_CURVE ( 'NONE', #68105, #64619, #67931, .T. ) ;
#35987 = FILL_AREA_STYLE_COLOUR ( '', #56468 ) ;
#35988 = EDGE_LOOP ( 'NONE', ( #19381, #52748, #66962, #47970 ) ) ;
#35989 = LINE ( 'NONE', #29663, #59839 ) ;
#35990 = DIRECTION ( 'NONE',  ( -0.000000000000000000, -0.000000000000000000, 1.000000000000000000 ) ) ;
#35992 = CARTESIAN_POINT ( 'NONE',  ( -180.6550000000000011, -7.632228543268600340, -2.479861379858950166 ) ) ;
#35991 = CIRCLE ( 'NONE', #19134, 1.000000000000000888 ) ;
#35993 = ORIENTED_EDGE ( 'NONE', *, *, #51973, .T. ) ;
#35994 = DIRECTION ( 'NONE',  ( -0.000000000000000000, -1.000000000000000000, -0.000000000000000000 ) ) ;
#35995 = ADVANCED_FACE ( 'NONE', ( #66886 ), #3132, .F. ) ;
#35996 = CARTESIAN_POINT ( 'NONE',  ( 27.00000000000001776, 42.00000000000000000, 35.50000000000000000 ) ) ;
#35997 = CARTESIAN_POINT ( 'NONE',  ( -86.54292637653379927, 9.058813317711329915, 2.943386871421369566 ) ) ;
#35998 = AXIS2_PLACEMENT_3D ( 'NONE', #56609, #47132, #18949 ) ;
#35999 = VERTEX_POINT ( 'NONE', #18690 ) ;
#36000 = CARTESIAN_POINT ( 'NONE',  ( 44.00000000000000000, 18.74999999999998224, -3.750000000000000000 ) ) ;
#36001 = DIRECTION ( 'NONE',  ( 0.000000000000000000, 0.000000000000000000, 1.000000000000000000 ) ) ;
#36002 = ORIENTED_EDGE ( 'NONE', *, *, #48971, .T. ) ;
#36003 = SURFACE_SIDE_STYLE ('',( #36389 ) ) ;
#36004 = CARTESIAN_POINT ( 'NONE',  ( -93.35499999999998977, -4.716976649647093289, -6.492361379858945902 ) ) ;
#36005 = EDGE_LOOP ( 'NONE', ( #49663, #2115, #23665, #56149 ) ) ;
#36006 = CARTESIAN_POINT ( 'NONE',  ( 53.00000000000000000, 25.24999999999998579, 4.000000000000000000 ) ) ;
#36007 =( GEOMETRIC_REPRESENTATION_CONTEXT ( 3 ) GLOBAL_UNCERTAINTY_ASSIGNED_CONTEXT ( ( #4725 ) ) GLOBAL_UNIT_ASSIGNED_CONTEXT ( ( #40644, #9676, #20188 ) ) REPRESENTATION_CONTEXT ( 'NONE', 'WORKASPACE' ) );
#36008 = EDGE_CURVE ( 'NONE', #29977, #26396, #34022, .T. ) ;
#36009 = DIRECTION ( 'NONE',  ( 1.000000000000000000, 0.000000000000000000, 0.000000000000000000 ) ) ;
#36010 = STYLED_ITEM ( 'NONE', ( #50282 ), #11369 ) ;
#36011 = CARTESIAN_POINT ( 'NONE',  ( -136.5570736234661808, -1.166476076187852838E-15, -9.524999999999991473 ) ) ;
#36012 = AXIS2_PLACEMENT_3D ( 'NONE', #13714, #25307, #19683 ) ;
#36013 = CARTESIAN_POINT ( 'NONE',  ( 8.102448949553179958, 153.3950000000000102, 5.886773742842750679 ) ) ;
#36014 = CARTESIAN_POINT ( 'NONE',  ( -76.25707362346616947, 5.598654528085800663, -7.705886871421367523 ) ) ;
#36016 = ADVANCED_FACE ( 'NONE', ( #3490 ), #45794, .F. ) ;
#36015 = TOROIDAL_SURFACE ( 'NONE', #7922, 1.000000000000000000, 0.5000000000000000000 ) ;
#36017 = DIRECTION ( 'NONE',  ( 7.709882115452468306E-16, -1.000000000000000000, 0.000000000000000000 ) ) ;
#36018 = VERTEX_POINT ( 'NONE', #30243 ) ;
#36019 = CARTESIAN_POINT ( 'NONE',  ( -22.25000000000000711, 34.24999999999999289, -3.750000000000000000 ) ) ;
#36020 = CARTESIAN_POINT ( 'NONE',  ( -18.96673260019409213, -11.60629586887077203, 3.061218697616527429 ) ) ;
#36022 = CARTESIAN_POINT ( 'NONE',  ( 3.249999999999998668, 36.99999999999999289, 4.000000000000000000 ) ) ;
#36021 = DIRECTION ( 'NONE',  ( 0.000000000000000000, -0.7431448254773944662, 0.6691306063588580155 ) ) ;
#36023 = CARTESIAN_POINT ( 'NONE',  ( -124.8549999999999898, 4.716976649647094177, 6.492361379858945902 ) ) ;
#36024 = CARTESIAN_POINT ( 'NONE',  ( 8.102448949553183510, 117.9949999999999761, -5.886773742842746238 ) ) ;
#36025 = CARTESIAN_POINT ( 'NONE',  ( -126.5949999999999847, 2.607480562269073321, 8.024999999999991473 ) ) ;
#36026 = PRESENTATION_LAYER_ASSIGNMENT (  '', '', ( #22511 ) ) ;
#36027 = VECTOR ( 'NONE', #32620, 1000.000000000000000 ) ;
#36028 = PRESENTATION_STYLE_ASSIGNMENT (( #47676 ) ) ;
#36029 = VERTEX_POINT ( 'NONE', #35209 ) ;
#36030 = AXIS2_PLACEMENT_3D ( 'NONE', #46813, #36231, #58686 ) ;
#36031 = PRODUCT_DEFINITION_FORMATION_WITH_SPECIFIED_SOURCE ( 'ANY', '', #30428, .NOT_KNOWN. ) ;
#36032 = CARTESIAN_POINT ( 'NONE',  ( 72.00000000000000000, 35.92875272052971525, -7.500000000000000000 ) ) ;
#36033 = ORIENTED_EDGE ( 'NONE', *, *, #5520, .F. ) ;
#36034 = CARTESIAN_POINT ( 'NONE',  ( -167.3070736234662093, -10.01517768586948698, 6.132527647946031529E-16 ) ) ;
#36035 = CARTESIAN_POINT ( 'NONE',  ( -167.5429263765338135, 9.058813317711329915, 2.943386871421369566 ) ) ;
#36036 =( LENGTH_UNIT ( ) NAMED_UNIT ( * ) SI_UNIT ( .MILLI., .METRE. ) );
#36037 = LINE ( 'NONE', #9302, #23065 ) ;
#36038 = CARTESIAN_POINT ( 'NONE',  ( -2.607480562269074653, 125.4070736234661467, 8.025000000000000355 ) ) ;
#36039 = DIRECTION ( 'NONE',  ( -0.000000000000000000, -0.000000000000000000, -1.000000000000000000 ) ) ;
#36040 = DIRECTION ( 'NONE',  ( 0.000000000000000000, 1.000000000000000000, 0.000000000000000000 ) ) ;
#36041 = ORIENTED_EDGE ( 'NONE', *, *, #44287, .T. ) ;
#36042 = AXIS2_PLACEMENT_3D ( 'NONE', #24488, #63100, #58516 ) ;
#36043 = CARTESIAN_POINT ( 'NONE',  ( -82.19292637653380496, -10.01517768586948698, 6.132527647946031529E-16 ) ) ;
#36044 =( LENGTH_UNIT ( ) NAMED_UNIT ( * ) SI_UNIT ( .MILLI., .METRE. ) );
#36045 = CARTESIAN_POINT ( 'NONE',  ( -71.50000000000000000, 14.49137674618942562, -7.500000000000000000 ) ) ;
#36046 = EDGE_CURVE ( 'NONE', #24116, #13211, #49809, .T. ) ;
#36047 = CIRCLE ( 'NONE', #33763, 0.2500000000000002220 ) ;
#36048 = STYLED_ITEM ( 'NONE', ( #23890 ), #12423 ) ;
#36049 = CARTESIAN_POINT ( 'NONE',  ( 6.999798566743343997, 9.396926207859090496, 11.50901484383454942 ) ) ;
#36050 = EDGE_CURVE ( 'NONE', #30149, #52109, #24296, .T. ) ;
#36051 = FACE_OUTER_BOUND ( 'NONE', #60129, .T. ) ;
#36052 = ORIENTED_EDGE ( 'NONE', *, *, #47226, .F. ) ;
#36053 = CARTESIAN_POINT ( 'NONE',  ( 5.705565085145811288, 4.117671386636414077, 0.02778322089669325520 ) ) ;
#36054 = DIRECTION ( 'NONE',  ( -1.000000000000000000, -1.224646799147353207E-16, 0.000000000000000000 ) ) ;
#36055 =( NAMED_UNIT ( * ) SI_UNIT ( $, .STERADIAN. ) SOLID_ANGLE_UNIT ( ) );
#36056 = ORIENTED_EDGE ( 'NONE', *, *, #4602, .T. ) ;
#36057 = CARTESIAN_POINT ( 'NONE',  ( -103.9429263765338050, 0.000000000000000000, 9.524999999999991473 ) ) ;
#36058 = DIRECTION ( 'NONE',  ( 0.000000000000000000, 0.000000000000000000, -1.000000000000000000 ) ) ;
#36059 = CARTESIAN_POINT ( 'NONE',  ( -9.827790563157511022E-16, 131.5570736234661524, 8.025000000000000355 ) ) ;
#36060 = CYLINDRICAL_SURFACE ( 'NONE', #25933, 0.2500000000000002220 ) ;
#36061 = AXIS2_PLACEMENT_3D ( 'NONE', #23467, #57938, #4076 ) ;
#36062 = EDGE_LOOP ( 'NONE', ( #29092, #20541 ) ) ;
#36063 = DIRECTION ( 'NONE',  ( 1.000000000000000000, 0.000000000000000000, 0.000000000000000000 ) ) ;
#36064 = CARTESIAN_POINT ( 'NONE',  ( -106.5549999999999784, 0.000000000000000000, 8.024999999999991473 ) ) ;
#36065 = EDGE_LOOP ( 'NONE', ( #26091, #7723, #59787 ) ) ;
#36066 = CARTESIAN_POINT ( 'NONE',  ( 0.000000000000000000, 2.299999999999999822, 0.000000000000000000 ) ) ;
#36067 = EDGE_CURVE ( 'NONE', #28627, #26545, #27263, .T. ) ;
#36068 = DIRECTION ( 'NONE',  ( -0.000000000000000000, -0.000000000000000000, -1.000000000000000000 ) ) ;
#36069 = ADVANCED_FACE ( 'NONE', ( #24625 ), #55627, .T. ) ;
#36070 = CARTESIAN_POINT ( 'NONE',  ( -74.99999999999998579, 50.00000000000000000, 7.500000000000000000 ) ) ;
#36071 =( NAMED_UNIT ( * ) PLANE_ANGLE_UNIT ( ) SI_UNIT ( $, .RADIAN. ) );
#36072 = COLOUR_RGB ( '', 0.09019608, 0.27058824, 0.51372549) ;
#36073 = ORIENTED_EDGE ( 'NONE', *, *, #58691, .F. ) ;
#36074 = CARTESIAN_POINT ( 'NONE',  ( -68.54499999999998749, -7.632228543268600340, -2.479861379858950166 ) ) ;
#36075 = VERTEX_POINT ( 'NONE', #19002 ) ;
#36076 = AXIS2_PLACEMENT_3D ( 'NONE', #3351, #41075, #24845 ) ;
#36077 = CARTESIAN_POINT ( 'NONE',  ( 59.00000000000000000, 11.99999999999999822, 3.499999999999992895 ) ) ;
#36078 = LINE ( 'NONE', #4030, #43630 ) ;
#36079 = EDGE_CURVE ( 'NONE', #57523, #7926, #5951, .T. ) ;
#36080 = UNCERTAINTY_MEASURE_WITH_UNIT (LENGTH_MEASURE( 1.000000000000000082E-05 ), #61400, 'distance_accuracy_value', 'NONE');
#36081 = ORIENTED_EDGE ( 'NONE', *, *, #50914, .T. ) ;
#36082 = DIRECTION ( 'NONE',  ( 0.000000000000000000, 0.000000000000000000, -1.000000000000000000 ) ) ;
#36083 = DIRECTION ( 'NONE',  ( -1.000000000000000000, -0.000000000000000000, -0.000000000000000000 ) ) ;
#36084 = EDGE_CURVE ( 'NONE', #52546, #58067, #59884, .T. ) ;
#36085 = DIRECTION ( 'NONE',  ( 0.000000000000000000, 0.000000000000000000, -1.000000000000000000 ) ) ;
#36086 = ORIENTED_EDGE ( 'NONE', *, *, #11480, .T. ) ;
#36087 = CARTESIAN_POINT ( 'NONE',  ( -74.99999999999998579, 50.00000000000000000, -11.50000000000000000 ) ) ;
#36088 = ORIENTED_EDGE ( 'NONE', *, *, #16931, .F. ) ;
#36089 = EDGE_CURVE ( 'NONE', #54598, #11986, #51446, .T. ) ;
#36090 = DIRECTION ( 'NONE',  ( 0.000000000000000000, -0.3420201433256629953, -0.9396926207859104263 ) ) ;
#36091 = DIRECTION ( 'NONE',  ( 1.000000000000000000, 0.000000000000000000, 0.000000000000000000 ) ) ;
#36092 = CARTESIAN_POINT ( 'NONE',  ( -45.50000000000000000, -1.469576158976824302E-14, -9.500000000000000000 ) ) ;
#36093 = CARTESIAN_POINT ( 'NONE',  ( -169.8570736234661922, -5.598654528085803328, -7.705886871421366635 ) ) ;
#36094 = AXIS2_PLACEMENT_3D ( 'NONE', #29066, #54766, #6579 ) ;
#36095 = CARTESIAN_POINT ( 'NONE',  ( 10.01517768586949408, 126.6950000000000074, 1.839758294383810543E-15 ) ) ;
#36096 = CARTESIAN_POINT ( 'NONE',  ( -102.0570736234661808, 0.000000000000000000, 9.524999999999991473 ) ) ;
#36097 = AXIS2_PLACEMENT_3D ( 'NONE', #66505, #18325, #44746 ) ;
#36098 = CARTESIAN_POINT ( 'NONE',  ( 0.000000000000000000, 114.9999999999999574, 16.50000000000000000 ) ) ;
#36099 = AXIS2_PLACEMENT_3D ( 'NONE', #36495, #64207, #25877 ) ;
#36100 = EDGE_CURVE ( 'NONE', #29677, #25215, #43078, .T. ) ;
#36101 = CARTESIAN_POINT ( 'NONE',  ( 3.000000000000000444, 3.673940397442060361E-16, 32.50000000000000000 ) ) ;
#36102 = VERTEX_POINT ( 'NONE', #51049 ) ;
#36103 = FACE_OUTER_BOUND ( 'NONE', #35166, .T. ) ;
#36104 = CARTESIAN_POINT ( 'NONE',  ( -105.8070736234661666, 10.01517768586948698, -1.839758294383808966E-15 ) ) ;
#36107 = CIRCLE ( 'NONE', #64143, 0.5000000000000004441 ) ;
#36106 = SURFACE_STYLE_FILL_AREA ( #35408 ) ;
#36105 = DIRECTION ( 'NONE',  ( 0.000000000000000000, 0.000000000000000000, -1.000000000000000000 ) ) ;
#36108 = DIRECTION ( 'NONE',  ( -0.000000000000000000, -0.000000000000000000, -1.000000000000000000 ) ) ;
#36109 = CARTESIAN_POINT ( 'NONE',  ( -152.4550000000000125, 7.632228543268599452, -2.479861379858951942 ) ) ;
#36110 = CARTESIAN_POINT ( 'NONE',  ( -75.00000000000000000, 8.554728201919930441, 6.928664365919924961 ) ) ;
#36111 = CARTESIAN_POINT ( 'NONE',  ( -60.05707362346616662, 0.000000000000000000, 9.524999999999991473 ) ) ;
#36112 = AXIS2_PLACEMENT_3D ( 'NONE', #56269, #8095, #24591 ) ;
#36113 = CARTESIAN_POINT ( 'NONE',  ( -153.2949999999999875, -2.607480562269069768, 8.024999999999991473 ) ) ;
#36114 = CARTESIAN_POINT ( 'NONE',  ( -145.7950000000000443, 2.607480562269069324, -8.024999999999993250 ) ) ;
#36115 =( GEOMETRIC_REPRESENTATION_CONTEXT ( 3 ) GLOBAL_UNCERTAINTY_ASSIGNED_CONTEXT ( ( #35558 ) ) GLOBAL_UNIT_ASSIGNED_CONTEXT ( ( #503, #22033, #28670 ) ) REPRESENTATION_CONTEXT ( 'NONE', 'WORKASPACE' ) );
#36116 = ORIENTED_EDGE ( 'NONE', *, *, #19374, .F. ) ;
#36117 = STYLED_ITEM ( 'NONE', ( #17120 ), #54231 ) ;
#36118 = CARTESIAN_POINT ( 'NONE',  ( 44.24703880899743069, 10.19173881602633536, -3.568710496479958749 ) ) ;
#36119 =( REPRESENTATION_RELATIONSHIP ('NONE','NONE', #5102, #40670 ) REPRESENTATION_RELATIONSHIP_WITH_TRANSFORMATION ( #4326 )SHAPE_REPRESENTATION_RELATIONSHIP( ) );
#36120 = DIRECTION ( 'NONE',  ( 0.000000000000000000, -1.000000000000000000, 0.000000000000000000 ) ) ;
#36121 =( NAMED_UNIT ( * ) SI_UNIT ( $, .STERADIAN. ) SOLID_ANGLE_UNIT ( ) );
#36122 = UNCERTAINTY_MEASURE_WITH_UNIT (LENGTH_MEASURE( 1.000000000000000082E-05 ), #50703, 'distance_accuracy_value', 'NONE');
#36123 = CARTESIAN_POINT ( 'NONE',  ( -59.75499999999998835, 4.716976649647091513, -6.492361379858946790 ) ) ;
#36124 = AXIS2_PLACEMENT_3D ( 'NONE', #21217, #53590, #31780 ) ;
#36125 =( LENGTH_UNIT ( ) NAMED_UNIT ( * ) SI_UNIT ( .MILLI., .METRE. ) );
#36126 = CARTESIAN_POINT ( 'NONE',  ( -66.29499999999998749, -2.607480562269069768, 8.024999999999991473 ) ) ;
#36127 = CARTESIAN_POINT ( 'NONE',  ( 9.058813317711337021, 154.6549999999999727, 2.943386871421375783 ) ) ;
#36128 = DIRECTION ( 'NONE',  ( 1.000000000000000000, 0.000000000000000000, 0.000000000000000000 ) ) ;
#36129 = AXIS2_PLACEMENT_3D ( 'NONE', #4111, #3397, #24891 ) ;
#36130 = CARTESIAN_POINT ( 'NONE',  ( 36.00000000000002132, 5.000000000000000000, -77.00402776293825013 ) ) ;
#36131 = UNCERTAINTY_MEASURE_WITH_UNIT (LENGTH_MEASURE( 1.000000000000000082E-05 ), #53572, 'distance_accuracy_value', 'NONE');
#36132 = PRESENTATION_LAYER_ASSIGNMENT (  '', '', ( #14788 ) ) ;
#36133 = FILL_AREA_STYLE ('',( #9398 ) ) ;
#36134 = CARTESIAN_POINT ( 'NONE',  ( 60.00000000000000000, 1.797044900979284448E-15, -10.00000000000000000 ) ) ;
#36135 = EDGE_CURVE ( 'NONE', #23192, #19551, #2808, .T. ) ;
#36136 = AXIS2_PLACEMENT_3D ( 'NONE', #22938, #44769, #45470 ) ;
#36137 = PRESENTATION_STYLE_ASSIGNMENT (( #9403 ) ) ;
#36138 = CARTESIAN_POINT ( 'NONE',  ( -178.4929263765338021, -8.102448949553174629, 5.886773742842742685 ) ) ;
#36139 = AXIS2_PLACEMENT_3D ( 'NONE', #21450, #27402, #64367 ) ;
#36140 = DIRECTION ( 'NONE',  ( 0.000000000000000000, 0.000000000000000000, -1.000000000000000000 ) ) ;
#36141 = CARTESIAN_POINT ( 'NONE',  ( -195.0000000000000000, 1.166476076187852838E-15, -9.524999999999991473 ) ) ;
#36142 = CARTESIAN_POINT ( 'NONE',  ( 0.000000000000000000, 0.000000000000000000, 0.7500000000000000000 ) ) ;
#36143 = DIRECTION ( 'NONE',  ( -0.000000000000000000, -0.000000000000000000, 1.000000000000000000 ) ) ;
#36144 = ORIENTED_EDGE ( 'NONE', *, *, #29960, .T. ) ;
#36145 = EDGE_LOOP ( 'NONE', ( #63702, #4090, #69606, #22447 ) ) ;
#36146 = DIRECTION ( 'NONE',  ( 1.000000000000000000, -0.000000000000000000, 0.000000000000000000 ) ) ;
#36147 =( BOUNDED_CURVE ( )  B_SPLINE_CURVE ( 2, ( #61753, #40705, #8676, #20251, #14647, #56860, #14287, #30102, #25188, #35050, #56498 ),
 .UNSPECIFIED., .F., .F. ) 
 B_SPLINE_CURVE_WITH_KNOTS ( ( 3, 2, 2, 2, 2, 3 ),
 ( 0.2608695652173851354, 0.2630434782608633282, 0.2652173913043415765, 0.2673913043478197693, 0.2695652173912979621, 0.2717391304347761549 ),
 .UNSPECIFIED. ) 
 CURVE ( )  GEOMETRIC_REPRESENTATION_ITEM ( )  RATIONAL_B_SPLINE_CURVE ( ( 1.000000000000138778, 0.9510565162950147533, 1.000000000000000000, 0.9510565162951535312, 1.000000000000000000, 0.9510565162951535312, 1.000000000000000000, 0.9510565162951535312, 1.000000000000000000, 0.9510565162952985263, 0.9999999999998550049 ) ) 
 REPRESENTATION_ITEM ( '' )  );
#36148 = MECHANICAL_DESIGN_GEOMETRIC_PRESENTATION_REPRESENTATION (  '', ( #30475 ), #32761 ) ;
#36149 = EDGE_CURVE ( 'NONE', #17985, #31091, #61923, .T. ) ;
#36150 = PRESENTATION_LAYER_ASSIGNMENT (  '', '', ( #28256 ) ) ;
#36151 = CARTESIAN_POINT ( 'NONE',  ( -20.57648122633967347, 114.5694469452588038, 10.27659575647942169 ) ) ;
#36152 = CARTESIAN_POINT ( 'NONE',  ( 22.84135002011590387, 24.77014762460473563, -27.27734489800906914 ) ) ;
#36154 = EDGE_CURVE ( 'NONE', #22530, #7454, #40865, .T. ) ;
#36153 = CARTESIAN_POINT ( 'NONE',  ( -77.00707362346618368, -8.102448949553174629, -5.886773742842741797 ) ) ;
#36155 = ORIENTED_EDGE ( 'NONE', *, *, #22716, .F. ) ;
#36156 = PRESENTATION_LAYER_ASSIGNMENT (  '', '', ( #107 ) ) ;
#36157 = ORIENTED_EDGE ( 'NONE', *, *, #42530, .F. ) ;
#36158 = CARTESIAN_POINT ( 'NONE',  ( -108.2070736234670818, 3.094860106633760211, 9.524999999988855492 ) ) ;
#36159 = CYLINDRICAL_SURFACE ( 'NONE', #10671, 19.99999999999998934 ) ;
#36160 = EDGE_CURVE ( 'NONE', #19151, #43113, #26699, .T. ) ;
#36161 = CARTESIAN_POINT ( 'NONE',  ( -24.21231517720798365, 117.4999999999999716, 7.000000000000000000 ) ) ;
#36162 = ORIENTED_EDGE ( 'NONE', *, *, #67853, .F. ) ;
#36163 = EDGE_CURVE ( 'NONE', #58121, #16885, #37501, .T. ) ;
#36164 = CARTESIAN_POINT ( 'NONE',  ( -8.102448949553181734, 120.6049999999999756, 5.886773742842747126 ) ) ;
#36165 = CARTESIAN_POINT ( 'NONE',  ( 66.74999999999998579, 36.75000000000000000, -3.750000000000000000 ) ) ;
#36166 = VERTEX_POINT ( 'NONE', #31292 ) ;
#36167 =( GEOMETRIC_REPRESENTATION_CONTEXT ( 3 ) GLOBAL_UNCERTAINTY_ASSIGNED_CONTEXT ( ( #65112 ) ) GLOBAL_UNIT_ASSIGNED_CONTEXT ( ( #59386, #8385, #67449 ) ) REPRESENTATION_CONTEXT ( 'NONE', 'WORKASPACE' ) );
#36168 = SURFACE_SIDE_STYLE ('',( #53691 ) ) ;
#36169 = CARTESIAN_POINT ( 'NONE',  ( -112.7949999999999733, 2.607480562269068880, -8.024999999999993250 ) ) ;
#36170 = VERTEX_POINT ( 'NONE', #32000 ) ;
#36171 =( NAMED_UNIT ( * ) SI_UNIT ( $, .STERADIAN. ) SOLID_ANGLE_UNIT ( ) );
#36172 = CARTESIAN_POINT ( 'NONE',  ( -156.4429263765338192, -1.166476076187852838E-15, -9.524999999999991473 ) ) ;
#36173 = FILL_AREA_STYLE_COLOUR ( '', #46371 ) ;
#36174 = ADVANCED_FACE ( 'NONE', ( #69305 ), #41913, .T. ) ;
#36175 = CARTESIAN_POINT ( 'NONE',  ( -179.0070736234661695, -8.102448949553174629, -5.886773742842741797 ) ) ;
#36176 = ORIENTED_EDGE ( 'NONE', *, *, #49266, .F. ) ;
#36177 = CARTESIAN_POINT ( 'NONE',  ( 6.826472737025119919, 157.8929263765338078, 4.959722759717908325 ) ) ;
#36178 = DIRECTION ( 'NONE',  ( -1.000000000000000000, -0.000000000000000000, -0.000000000000000000 ) ) ;
#36179 = AXIS2_PLACEMENT_3D ( 'NONE', #6771, #17707, #18030 ) ;
#36180 = EDGE_CURVE ( 'NONE', #65996, #20493, #63259, .T. ) ;
#36181 = COLOUR_RGB ( '', 0.08235294, 0.09019608, 0.10196078) ;
#36182 = DIRECTION ( 'NONE',  ( 0.000000000000000000, -0.7071067811865474617, -0.7071067811865474617 ) ) ;
#36183 = ORIENTED_EDGE ( 'NONE', *, *, #59164, .F. ) ;
#36184 = AXIS2_PLACEMENT_3D ( 'NONE', #22590, #12709, #27825 ) ;
#36185 = CARTESIAN_POINT ( 'NONE',  ( 20.26251832593580104, 115.0246525964671207, -10.00000000000000178 ) ) ;
#36186 = VERTEX_POINT ( 'NONE', #36646 ) ;
#36187 =( NAMED_UNIT ( * ) PLANE_ANGLE_UNIT ( ) SI_UNIT ( $, .RADIAN. ) );
#36188 = CARTESIAN_POINT ( 'NONE',  ( 47.50000000000000000, 14.49137674618942562, 9.500000000000000000 ) ) ;
#36189 = CARTESIAN_POINT ( 'NONE',  ( -61.94292637653379785, 0.000000000000000000, 9.524999999999991473 ) ) ;
#36190 = FACE_OUTER_BOUND ( 'NONE', #2976, .T. ) ;
#36191 = CARTESIAN_POINT ( 'NONE',  ( -124.7049999999999841, 2.607480562269073321, 8.024999999999991473 ) ) ;
#36192 = DIRECTION ( 'NONE',  ( -0.000000000000000000, 1.000000000000000000, -0.000000000000000000 ) ) ;
#36193 = CARTESIAN_POINT ( 'NONE',  ( -72.00000000000000000, 36.32520566882265456, 7.500000000000000000 ) ) ;
#36194 = CARTESIAN_POINT ( 'NONE',  ( 45.00000000000000000, 9.999999999999982236, 6.000000000000000888 ) ) ;
#36195 = FACE_OUTER_BOUND ( 'NONE', #53558, .T. ) ;
#36196 = DIRECTION ( 'NONE',  ( -1.000000000000000000, 0.000000000000000000, 0.000000000000000000 ) ) ;
#36197 = CARTESIAN_POINT ( 'NONE',  ( 0.000000000000000000, 2.500000000000000000, 0.000000000000000000 ) ) ;
#36198 = ORIENTED_EDGE ( 'NONE', *, *, #59030, .F. ) ;
#36199 = AXIS2_PLACEMENT_3D ( 'NONE', #68422, #35724, #48054 ) ;
#36200 = VERTEX_POINT ( 'NONE', #20773 ) ;
#36201 = CARTESIAN_POINT ( 'NONE',  ( -71.49999999999998579, 64.07124727947029896, -7.000000000000000000 ) ) ;
#36202 = FACE_OUTER_BOUND ( 'NONE', #5216, .T. ) ;
#36203 = CARTESIAN_POINT ( 'NONE',  ( -34.99999999999999289, 99.99999999999998579, 10.00000000000000000 ) ) ;
#36204 = ORIENTED_EDGE ( 'NONE', *, *, #45647, .T. ) ;
#36205 = DIRECTION ( 'NONE',  ( 0.000000000000000000, 0.000000000000000000, -1.000000000000000000 ) ) ;
#36206 = CARTESIAN_POINT ( 'NONE',  ( -182.9050000000000011, 2.607480562269068880, -8.024999999999993250 ) ) ;
#36207 = EDGE_CURVE ( 'NONE', #25561, #55142, #39679, .T. ) ;
#36208 = CARTESIAN_POINT ( 'NONE',  ( 34.99999999999992895, 112.9999999999999858, -7.500000000000000000 ) ) ;
#36209 = CARTESIAN_POINT ( 'NONE',  ( -51.05707362346617373, 0.000000000000000000, 9.524999999999991473 ) ) ;
#36210 = VECTOR ( 'NONE', #18962, 1000.000000000000000 ) ;
#36211 = CARTESIAN_POINT ( 'NONE',  ( -174.8949999999999818, 6.826472737025115478, 4.959722759717899443 ) ) ;
#36212 = EDGE_CURVE ( 'NONE', #23656, #18515, #1914, .T. ) ;
#36213 =( LENGTH_UNIT ( ) NAMED_UNIT ( * ) SI_UNIT ( .MILLI., .METRE. ) );
#36214 = VERTEX_POINT ( 'NONE', #9876 ) ;
#36215 = PRESENTATION_LAYER_ASSIGNMENT (  '', '', ( #63143 ) ) ;
#36216 = VECTOR ( 'NONE', #19482, 1000.000000000000000 ) ;
#36217 = DIRECTION ( 'NONE',  ( -0.000000000000000000, -0.000000000000000000, -1.000000000000000000 ) ) ;
#36218 = CARTESIAN_POINT ( 'NONE',  ( 57.00000000000000000, 15.00000000000000000, 34.49999999999998579 ) ) ;
#36219 = CARTESIAN_POINT ( 'NONE',  ( -88.70499999999998408, 2.607480562269073321, 8.024999999999991473 ) ) ;
#36220 = CARTESIAN_POINT ( 'NONE',  ( 7.911516905016148904, 154.4999999999999432, 5.322522116219993826 ) ) ;
#36221 = AXIS2_PLACEMENT_3D ( 'NONE', #68164, #41105, #13994 ) ;
#36222 = CARTESIAN_POINT ( 'NONE',  ( -86.39499999999998181, -6.826472737025113702, -4.959722759717900331 ) ) ;
#36223 = CARTESIAN_POINT ( 'NONE',  ( 10.01517768586949231, 124.8049999999999642, 1.839758294383810543E-15 ) ) ;
#36224 = CARTESIAN_POINT ( 'NONE',  ( -71.09499999999999886, -2.607480562269071545, -8.024999999999991473 ) ) ;
#36225 = DIRECTION ( 'NONE',  ( 0.000000000000000000, 1.000000000000000000, 0.000000000000000000 ) ) ;
#36226 = CARTESIAN_POINT ( 'NONE',  ( 1.999798566743339334, 49.09558629977726696, 2.000000000000000000 ) ) ;
#36227 = CIRCLE ( 'NONE', #57536, 26.49999999999999645 ) ;
#36228 = FACE_OUTER_BOUND ( 'NONE', #335, .T. ) ;
#36229 = UNCERTAINTY_MEASURE_WITH_UNIT (LENGTH_MEASURE( 1.000000000000000082E-05 ), #22598, 'distance_accuracy_value', 'NONE');
#36230 = PRESENTATION_LAYER_ASSIGNMENT (  '', '', ( #31718 ) ) ;
#36231 = DIRECTION ( 'NONE',  ( 0.000000000000000000, 1.000000000000000000, -0.000000000000000000 ) ) ;
#36232 = DIRECTION ( 'NONE',  ( -1.000000000000000000, 0.000000000000000000, 0.000000000000000000 ) ) ;
#36233 = ORIENTED_EDGE ( 'NONE', *, *, #33012, .F. ) ;
#36234 = CARTESIAN_POINT ( 'NONE',  ( -104.5429263765337993, 9.058813317711329915, 2.943386871421369566 ) ) ;
#36235 = CARTESIAN_POINT ( 'NONE',  ( -129.7450000000000045, 4.716976649647094177, 6.492361379858945902 ) ) ;
#36236 =( NAMED_UNIT ( * ) SI_UNIT ( $, .STERADIAN. ) SOLID_ANGLE_UNIT ( ) );
#36237 = CYLINDRICAL_SURFACE ( 'NONE', #49459, 1.000000000000000888 ) ;
#36238 = MECHANICAL_DESIGN_GEOMETRIC_PRESENTATION_REPRESENTATION (  '', ( #12541 ), #39608 ) ;
#36239 = EDGE_CURVE ( 'NONE', #34430, #69671, #56511, .T. ) ;
#36240 = DIRECTION ( 'NONE',  ( 0.000000000000000000, 0.000000000000000000, -1.000000000000000000 ) ) ;
#36241 = CARTESIAN_POINT ( 'NONE',  ( 4.000000000000002665, 43.00000000000000000, -79.00402776293826435 ) ) ;
#36242 = ORIENTED_EDGE ( 'NONE', *, *, #14223, .T. ) ;
#36243 = ORIENTED_EDGE ( 'NONE', *, *, #60745, .T. ) ;
#36244 = FACE_BOUND ( 'NONE', #39467, .T. ) ;
#36245 = CARTESIAN_POINT ( 'NONE',  ( -87.50000000000000000, -8.499999999999989342, 21.00000000000000000 ) ) ;
#36246 = UNCERTAINTY_MEASURE_WITH_UNIT (LENGTH_MEASURE( 1.000000000000000082E-05 ), #15037, 'distance_accuracy_value', 'NONE');
#36247 = TOROIDAL_SURFACE ( 'NONE', #64269, 9.525000000000000355, 1.000000000000000888 ) ;
#36248 = EDGE_CURVE ( 'NONE', #44275, #4197, #30957, .T. ) ;
#36249 = FILL_AREA_STYLE_COLOUR ( '', #1221 ) ;
#36250 = DIRECTION ( 'NONE',  ( -1.734723475976803545E-15, 0.7431448254773944662, 0.6691306063588580155 ) ) ;
#36251 = AXIS2_PLACEMENT_3D ( 'NONE', #40170, #66167, #23956 ) ;
#36252 =( NAMED_UNIT ( * ) SI_UNIT ( $, .STERADIAN. ) SOLID_ANGLE_UNIT ( ) );
#36253 = SURFACE_SIDE_STYLE ('',( #47518 ) ) ;
#36254 = ORIENTED_EDGE ( 'NONE', *, *, #28495, .F. ) ;
#36255 = CARTESIAN_POINT ( 'NONE',  ( -122.4549999999999983, 7.632228543268599452, -2.479861379858951942 ) ) ;
#36256 = ORIENTED_EDGE ( 'NONE', *, *, #67963, .F. ) ;
#36257 = PLANE ( 'NONE',  #6146 ) ;
#36258 = CARTESIAN_POINT ( 'NONE',  ( -121.4070736234661751, 3.094860106618428031, -9.524999999999993250 ) ) ;
#36259 = EDGE_CURVE ( 'NONE', #50952, #29891, #9341, .T. ) ;
#36260 = ORIENTED_EDGE ( 'NONE', *, *, #68555, .F. ) ;
#36261 = DIRECTION ( 'NONE',  ( 0.5000000000000003331, -0.8660254037844383745, 0.000000000000000000 ) ) ;
#36262 = CARTESIAN_POINT ( 'NONE',  ( 60.00000000000000000, 1.797044900979284448E-15, 10.50000000000000000 ) ) ;
#36263 = ORIENTED_EDGE ( 'NONE', *, *, #24154, .F. ) ;
#36264 = DIRECTION ( 'NONE',  ( 0.000000000000000000, 0.000000000000000000, 1.000000000000000000 ) ) ;
#36265 = CARTESIAN_POINT ( 'NONE',  ( -9.058813317711338797, 146.3449999999999989, 2.943386871421373563 ) ) ;
#36266 = ORIENTED_EDGE ( 'NONE', *, *, #21472, .T. ) ;
#36267 = VECTOR ( 'NONE', #41905, 1000.000000000000000 ) ;
#36268 = DIRECTION ( 'NONE',  ( 1.000000000000000000, 0.000000000000000000, 0.000000000000000000 ) ) ;
#36269 = CARTESIAN_POINT ( 'NONE',  ( 6.778496103158111019, 154.4256832137428717, 6.848681790822515936 ) ) ;
#36270 =( NAMED_UNIT ( * ) PLANE_ANGLE_UNIT ( ) SI_UNIT ( $, .RADIAN. ) );
#36271 = DIRECTION ( 'NONE',  ( 1.000000000000000000, 0.000000000000000000, 0.000000000000000000 ) ) ;
#36272 = ORIENTED_EDGE ( 'NONE', *, *, #68284, .F. ) ;
#36273 = CARTESIAN_POINT ( 'NONE',  ( 7.632228543268607446, 116.0429263765338277, 2.479861379858954606 ) ) ;
#36274 = FACE_OUTER_BOUND ( 'NONE', #50328, .T. ) ;
#36275 = UNCERTAINTY_MEASURE_WITH_UNIT (LENGTH_MEASURE( 1.000000000000000082E-05 ), #14419, 'distance_accuracy_value', 'NONE');
#36276 = CARTESIAN_POINT ( 'NONE',  ( 24.75000000000000355, 36.75000000000000000, 4.000000000000000000 ) ) ;
#36277 = CIRCLE ( 'NONE', #4740, 4.000000000000003553 ) ;
#36278 = CARTESIAN_POINT ( 'NONE',  ( 45.00000000000000000, 10.69371294336137979, 6.000000000000000888 ) ) ;
#36279 = EDGE_CURVE ( 'NONE', #29817, #30586, #49844, .T. ) ;
#36280 = DIRECTION ( 'NONE',  ( 0.000000000000000000, 0.000000000000000000, 1.000000000000000000 ) ) ;
#36281 = ORIENTED_EDGE ( 'NONE', *, *, #41645, .F. ) ;
#36282 = COLOUR_RGB ( '', 0.09019608, 0.27058824, 0.51372549) ;
#36283 = CARTESIAN_POINT ( 'NONE',  ( 40.99999999999997868, 107.7459666924147967, 3.050022167383940719 ) ) ;
#36284 = ORIENTED_EDGE ( 'NONE', *, *, #5147, .F. ) ;
#36285 = CARTESIAN_POINT ( 'NONE',  ( -57.44292637653381206, -1.166476076187852838E-15, -9.524999999999991473 ) ) ;
#36286 = DIRECTION ( 'NONE',  ( 0.000000000000000000, 1.000000000000000000, 0.000000000000000000 ) ) ;
#36287 = CARTESIAN_POINT ( 'NONE',  ( -4.041451884327381450, -7.000000000000002665, 1.082903768654759791 ) ) ;
#36288 = CARTESIAN_POINT ( 'NONE',  ( -155.3050000000000068, 8.437984349512085203, -1.550032578732815448E-15 ) ) ;
#36290 = EDGE_LOOP ( 'NONE', ( #53514, #27269, #45192, #38970 ) ) ;
#36289 = MECHANICAL_DESIGN_GEOMETRIC_PRESENTATION_REPRESENTATION (  '', ( #10442 ), #5895 ) ;
#36291 = SURFACE_STYLE_FILL_AREA ( #47556 ) ;
#36292 = UNCERTAINTY_MEASURE_WITH_UNIT (LENGTH_MEASURE( 1.000000000000000082E-05 ), #7679, 'distance_accuracy_value', 'NONE');
#36293 = TOROIDAL_SURFACE ( 'NONE', #26141, 10.49999999999999822, 0.5000000000000000000 ) ;
#36294 = PLANE ( 'NONE',  #28355 ) ;
#36295 = CARTESIAN_POINT ( 'NONE',  ( -53.01121866695764595, -10.53184416402257462, 3.891476709836703574 ) ) ;
#36296 = CARTESIAN_POINT ( 'NONE',  ( -70.34292637653381064, -9.058813317711329915, 2.943386871421371787 ) ) ;
#36297 = CARTESIAN_POINT ( 'NONE',  ( 2.607480562268992941, 146.7929263765338419, -8.025000000000060751 ) ) ;
#36298 = ORIENTED_EDGE ( 'NONE', *, *, #12007, .F. ) ;
#36299 = EDGE_LOOP ( 'NONE', ( #27449, #5519, #12503, #30780 ) ) ;
#36300 = CARTESIAN_POINT ( 'NONE',  ( 22.39276236906906448, 26.60476906391062002, 27.44839360434220410 ) ) ;
#36301 =( NAMED_UNIT ( * ) PLANE_ANGLE_UNIT ( ) SI_UNIT ( $, .RADIAN. ) );
#36302 = COLOUR_RGB ( '', 0.66274510, 0.83137255, 0.94901961) ;
#36303 = CARTESIAN_POINT ( 'NONE',  ( -61.55499999999998550, 0.000000000000000000, 8.024999999999991473 ) ) ;
#36304 = EDGE_LOOP ( 'NONE', ( #36366, #39657, #23847, #49539 ) ) ;
#36305 = LINE ( 'NONE', #57726, #46119 ) ;
#36306 = CARTESIAN_POINT ( 'NONE',  ( -66.49999999999998579, 50.00000000000000000, 11.50000000000000000 ) ) ;
#36307 = CARTESIAN_POINT ( 'NONE',  ( -90.80707362346615241, 10.01517768586948698, -1.839758294383808966E-15 ) ) ;
#36308 = FACE_BOUND ( 'NONE', #65181, .T. ) ;
#36309 = VERTEX_POINT ( 'NONE', #5948 ) ;
#36310 = STYLED_ITEM ( 'NONE', ( #16647 ), #25798 ) ;
#36311 = CARTESIAN_POINT ( 'NONE',  ( -34.01388385445504525, -9.805546523439568674, -3.361664814432062887 ) ) ;
#36312 = CIRCLE ( 'NONE', #40759, 0.2500000000000002220 ) ;
#36314 = PRESENTATION_STYLE_ASSIGNMENT (( #40185 ) ) ;
#36313 = CARTESIAN_POINT ( 'NONE',  ( 10.99999999999999645, 11.99999999999999289, -3.499999999999991118 ) ) ;
#36315 = CARTESIAN_POINT ( 'NONE',  ( 3.094860106618431583, 147.0949999999999704, 9.525000000000000355 ) ) ;
#36316 = CARTESIAN_POINT ( 'NONE',  ( -98.54499999999998749, -7.632228543268600340, -2.479861379858950166 ) ) ;
#36317 = CONICAL_SURFACE ( 'NONE', #46405, 3.600000000000005862, 0.7853981633974447263 ) ;
#36318 = CIRCLE ( 'NONE', #10430, 0.5000000000000004441 ) ;
#36319 = CARTESIAN_POINT ( 'NONE',  ( 26.00000000000001776, -3.148064030671221758, 34.49999999999999289 ) ) ;
#36320 = UNCERTAINTY_MEASURE_WITH_UNIT (LENGTH_MEASURE( 1.000000000000000082E-05 ), #14261, 'distance_accuracy_value', 'NONE');
#36321 = DIRECTION ( 'NONE',  ( 0.000000000000000000, 0.000000000000000000, 1.000000000000000000 ) ) ;
#36322 = VERTEX_POINT ( 'NONE', #60117 ) ;
#36323 = CARTESIAN_POINT ( 'NONE',  ( -135.4429263765338192, -1.166476076187852838E-15, -9.524999999999991473 ) ) ;
#36324 = SURFACE_STYLE_USAGE ( .BOTH. , #37023 ) ;
#36325 = DIRECTION ( 'NONE',  ( 1.000000000000000000, -0.000000000000000000, -0.000000000000000000 ) ) ;
#36326 = CARTESIAN_POINT ( 'NONE',  ( -156.4449999999999932, 0.000000000000000000, 8.024999999999991473 ) ) ;
#36327 = SURFACE_STYLE_USAGE ( .BOTH. , #2573 ) ;
#36328 = CARTESIAN_POINT ( 'NONE',  ( 18.00000000000000711, 31.24999999999999289, 3.750000000000000000 ) ) ;
#36329 = CIRCLE ( 'NONE', #60977, 0.5000000000000004441 ) ;
#36330 = EDGE_CURVE ( 'NONE', #12034, #40909, #26182, .T. ) ;
#36331 = DIRECTION ( 'NONE',  ( -0.000000000000000000, -1.000000000000000000, -0.000000000000000000 ) ) ;
#36332 = VERTEX_POINT ( 'NONE', #1311 ) ;
#36333 = SURFACE_STYLE_FILL_AREA ( #27687 ) ;
#36334 = VERTEX_POINT ( 'NONE', #38368 ) ;
#36335 = AXIS2_PLACEMENT_3D ( 'NONE', #22490, #65400, #22844 ) ;
#36336 = CARTESIAN_POINT ( 'NONE',  ( 5.185928986913072691, -2.291132984336067935, 5.017707510222361833 ) ) ;
#36338 = UNCERTAINTY_MEASURE_WITH_UNIT (LENGTH_MEASURE( 1.000000000000000082E-05 ), #39730, 'distance_accuracy_value', 'NONE');
#36337 = TOROIDAL_SURFACE ( 'NONE', #10497, 0.5000000000000000000, 0.2500000000000000000 ) ;
#36339 =( NAMED_UNIT ( * ) SI_UNIT ( $, .STERADIAN. ) SOLID_ANGLE_UNIT ( ) );
#36340 = CARTESIAN_POINT ( 'NONE',  ( -45.00000000000000000, 9.372809501821778966, 6.584099566153143179 ) ) ;
#36341 = DIRECTION ( 'NONE',  ( -1.000000000000000000, 0.000000000000000000, 0.000000000000000000 ) ) ;
#36342 = ADVANCED_FACE ( 'NONE', ( #28419 ), #27392, .T. ) ;
#36343 = CARTESIAN_POINT ( 'NONE',  ( -57.66965831571685897, -8.499999999999992895, 0.3729812355688906789 ) ) ;
#36344 = CONICAL_SURFACE ( 'NONE', #52098, 5.000000000000004441, 0.7853981633974587151 ) ;
#36345 = ORIENTED_EDGE ( 'NONE', *, *, #11612, .F. ) ;
#36346 = CARTESIAN_POINT ( 'NONE',  ( -151.2549999999999955, -4.716976649647092401, 6.492361379858946790 ) ) ;
#36347 = MECHANICAL_DESIGN_GEOMETRIC_PRESENTATION_REPRESENTATION (  '', ( #18342 ), #59894 ) ;
#36348 = EDGE_CURVE ( 'NONE', #11645, #28799, #1430, .T. ) ;
#36349 = ORIENTED_EDGE ( 'NONE', *, *, #14593, .T. ) ;
#36350 = AXIS2_PLACEMENT_3D ( 'NONE', #27228, #64884, #59245 ) ;
#36351 = CARTESIAN_POINT ( 'NONE',  ( -21.02379604162863913, 110.4999999999999858, 10.50000000000000000 ) ) ;
#36352 = DIRECTION ( 'NONE',  ( 0.000000000000000000, 1.000000000000000000, 1.224646799147353207E-16 ) ) ;
#36354 = ORIENTED_EDGE ( 'NONE', *, *, #61433, .T. ) ;
#36353 = EDGE_CURVE ( 'NONE', #31691, #28799, #16553, .T. ) ;
#36355 = CARTESIAN_POINT ( 'NONE',  ( 22.99999999999998224, 0.000000000000000000, 72.00402776293825013 ) ) ;
#36356 = EDGE_CURVE ( 'NONE', #3561, #11185, #35185, .T. ) ;
#36357 = FACE_OUTER_BOUND ( 'NONE', #31661, .T. ) ;
#36358 = CARTESIAN_POINT ( 'NONE',  ( 3.094860106618435136, 118.2949999999999875, -9.525000000000000355 ) ) ;
#36359 = CONICAL_SURFACE ( 'NONE', #68864, 22.49999999999999645, 0.7853981633974239651 ) ;
#36360 = ORIENTED_EDGE ( 'NONE', *, *, #50771, .T. ) ;
#36361 = DIRECTION ( 'NONE',  ( 0.000000000000000000, -1.000000000000000000, 0.000000000000000000 ) ) ;
#36363 = EDGE_CURVE ( 'NONE', #27627, #31626, #11579, .T. ) ;
#36362 = CARTESIAN_POINT ( 'NONE',  ( 8.102448949553181734, 122.1049999999999898, -5.886773742842746238 ) ) ;
#36364 = CARTESIAN_POINT ( 'NONE',  ( -74.30499999999997840, 8.437984349512086979, -1.550032578732815448E-15 ) ) ;
#36365 = CARTESIAN_POINT ( 'NONE',  ( -80.45707362346617231, -9.058813317711329915, 2.943386871421371787 ) ) ;
#36366 = ORIENTED_EDGE ( 'NONE', *, *, #13098, .T. ) ;
#36367 = CARTESIAN_POINT ( 'NONE',  ( 9.058813317711338797, 142.9550000000000125, -2.943386871421372675 ) ) ;
#36368 = UNCERTAINTY_MEASURE_WITH_UNIT (LENGTH_MEASURE( 1.000000000000000082E-05 ), #45424, 'distance_accuracy_value', 'NONE');
#36369 = DIRECTION ( 'NONE',  ( 1.000000000000000000, 0.000000000000000000, 0.000000000000000000 ) ) ;
#36370 = CARTESIAN_POINT ( 'NONE',  ( -4.500000000000002665, 24.99999999999998579, 3.750000000000000000 ) ) ;
#36371 = CARTESIAN_POINT ( 'NONE',  ( 27.00000000000001776, 42.00000000000000000, 36.50000000000000000 ) ) ;
#36372 = ORIENTED_EDGE ( 'NONE', *, *, #26144, .F. ) ;
#36373 = VECTOR ( 'NONE', #41047, 1000.000000000000000 ) ;
#36374 = AXIS2_PLACEMENT_3D ( 'NONE', #13022, #6105, #19330 ) ;
#36375 = CYLINDRICAL_SURFACE ( 'NONE', #14269, 1.000000000000000888 ) ;
#36376 =( NAMED_UNIT ( * ) PLANE_ANGLE_UNIT ( ) SI_UNIT ( $, .RADIAN. ) );
#36377 = FACE_OUTER_BOUND ( 'NONE', #37500, .T. ) ;
#36378 = CARTESIAN_POINT ( 'NONE',  ( -47.39499999999998181, -6.826472737025115478, -4.959722759717899443 ) ) ;
#36379 = VERTEX_POINT ( 'NONE', #32682 ) ;
#36380 = CARTESIAN_POINT ( 'NONE',  ( 5.237322049151770464, 111.7848139822559972, -6.367445604021527039 ) ) ;
#36381 = AXIS2_PLACEMENT_3D ( 'NONE', #48668, #15951, #55633 ) ;
#36382 = FILL_AREA_STYLE ('',( #31378 ) ) ;
#36383 = SURFACE_STYLE_USAGE ( .BOTH. , #21540 ) ;
#36384 = ORIENTED_EDGE ( 'NONE', *, *, #40363, .T. ) ;
#36385 = PLANE ( 'NONE',  #61261 ) ;
#36386 = CARTESIAN_POINT ( 'NONE',  ( 66.74999999999998579, 36.75000000000000000, 3.750000000000000000 ) ) ;
#36387 = ORIENTED_EDGE ( 'NONE', *, *, #68811, .F. ) ;
#36388 = DIRECTION ( 'NONE',  ( 0.000000000000000000, 0.000000000000000000, 1.000000000000000000 ) ) ;
#36389 = SURFACE_STYLE_FILL_AREA ( #40246 ) ;
#36390 = CARTESIAN_POINT ( 'NONE',  ( -97.70499999999998408, 2.607480562269073321, 8.024999999999991473 ) ) ;
#36392 = ORIENTED_EDGE ( 'NONE', *, *, #27840, .F. ) ;
#36391 = CIRCLE ( 'NONE', #18376, 5.500000000000005329 ) ;
#36393 = CARTESIAN_POINT ( 'NONE',  ( 27.99999999999998224, 5.000000000000000000, 72.00402776293822171 ) ) ;
#36394 = DIRECTION ( 'NONE',  ( 0.000000000000000000, 0.000000000000000000, -1.000000000000000000 ) ) ;
#36395 = CARTESIAN_POINT ( 'NONE',  ( -129.8070736234661240, 10.01517768586948698, -1.839758294383808571E-15 ) ) ;
#36396 = CIRCLE ( 'NONE', #23984, 0.4999999999999991118 ) ;
#36397 = SURFACE_STYLE_USAGE ( .BOTH. , #4296 ) ;
#36398 = CARTESIAN_POINT ( 'NONE',  ( 5.598654528085805993, 153.2450000000000045, 7.705886871421374629 ) ) ;
#36399 = CARTESIAN_POINT ( 'NONE',  ( -74.00707362346615525, -8.102448949553172852, -5.886773742842741797 ) ) ;
#36400 = AXIS2_PLACEMENT_3D ( 'NONE', #61816, #41456, #68177 ) ;
#36401 = CARTESIAN_POINT ( 'NONE',  ( -92.39292637653379359, 8.102448949553176405, 5.886773742842740909 ) ) ;
#36402 = AXIS2_PLACEMENT_3D ( 'NONE', #49898, #17551, #1642 ) ;
#36403 = ORIENTED_EDGE ( 'NONE', *, *, #12347, .T. ) ;
#36404 = DIRECTION ( 'NONE',  ( 0.000000000000000000, 0.000000000000000000, -1.000000000000000000 ) ) ;
#36405 = CARTESIAN_POINT ( 'NONE',  ( -15.32976068146453485, -10.90871211463571555, -4.999999999999998224 ) ) ;
#36406 = FILL_AREA_STYLE ('',( #69074 ) ) ;
#36407 = CIRCLE ( 'NONE', #6012, 12.50000000000001066 ) ;
#36408 = AXIS2_PLACEMENT_3D ( 'NONE', #65701, #35074, #47415 ) ;
#36409 = CARTESIAN_POINT ( 'NONE',  ( -107.4549999999999983, 7.632228543268599452, -2.479861379858951942 ) ) ;
#36410 = CARTESIAN_POINT ( 'NONE',  ( 8.102448949553181734, 123.3949999999999676, 5.886773742842750679 ) ) ;
#36411 = CARTESIAN_POINT ( 'NONE',  ( -128.0949999999999704, -2.607480562269071545, -8.024999999999991473 ) ) ;
#36412 = CARTESIAN_POINT ( 'NONE',  ( -112.5570736234661808, -1.166476076187852838E-15, -9.524999999999991473 ) ) ;
#36413 = SURFACE_STYLE_USAGE ( .BOTH. , #3984 ) ;
#36414 = AXIS2_PLACEMENT_3D ( 'NONE', #55809, #28002, #49512 ) ;
#36415 = CYLINDRICAL_SURFACE ( 'NONE', #49242, 0.2500000000000002220 ) ;
#36416 = AXIS2_PLACEMENT_3D ( 'NONE', #60334, #1184, #49804 ) ;
#36417 = ORIENTED_EDGE ( 'NONE', *, *, #18298, .F. ) ;
#36418 = CARTESIAN_POINT ( 'NONE',  ( -87.50000000000000000, -7.499999999999990230, 24.00000000000000000 ) ) ;
#36419 = CARTESIAN_POINT ( 'NONE',  ( -160.3429263765337964, -9.058813317711329915, 2.943386871421371787 ) ) ;
#36420 = CARTESIAN_POINT ( 'NONE',  ( 8.920833891111504599, -2.548662454712529613, 0.2685431138779699189 ) ) ;
#36421 =( GEOMETRIC_REPRESENTATION_CONTEXT ( 3 ) GLOBAL_UNCERTAINTY_ASSIGNED_CONTEXT ( ( #37633 ) ) GLOBAL_UNIT_ASSIGNED_CONTEXT ( ( #17828, #16810, #39307 ) ) REPRESENTATION_CONTEXT ( 'NONE', 'WORKASPACE' ) );
#36422 = CARTESIAN_POINT ( 'NONE',  ( -44.99154893936434263, 9.591540374752314690, -3.105018539189321913 ) ) ;
#36423 = ADVANCED_FACE ( 'NONE', ( #28068 ), #6298, .T. ) ;
#36424 = AXIS2_PLACEMENT_3D ( 'NONE', #584, #17212, #22109 ) ;
#36425 = FACE_OUTER_BOUND ( 'NONE', #24960, .T. ) ;
#36426 = DIRECTION ( 'NONE',  ( -0.6216216216216311485, -0.7833176619561784682, 0.000000000000000000 ) ) ;
#36427 = DIRECTION ( 'NONE',  ( 0.000000000000000000, 1.000000000000000000, -0.000000000000000000 ) ) ;
#36428 = ORIENTED_EDGE ( 'NONE', *, *, #40101, .T. ) ;
#36429 = CARTESIAN_POINT ( 'NONE',  ( -85.79292637653378506, -3.094860106618429807, 9.524999999999991473 ) ) ;
#36430 = ADVANCED_FACE ( 'NONE', ( #16208 ), #59769, .T. ) ;
#36431 = CARTESIAN_POINT ( 'NONE',  ( -166.0429263765338135, -9.058813317711329915, -2.943386871421370898 ) ) ;
#36432 = MECHANICAL_DESIGN_GEOMETRIC_PRESENTATION_REPRESENTATION (  '', ( #17339 ), #27354 ) ;
#36433 = DIRECTION ( 'NONE',  ( 1.000000000000000000, 0.000000000000000000, 0.000000000000000000 ) ) ;
#36434 = FILL_AREA_STYLE_COLOUR ( '', #30339 ) ;
#36435 =( NAMED_UNIT ( * ) SI_UNIT ( $, .STERADIAN. ) SOLID_ANGLE_UNIT ( ) );
#36436 = CARTESIAN_POINT ( 'NONE',  ( -99.44292637653380496, -1.166476076187852838E-15, -9.524999999999991473 ) ) ;
#36437 = CONICAL_SURFACE ( 'NONE', #38687, 5.000000000000004441, 0.7853981633974587151 ) ;
#36438 = ORIENTED_EDGE ( 'NONE', *, *, #37788, .T. ) ;
#36439 = CARTESIAN_POINT ( 'NONE',  ( 5.185928986913072691, 5.017707510222363609, 0.2088670156639309550 ) ) ;
#36440 = EDGE_CURVE ( 'NONE', #69284, #68902, #64362, .T. ) ;
#36441 = CARTESIAN_POINT ( 'NONE',  ( 71.49999999999998579, 99.99999999999998579, -7.000000000000000000 ) ) ;
#36442 = ORIENTED_EDGE ( 'NONE', *, *, #9246, .T. ) ;
#36443 = CARTESIAN_POINT ( 'NONE',  ( 6.020204320972966094, -1.861307952554195122, 7.572700244129132230 ) ) ;
#36444 = VECTOR ( 'NONE', #7601, 1000.000000000000000 ) ;
#36445 = CARTESIAN_POINT ( 'NONE',  ( -8.437984349512095861, 136.8070736234661808, -5.166775262442723748E-16 ) ) ;
#36446 = CARTESIAN_POINT ( 'NONE',  ( 25.00000000000000355, 36.75000000000000000, -3.750000000000000000 ) ) ;
#36447 = ORIENTED_EDGE ( 'NONE', *, *, #15041, .T. ) ;
#36449 = ADVANCED_FACE ( 'NONE', ( #22142 ), #49231, .F. ) ;
#36448 = CARTESIAN_POINT ( 'NONE',  ( -102.0570736234661808, 0.000000000000000000, 9.524999999999991473 ) ) ;
#36450 = CARTESIAN_POINT ( 'NONE',  ( -99.20499999999998408, -2.607480562269071545, -8.024999999999991473 ) ) ;
#36451 = UNCERTAINTY_MEASURE_WITH_UNIT (LENGTH_MEASURE( 1.000000000000000082E-05 ), #48361, 'distance_accuracy_value', 'NONE');
#36452 = FILL_AREA_STYLE_COLOUR ( '', #58927 ) ;
#36453 = ORIENTED_EDGE ( 'NONE', *, *, #24318, .F. ) ;
#36454 = MECHANICAL_DESIGN_GEOMETRIC_PRESENTATION_REPRESENTATION (  '', ( #57753 ), #11697 ) ;
#36455 = CARTESIAN_POINT ( 'NONE',  ( 6.826472737025121695, 143.4929263765338305, -4.959722759717905660 ) ) ;
#36456 = EDGE_LOOP ( 'NONE', ( #16049, #8051, #59153, #15376 ) ) ;
#36457 = CIRCLE ( 'NONE', #6075, 0.2500000000000002220 ) ;
#36458 = CARTESIAN_POINT ( 'NONE',  ( -74.99499999999999034, -6.826472737025115478, 4.959722759717900331 ) ) ;
#36459 = ORIENTED_EDGE ( 'NONE', *, *, #29248, .T. ) ;
#36460 =( GEOMETRIC_REPRESENTATION_CONTEXT ( 3 ) GLOBAL_UNCERTAINTY_ASSIGNED_CONTEXT ( ( #34239 ) ) GLOBAL_UNIT_ASSIGNED_CONTEXT ( ( #24472, #13942, #51937 ) ) REPRESENTATION_CONTEXT ( 'NONE', 'WORKASPACE' ) );
#36461 =( NAMED_UNIT ( * ) PLANE_ANGLE_UNIT ( ) SI_UNIT ( $, .RADIAN. ) );
#36462 = ORIENTED_EDGE ( 'NONE', *, *, #66292, .T. ) ;
#36463 = CARTESIAN_POINT ( 'NONE',  ( 4.041451884327377897, 1.417096231345241319, 7.000000000000000888 ) ) ;
#36465 = CYLINDRICAL_SURFACE ( 'NONE', #46053, 0.2500000000000002220 ) ;
#36464 = CIRCLE ( 'NONE', #11710, 10.00000000000000000 ) ;
#36466 = FILL_AREA_STYLE_COLOUR ( '', #4249 ) ;
#36467 = ORIENTED_EDGE ( 'NONE', *, *, #64613, .T. ) ;
#36468 = FACE_OUTER_BOUND ( 'NONE', #63641, .T. ) ;
#36469 = VERTEX_POINT ( 'NONE', #48573 ) ;
#36470 = DIRECTION ( 'NONE',  ( -1.000000000000000000, -0.000000000000000000, -0.000000000000000000 ) ) ;
#36471 = DIRECTION ( 'NONE',  ( 1.000000000000000000, 0.000000000000000000, -1.300977106640434891E-16 ) ) ;
#36472 = CONICAL_SURFACE ( 'NONE', #21823, 6.999999999999997335, 0.7853981633974500554 ) ;
#36473 = MECHANICAL_DESIGN_GEOMETRIC_PRESENTATION_REPRESENTATION (  '', ( #3803 ), #38677 ) ;
#36474 = CARTESIAN_POINT ( 'NONE',  ( -170.6070736234661638, -8.102448949553172852, 5.886773742842742685 ) ) ;
#36475 = CARTESIAN_POINT ( 'NONE',  ( 3.094860106618435136, 127.2949999999999875, -9.525000000000000355 ) ) ;
#36476 = CARTESIAN_POINT ( 'NONE',  ( -100.8570736234661780, -5.598654528085803328, -7.705886871421366635 ) ) ;
#36477 = ADVANCED_FACE ( 'NONE', ( #43639 ), #16891, .F. ) ;
#36478 = DIRECTION ( 'NONE',  ( 0.000000000000000000, 0.000000000000000000, -1.000000000000000000 ) ) ;
#36479 = CARTESIAN_POINT ( 'NONE',  ( -64.55707362346618083, -1.166476076187852838E-15, -9.524999999999991473 ) ) ;
#36480 = ORIENTED_EDGE ( 'NONE', *, *, #63216, .F. ) ;
#36481 = SURFACE_STYLE_FILL_AREA ( #9727 ) ;
#36483 = CARTESIAN_POINT ( 'NONE',  ( -114.8070736234661808, 10.01517768586948698, -1.839758294383808966E-15 ) ) ;
#36482 = DIRECTION ( 'NONE',  ( -0.000000000000000000, -0.000000000000000000, -1.000000000000000000 ) ) ;
#36484 =( LENGTH_UNIT ( ) NAMED_UNIT ( * ) SI_UNIT ( .MILLI., .METRE. ) );
#36485 = CARTESIAN_POINT ( 'NONE',  ( -140.1550000000000011, 7.632228543268600340, 2.479861379858949277 ) ) ;
#36486 = CARTESIAN_POINT ( 'NONE',  ( -75.00000000000000000, 9.708372675170620525, 6.000000000000000888 ) ) ;
#36487 = CARTESIAN_POINT ( 'NONE',  ( 4.000000000000001776, 34.36176364315826248, -80.00402776293826435 ) ) ;
#36488 = CARTESIAN_POINT ( 'NONE',  ( -152.8449999999999989, -7.632228543268599452, 2.479861379858951054 ) ) ;
#36489 = CARTESIAN_POINT ( 'NONE',  ( -148.0449999999999875, 7.632228543268600340, 2.479861379858949277 ) ) ;
#36490 =( BOUNDED_CURVE ( )  B_SPLINE_CURVE ( 2, ( #12531, #51231, #12890, #33997, #67398, #66008, #23116, #28348, #18844, #2977, #45971 ),
 .UNSPECIFIED., .F., .F. ) 
 B_SPLINE_CURVE_WITH_KNOTS ( ( 3, 2, 2, 2, 2, 3 ),
 ( 0.2058823529411763498, 0.2117647058823528272, 0.2176470588235293047, 0.2235294117647058099, 0.2294117647058822596, 0.2352941176470587370 ),
 .UNSPECIFIED. ) 
 CURVE ( )  GEOMETRIC_REPRESENTATION_ITEM ( )  RATIONAL_B_SPLINE_CURVE ( ( 1.000000000000000888, 0.9510565162951526430, 1.000000000000000000, 0.9510565162951535312, 1.000000000000000000, 0.9510565162951535312, 1.000000000000000000, 0.9510565162951535312, 1.000000000000000000, 0.9510565162951541973, 0.9999999999999993339 ) ) 
 REPRESENTATION_ITEM ( '' )  );
#36491 = ORIENTED_EDGE ( 'NONE', *, *, #61075, .F. ) ;
#36492 = AXIS2_PLACEMENT_3D ( 'NONE', #14440, #46153, #35577 ) ;
#36493 = CARTESIAN_POINT ( 'NONE',  ( -180.8070736234661524, 10.01517768586948698, -1.839758294383808966E-15 ) ) ;
#36494 = CARTESIAN_POINT ( 'NONE',  ( -79.99999999999998579, 50.00000000000000000, -12.00000000000000000 ) ) ;
#36495 = CARTESIAN_POINT ( 'NONE',  ( -75.50000000000000000, 64.49137674618943095, 9.500000000000001776 ) ) ;
#36496 = AXIS2_PLACEMENT_3D ( 'NONE', #14379, #36225, #42547 ) ;
#36497 = CARTESIAN_POINT ( 'NONE',  ( -63.20499999999998408, -2.607480562269071545, -8.024999999999991473 ) ) ;
#36498 = LINE ( 'NONE', #29787, #44983 ) ;
#36499 = EDGE_CURVE ( 'NONE', #30149, #13760, #67832, .T. ) ;
#36500 = AXIS2_PLACEMENT_3D ( 'NONE', #46107, #51013, #13021 ) ;
#36501 = CARTESIAN_POINT ( 'NONE',  ( -65.09499999999998465, -2.607480562269071545, -8.024999999999991473 ) ) ;
#36502 = ADVANCED_FACE ( 'NONE', ( #35114 ), #49862, .T. ) ;
#36503 = CARTESIAN_POINT ( 'NONE',  ( 0.000000000000000000, 152.5550000000000068, -9.525000000000000355 ) ) ;
#36504 = DIRECTION ( 'NONE',  ( 0.000000000000000000, 0.000000000000000000, 1.000000000000000000 ) ) ;
#36505 = SURFACE_STYLE_FILL_AREA ( #69171 ) ;
#36506 = CIRCLE ( 'NONE', #39866, 4.999999999999997335 ) ;
#36507 = CARTESIAN_POINT ( 'NONE',  ( -151.9429263765338192, 0.000000000000000000, 9.524999999999991473 ) ) ;
#36508 = TOROIDAL_SURFACE ( 'NONE', #24104, 0.5000000000000000000, 0.2500000000000000000 ) ;
#36509 = EDGE_CURVE ( 'NONE', #35442, #38534, #47659, .T. ) ;
#36510 = CARTESIAN_POINT ( 'NONE',  ( 86.21825843581756033, 0.000000000000000000, 39.83014742847163348 ) ) ;
#36511 = DIRECTION ( 'NONE',  ( 1.000000000000000000, -0.000000000000000000, -1.300977106640434891E-16 ) ) ;
#36512 = DIRECTION ( 'NONE',  ( 0.000000000000000000, 0.000000000000000000, 1.000000000000000000 ) ) ;
#36513 = CARTESIAN_POINT ( 'NONE',  ( -74.99999999999998579, 50.00000000000000000, -7.000000000000000000 ) ) ;
#36514 = FACE_OUTER_BOUND ( 'NONE', #34057, .T. ) ;
#36515 = EDGE_CURVE ( 'NONE', #12616, #44582, #36396, .T. ) ;
#36516 = DIRECTION ( 'NONE',  ( 1.000000000000000000, -0.000000000000000000, -0.000000000000000000 ) ) ;
#36517 = ORIENTED_EDGE ( 'NONE', *, *, #2748, .F. ) ;
#36519 = EDGE_LOOP ( 'NONE', ( #39451, #47916, #58438, #62937 ) ) ;
#36518 =( GEOMETRIC_REPRESENTATION_CONTEXT ( 3 ) GLOBAL_UNCERTAINTY_ASSIGNED_CONTEXT ( ( #41763 ) ) GLOBAL_UNIT_ASSIGNED_CONTEXT ( ( #18974, #12403, #20022 ) ) REPRESENTATION_CONTEXT ( 'NONE', 'WORKASPACE' ) );
#36520 =( GEOMETRIC_REPRESENTATION_CONTEXT ( 3 ) GLOBAL_UNCERTAINTY_ASSIGNED_CONTEXT ( ( #28372 ) ) GLOBAL_UNIT_ASSIGNED_CONTEXT ( ( #52259, #8635, #51531 ) ) REPRESENTATION_CONTEXT ( 'NONE', 'WORKASPACE' ) );
#36521 = PRESENTATION_STYLE_ASSIGNMENT (( #15047 ) ) ;
#36522 = CARTESIAN_POINT ( 'NONE',  ( 3.000000000000030198, 43.00000000000000000, 79.00402776293826435 ) ) ;
#36524 = EDGE_CURVE ( 'NONE', #44927, #4250, #62413, .T. ) ;
#36523 = CARTESIAN_POINT ( 'NONE',  ( -195.0000000000000000, 1.166476076187852838E-15, -9.524999999999991473 ) ) ;
#36525 = FILL_AREA_STYLE_COLOUR ( '', #3554 ) ;
#36526 = CIRCLE ( 'NONE', #6153, 0.2500000000000002220 ) ;
#36527 = CARTESIAN_POINT ( 'NONE',  ( -77.45707362346617231, -9.058813317711329915, 2.943386871421371787 ) ) ;
#36528 = ORIENTED_EDGE ( 'NONE', *, *, #63368, .T. ) ;
#36529 = ORIENTED_EDGE ( 'NONE', *, *, #61769, .F. ) ;
#36530 = LINE ( 'NONE', #57952, #2835 ) ;
#36531 = DIRECTION ( 'NONE',  ( 0.000000000000000000, -1.000000000000000000, 0.000000000000000000 ) ) ;
#36532 = AXIS2_PLACEMENT_3D ( 'NONE', #45927, #19504, #35703 ) ;
#36533 = CARTESIAN_POINT ( 'NONE',  ( -17.75000000000000711, 31.24999999999999289, 3.750000000000000000 ) ) ;
#36534 = ORIENTED_EDGE ( 'NONE', *, *, #19378, .T. ) ;
#36535 = CARTESIAN_POINT ( 'NONE',  ( 5.598654528085805993, 118.3549999999999898, 7.705886871421374629 ) ) ;
#36536 = CARTESIAN_POINT ( 'NONE',  ( 27.99999999999999645, 0.000000000000000000, -72.00402776293822171 ) ) ;
#36537 = CARTESIAN_POINT ( 'NONE',  ( 45.00000000000000000, 9.639620389971920389, 6.999999999999999112 ) ) ;
#36538 = COLOUR_RGB ( '', 0.40784314, 0.44705882, 0.49803922) ;
#36539 = AXIS2_PLACEMENT_3D ( 'NONE', #12745, #66207, #39176 ) ;
#36540 = LINE ( 'NONE', #63892, #65352 ) ;
#36541 = CARTESIAN_POINT ( 'NONE',  ( -100.9449999999999932, -9.827790563157499189E-16, -8.024999999999991473 ) ) ;
#36542 = ORIENTED_EDGE ( 'NONE', *, *, #16409, .T. ) ;
#36543 = AXIS2_PLACEMENT_3D ( 'NONE', #57419, #9247, #30666 ) ;
#36544 = CARTESIAN_POINT ( 'NONE',  ( -9.451804584015965460, 110.5000000000000426, 1.257324542065831441 ) ) ;
#36545 = SURFACE_STYLE_USAGE ( .BOTH. , #21336 ) ;
#36546 = CONICAL_SURFACE ( 'NONE', #64575, 9.000000000000000000, 0.7853981633974500554 ) ;
#36547 = EDGE_LOOP ( 'NONE', ( #69016, #53693, #44482 ) ) ;
#36548 = CARTESIAN_POINT ( 'NONE',  ( -6.826472737025120807, 156.9929263765338305, 4.959722759717906548 ) ) ;
#36549 = SURFACE_STYLE_FILL_AREA ( #53698 ) ;
#36550 = CYLINDRICAL_SURFACE ( 'NONE', #64342, 9.524999999999991473 ) ;
#36551 = FACE_OUTER_BOUND ( 'NONE', #41210, .T. ) ;
#36552 = ORIENTED_EDGE ( 'NONE', *, *, #12714, .F. ) ;
#36553 = CARTESIAN_POINT ( 'NONE',  ( 20.68718488045382742, 114.6829008731431543, -10.00000000000011724 ) ) ;
#36554 = EDGE_LOOP ( 'NONE', ( #45957, #28335, #40924, #20133 ) ) ;
#36555 = SURFACE_SIDE_STYLE ('',( #26279 ) ) ;
#36556 = DIRECTION ( 'NONE',  ( 0.000000000000000000, 0.000000000000000000, -1.000000000000000000 ) ) ;
#36557 = CARTESIAN_POINT ( 'NONE',  ( -141.4429263765337907, -1.166476076187852838E-15, -9.524999999999991473 ) ) ;
#36558 = DIRECTION ( 'NONE',  ( 0.000000000000000000, -1.000000000000000000, -0.000000000000000000 ) ) ;
#36559 = LINE ( 'NONE', #30510, #35005 ) ;
#36560 =( NAMED_UNIT ( * ) SI_UNIT ( $, .STERADIAN. ) SOLID_ANGLE_UNIT ( ) );
#36561 = ADVANCED_FACE ( 'NONE', ( #24534 ), #60786, .F. ) ;
#36562 = PRESENTATION_LAYER_ASSIGNMENT (  '', '', ( #5066 ) ) ;
#36563 = CARTESIAN_POINT ( 'NONE',  ( -74.99999999999998579, 50.00000000000000000, 9.500000000000000000 ) ) ;
#36564 = DIRECTION ( 'NONE',  ( 0.000000000000000000, 0.6449798928094537809, 0.7641995406119435064 ) ) ;
#36565 = CARTESIAN_POINT ( 'NONE',  ( -5.603096392576912166, 8.295152368350910521, 0.9853608755428879817 ) ) ;
#36566 = CARTESIAN_POINT ( 'NONE',  ( 7.999999999999992895, 5.000000000000000000, 24.00402776293826079 ) ) ;
#36567 = EDGE_LOOP ( 'NONE', ( #9048, #54218 ) ) ;
#36568 = EDGE_LOOP ( 'NONE', ( #38348, #45396, #28487, #67539 ) ) ;
#36569 = FILL_AREA_STYLE ('',( #63923 ) ) ;
#36570 = CYLINDRICAL_SURFACE ( 'NONE', #24206, 1.000000000000000000 ) ;
#36571 = DIRECTION ( 'NONE',  ( 0.000000000000000000, 0.000000000000000000, 1.000000000000000000 ) ) ;
#36573 = SURFACE_SIDE_STYLE ('',( #15100 ) ) ;
#36572 = VECTOR ( 'NONE', #12631, 1000.000000000000000 ) ;
#36574 = VERTEX_POINT ( 'NONE', #34075 ) ;
#36575 = CARTESIAN_POINT ( 'NONE',  ( 3.000000000000030198, 42.58578643762690064, 89.58578643762690774 ) ) ;
#36576 = CARTESIAN_POINT ( 'NONE',  ( -178.1049999999999329, -6.826472737025115478, 4.959722759717900331 ) ) ;
#36577 = CARTESIAN_POINT ( 'NONE',  ( -8.920833891111501046, 2.231456886122024752, 2.548662454712524283 ) ) ;
#36578 = CARTESIAN_POINT ( 'NONE',  ( 25.00000000000001421, 42.00000000000000000, 0.000000000000000000 ) ) ;
#36579 = CARTESIAN_POINT ( 'NONE',  ( -179.8449999999999989, -7.632228543268599452, 2.479861379858951054 ) ) ;
#36580 =( GEOMETRIC_REPRESENTATION_CONTEXT ( 3 ) GLOBAL_UNCERTAINTY_ASSIGNED_CONTEXT ( ( #11436 ) ) GLOBAL_UNIT_ASSIGNED_CONTEXT ( ( #1647, #60088, #11550 ) ) REPRESENTATION_CONTEXT ( 'NONE', 'WORKASPACE' ) );
#36581 = CARTESIAN_POINT ( 'NONE',  ( -178.0450000000000159, 7.632228543268600340, 2.479861379858949277 ) ) ;
#36582 = EDGE_LOOP ( 'NONE', ( #45841, #39361, #2100, #41972 ) ) ;
#36583 = SURFACE_SIDE_STYLE ('',( #57283 ) ) ;
#36584 = EDGE_CURVE ( 'NONE', #30410, #57684, #59926, .T. ) ;
#36585 = CARTESIAN_POINT ( 'NONE',  ( 57.49999999999999289, 28.24999999999998934, -3.750000000000000000 ) ) ;
#36586 = CARTESIAN_POINT ( 'NONE',  ( -53.78504481823340200, -9.584004935223168431, -3.223153552129623733 ) ) ;
#36587 = CARTESIAN_POINT ( 'NONE',  ( -97.25499999999999545, -4.716976649647092401, 6.492361379858946790 ) ) ;
#36588 = CARTESIAN_POINT ( 'NONE',  ( 9.189246016727048882, 154.4999999999999432, 2.545277832678562557 ) ) ;
#36589 = CARTESIAN_POINT ( 'NONE',  ( 0.000000000000000000, -2.500000000000000000, 0.000000000000000000 ) ) ;
#36590 = CARTESIAN_POINT ( 'NONE',  ( -75.41277076832422210, 36.04285368632835684, -9.691745530926853647 ) ) ;
#36591 = EDGE_CURVE ( 'NONE', #12165, #4746, #42023, .T. ) ;
#36592 = CIRCLE ( 'NONE', #53420, 3.499999999999997780 ) ;
#36593 = CARTESIAN_POINT ( 'NONE',  ( -88.94499999999997897, -9.827790563157499189E-16, -8.024999999999991473 ) ) ;
#36594 = EDGE_CURVE ( 'NONE', #11684, #44405, #24204, .T. ) ;
#36595 = CARTESIAN_POINT ( 'NONE',  ( -8.102448949553181734, 126.6050000000000040, 5.886773742842747126 ) ) ;
#36596 = CARTESIAN_POINT ( 'NONE',  ( -68.99499999999999034, -6.826472737025115478, 4.959722759717900331 ) ) ;
#36597 = CARTESIAN_POINT ( 'NONE',  ( 23.50000000000001776, 43.00000000000000000, -28.18999999999999773 ) ) ;
#36598 = AXIS2_PLACEMENT_3D ( 'NONE', #23947, #44430, #45107 ) ;
#36599 = CARTESIAN_POINT ( 'NONE',  ( 2.418535808707046542, -7.000000000000002665, 0.3989014552058374741 ) ) ;
#36600 = DIRECTION ( 'NONE',  ( -1.000000000000000000, -0.000000000000000000, -0.000000000000000000 ) ) ;
#36601 = AXIS2_PLACEMENT_3D ( 'NONE', #14786, #36264, #57689 ) ;
#36602 =( BOUNDED_CURVE ( )  B_SPLINE_CURVE ( 2, ( #26234, #49122, #59624, #17107, #27248, #6169, #38581, #10762, #63865, #32212, #58952 ),
 .UNSPECIFIED., .F., .F. ) 
 B_SPLINE_CURVE_WITH_KNOTS ( ( 3, 2, 2, 2, 2, 3 ),
 ( 0.3260869565217314192, 0.3282608695652096120, 0.3304347826086878048, 0.3326086956521661087, 0.3347826086956443015, 0.3369565217391224943 ),
 .UNSPECIFIED. ) 
 CURVE ( )  GEOMETRIC_REPRESENTATION_ITEM ( )  RATIONAL_B_SPLINE_CURVE ( ( 1.000000000000173639, 0.9510565162949797813, 1.000000000000000000, 0.9510565162951535312, 1.000000000000000000, 0.9510565162951535312, 1.000000000000000000, 0.9510565162951535312, 1.000000000000000000, 0.9510565162953322771, 0.9999999999998212541 ) ) 
 REPRESENTATION_ITEM ( '' )  );
#36603 = DIRECTION ( 'NONE',  ( 1.000000000000000000, -6.938893903907222067E-15, 0.000000000000000000 ) ) ;
#36604 = ORIENTED_EDGE ( 'NONE', *, *, #64087, .F. ) ;
#36605 = EDGE_CURVE ( 'NONE', #22912, #28559, #45712, .T. ) ;
#36606 =( GEOMETRIC_REPRESENTATION_CONTEXT ( 3 ) GLOBAL_UNCERTAINTY_ASSIGNED_CONTEXT ( ( #31367 ) ) GLOBAL_UNIT_ASSIGNED_CONTEXT ( ( #59264, #38224, #26235 ) ) REPRESENTATION_CONTEXT ( 'NONE', 'WORKASPACE' ) );
#36607 = CARTESIAN_POINT ( 'NONE',  ( -132.4449999999999932, 0.000000000000000000, 8.024999999999991473 ) ) ;
#36608 = CARTESIAN_POINT ( 'NONE',  ( 23.21231517720797655, 117.4999999999999716, -7.000000000000000000 ) ) ;
#36609 = ADVANCED_FACE ( 'NONE', ( #23862 ), #15032, .F. ) ;
#36610 = CARTESIAN_POINT ( 'NONE',  ( 68.99999999999998579, 1.000000000000008438, -3.000000000000000000 ) ) ;
#36612 = PRESENTATION_STYLE_ASSIGNMENT (( #51699 ) ) ;
#36611 = DIRECTION ( 'NONE',  ( -1.000000000000000000, 0.000000000000000000, 0.000000000000000000 ) ) ;
#36613 = DIRECTION ( 'NONE',  ( -1.000000000000000000, -3.469446951953610639E-15, -0.000000000000000000 ) ) ;
#36614 = ORIENTED_EDGE ( 'NONE', *, *, #67686, .T. ) ;
#36615 = ORIENTED_EDGE ( 'NONE', *, *, #3838, .T. ) ;
#36616 = DIRECTION ( 'NONE',  ( 0.000000000000000000, 1.000000000000000000, 0.000000000000000000 ) ) ;
#36617 = DIRECTION ( 'NONE',  ( 0.000000000000000000, 0.000000000000000000, -1.000000000000000000 ) ) ;
#36618 = CARTESIAN_POINT ( 'NONE',  ( 24.00000000000000000, 0.000000000000000000, 3.000000000000000000 ) ) ;
#36619 = VERTEX_POINT ( 'NONE', #63910 ) ;
#36620 = CARTESIAN_POINT ( 'NONE',  ( -118.2549999999999812, -4.716976649647092401, 6.492361379858946790 ) ) ;
#36621 = ORIENTED_EDGE ( 'NONE', *, *, #38732, .F. ) ;
#36622 = DIRECTION ( 'NONE',  ( -0.000000000000000000, -0.000000000000000000, 1.000000000000000000 ) ) ;
#36623 = DIRECTION ( 'NONE',  ( -1.000000000000000000, -0.000000000000000000, -0.000000000000000000 ) ) ;
#36624 = ORIENTED_EDGE ( 'NONE', *, *, #19817, .T. ) ;
#36625 = CARTESIAN_POINT ( 'NONE',  ( -71.50000000000000000, 14.49137674618942562, 7.000000000000000000 ) ) ;
#36626 =( LENGTH_UNIT ( ) NAMED_UNIT ( * ) SI_UNIT ( .MILLI., .METRE. ) );
#36627 = ORIENTED_EDGE ( 'NONE', *, *, #57435, .F. ) ;
#36628 = AXIS2_PLACEMENT_3D ( 'NONE', #54063, #22766, #38289 ) ;
#36629 = EDGE_CURVE ( 'NONE', #43704, #46026, #3399, .T. ) ;
#36630 = CARTESIAN_POINT ( 'NONE',  ( -1.166476076187854022E-15, 146.9449999999999932, 9.525000000000000355 ) ) ;
#36631 = CARTESIAN_POINT ( 'NONE',  ( 1.000000000000000000, 0.000000000000000000, 4.000000000000000000 ) ) ;
#36632 = VERTEX_POINT ( 'NONE', #36189 ) ;
#36633 = CARTESIAN_POINT ( 'NONE',  ( -5.598654528085808657, 147.7549999999999955, 7.705886871421373741 ) ) ;
#36634 = DIRECTION ( 'NONE',  ( -1.000000000000000000, 0.000000000000000000, 0.000000000000000000 ) ) ;
#36635 = ORIENTED_EDGE ( 'NONE', *, *, #9867, .F. ) ;
#36636 = CARTESIAN_POINT ( 'NONE',  ( 2.607480562269076430, 128.7929263765338135, -8.025000000000000355 ) ) ;
#36637 = DIRECTION ( 'NONE',  ( 0.000000000000000000, 0.000000000000000000, -1.000000000000000000 ) ) ;
#36638 = VECTOR ( 'NONE', #27792, 1000.000000000000000 ) ;
#36639 = CARTESIAN_POINT ( 'NONE',  ( 45.65811388300841855, 10.21937129433612235, -6.000000000000000000 ) ) ;
#36640 = EDGE_LOOP ( 'NONE', ( #37344, #27535, #61933, #68600 ) ) ;
#36641 = CARTESIAN_POINT ( 'NONE',  ( -24.00000000000000355, 36.75000000000000000, -3.000000000000000000 ) ) ;
#36642 = ORIENTED_EDGE ( 'NONE', *, *, #3809, .T. ) ;
#36643 = CARTESIAN_POINT ( 'NONE',  ( -59.84292637653379643, 9.058813317711329915, -2.943386871421373119 ) ) ;
#36644 =( GEOMETRIC_REPRESENTATION_CONTEXT ( 3 ) GLOBAL_UNCERTAINTY_ASSIGNED_CONTEXT ( ( #46676 ) ) GLOBAL_UNIT_ASSIGNED_CONTEXT ( ( #8, #64458, #22235 ) ) REPRESENTATION_CONTEXT ( 'NONE', 'WORKASPACE' ) );
#36645 =( LENGTH_UNIT ( ) NAMED_UNIT ( * ) SI_UNIT ( .MILLI., .METRE. ) );
#36646 = CARTESIAN_POINT ( 'NONE',  ( -48.50000000000000000, 99.99999999999992895, 7.000000000000000000 ) ) ;
#36647 = CARTESIAN_POINT ( 'NONE',  ( -149.7549999999999955, 4.716976649647091513, -6.492361379858946790 ) ) ;
#36648 = ORIENTED_EDGE ( 'NONE', *, *, #3352, .F. ) ;
#36649 = AXIS2_PLACEMENT_3D ( 'NONE', #38692, #39368, #12940 ) ;
#36650 = VECTOR ( 'NONE', #42395, 1000.000000000000000 ) ;
#36651 = LINE ( 'NONE', #10904, #369 ) ;
#36652 = CARTESIAN_POINT ( 'NONE',  ( -53.48759684591490071, -9.962924773521274702, 4.367854888790892787 ) ) ;
#36653 = CARTESIAN_POINT ( 'NONE',  ( 75.00000000000000000, 19.95407619327928828, 6.799666827783449108 ) ) ;
#36654 = ORIENTED_EDGE ( 'NONE', *, *, #14642, .T. ) ;
#36655 = VERTEX_POINT ( 'NONE', #41460 ) ;
#36656 = DIRECTION ( 'NONE',  ( 0.000000000000000000, 0.000000000000000000, 1.000000000000000000 ) ) ;
#36657 = FILL_AREA_STYLE ('',( #42611 ) ) ;
#36658 = CARTESIAN_POINT ( 'NONE',  ( -66.50499999999996703, -6.826472737025115478, -4.959722759717899443 ) ) ;
#36659 = ORIENTED_EDGE ( 'NONE', *, *, #43649, .F. ) ;
#36660 = FACE_OUTER_BOUND ( 'NONE', #29769, .T. ) ;
#36661 = ADVANCED_FACE ( 'NONE', ( #25930 ), #65556, .F. ) ;
#36662 = DIRECTION ( 'NONE',  ( -1.000000000000000000, -0.000000000000000000, -0.000000000000000000 ) ) ;
#36663 = CARTESIAN_POINT ( 'NONE',  ( -24.21231517720798010, 112.4999999999999858, -9.500000000000000000 ) ) ;
#36664 = ORIENTED_EDGE ( 'NONE', *, *, #55922, .T. ) ;
#36665 = CIRCLE ( 'NONE', #25361, 0.5000000000000004441 ) ;
#36666 = EDGE_CURVE ( 'NONE', #45861, #50251, #11270, .T. ) ;
#36667 = SURFACE_STYLE_FILL_AREA ( #37710 ) ;
#36668 = DIRECTION ( 'NONE',  ( 5.782411586589351722E-16, -1.000000000000000000, -0.000000000000000000 ) ) ;
#36669 = CARTESIAN_POINT ( 'NONE',  ( 35.99999999999999289, 0.000000000000000000, 37.00402776293825724 ) ) ;
#36671 = CARTESIAN_POINT ( 'NONE',  ( 2.607480562269075985, 126.9070736234661467, -8.025000000000000355 ) ) ;
#36670 = DIRECTION ( 'NONE',  ( -1.000000000000000000, 0.000000000000000000, 0.000000000000000000 ) ) ;
#36672 = AXIS2_PLACEMENT_3D ( 'NONE', #56213, #61827, #34076 ) ;
#36673 = ADVANCED_FACE ( 'NONE', ( #68877 ), #25250, .F. ) ;
#36674 = CARTESIAN_POINT ( 'NONE',  ( -1.166476076187854022E-15, 146.9449999999999932, 9.525000000000000355 ) ) ;
#36675 = CARTESIAN_POINT ( 'NONE',  ( -97.64499999999999602, 4.716976649647091513, -6.492361379858946790 ) ) ;
#36676 = CYLINDRICAL_SURFACE ( 'NONE', #64474, 0.2500000000000002220 ) ;
#36677 = STYLED_ITEM ( 'NONE', ( #32484 ), #49822 ) ;
#36678 = PRESENTATION_LAYER_ASSIGNMENT (  '', '', ( #18651 ) ) ;
#36679 = STYLED_ITEM ( 'NONE', ( #24140 ), #5396 ) ;
#36680 = DIRECTION ( 'NONE',  ( -0.5000000000000003331, 0.8660254037844383745, 0.000000000000000000 ) ) ;
#36681 = ORIENTED_EDGE ( 'NONE', *, *, #13743, .F. ) ;
#36682 = CARTESIAN_POINT ( 'NONE',  ( -129.8929263765338362, -8.102448949553172852, -5.886773742842741797 ) ) ;
#36683 = SURFACE_STYLE_FILL_AREA ( #15217 ) ;
#36684 = CARTESIAN_POINT ( 'NONE',  ( 57.74999999999998579, 30.99999999999999289, -3.750000000000000000 ) ) ;
#36685 = CARTESIAN_POINT ( 'NONE',  ( -158.2450000000000045, -4.716976649647093289, -6.492361379858945902 ) ) ;
#36686 = FILL_AREA_STYLE ('',( #45586 ) ) ;
#36687 = EDGE_CURVE ( 'NONE', #62990, #50964, #40894, .T. ) ;
#36688 = AXIS2_PLACEMENT_3D ( 'NONE', #53107, #4538, #14782 ) ;
#36689 = FILL_AREA_STYLE_COLOUR ( '', #2178 ) ;
#36690 = VECTOR ( 'NONE', #64100, 1000.000000000000000 ) ;
#36691 =( NAMED_UNIT ( * ) SI_UNIT ( $, .STERADIAN. ) SOLID_ANGLE_UNIT ( ) );
#36692 = DIRECTION ( 'NONE',  ( 0.000000000000000000, 0.000000000000000000, 1.000000000000000000 ) ) ;
#36693 = VERTEX_POINT ( 'NONE', #21347 ) ;
#36694 = ORIENTED_EDGE ( 'NONE', *, *, #20434, .T. ) ;
#36695 = TOROIDAL_SURFACE ( 'NONE', #5048, 2.000000000000000000, 1.000000000000000000 ) ;
#36696 = CARTESIAN_POINT ( 'NONE',  ( 4.358330484967978258, -1.733974831985841458, 6.451150163859151299 ) ) ;
#36697 =( LENGTH_UNIT ( ) NAMED_UNIT ( * ) SI_UNIT ( .MILLI., .METRE. ) );
#36698 = CARTESIAN_POINT ( 'NONE',  ( -45.00000000000000000, 9.701644063436994259, 6.099264075924462958 ) ) ;
#36699 = CARTESIAN_POINT ( 'NONE',  ( 23.21231517720797655, 117.4999999999999716, -9.500000000000000000 ) ) ;
#36700 = FILL_AREA_STYLE ('',( #9595 ) ) ;
#36701 = ORIENTED_EDGE ( 'NONE', *, *, #42500, .T. ) ;
#36702 = CARTESIAN_POINT ( 'NONE',  ( -152.7549999999999955, 4.716976649647091513, -6.492361379858946790 ) ) ;
#36703 = ORIENTED_EDGE ( 'NONE', *, *, #18026, .T. ) ;
#36704 = CARTESIAN_POINT ( 'NONE',  ( 30.99999999999998579, 5.000000000000000000, -72.00402776293822171 ) ) ;
#36705 = SURFACE_STYLE_USAGE ( .BOTH. , #16274 ) ;
#36706 = ORIENTED_EDGE ( 'NONE', *, *, #39558, .F. ) ;
#36707 = DIRECTION ( 'NONE',  ( -1.000000000000000000, 0.000000000000000000, 0.000000000000000000 ) ) ;
#36708 = ADVANCED_FACE ( 'NONE', ( #26944 ), #17500, .T. ) ;
#36709 = CARTESIAN_POINT ( 'NONE',  ( 3.094860106618435136, 124.2949999999999733, -9.525000000000000355 ) ) ;
#36710 = FACE_BOUND ( 'NONE', #21076, .T. ) ;
#36711 = VERTEX_POINT ( 'NONE', #32259 ) ;
#36712 = CARTESIAN_POINT ( 'NONE',  ( -5.365183871890746303, 4.707228941936129729, 0.1074872947962681735 ) ) ;
#36713 = CARTESIAN_POINT ( 'NONE',  ( 3.094860106618435136, 119.4049999999999727, -9.525000000000000355 ) ) ;
#36714 = CARTESIAN_POINT ( 'NONE',  ( -60.20499999999998408, -2.607480562269071545, -8.024999999999991473 ) ) ;
#36715 = PRESENTATION_STYLE_ASSIGNMENT (( #3203 ) ) ;
#36716 = PRODUCT_DEFINITION_SHAPE ( 'NONE', 'NONE',  #35663 ) ;
#36717 = ORIENTED_EDGE ( 'NONE', *, *, #10579, .T. ) ;
#36718 = CARTESIAN_POINT ( 'NONE',  ( -3.094860106618432471, 143.7050000000000125, -9.525000000000000355 ) ) ;
#36719 = SURFACE_SIDE_STYLE ('',( #58470 ) ) ;
#36720 = AXIS2_PLACEMENT_3D ( 'NONE', #68878, #63581, #62867 ) ;
#36721 = STYLED_ITEM ( 'NONE', ( #40159 ), #50223 ) ;
#36722 = VERTEX_POINT ( 'NONE', #64951 ) ;
#36723 = CARTESIAN_POINT ( 'NONE',  ( -10.11618306975752368, 54.14354156754873060, -2.000000000000000000 ) ) ;
#36724 = DIRECTION ( 'NONE',  ( 0.000000000000000000, 1.000000000000000000, 0.000000000000000000 ) ) ;
#36725 = FACE_OUTER_BOUND ( 'NONE', #5161, .T. ) ;
#36726 = CARTESIAN_POINT ( 'NONE',  ( -179.4550000000000125, 7.632228543268599452, -2.479861379858951942 ) ) ;
#36727 = EDGE_LOOP ( 'NONE', ( #50694, #62121, #59781, #17706 ) ) ;
#36728 = CARTESIAN_POINT ( 'NONE',  ( 7.514523004098860426, 111.2423389163705139, 4.578433682763816570 ) ) ;
#36729 = DIRECTION ( 'NONE',  ( 1.000000000000000000, 0.000000000000000000, 0.000000000000000000 ) ) ;
#36730 = DIRECTION ( 'NONE',  ( -1.000000000000000000, -0.000000000000000000, -0.000000000000000000 ) ) ;
#36731 = ORIENTED_EDGE ( 'NONE', *, *, #41473, .F. ) ;
#36732 = FACE_OUTER_BOUND ( 'NONE', #20720, .T. ) ;
#36733 =( LENGTH_UNIT ( ) NAMED_UNIT ( * ) SI_UNIT ( .MILLI., .METRE. ) );
#36734 = ORIENTED_EDGE ( 'NONE', *, *, #27454, .T. ) ;
#36735 = DIRECTION ( 'NONE',  ( 1.239088197126290324E-16, 0.000000000000000000, 1.000000000000000000 ) ) ;
#36736 = AXIS2_PLACEMENT_3D ( 'NONE', #53689, #25229, #46748 ) ;
#36737 = FILL_AREA_STYLE_COLOUR ( '', #15580 ) ;
#36738 = CARTESIAN_POINT ( 'NONE',  ( -99.05499999999999261, -9.827790563157499189E-16, -8.024999999999991473 ) ) ;
#36739 = ORIENTED_EDGE ( 'NONE', *, *, #59631, .T. ) ;
#36740 = EDGE_CURVE ( 'NONE', #52271, #40048, #16185, .T. ) ;
#36741 = DIRECTION ( 'NONE',  ( 1.000000000000000000, 0.000000000000000000, 0.000000000000000000 ) ) ;
#36742 = CARTESIAN_POINT ( 'NONE',  ( -128.7570736234661695, -5.598654528085801552, 7.705886871421367523 ) ) ;
#36743 = DIRECTION ( 'NONE',  ( 0.000000000000000000, 0.000000000000000000, 1.000000000000000000 ) ) ;
#36744 = CARTESIAN_POINT ( 'NONE',  ( 8.102448949553181734, 147.9949999999999193, -5.886773742842746238 ) ) ;
#36745 = CARTESIAN_POINT ( 'NONE',  ( -71.90707362346614673, -3.094860106618429807, 9.524999999999991473 ) ) ;
#36746 = VERTEX_POINT ( 'NONE', #38626 ) ;
#36747 = PLANE ( 'NONE',  #67619 ) ;
#36748 = CARTESIAN_POINT ( 'NONE',  ( -19.33026007562384052, -11.73551398946232460, 2.520887762979119540 ) ) ;
#36749 = DIRECTION ( 'NONE',  ( 0.000000000000000000, 0.000000000000000000, -1.000000000000000000 ) ) ;
#36750 = CARTESIAN_POINT ( 'NONE',  ( -116.3049999999999784, 8.437984349512085203, -1.550032578732815448E-15 ) ) ;
#36751 = ADVANCED_FACE ( 'NONE', ( #33312 ), #44251, .F. ) ;
#36752 = DIRECTION ( 'NONE',  ( -1.000000000000000000, 0.000000000000000000, 0.000000000000000000 ) ) ;
#36753 = CARTESIAN_POINT ( 'NONE',  ( 5.598654528085809545, 118.1449999999999818, -7.705886871421373741 ) ) ;
#36754 = CARTESIAN_POINT ( 'NONE',  ( -122.5449999999999875, -7.632228543268600340, -2.479861379858950166 ) ) ;
#36755 = EDGE_CURVE ( 'NONE', #13126, #30231, #26615, .T. ) ;
#36756 = CARTESIAN_POINT ( 'NONE',  ( -111.5070736234661837, 8.102448949553176405, 5.886773742842740909 ) ) ;
#36757 = FACE_OUTER_BOUND ( 'NONE', #3363, .T. ) ;
#36758 = EDGE_CURVE ( 'NONE', #46687, #3561, #49910, .T. ) ;
#36759 = ORIENTED_EDGE ( 'NONE', *, *, #6486, .T. ) ;
#36760 = CARTESIAN_POINT ( 'NONE',  ( -160.0429263765338135, -9.058813317711329915, -2.943386871421370898 ) ) ;
#36761 = DIRECTION ( 'NONE',  ( -0.000000000000000000, 1.000000000000000000, -0.000000000000000000 ) ) ;
#36762 = STYLED_ITEM ( 'NONE', ( #56846 ), #65101 ) ;
#36763 = EDGE_CURVE ( 'NONE', #11295, #7436, #43902, .T. ) ;
#36764 = VECTOR ( 'NONE', #14894, 1000.000000000000000 ) ;
#36765 = COLOUR_RGB ( '', 0.40784314, 0.44705882, 0.49803922) ;
#36766 = CARTESIAN_POINT ( 'NONE',  ( 72.49999999999998579, 64.07124727947029896, 10.00000000000000000 ) ) ;
#36767 = LINE ( 'NONE', #20180, #58254 ) ;
#36768 = CARTESIAN_POINT ( 'NONE',  ( 66.74999999999998579, 0.000000000000000000, 3.750000000000000000 ) ) ;
#36769 = ORIENTED_EDGE ( 'NONE', *, *, #13985, .T. ) ;
#36770 = CARTESIAN_POINT ( 'NONE',  ( -76.04292637653379927, -9.058813317711329915, -2.943386871421370898 ) ) ;
#36771 = CONTEXT_DEPENDENT_SHAPE_REPRESENTATION ( #49673, #59239 ) ;
#36772 = DIRECTION ( 'NONE',  ( -0.000000000000000000, -0.000000000000000000, -1.000000000000000000 ) ) ;
#36773 =( LENGTH_UNIT ( ) NAMED_UNIT ( * ) SI_UNIT ( .MILLI., .METRE. ) );
#36774 = DIRECTION ( 'NONE',  ( 0.000000000000000000, 0.000000000000000000, 1.000000000000000000 ) ) ;
#36775 = PLANE ( 'NONE',  #53861 ) ;
#36776 = CIRCLE ( 'NONE', #7554, 1.000000000000000888 ) ;
#36777 = CARTESIAN_POINT ( 'NONE',  ( -180.8050000000000068, -8.437984349512086979, 5.166775262442717831E-16 ) ) ;
#36778 = ORIENTED_EDGE ( 'NONE', *, *, #11292, .F. ) ;
#36779 = SURFACE_STYLE_FILL_AREA ( #49064 ) ;
#36780 = FILL_AREA_STYLE ('',( #20551 ) ) ;
#36781 = VERTEX_POINT ( 'NONE', #21705 ) ;
#36782 = CARTESIAN_POINT ( 'NONE',  ( -102.8929263765337936, -8.102448949553174629, -5.886773742842741797 ) ) ;
#36783 = DIRECTION ( 'NONE',  ( 1.000000000000000000, 0.000000000000000000, 0.000000000000000000 ) ) ;
#36784 = CARTESIAN_POINT ( 'NONE',  ( -2.607480562269075097, 140.4070736234661751, 8.025000000000000355 ) ) ;
#36785 =( NAMED_UNIT ( * ) SI_UNIT ( $, .STERADIAN. ) SOLID_ANGLE_UNIT ( ) );
#36786 = ORIENTED_EDGE ( 'NONE', *, *, #3914, .T. ) ;
#36787 = LINE ( 'NONE', #53281, #25984 ) ;
#36788 = CARTESIAN_POINT ( 'NONE',  ( -93.80499999999999261, -8.437984349512086979, 5.166775262442717831E-16 ) ) ;
#36789 = ORIENTED_EDGE ( 'NONE', *, *, #68383, .F. ) ;
#36790 = FILL_AREA_STYLE_COLOUR ( '', #49019 ) ;
#36791 = DIRECTION ( 'NONE',  ( 0.000000000000000000, 0.000000000000000000, 1.000000000000000000 ) ) ;
#36792 = FACE_OUTER_BOUND ( 'NONE', #62854, .T. ) ;
#36793 = FILL_AREA_STYLE_COLOUR ( '', #16249 ) ;
#36794 = ORIENTED_EDGE ( 'NONE', *, *, #57620, .F. ) ;
#36795 = CARTESIAN_POINT ( 'NONE',  ( 21.00000000000001776, 42.00000000000000000, 29.68999999999999417 ) ) ;
#36796 = CARTESIAN_POINT ( 'NONE',  ( -70.64499999999998181, 4.716976649647091513, -6.492361379858946790 ) ) ;
#36797 = EDGE_LOOP ( 'NONE', ( #36534, #27483, #31781 ) ) ;
#36798 = FACE_OUTER_BOUND ( 'NONE', #14247, .T. ) ;
#36799 = LINE ( 'NONE', #47729, #63767 ) ;
#36800 = FACE_OUTER_BOUND ( 'NONE', #30910, .T. ) ;
#36801 = ORIENTED_EDGE ( 'NONE', *, *, #7932, .F. ) ;
#36802 = DIRECTION ( 'NONE',  ( 0.000000000000000000, 0.000000000000000000, -1.000000000000000000 ) ) ;
#36803 = CARTESIAN_POINT ( 'NONE',  ( 4.000000000000002665, 38.70020753820971748, -89.00000000000000000 ) ) ;
#36804 = CIRCLE ( 'NONE', #37914, 0.2500000000000002220 ) ;
#36805 = ORIENTED_EDGE ( 'NONE', *, *, #9393, .T. ) ;
#36807 = EDGE_LOOP ( 'NONE', ( #7784, #58491, #21115, #42199 ) ) ;
#36806 = EDGE_CURVE ( 'NONE', #51506, #63065, #43223, .T. ) ;
#36808 = SURFACE_SIDE_STYLE ('',( #47021 ) ) ;
#36809 = CARTESIAN_POINT ( 'NONE',  ( -4.750000000000000000, 0.000000000000000000, 1.000000000000000000 ) ) ;
#36810 = LINE ( 'NONE', #3677, #15401 ) ;
#36811 = CARTESIAN_POINT ( 'NONE',  ( -160.4070736234661751, 3.094860106618428031, -9.524999999999993250 ) ) ;
#36812 = CARTESIAN_POINT ( 'NONE',  ( -8.102448949553179958, 121.8949999999999818, -5.886773742842749790 ) ) ;
#36813 = EDGE_CURVE ( 'NONE', #56663, #3150, #35512, .T. ) ;
#36814 = CARTESIAN_POINT ( 'NONE',  ( -99.95707362346617231, 9.058813317711329915, -2.943386871421373119 ) ) ;
#36815 = EDGE_CURVE ( 'NONE', #60196, #51351, #52139, .T. ) ;
#36816 = ORIENTED_EDGE ( 'NONE', *, *, #21038, .F. ) ;
#36817 = CARTESIAN_POINT ( 'NONE',  ( -107.6929263765338050, 10.01517768586948698, -1.839758294383808966E-15 ) ) ;
#36818 = ADVANCED_FACE ( 'NONE', ( #32966, #54401 ), #45284, .F. ) ;
#36820 = CARTESIAN_POINT ( 'NONE',  ( -15.98999599679679839, 117.9999999999999716, -10.00000000000000000 ) ) ;
#36819 = CARTESIAN_POINT ( 'NONE',  ( 44.50000000000000000, 10.36037961002804408, 3.500000000000000000 ) ) ;
#36821 =( LENGTH_UNIT ( ) NAMED_UNIT ( * ) SI_UNIT ( .MILLI., .METRE. ) );
#36822 = AXIS2_PLACEMENT_3D ( 'NONE', #32673, #68953, #63994 ) ;
#36823 = CARTESIAN_POINT ( 'NONE',  ( -143.4550000000000125, 7.632228543268599452, -2.479861379858951942 ) ) ;
#36824 = ADVANCED_FACE ( 'NONE', ( #35032 ), #24032, .F. ) ;
#36825 = DIRECTION ( 'NONE',  ( 1.000000000000000000, -1.445602896647339656E-16, -0.000000000000000000 ) ) ;
#36826 = CYLINDRICAL_SURFACE ( 'NONE', #32481, 8.025000000000000355 ) ;
#36827 = CARTESIAN_POINT ( 'NONE',  ( -151.9449999999999932, -9.827790563157499189E-16, -8.024999999999991473 ) ) ;
#36828 = EDGE_CURVE ( 'NONE', #41176, #50598, #4957, .T. ) ;
#36829 = CARTESIAN_POINT ( 'NONE',  ( -141.1449999999999818, -4.716976649647092401, 6.492361379858946790 ) ) ;
#36830 = ORIENTED_EDGE ( 'NONE', *, *, #2415, .T. ) ;
#36831 = DIRECTION ( 'NONE',  ( 0.000000000000000000, -0.000000000000000000, 1.000000000000000000 ) ) ;
#36832 =( NAMED_UNIT ( * ) PLANE_ANGLE_UNIT ( ) SI_UNIT ( $, .RADIAN. ) );
#36833 = ADVANCED_FACE ( 'NONE', ( #67054 ), #8316, .T. ) ;
#36834 =( NAMED_UNIT ( * ) PLANE_ANGLE_UNIT ( ) SI_UNIT ( $, .RADIAN. ) );
#36835 = UNCERTAINTY_MEASURE_WITH_UNIT (LENGTH_MEASURE( 1.000000000000000082E-05 ), #38466, 'distance_accuracy_value', 'NONE');
#36836 = CARTESIAN_POINT ( 'NONE',  ( -50.90499999999997982, 2.607480562269068880, -8.024999999999993250 ) ) ;
#36837 = CARTESIAN_POINT ( 'NONE',  ( -9.058813317711337021, 156.1550000000000011, -2.943386871421374895 ) ) ;
#36838 = FILL_AREA_STYLE ('',( #37895 ) ) ;
#36839 = CARTESIAN_POINT ( 'NONE',  ( -142.5570736234661808, -1.166476076187852838E-15, -9.524999999999991473 ) ) ;
#36840 = CARTESIAN_POINT ( 'NONE',  ( -154.5570736234661808, -1.166476076187852838E-15, -9.524999999999991473 ) ) ;
#36841 = UNCERTAINTY_MEASURE_WITH_UNIT (LENGTH_MEASURE( 1.000000000000000082E-05 ), #49351, 'distance_accuracy_value', 'NONE');
#36842 = CARTESIAN_POINT ( 'NONE',  ( 15.99999999999998224, 325.6078173946806942, -8.681240676409324175E-14 ) ) ;
#36843 = DIRECTION ( 'NONE',  ( -8.705236002253083981E-17, -0.7431448254773934670, -0.6691306063588592368 ) ) ;
#36844 = AXIS2_PLACEMENT_3D ( 'NONE', #20442, #37010, #9568 ) ;
#36845 = PRESENTATION_LAYER_ASSIGNMENT (  '', '', ( #3003 ) ) ;
#36846 = CIRCLE ( 'NONE', #49183, 1.000000000000000888 ) ;
#36847 = DIRECTION ( 'NONE',  ( -1.000000000000000000, 0.000000000000000000, 0.000000000000000000 ) ) ;
#36848 = DIRECTION ( 'NONE',  ( -0.000000000000000000, -0.000000000000000000, 1.000000000000000000 ) ) ;
#36849 = CARTESIAN_POINT ( 'NONE',  ( -78.59292637653379643, -3.094860106618431139, -9.524999999999991473 ) ) ;
#36850 = CARTESIAN_POINT ( 'NONE',  ( 8.256904162901424371, 56.03086067945960025, -6.591072975109653953 ) ) ;
#36851 = EDGE_LOOP ( 'NONE', ( #25352, #15201, #53755, #24603 ) ) ;
#36852 = VERTEX_POINT ( 'NONE', #55792 ) ;
#36853 = TOROIDAL_SURFACE ( 'NONE', #4240, 10.50000000000000533, 0.5000000000000000000 ) ;
#36854 = CARTESIAN_POINT ( 'NONE',  ( 6.826472737025119919, 114.0070736234661695, 4.959722759717908325 ) ) ;
#36855 = EDGE_CURVE ( 'NONE', #17287, #54496, #7222, .T. ) ;
#36856 = SURFACE_SIDE_STYLE ('',( #15397 ) ) ;
#36857 = DIRECTION ( 'NONE',  ( 1.000000000000000000, 0.000000000000000000, 0.000000000000000000 ) ) ;
#36858 = COLOUR_RGB ( '', 0.40784314, 0.44705882, 0.49803922) ;
#36859 = ORIENTED_EDGE ( 'NONE', *, *, #52741, .T. ) ;
#36860 = ORIENTED_EDGE ( 'NONE', *, *, #32313, .T. ) ;
#36861 = CARTESIAN_POINT ( 'NONE',  ( 28.58578643762690419, 43.00000000000000711, -89.99999999999998579 ) ) ;
#36862 = MECHANICAL_DESIGN_GEOMETRIC_PRESENTATION_REPRESENTATION (  '', ( #27808 ), #43824 ) ;
#36863 = PLANE ( 'NONE',  #35377 ) ;
#36864 = CARTESIAN_POINT ( 'NONE',  ( -20.83146879675249963, 149.9524772093542708, 9.749920261344563244 ) ) ;
#36865 = ORIENTED_EDGE ( 'NONE', *, *, #8032, .T. ) ;
#36866 = CARTESIAN_POINT ( 'NONE',  ( 9.058813317711337021, 115.6549999999999869, 2.943386871421375783 ) ) ;
#36867 = CARTESIAN_POINT ( 'NONE',  ( -85.94292637653380496, 0.000000000000000000, 9.524999999999991473 ) ) ;
#36868 = PRESENTATION_STYLE_ASSIGNMENT (( #42171 ) ) ;
#36869 = CARTESIAN_POINT ( 'NONE',  ( 17.25000000000000711, 24.74999999999997868, 3.750000000000000000 ) ) ;
#36870 = CARTESIAN_POINT ( 'NONE',  ( -98.24499999999999034, -4.716976649647093289, -6.492361379858945902 ) ) ;
#36871 = ORIENTED_EDGE ( 'NONE', *, *, #5075, .F. ) ;
#36872 = CARTESIAN_POINT ( 'NONE',  ( 6.088690765491501011, 153.9475726876337376, -6.602727378241971756 ) ) ;
#36873 = UNCERTAINTY_MEASURE_WITH_UNIT (LENGTH_MEASURE( 1.000000000000000082E-05 ), #68256, 'distance_accuracy_value', 'NONE');
#36874 = ORIENTED_EDGE ( 'NONE', *, *, #3213, .F. ) ;
#36875 = CARTESIAN_POINT ( 'NONE',  ( 4.716976649647099507, 155.6429263765338078, -6.492361379858953008 ) ) ;
#36876 = CARTESIAN_POINT ( 'NONE',  ( 57.00000000000000000, 14.00000000000000000, 47.50402776293824303 ) ) ;
#36877 = CARTESIAN_POINT ( 'NONE',  ( 12.50000000000000533, 28.24999999999998224, 3.750000000000000000 ) ) ;
#36878 = CARTESIAN_POINT ( 'NONE',  ( -20.88905466131707200, 149.9999999999999432, -9.626351540309148191 ) ) ;
#36879 = EDGE_CURVE ( 'NONE', #68764, #62693, #28338, .T. ) ;
#36880 = LINE ( 'NONE', #53035, #6005 ) ;
#36881 = ORIENTED_EDGE ( 'NONE', *, *, #23092, .T. ) ;
#36882 = CYLINDRICAL_SURFACE ( 'NONE', #39505, 0.5000000000000004441 ) ;
#36883 = DIRECTION ( 'NONE',  ( 0.000000000000000000, 0.000000000000000000, 1.000000000000000000 ) ) ;
#36884 = CARTESIAN_POINT ( 'NONE',  ( -140.9929263765338305, 8.102448949553172852, -5.886773742842744461 ) ) ;
#36885 = CARTESIAN_POINT ( 'NONE',  ( -35.31117902378667850, -9.718525487688223663, 4.712719346061684966 ) ) ;
#36886 = CARTESIAN_POINT ( 'NONE',  ( 22.25000000000000711, 34.24999999999999289, 4.000000000000000000 ) ) ;
#36887 =( BOUNDED_CURVE ( )  B_SPLINE_CURVE ( 2, ( #14955, #67351, #19147, #68067, #41003, #40650, #62059, #68398, #20192, #35702, #41347 ),
 .UNSPECIFIED., .F., .F. ) 
 B_SPLINE_CURVE_WITH_KNOTS ( ( 3, 2, 2, 2, 2, 3 ),
 ( 0.3478260869565133473, 0.3499999999999915401, 0.3521739130434697884, 0.3543478260869480367, 0.3565217391304262295, 0.3586956521739044224 ),
 .UNSPECIFIED. ) 
 CURVE ( )  GEOMETRIC_REPRESENTATION_ITEM ( )  RATIONAL_B_SPLINE_CURVE ( ( 1.000000000000188738, 0.9510565162949647933, 1.000000000000000000, 0.9510565162951535312, 1.000000000000000000, 0.9510565162951535312, 1.000000000000000000, 0.9510565162951535312, 1.000000000000000000, 0.9510565162953472651, 0.9999999999998062661 ) ) 
 REPRESENTATION_ITEM ( '' )  );
#36888 = FILL_AREA_STYLE_COLOUR ( '', #62007 ) ;
#36889 = LINE ( 'NONE', #26947, #402 ) ;
#36890 = EDGE_CURVE ( 'NONE', #25507, #49241, #33027, .T. ) ;
#36891 = DIRECTION ( 'NONE',  ( 0.000000000000000000, 0.000000000000000000, 1.000000000000000000 ) ) ;
#36892 = DIRECTION ( 'NONE',  ( -1.000000000000000000, -5.782411586589331015E-16, 0.000000000000000000 ) ) ;
#36893 = CARTESIAN_POINT ( 'NONE',  ( -40.99999999999997868, 9.999999999999980460, 3.000000000000000000 ) ) ;
#36894 = DIRECTION ( 'NONE',  ( 1.000000000000000000, 0.000000000000000000, 0.000000000000000000 ) ) ;
#36895 = ORIENTED_EDGE ( 'NONE', *, *, #44467, .F. ) ;
#36896 = MECHANICAL_DESIGN_GEOMETRIC_PRESENTATION_REPRESENTATION (  '', ( #819 ), #10999 ) ;
#36897 = ORIENTED_EDGE ( 'NONE', *, *, #24418, .T. ) ;
#36898 = PRESENTATION_STYLE_ASSIGNMENT (( #58315 ) ) ;
#36899 = VECTOR ( 'NONE', #20955, 1000.000000000000000 ) ;
#36900 = SURFACE_STYLE_USAGE ( .BOTH. , #9102 ) ;
#36901 = DIRECTION ( 'NONE',  ( 0.000000000000000000, 0.000000000000000000, 1.000000000000000000 ) ) ;
#36902 =( NAMED_UNIT ( * ) SI_UNIT ( $, .STERADIAN. ) SOLID_ANGLE_UNIT ( ) );
#36903 = EDGE_LOOP ( 'NONE', ( #15565, #32950, #61127, #39366, #748, #17522, #31303 ) ) ;
#36904 = SURFACE_STYLE_FILL_AREA ( #68535 ) ;
#36905 = CARTESIAN_POINT ( 'NONE',  ( -165.8050000000000068, -8.437984349512085203, 5.166775262442717831E-16 ) ) ;
#36906 = CARTESIAN_POINT ( 'NONE',  ( -12.72792206135785520, 114.9999999999999574, 10.50000000000000000 ) ) ;
#36907 = CARTESIAN_POINT ( 'NONE',  ( 39.74999999999999289, 16.24999999999997513, 3.750000000000000000 ) ) ;
#36908 = CARTESIAN_POINT ( 'NONE',  ( -182.9949999999999761, -6.826472737025115478, 4.959722759717900331 ) ) ;
#36909 = EDGE_CURVE ( 'NONE', #32880, #39571, #50186, .T. ) ;
#36910 = CIRCLE ( 'NONE', #41416, 0.5000000000000004441 ) ;
#36911 = CARTESIAN_POINT ( 'NONE',  ( -167.3949999999999534, -6.826472737025113702, -4.959722759717900331 ) ) ;
#36912 = ORIENTED_EDGE ( 'NONE', *, *, #2824, .F. ) ;
#36913 = LINE ( 'NONE', #31225, #62736 ) ;
#36914 = CARTESIAN_POINT ( 'NONE',  ( 0.000000000000000000, 0.000000000000000000, 0.000000000000000000 ) ) ;
#36915 = ADVANCED_FACE ( 'NONE', ( #57894 ), #25856, .T. ) ;
#36916 = CARTESIAN_POINT ( 'NONE',  ( -86.90499999999998693, 2.607480562269068880, -8.024999999999993250 ) ) ;
#36917 = CARTESIAN_POINT ( 'NONE',  ( 8.570369358082762901, 154.5000000000000000, 4.179281154892271033 ) ) ;
#36918 = CARTESIAN_POINT ( 'NONE',  ( -169.1070736234661922, 8.102448949553172852, -5.886773742842744461 ) ) ;
#36919 = SURFACE_SIDE_STYLE ('',( #57646 ) ) ;
#36920 = CARTESIAN_POINT ( 'NONE',  ( -91.64499999999999602, 4.716976649647091513, -6.492361379858946790 ) ) ;
#36921 = CARTESIAN_POINT ( 'NONE',  ( 10.01517768586949231, 130.8049999999999784, 1.839758294383810543E-15 ) ) ;
#36922 = CARTESIAN_POINT ( 'NONE',  ( -74.50000000000000000, 64.49137674618943095, 9.500000000000000000 ) ) ;
#36923 = CARTESIAN_POINT ( 'NONE',  ( -171.4429263765337907, -1.166476076187852838E-15, -9.524999999999991473 ) ) ;
#36924 = CARTESIAN_POINT ( 'NONE',  ( 45.50000000000000000, 99.99999999999992895, -10.00000000000000000 ) ) ;
#36925 = UNCERTAINTY_MEASURE_WITH_UNIT (LENGTH_MEASURE( 1.000000000000000082E-05 ), #56067, 'distance_accuracy_value', 'NONE');
#36926 = CARTESIAN_POINT ( 'NONE',  ( -74.39292637653380780, 8.102448949553176405, 5.886773742842740909 ) ) ;
#36927 = CARTESIAN_POINT ( 'NONE',  ( -75.50000000000000000, 64.49137674618943095, 9.500000000000001776 ) ) ;
#36928 = ORIENTED_EDGE ( 'NONE', *, *, #47719, .F. ) ;
#36929 = CARTESIAN_POINT ( 'NONE',  ( 6.062177826491068622, -2.500000000000000000, -3.500000000000001332 ) ) ;
#36931 = LINE ( 'NONE', #58345, #66323 ) ;
#36930 = DIRECTION ( 'NONE',  ( -1.156482317317873451E-16, -1.000000000000000000, 0.000000000000000000 ) ) ;
#36932 = DIRECTION ( 'NONE',  ( 0.000000000000000000, 0.000000000000000000, -1.000000000000000000 ) ) ;
#36933 = EDGE_LOOP ( 'NONE', ( #68297, #27458, #28425, #42792, #60288, #7852 ) ) ;
#36934 = CIRCLE ( 'NONE', #6540, 0.5000000000000004441 ) ;
#36935 = EDGE_LOOP ( 'NONE', ( #48765, #16895, #65622, #30347, #43559, #68739 ) ) ;
#36936 = PRESENTATION_STYLE_ASSIGNMENT (( #9499 ) ) ;
#36937 = B_SPLINE_CURVE_WITH_KNOTS ( 'NONE', 3,
 ( #14073, #34132, #7738, #1727, #17961, #35172 ),
 .UNSPECIFIED., .F., .F.,
 ( 4, 2, 4 ),
 ( 0.004189585287972440175, 0.006269578072783814175, 0.008349570857595188175 ),
 .UNSPECIFIED. ) ;
#36938 = CARTESIAN_POINT ( 'NONE',  ( -8.750000000000001776, 24.99999999999998579, -3.750000000000000000 ) ) ;
#36939 = AXIS2_PLACEMENT_3D ( 'NONE', #31557, #15425, #9790 ) ;
#36940 = EDGE_CURVE ( 'NONE', #13277, #25360, #28538, .T. ) ;
#36941 = FILL_AREA_STYLE ('',( #10179 ) ) ;
#36942 = DIRECTION ( 'NONE',  ( 0.000000000000000000, 0.000000000000000000, 1.000000000000000000 ) ) ;
#36943 = VECTOR ( 'NONE', #58145, 1000.000000000000000 ) ;
#36944 = SURFACE_STYLE_USAGE ( .BOTH. , #63970 ) ;
#36946 =( LENGTH_UNIT ( ) NAMED_UNIT ( * ) SI_UNIT ( .MILLI., .METRE. ) );
#36945 = MECHANICAL_DESIGN_GEOMETRIC_PRESENTATION_REPRESENTATION (  '', ( #41412 ), #43685 ) ;
#36947 = ORIENTED_EDGE ( 'NONE', *, *, #21684, .T. ) ;
#36948 = CARTESIAN_POINT ( 'NONE',  ( -126.6549999999999869, -7.632228543268600340, -2.479861379858950166 ) ) ;
#36949 = ORIENTED_EDGE ( 'NONE', *, *, #35675, .T. ) ;
#36950 = CARTESIAN_POINT ( 'NONE',  ( 6.826472737025121695, 129.6070736234661638, -4.959722759717905660 ) ) ;
#36951 = ORIENTED_EDGE ( 'NONE', *, *, #47378, .T. ) ;
#36952 = CARTESIAN_POINT ( 'NONE',  ( -195.0000000000000000, 1.166476076187852838E-15, -9.524999999999991473 ) ) ;
#36953 = CARTESIAN_POINT ( 'NONE',  ( 57.00000000000000000, 1.000000000000000000, -79.00402776293826435 ) ) ;
#36954 = VERTEX_POINT ( 'NONE', #36809 ) ;
#36955 = CIRCLE ( 'NONE', #13296, 0.2500000000000002220 ) ;
#36956 = LINE ( 'NONE', #31630, #45621 ) ;
#36957 = CARTESIAN_POINT ( 'NONE',  ( 9.058813317711337021, 150.5449999999999875, 2.943386871421375783 ) ) ;
#36958 = CARTESIAN_POINT ( 'NONE',  ( 4.041451884327376121, 7.000000000000007105, 1.082903768654759569 ) ) ;
#36959 =( GEOMETRIC_REPRESENTATION_CONTEXT ( 3 ) GLOBAL_UNCERTAINTY_ASSIGNED_CONTEXT ( ( #65646 ) ) GLOBAL_UNIT_ASSIGNED_CONTEXT ( ( #64620, #58292, #25573 ) ) REPRESENTATION_CONTEXT ( 'NONE', 'WORKASPACE' ) );
#36960 = VERTEX_POINT ( 'NONE', #35394 ) ;
#36961 = CARTESIAN_POINT ( 'NONE',  ( -54.65707362346616804, 9.058813317711329915, 2.943386871421369566 ) ) ;
#36962 = CARTESIAN_POINT ( 'NONE',  ( -9.058813317711338797, 153.4549999999999841, 2.943386871421373563 ) ) ;
#36963 =( NAMED_UNIT ( * ) SI_UNIT ( $, .STERADIAN. ) SOLID_ANGLE_UNIT ( ) );
#36964 = DIRECTION ( 'NONE',  ( -1.000000000000000000, 0.000000000000000000, 0.000000000000000000 ) ) ;
#36965 = ORIENTED_EDGE ( 'NONE', *, *, #24005, .T. ) ;
#36966 = CARTESIAN_POINT ( 'NONE',  ( 7.632228543268607446, 128.0429263765338135, 2.479861379858954606 ) ) ;
#36967 = CARTESIAN_POINT ( 'NONE',  ( -72.49999999999998579, 64.07124727947029896, 10.00000000000000000 ) ) ;
#36968 = UNCERTAINTY_MEASURE_WITH_UNIT (LENGTH_MEASURE( 1.000000000000000082E-05 ), #43826, 'distance_accuracy_value', 'NONE');
#36969 = CARTESIAN_POINT ( 'NONE',  ( -74.88655845637370589, 36.30736609777607526, -9.975975838750319014 ) ) ;
#36970 = STYLED_ITEM ( 'NONE', ( #29850 ), #68163 ) ;
#36971 = CARTESIAN_POINT ( 'NONE',  ( 82.09357085539578236, 5.000000000000000000, 37.00402776293825724 ) ) ;
#36972 = EDGE_CURVE ( 'NONE', #11136, #11113, #9005, .T. ) ;
#36973 = FILL_AREA_STYLE_COLOUR ( '', #5884 ) ;
#36974 = EDGE_CURVE ( 'NONE', #44704, #24621, #47366, .T. ) ;
#36975 = ORIENTED_EDGE ( 'NONE', *, *, #42098, .T. ) ;
#36976 = CARTESIAN_POINT ( 'NONE',  ( -4.750000000000002665, 0.000000000000000000, 4.000000000000000000 ) ) ;
#36977 = ORIENTED_EDGE ( 'NONE', *, *, #1776, .F. ) ;
#36978 = CARTESIAN_POINT ( 'NONE',  ( -57.29292637653379217, 3.094860106618428031, -9.524999999999993250 ) ) ;
#36979 = CARTESIAN_POINT ( 'NONE',  ( -151.5550000000000068, 0.000000000000000000, 8.024999999999991473 ) ) ;
#36980 = FACE_OUTER_BOUND ( 'NONE', #68456, .T. ) ;
#36981 = UNCERTAINTY_MEASURE_WITH_UNIT (LENGTH_MEASURE( 1.000000000000000082E-05 ), #11403, 'distance_accuracy_value', 'NONE');
#36982 = ADVANCED_FACE ( 'NONE', ( #62788 ), #42442, .T. ) ;
#36983 = AXIS2_PLACEMENT_3D ( 'NONE', #26303, #47847, #69244 ) ;
#36984 = CARTESIAN_POINT ( 'NONE',  ( -5.885195493260865440, -3.806542393196800766, 1.022368767335940312E-15 ) ) ;
#36985 =( NAMED_UNIT ( * ) SI_UNIT ( $, .STERADIAN. ) SOLID_ANGLE_UNIT ( ) );
#36986 = CARTESIAN_POINT ( 'NONE',  ( -4.750000000000002665, 22.24999999999998579, -3.750000000000000000 ) ) ;
#36987 = VERTEX_POINT ( 'NONE', #8657 ) ;
#36989 = EDGE_CURVE ( 'NONE', #12632, #43539, #30418, .T. ) ;
#36988 = ORIENTED_EDGE ( 'NONE', *, *, #67147, .F. ) ;
#36990 = CARTESIAN_POINT ( 'NONE',  ( 23.32315385395093799, 24.57035872801869658, 27.19478135492500925 ) ) ;
#36991 = PRESENTATION_LAYER_ASSIGNMENT (  '', '', ( #68382 ) ) ;
#36992 = CARTESIAN_POINT ( 'NONE',  ( -84.44292637653380496, -1.166476076187852838E-15, -9.524999999999991473 ) ) ;
#36993 = CARTESIAN_POINT ( 'NONE',  ( -68.15499999999997272, 7.632228543268600340, 2.479861379858949277 ) ) ;
#36994 = ORIENTED_EDGE ( 'NONE', *, *, #16153, .F. ) ;
#36995 = DIRECTION ( 'NONE',  ( 1.000000000000000000, 0.000000000000000000, 0.000000000000000000 ) ) ;
#36996 = FILL_AREA_STYLE_COLOUR ( '', #11054 ) ;
#36997 = STYLED_ITEM ( 'NONE', ( #43244 ), #20089 ) ;
#36998 = EDGE_CURVE ( 'NONE', #6742, #65490, #13399, .T. ) ;
#36999 =( GEOMETRIC_REPRESENTATION_CONTEXT ( 3 ) GLOBAL_UNCERTAINTY_ASSIGNED_CONTEXT ( ( #46866 ) ) GLOBAL_UNIT_ASSIGNED_CONTEXT ( ( #43961, #60091, #11553 ) ) REPRESENTATION_CONTEXT ( 'NONE', 'WORKASPACE' ) );
#37000 = CARTESIAN_POINT ( 'NONE',  ( 0.000000000000000000, 113.9429263765338192, -8.025000000000000355 ) ) ;
#37001 = DIRECTION ( 'NONE',  ( 0.000000000000000000, 0.000000000000000000, 1.000000000000000000 ) ) ;
#37002 = STYLED_ITEM ( 'NONE', ( #57169 ), #4509 ) ;
#37003 = VERTEX_POINT ( 'NONE', #47744 ) ;
#37004 =( BOUNDED_CURVE ( )  B_SPLINE_CURVE ( 2, ( #5544, #43598, #11534, #48179, #26994, #20721, #64989, #37638, #42235, #37980, #53430 ),
 .UNSPECIFIED., .F., .F. ) 
 B_SPLINE_CURVE_WITH_KNOTS ( ( 3, 2, 2, 2, 2, 3 ),
 ( 0.4117647058823530326, 0.4176470588235295378, 0.4235294117647059875, 0.4294117647058824372, 0.4352941176470589424, 0.4411764705882353921 ),
 .UNSPECIFIED. ) 
 CURVE ( )  GEOMETRIC_REPRESENTATION_ITEM ( )  RATIONAL_B_SPLINE_CURVE ( ( 0.9999999999999991118, 0.9510565162951544194, 1.000000000000000000, 0.9510565162951535312, 1.000000000000000000, 0.9510565162951535312, 1.000000000000000000, 0.9510565162951535312, 1.000000000000000000, 0.9510565162951526430, 1.000000000000000888 ) ) 
 REPRESENTATION_ITEM ( '' )  );
#37005 = DIRECTION ( 'NONE',  ( 0.000000000000000000, 1.000000000000000000, 0.000000000000000000 ) ) ;
#37006 = ADVANCED_FACE ( 'NONE', ( #14997 ), #8334, .T. ) ;
#37007 = DIRECTION ( 'NONE',  ( -0.000000000000000000, 1.000000000000000000, -0.000000000000000000 ) ) ;
#37008 = SURFACE_SIDE_STYLE ('',( #26047 ) ) ;
#37009 = PRESENTATION_LAYER_ASSIGNMENT (  '', '', ( #39199 ) ) ;
#37010 = DIRECTION ( 'NONE',  ( 1.000000000000000000, 0.000000000000000000, -1.300977106640434891E-16 ) ) ;
#37011 = PRESENTATION_LAYER_ASSIGNMENT (  '', '', ( #65001 ) ) ;
#37012 = CARTESIAN_POINT ( 'NONE',  ( -121.9449999999999932, -9.827790563157499189E-16, -8.024999999999991473 ) ) ;
#37013 = CARTESIAN_POINT ( 'NONE',  ( 3.094860106618431583, 150.0949999999999420, 9.525000000000000355 ) ) ;
#37014 = CARTESIAN_POINT ( 'NONE',  ( -88.79499999999998749, 2.607480562269068880, -8.024999999999993250 ) ) ;
#37015 = SURFACE_STYLE_FILL_AREA ( #47223 ) ;
#37016 = STYLED_ITEM ( 'NONE', ( #62113 ), #14700 ) ;
#37017 = FACE_OUTER_BOUND ( 'NONE', #1833, .T. ) ;
#37018 = UNCERTAINTY_MEASURE_WITH_UNIT (LENGTH_MEASURE( 1.000000000000000082E-05 ), #49008, 'distance_accuracy_value', 'NONE');
#37019 = MECHANICAL_DESIGN_GEOMETRIC_PRESENTATION_REPRESENTATION (  '', ( #58305 ), #6608 ) ;
#37020 = DIRECTION ( 'NONE',  ( -0.000000000000000000, 1.000000000000000000, -0.000000000000000000 ) ) ;
#37021 = ORIENTED_EDGE ( 'NONE', *, *, #16044, .T. ) ;
#37022 = CARTESIAN_POINT ( 'NONE',  ( -132.8929263765337794, -8.102448949553172852, -5.886773742842741797 ) ) ;
#37023 = SURFACE_SIDE_STYLE ('',( #36683 ) ) ;
#37024 = DIRECTION ( 'NONE',  ( 1.000000000000000000, -0.000000000000000000, -0.000000000000000000 ) ) ;
#37025 = CARTESIAN_POINT ( 'NONE',  ( -159.2949999999999875, -2.607480562269069768, 8.024999999999991473 ) ) ;
#37026 = CARTESIAN_POINT ( 'NONE',  ( 0.04677136509298115974, 68.99999999999998579, -6.349999999999994316 ) ) ;
#37027 = AXIS2_PLACEMENT_3D ( 'NONE', #12187, #22772, #18176 ) ;
#37028 = CARTESIAN_POINT ( 'NONE',  ( 0.000000000000000000, 154.9999999999999716, 0.000000000000000000 ) ) ;
#37029 = EDGE_LOOP ( 'NONE', ( #50314, #2026, #1232, #13383 ) ) ;
#37030 = ORIENTED_EDGE ( 'NONE', *, *, #14168, .F. ) ;
#37031 = FACE_OUTER_BOUND ( 'NONE', #52227, .T. ) ;
#37032 = PRESENTATION_LAYER_ASSIGNMENT (  '', '', ( #50498 ) ) ;
#37033 = CARTESIAN_POINT ( 'NONE',  ( -144.4429263765337907, -1.166476076187852838E-15, -9.524999999999991473 ) ) ;
#37034 = CARTESIAN_POINT ( 'NONE',  ( -45.00000000000000000, 8.062885781073939384, 6.000000000000002665 ) ) ;
#37035 = DIRECTION ( 'NONE',  ( -0.000000000000000000, 1.000000000000000000, -0.000000000000000000 ) ) ;
#37036 = CIRCLE ( 'NONE', #20097, 8.999999999999994671 ) ;
#37037 = VERTEX_POINT ( 'NONE', #20946 ) ;
#37038 = CARTESIAN_POINT ( 'NONE',  ( -151.7050000000000125, 2.607480562269072433, 8.024999999999991473 ) ) ;
#37039 = EDGE_LOOP ( 'NONE', ( #68200, #33786, #48523, #63346 ) ) ;
#37040 = ORIENTED_EDGE ( 'NONE', *, *, #17608, .T. ) ;
#37041 = STYLED_ITEM ( 'NONE', ( #62154 ), #10382 ) ;
#37042 = CIRCLE ( 'NONE', #54947, 7.500000000000007105 ) ;
#37043 = CARTESIAN_POINT ( 'NONE',  ( -9.058813317711337021, 122.0449999999999875, -2.943386871421374895 ) ) ;
#37044 = AXIS2_PLACEMENT_3D ( 'NONE', #19461, #40604, #9277 ) ;
#37045 = AXIS2_PLACEMENT_3D ( 'NONE', #56446, #25474, #57859 ) ;
#37046 = VERTEX_POINT ( 'NONE', #35736 ) ;
#37047 = EDGE_CURVE ( 'NONE', #15297, #40156, #20592, .T. ) ;
#37048 =( LENGTH_UNIT ( ) NAMED_UNIT ( * ) SI_UNIT ( .MILLI., .METRE. ) );
#37049 = CARTESIAN_POINT ( 'NONE',  ( -9.058813317711338797, 117.4549999999999841, 2.943386871421373563 ) ) ;
#37050 = CARTESIAN_POINT ( 'NONE',  ( -66.95499999999998408, -7.632228543268599452, 2.479861379858951054 ) ) ;
#37051 = CARTESIAN_POINT ( 'NONE',  ( -41.03182778381239615, 107.9802461459568690, -3.207526698639570295 ) ) ;
#37052 = VERTEX_POINT ( 'NONE', #57170 ) ;
#37053 = CARTESIAN_POINT ( 'NONE',  ( -3.094860106618434248, 144.9050000000000011, 9.525000000000000355 ) ) ;
#37054 = UNCERTAINTY_MEASURE_WITH_UNIT (LENGTH_MEASURE( 1.000000000000000082E-05 ), #10221, 'distance_accuracy_value', 'NONE');
#37055 = EDGE_CURVE ( 'NONE', #11185, #29083, #62242, .T. ) ;
#37056 =( NAMED_UNIT ( * ) SI_UNIT ( $, .STERADIAN. ) SOLID_ANGLE_UNIT ( ) );
#37057 = ADVANCED_FACE ( 'NONE', ( #19883 ), #31126, .F. ) ;
#37058 = DIRECTION ( 'NONE',  ( -1.000000000000000000, 0.000000000000000000, 0.000000000000000000 ) ) ;
#37059 = CARTESIAN_POINT ( 'NONE',  ( 27.99999999999999645, 5.000000000000000000, 24.00402776293821816 ) ) ;
#37060 =( LENGTH_UNIT ( ) NAMED_UNIT ( * ) SI_UNIT ( .MILLI., .METRE. ) );
#37061 = ORIENTED_EDGE ( 'NONE', *, *, #32707, .F. ) ;
#37062 = AXIS2_PLACEMENT_3D ( 'NONE', #23364, #2554, #40260 ) ;
#37063 =( NAMED_UNIT ( * ) PLANE_ANGLE_UNIT ( ) SI_UNIT ( $, .RADIAN. ) );
#37064 =( NAMED_UNIT ( * ) PLANE_ANGLE_UNIT ( ) SI_UNIT ( $, .RADIAN. ) );
#37065 = CARTESIAN_POINT ( 'NONE',  ( -47.69499999999999318, -8.437984349512085203, 5.166775262442717831E-16 ) ) ;
#37066 = VERTEX_POINT ( 'NONE', #4042 ) ;
#37067 = CARTESIAN_POINT ( 'NONE',  ( 27.99999999999998934, 5.000000000000000000, 37.00402776293829277 ) ) ;
#37068 = VECTOR ( 'NONE', #7472, 1000.000000000000000 ) ;
#37069 = APPLICATION_CONTEXT ( 'automotive_design' ) ;
#37070 = CARTESIAN_POINT ( 'NONE',  ( 10.00000000000000178, 43.00000000000000000, -90.00000000000000000 ) ) ;
#37071 = ORIENTED_EDGE ( 'NONE', *, *, #18440, .F. ) ;
#37072 = CARTESIAN_POINT ( 'NONE',  ( 28.00000000000000000, 37.76051491742381216, -89.34202014332566932 ) ) ;
#37073 = LINE ( 'NONE', #63063, #57999 ) ;
#37074 = ORIENTED_EDGE ( 'NONE', *, *, #20950, .T. ) ;
#37075 = CIRCLE ( 'NONE', #3276, 0.5000000000000004441 ) ;
#37076 = ADVANCED_FACE ( 'NONE', ( #25509 ), #47022, .F. ) ;
#37077 =( LENGTH_UNIT ( ) NAMED_UNIT ( * ) SI_UNIT ( .MILLI., .METRE. ) );
#37078 = CARTESIAN_POINT ( 'NONE',  ( -91.55499999999997840, 0.000000000000000000, 8.024999999999991473 ) ) ;
#37079 = ORIENTED_EDGE ( 'NONE', *, *, #47898, .F. ) ;
#37080 =( NAMED_UNIT ( * ) PLANE_ANGLE_UNIT ( ) SI_UNIT ( $, .RADIAN. ) );
#37081 = CARTESIAN_POINT ( 'NONE',  ( -132.2070736234661297, 3.094860106618433360, 9.524999999999991473 ) ) ;
#37082 = AXIS2_PLACEMENT_3D ( 'NONE', #17492, #11487, #38621 ) ;
#37083 = VECTOR ( 'NONE', #45630, 1000.000000000000000 ) ;
#37084 = PRESENTATION_STYLE_ASSIGNMENT (( #36397 ) ) ;
#37085 = CARTESIAN_POINT ( 'NONE',  ( -10.01517768586949408, 152.1949999999999932, -6.132527647946036459E-16 ) ) ;
#37086 = CARTESIAN_POINT ( 'NONE',  ( -62.15707362346617515, -9.058813317711329915, -2.943386871421370898 ) ) ;
#37087 = CIRCLE ( 'NONE', #8974, 1.000000000000000888 ) ;
#37088 = CARTESIAN_POINT ( 'NONE',  ( -80.54292637653379927, 9.058813317711329915, 2.943386871421369566 ) ) ;
#37089 = VERTEX_POINT ( 'NONE', #37866 ) ;
#37090 = DIRECTION ( 'NONE',  ( 0.000000000000000000, 0.000000000000000000, 1.000000000000000000 ) ) ;
#37092 = CARTESIAN_POINT ( 'NONE',  ( 98.00000000000000000, 5.000000000000000000, 0.000000000000000000 ) ) ;
#37091 = CARTESIAN_POINT ( 'NONE',  ( 49.12162162162162105, 13.70805908423323238, 10.00000000000000000 ) ) ;
#37093 = AXIS2_PLACEMENT_3D ( 'NONE', #2179, #49767, #23710 ) ;
#37094 = CARTESIAN_POINT ( 'NONE',  ( -109.4049999999999727, -2.607480562269069768, 8.024999999999991473 ) ) ;
#37095 = EDGE_CURVE ( 'NONE', #30008, #31521, #16242, .T. ) ;
#37096 = CARTESIAN_POINT ( 'NONE',  ( 9.058813317711337021, 120.5449999999999875, 2.943386871421375783 ) ) ;
#37097 = CARTESIAN_POINT ( 'NONE',  ( -128.8449999999999989, -7.632228543268599452, 2.479861379858951054 ) ) ;
#37098 = VECTOR ( 'NONE', #29576, 1000.000000000000000 ) ;
#37099 = CIRCLE ( 'NONE', #40433, 0.5000000000000004441 ) ;
#37100 = EDGE_CURVE ( 'NONE', #53532, #67533, #33085, .T. ) ;
#37101 = COLOUR_RGB ( '', 0.08235294, 0.09019608, 0.10196078) ;
#37102 = CARTESIAN_POINT ( 'NONE',  ( -9.827790563157511022E-16, 145.4429263765338192, 8.025000000000000355 ) ) ;
#37103 = ORIENTED_EDGE ( 'NONE', *, *, #65982, .F. ) ;
#37104 = COLOUR_RGB ( '', 0.09019608, 0.27058824, 0.51372549) ;
#37105 = CARTESIAN_POINT ( 'NONE',  ( -161.2429263765338021, 5.598654528085804216, 7.705886871421366635 ) ) ;
#37106 =( NAMED_UNIT ( * ) SI_UNIT ( $, .STERADIAN. ) SOLID_ANGLE_UNIT ( ) );
#37107 = DIRECTION ( 'NONE',  ( -1.000000000000000000, 0.000000000000000000, 0.000000000000000000 ) ) ;
#37108 = VECTOR ( 'NONE', #40726, 1000.000000000000000 ) ;
#37109 = CARTESIAN_POINT ( 'NONE',  ( -190.0000000000000000, 0.000000000000000000, 0.000000000000000000 ) ) ;
#37110 = AXIS2_PLACEMENT_3D ( 'NONE', #64738, #42628, #32714 ) ;
#37111 = CARTESIAN_POINT ( 'NONE',  ( -20.68758241885016247, 114.6823486699484107, -10.00000000000000178 ) ) ;
#37112 = CARTESIAN_POINT ( 'NONE',  ( -53.72233514740115368, -9.706441612173417610, -3.029717619416509411 ) ) ;
#37113 = DIRECTION ( 'NONE',  ( 0.000000000000000000, 0.000000000000000000, -1.000000000000000000 ) ) ;
#37114 = EDGE_LOOP ( 'NONE', ( #47170, #46840, #53871 ) ) ;
#37115 = CARTESIAN_POINT ( 'NONE',  ( -75.44292637653379074, -1.166476076187852838E-15, -9.524999999999991473 ) ) ;
#37116 = PRESENTATION_LAYER_ASSIGNMENT (  '', '', ( #12346 ) ) ;
#37117 = FACE_OUTER_BOUND ( 'NONE', #57132, .T. ) ;
#37118 = CARTESIAN_POINT ( 'NONE',  ( 20.00000000000001776, 14.00000000000000000, -29.68999999999999417 ) ) ;
#37119 =( GEOMETRIC_REPRESENTATION_CONTEXT ( 3 ) GLOBAL_UNCERTAINTY_ASSIGNED_CONTEXT ( ( #30455 ) ) GLOBAL_UNIT_ASSIGNED_CONTEXT ( ( #37729, #52829, #69673 ) ) REPRESENTATION_CONTEXT ( 'NONE', 'WORKASPACE' ) );
#37120 = DIRECTION ( 'NONE',  ( 1.000000000000000000, 0.000000000000000000, 0.000000000000000000 ) ) ;
#37121 = CARTESIAN_POINT ( 'NONE',  ( 22.00000000000000711, 50.00000000000000000, -59.99999999999999289 ) ) ;
#37122 = PRESENTATION_LAYER_ASSIGNMENT (  '', '', ( #53888 ) ) ;
#37123 = CARTESIAN_POINT ( 'NONE',  ( -181.5550000000000068, 0.000000000000000000, 8.024999999999991473 ) ) ;
#37124 = ORIENTED_EDGE ( 'NONE', *, *, #5192, .T. ) ;
#37125 = CARTESIAN_POINT ( 'NONE',  ( 2.000000000000022649, 50.00000000000000000, 60.00000000000000711 ) ) ;
#37126 = EDGE_CURVE ( 'NONE', #37491, #13013, #59594, .T. ) ;
#37127 = FACE_OUTER_BOUND ( 'NONE', #68412, .T. ) ;
#37128 = CARTESIAN_POINT ( 'NONE',  ( 0.000000000000000000, 87.30187232391182306, 0.000000000000000000 ) ) ;
#37129 = DIRECTION ( 'NONE',  ( -1.000000000000000000, 0.000000000000000000, 0.000000000000000000 ) ) ;
#37130 = CARTESIAN_POINT ( 'NONE',  ( -9.827790563157511022E-16, 140.5570736234661524, 8.025000000000000355 ) ) ;
#37131 = ORIENTED_EDGE ( 'NONE', *, *, #31688, .T. ) ;
#37132 = CARTESIAN_POINT ( 'NONE',  ( 34.99999999999999289, 99.99999999999997158, -3.500000000000000000 ) ) ;
#37133 = CARTESIAN_POINT ( 'NONE',  ( -90.80499999999996419, -8.437984349512086979, 5.166775262442717831E-16 ) ) ;
#37134 = UNCERTAINTY_MEASURE_WITH_UNIT (LENGTH_MEASURE( 1.000000000000000082E-05 ), #37584, 'distance_accuracy_value', 'NONE');
#37135 = CARTESIAN_POINT ( 'NONE',  ( 4.716976649647096842, 131.8570736234661638, 6.492361379858953896 ) ) ;
#37136 = ORIENTED_EDGE ( 'NONE', *, *, #29946, .T. ) ;
#37137 = CARTESIAN_POINT ( 'NONE',  ( -44.99999999999977973, 149.9999999999999716, -9.500000000000000000 ) ) ;
#37138 = EDGE_CURVE ( 'NONE', #51653, #17133, #52234, .T. ) ;
#37139 =( NAMED_UNIT ( * ) PLANE_ANGLE_UNIT ( ) SI_UNIT ( $, .RADIAN. ) );
#37140 = CARTESIAN_POINT ( 'NONE',  ( -83.60707362346617799, -8.102448949553174629, 5.886773742842742685 ) ) ;
#37141 = DIRECTION ( 'NONE',  ( 0.000000000000000000, 0.000000000000000000, -1.000000000000000000 ) ) ;
#37142 = MECHANICAL_DESIGN_GEOMETRIC_PRESENTATION_REPRESENTATION (  '', ( #28063 ), #20211 ) ;
#37143 = EDGE_LOOP ( 'NONE', ( #28596, #31346, #1968, #33846 ) ) ;
#37144 = CARTESIAN_POINT ( 'NONE',  ( -72.74499999999999034, 4.716976649647094177, 6.492361379858945902 ) ) ;
#37145 = VERTEX_POINT ( 'NONE', #64876 ) ;
#37146 = CARTESIAN_POINT ( 'NONE',  ( -30.38025804287906340, -13.49999999999999822, -2.000000000000000000 ) ) ;
#37147 = CARTESIAN_POINT ( 'NONE',  ( -60.00000000000000000, -2.024042244987997205E-14, 10.00000000000000000 ) ) ;
#37148 = STYLED_ITEM ( 'NONE', ( #31335 ), #33134 ) ;
#37149 = ORIENTED_EDGE ( 'NONE', *, *, #11431, .T. ) ;
#37150 = FILL_AREA_STYLE_COLOUR ( '', #46070 ) ;
#37151 = AXIS2_PLACEMENT_3D ( 'NONE', #65264, #23390, #55403 ) ;
#37152 = ADVANCED_FACE ( 'NONE', ( #5771 ), #53635, .F. ) ;
#37153 = DIRECTION ( 'NONE',  ( 1.000000000000000000, 0.000000000000000000, 0.000000000000000000 ) ) ;
#37154 = DIRECTION ( 'NONE',  ( 1.000000000000000000, 0.000000000000000000, 0.000000000000000000 ) ) ;
#37155 = VERTEX_POINT ( 'NONE', #26864 ) ;
#37156 = CARTESIAN_POINT ( 'NONE',  ( 0.000000000000000000, 0.000000000000000000, 7.500000000000000000 ) ) ;
#37157 = VECTOR ( 'NONE', #8780, 1000.000000000000000 ) ;
#37158 = ORIENTED_EDGE ( 'NONE', *, *, #23603, .T. ) ;
#37159 = PRESENTATION_STYLE_ASSIGNMENT (( #64875 ) ) ;
#37160 = DIRECTION ( 'NONE',  ( 0.000000000000000000, 0.000000000000000000, -1.000000000000000000 ) ) ;
#37161 = DIRECTION ( 'NONE',  ( -0.000000000000000000, 0.000000000000000000, -1.000000000000000000 ) ) ;
#37162 = CARTESIAN_POINT ( 'NONE',  ( -160.2570736234661979, 5.598654528085800663, -7.705886871421367523 ) ) ;
#37163 = CIRCLE ( 'NONE', #53973, 0.5000000000000004441 ) ;
#37164 = CARTESIAN_POINT ( 'NONE',  ( -3.094860106618434248, 122.7949999999999875, 9.525000000000000355 ) ) ;
#37165 = CARTESIAN_POINT ( 'NONE',  ( -94.55707362346616662, -1.166476076187852838E-15, -9.524999999999991473 ) ) ;
#37166 =( GEOMETRIC_REPRESENTATION_CONTEXT ( 3 ) GLOBAL_UNCERTAINTY_ASSIGNED_CONTEXT ( ( #48096 ) ) GLOBAL_UNIT_ASSIGNED_CONTEXT ( ( #3170, #46543, #45825 ) ) REPRESENTATION_CONTEXT ( 'NONE', 'WORKASPACE' ) );
#37167 = CARTESIAN_POINT ( 'NONE',  ( -44.99999999999998579, 119.9999999999999716, -9.500000000000000000 ) ) ;
#37168 = ORIENTED_EDGE ( 'NONE', *, *, #69110, .F. ) ;
#37169 = AXIS2_PLACEMENT_3D ( 'NONE', #29059, #18186, #61422 ) ;
#37170 =( NAMED_UNIT ( * ) SI_UNIT ( $, .STERADIAN. ) SOLID_ANGLE_UNIT ( ) );
#37172 = CARTESIAN_POINT ( 'NONE',  ( 57.00000000000000000, 0.000000000000000000, -60.00402776293827145 ) ) ;
#37171 = FACE_OUTER_BOUND ( 'NONE', #32232, .T. ) ;
#37173 = CARTESIAN_POINT ( 'NONE',  ( -7.794228634059950700, -4.500000000000003553, 0.000000000000000000 ) ) ;
#37174 = CARTESIAN_POINT ( 'NONE',  ( -143.6049999999999613, 6.826472737025113702, -4.959722759717902107 ) ) ;
#37175 = SURFACE_STYLE_FILL_AREA ( #32522 ) ;
#37176 = CARTESIAN_POINT ( 'NONE',  ( 55.89999999999999147, 11.99999999999999822, -3.499999999999999556 ) ) ;
#37177 = CARTESIAN_POINT ( 'NONE',  ( -157.9449999999999932, -9.827790563157499189E-16, -8.024999999999991473 ) ) ;
#37178 = CARTESIAN_POINT ( 'NONE',  ( -142.6449999999999818, 4.716976649647091513, -6.492361379858946790 ) ) ;
#37179 = COLOUR_RGB ( '', 0.31764706, 0.68627451, 0.89019608) ;
#37180 = ORIENTED_EDGE ( 'NONE', *, *, #59095, .F. ) ;
#37181 = DIRECTION ( 'NONE',  ( -0.000000000000000000, -0.000000000000000000, -1.000000000000000000 ) ) ;
#37182 = DIRECTION ( 'NONE',  ( -1.084202172485504434E-16, 0.000000000000000000, -1.000000000000000000 ) ) ;
#37183 = PRESENTATION_LAYER_ASSIGNMENT (  '', '', ( #51767 ) ) ;
#37184 = CYLINDRICAL_SURFACE ( 'NONE', #31601, 0.5000000000000004441 ) ;
#37185 = CARTESIAN_POINT ( 'NONE',  ( -49.40499999999996561, -2.607480562269069768, 8.024999999999991473 ) ) ;
#37186 = FILL_AREA_STYLE_COLOUR ( '', #10225 ) ;
#37187 = CARTESIAN_POINT ( 'NONE',  ( -44.50000000000000000, 9.499999999999980460, 3.500000000000000000 ) ) ;
#37188 = CARTESIAN_POINT ( 'NONE',  ( -52.49292637653380922, -8.102448949553174629, 5.886773742842742685 ) ) ;
#37189 = DIRECTION ( 'NONE',  ( -1.000000000000000000, -0.000000000000000000, -0.000000000000000000 ) ) ;
#37190 = AXIS2_PLACEMENT_3D ( 'NONE', #62660, #41602, #3544 ) ;
#37191 = MECHANICAL_DESIGN_GEOMETRIC_PRESENTATION_REPRESENTATION (  '', ( #15833 ), #27018 ) ;
#37192 = DIRECTION ( 'NONE',  ( 1.665334536937734811E-16, -0.2829836251474255882, 0.9591247405308765961 ) ) ;
#37193 = FACE_OUTER_BOUND ( 'NONE', #22204, .T. ) ;
#37194 = AXIS2_PLACEMENT_3D ( 'NONE', #67088, #40368, #36140 ) ;
#37195 = CARTESIAN_POINT ( 'NONE',  ( 25.00000000000000000, 0.000000000000000000, -3.000000000000000000 ) ) ;
#37196 = CARTESIAN_POINT ( 'NONE',  ( 0.000000000000000000, 151.0570736234661524, -8.025000000000000355 ) ) ;
#37197 = AXIS2_PLACEMENT_3D ( 'NONE', #26826, #43095, #37120 ) ;
#37198 = FACE_OUTER_BOUND ( 'NONE', #16777, .T. ) ;
#37199 = CARTESIAN_POINT ( 'NONE',  ( 0.000000000000000000, -2.500000000000000000, 0.000000000000000000 ) ) ;
#37200 = EDGE_CURVE ( 'NONE', #67825, #21253, #10400, .T. ) ;
#37201 = DIRECTION ( 'NONE',  ( 0.000000000000000000, 0.000000000000000000, -1.000000000000000000 ) ) ;
#37202 = CARTESIAN_POINT ( 'NONE',  ( 44.00000000000000000, 21.74999999999998579, 4.000000000000000000 ) ) ;
#37203 = VERTEX_POINT ( 'NONE', #48757 ) ;
#37204 =( LENGTH_UNIT ( ) NAMED_UNIT ( * ) SI_UNIT ( .MILLI., .METRE. ) );
#37205 = AXIS2_PLACEMENT_3D ( 'NONE', #61773, #23817, #35066 ) ;
#37206 = CARTESIAN_POINT ( 'NONE',  ( 4.716976649647096842, 110.8570736234661496, 6.492361379858953896 ) ) ;
#37207 = AXIS2_PLACEMENT_3D ( 'NONE', #52990, #20976, #10771 ) ;
#37208 = CARTESIAN_POINT ( 'NONE',  ( 66.74999999999998579, 34.24999999999999289, -4.000000000000000000 ) ) ;
#37209 = FACE_OUTER_BOUND ( 'NONE', #26021, .T. ) ;
#37210 =( GEOMETRIC_REPRESENTATION_CONTEXT ( 3 ) GLOBAL_UNCERTAINTY_ASSIGNED_CONTEXT ( ( #26239 ) ) GLOBAL_UNIT_ASSIGNED_CONTEXT ( ( #43170, #27598, #15704 ) ) REPRESENTATION_CONTEXT ( 'NONE', 'WORKASPACE' ) );
#37211 = ORIENTED_EDGE ( 'NONE', *, *, #43497, .T. ) ;
#37212 = ORIENTED_EDGE ( 'NONE', *, *, #33751, .F. ) ;
#37213 = CARTESIAN_POINT ( 'NONE',  ( -172.9429263765337907, 0.000000000000000000, 9.524999999999991473 ) ) ;
#37214 = DIRECTION ( 'NONE',  ( -0.000000000000000000, -1.000000000000000000, -0.000000000000000000 ) ) ;
#37215 = ADVANCED_FACE ( 'NONE', ( #16729 ), #27576, .F. ) ;
#37216 = CARTESIAN_POINT ( 'NONE',  ( -101.3929263765337794, 8.102448949553176405, 5.886773742842740909 ) ) ;
#37217 = ORIENTED_EDGE ( 'NONE', *, *, #62179, .F. ) ;
#37218 = CARTESIAN_POINT ( 'NONE',  ( 5.598654528085809545, 116.2549999999999812, -7.705886871421373741 ) ) ;
#37219 = CARTESIAN_POINT ( 'NONE',  ( -85.04292637653381348, -9.058813317711329915, -2.943386871421370898 ) ) ;
#37220 = DIRECTION ( 'NONE',  ( 0.000000000000000000, 0.000000000000000000, -1.000000000000000000 ) ) ;
#37221 = EDGE_CURVE ( 'NONE', #20613, #9417, #6106, .T. ) ;
#37222 = EDGE_CURVE ( 'NONE', #56906, #69443, #60624, .T. ) ;
#37223 = FILL_AREA_STYLE ('',( #9774 ) ) ;
#37224 = CARTESIAN_POINT ( 'NONE',  ( -101.0949999999999989, -2.607480562269071545, -8.024999999999991473 ) ) ;
#37225 = ORIENTED_EDGE ( 'NONE', *, *, #10279, .T. ) ;
#37226 = CARTESIAN_POINT ( 'NONE',  ( 8.255084434212841771, 153.3156119838025404, 1.257250715558700493 ) ) ;
#37227 = CARTESIAN_POINT ( 'NONE',  ( -140.7570736234661695, -5.598654528085801552, 7.705886871421367523 ) ) ;
#37228 = COLOUR_RGB ( '', 0.66274510, 0.83137255, 0.94901961) ;
#37229 = EDGE_CURVE ( 'NONE', #56118, #33883, #39927, .T. ) ;
#37230 = FACE_OUTER_BOUND ( 'NONE', #57542, .T. ) ;
#37231 = ORIENTED_EDGE ( 'NONE', *, *, #48092, .T. ) ;
#37232 = CARTESIAN_POINT ( 'NONE',  ( -8.437984349512095861, 156.6929263765338476, -5.166775262442723748E-16 ) ) ;
#37233 = B_SPLINE_CURVE_WITH_KNOTS ( 'NONE', 3,
 ( #41829, #24542, #14721, #52370, #36565, #9798 ),
 .UNSPECIFIED., .F., .F.,
 ( 4, 2, 4 ),
 ( 0.005386537104126978143, 0.008060814333094818568, 0.01073509156206266073 ),
 .UNSPECIFIED. ) ;
#37234 = PRESENTATION_STYLE_ASSIGNMENT (( #53031 ) ) ;
#37235 = CIRCLE ( 'NONE', #23729, 0.5000000000000004441 ) ;
#37236 = CARTESIAN_POINT ( 'NONE',  ( 6.667623377008403018, 2.231456886122029193, 6.451337545287477937 ) ) ;
#37237 = CARTESIAN_POINT ( 'NONE',  ( 71.62068965517239860, 36.41396814395972115, 9.500000000000000000 ) ) ;
#37238 = CIRCLE ( 'NONE', #52927, 7.000000000000000888 ) ;
#37239 = CARTESIAN_POINT ( 'NONE',  ( 20.51842522107655142, 114.9046575010689821, -10.00000000000000000 ) ) ;
#37240 = VERTEX_POINT ( 'NONE', #44521 ) ;
#37241 = DIRECTION ( 'NONE',  ( 0.000000000000000000, 0.000000000000000000, 1.000000000000000000 ) ) ;
#37242 = CARTESIAN_POINT ( 'NONE',  ( -8.082903768654761123, -1.417096231345241097, -1.759977097422839922E-15 ) ) ;
#37243 = CARTESIAN_POINT ( 'NONE',  ( 21.02379604162863558, 114.4999999999999574, 10.50000000000000000 ) ) ;
#37244 = DIRECTION ( 'NONE',  ( 1.000000000000000000, 0.000000000000000000, -0.000000000000000000 ) ) ;
#37245 = VECTOR ( 'NONE', #13537, 1000.000000000000000 ) ;
#37246 = DIRECTION ( 'NONE',  ( -1.000000000000000000, -1.224646799147353454E-16, 0.000000000000000000 ) ) ;
#37247 = AXIS2_PLACEMENT_3D ( 'NONE', #68479, #51261, #36512 ) ;
#37248 = CARTESIAN_POINT ( 'NONE',  ( -74.10000901193289735, 9.371467124235303814, 6.143012557965066733 ) ) ;
#37249 =( LENGTH_UNIT ( ) NAMED_UNIT ( * ) SI_UNIT ( .MILLI., .METRE. ) );
#37250 = CARTESIAN_POINT ( 'NONE',  ( -28.74999999999999645, -8.499999999999996447, 15.00000000000000178 ) ) ;
#37251 = CARTESIAN_POINT ( 'NONE',  ( -47.00571487472603138, -11.85301361210301607, 3.279042910798483312 ) ) ;
#37252 = ORIENTED_EDGE ( 'NONE', *, *, #24081, .T. ) ;
#37253 = ORIENTED_EDGE ( 'NONE', *, *, #17214, .F. ) ;
#37254 = PLANE ( 'NONE',  #48659 ) ;
#37255 = FACE_OUTER_BOUND ( 'NONE', #46987, .T. ) ;
#37256 = DIRECTION ( 'NONE',  ( 5.782411586589351722E-16, -1.000000000000000000, 0.000000000000000000 ) ) ;
#37257 = ORIENTED_EDGE ( 'NONE', *, *, #26051, .F. ) ;
#37258 = CARTESIAN_POINT ( 'NONE',  ( -153.5929263765342228, -3.094860106624985452, -9.524999999995230837 ) ) ;
#37259 = CARTESIAN_POINT ( 'NONE',  ( -172.1050000000000182, -6.826472737025115478, 4.959722759717900331 ) ) ;
#37260 = DIRECTION ( 'NONE',  ( 1.000000000000000000, 0.000000000000000000, 0.000000000000000000 ) ) ;
#37261 = CARTESIAN_POINT ( 'NONE',  ( -87.50000000000000000, -8.499999999999989342, 24.00000000000000000 ) ) ;
#37262 =( GEOMETRIC_REPRESENTATION_CONTEXT ( 3 ) GLOBAL_UNCERTAINTY_ASSIGNED_CONTEXT ( ( #2492 ) ) GLOBAL_UNIT_ASSIGNED_CONTEXT ( ( #53386, #28695, #62699 ) ) REPRESENTATION_CONTEXT ( 'NONE', 'WORKASPACE' ) );
#37263 = CARTESIAN_POINT ( 'NONE',  ( -46.55707362346617373, -1.166476076187852838E-15, -9.524999999999991473 ) ) ;
#37264 = CARTESIAN_POINT ( 'NONE',  ( -171.1449999999999818, -4.716976649647092401, 6.492361379858946790 ) ) ;
#37265 =( GEOMETRIC_REPRESENTATION_CONTEXT ( 3 ) GLOBAL_UNCERTAINTY_ASSIGNED_CONTEXT ( ( #27698 ) ) GLOBAL_UNIT_ASSIGNED_CONTEXT ( ( #36773, #58881, #26824 ) ) REPRESENTATION_CONTEXT ( 'NONE', 'WORKASPACE' ) );
#37266 = VERTEX_POINT ( 'NONE', #65925 ) ;
#37267 = CARTESIAN_POINT ( 'NONE',  ( 60.00000000000000000, 1.797044900979284448E-15, 12.00000000000000000 ) ) ;
#37268 = CARTESIAN_POINT ( 'NONE',  ( -40.70406133565712992, -11.89285714285713880, 3.265330863013266693 ) ) ;
#37269 = CARTESIAN_POINT ( 'NONE',  ( -15.00000000000000000, 10.90871211463577239, 5.000000000000000888 ) ) ;
#37270 = CARTESIAN_POINT ( 'NONE',  ( -78.65499999999998693, -7.632228543268600340, -2.479861379858950166 ) ) ;
#37271 = CARTESIAN_POINT ( 'NONE',  ( 4.041451884327376121, 7.000000000000007105, 7.500000000000000000 ) ) ;
#37273 = FILL_AREA_STYLE_COLOUR ( '', #60700 ) ;
#37272 =( GEOMETRIC_REPRESENTATION_CONTEXT ( 3 ) GLOBAL_UNCERTAINTY_ASSIGNED_CONTEXT ( ( #29795 ) ) GLOBAL_UNIT_ASSIGNED_CONTEXT ( ( #31771, #17006, #44465 ) ) REPRESENTATION_CONTEXT ( 'NONE', 'WORKASPACE' ) );
#37274 = CIRCLE ( 'NONE', #1196, 23.00000000000000000 ) ;
#37275 = CARTESIAN_POINT ( 'NONE',  ( -75.23309145305536560, 36.13215102747564345, -9.842748219394650278 ) ) ;
#37276 = CARTESIAN_POINT ( 'NONE',  ( -80.69499999999999318, -8.437984349512086979, 5.166775262442717831E-16 ) ) ;
#37277 = CARTESIAN_POINT ( 'NONE',  ( -3.094860106618434248, 135.9050000000000011, 9.525000000000000355 ) ) ;
#37278 = CARTESIAN_POINT ( 'NONE',  ( -134.7570736234661695, -5.598654528085801552, 7.705886871421367523 ) ) ;
#37279 = CARTESIAN_POINT ( 'NONE',  ( 41.49999999999997868, 9.999999999999980460, -3.000000000000000444 ) ) ;
#37280 = COLOUR_RGB ( '', 0.40784314, 0.44705882, 0.49803922) ;
#37281 = FACE_OUTER_BOUND ( 'NONE', #6784, .T. ) ;
#37282 = FILL_AREA_STYLE ('',( #63954 ) ) ;
#37284 = ORIENTED_EDGE ( 'NONE', *, *, #51797, .T. ) ;
#37283 =( GEOMETRIC_REPRESENTATION_CONTEXT ( 3 ) GLOBAL_UNCERTAINTY_ASSIGNED_CONTEXT ( ( #43841 ) ) GLOBAL_UNIT_ASSIGNED_CONTEXT ( ( #32162, #37139, #48733 ) ) REPRESENTATION_CONTEXT ( 'NONE', 'WORKASPACE' ) );
#37285 = PRODUCT_DEFINITION_SHAPE ( 'NONE', 'NONE',  #43868 ) ;
#37286 = DIRECTION ( 'NONE',  ( 0.000000000000000000, 0.000000000000000000, 1.000000000000000000 ) ) ;
#37287 = MECHANICAL_DESIGN_GEOMETRIC_PRESENTATION_REPRESENTATION (  '', ( #50757 ), #2379 ) ;
#37288 = ADVANCED_FACE ( 'NONE', ( #1844 ), #17753, .T. ) ;
#37290 = SURFACE_STYLE_FILL_AREA ( #10171 ) ;
#37289 = FACE_OUTER_BOUND ( 'NONE', #51015, .T. ) ;
#37291 = EDGE_LOOP ( 'NONE', ( #39726, #36816, #59603, #227 ) ) ;
#37292 = EDGE_LOOP ( 'NONE', ( #23278, #36701, #32012, #42258 ) ) ;
#37293 = CARTESIAN_POINT ( 'NONE',  ( -45.64578147489630311, 8.378235220106981629, -6.482771786488845223 ) ) ;
#37294 = CIRCLE ( 'NONE', #2381, 10.00000000000000000 ) ;
#37295 = CARTESIAN_POINT ( 'NONE',  ( 8.437984349512095861, 131.1929263765338192, 1.550032578732816828E-15 ) ) ;
#37296 = ADVANCED_FACE ( 'NONE', ( #45559 ), #49760, .T. ) ;
#37297 =( GEOMETRIC_REPRESENTATION_CONTEXT ( 3 ) GLOBAL_UNCERTAINTY_ASSIGNED_CONTEXT ( ( #13786 ) ) GLOBAL_UNIT_ASSIGNED_CONTEXT ( ( #5457, #26907, #64913 ) ) REPRESENTATION_CONTEXT ( 'NONE', 'WORKASPACE' ) );
#37298 =( NAMED_UNIT ( * ) SI_UNIT ( $, .STERADIAN. ) SOLID_ANGLE_UNIT ( ) );
#37299 = AXIS2_PLACEMENT_3D ( 'NONE', #57481, #67340, #51505 ) ;
#37300 = CYLINDRICAL_SURFACE ( 'NONE', #40851, 0.2500000000000002220 ) ;
#37301 = DIRECTION ( 'NONE',  ( 0.000000000000000000, 0.000000000000000000, -1.000000000000000000 ) ) ;
#37302 = ORIENTED_EDGE ( 'NONE', *, *, #57270, .T. ) ;
#37303 = CARTESIAN_POINT ( 'NONE',  ( -120.8049999999999784, -8.437984349512086979, 5.166775262442717831E-16 ) ) ;
#37304 = ORIENTED_EDGE ( 'NONE', *, *, #69358, .F. ) ;
#37305 = ORIENTED_EDGE ( 'NONE', *, *, #13500, .F. ) ;
#37306 = DIRECTION ( 'NONE',  ( -0.8660254037844384856, -0.5000000000000004441, 0.000000000000000000 ) ) ;
#37307 = DIRECTION ( 'NONE',  ( 0.000000000000000000, 0.000000000000000000, -1.000000000000000000 ) ) ;
#37308 = ORIENTED_EDGE ( 'NONE', *, *, #31942, .F. ) ;
#37309 = CIRCLE ( 'NONE', #38418, 0.2500000000000002220 ) ;
#37310 = ADVANCED_FACE ( 'NONE', ( #65574 ), #18442, .T. ) ;
#37311 =( LENGTH_UNIT ( ) NAMED_UNIT ( * ) SI_UNIT ( .MILLI., .METRE. ) );
#37312 =( BOUNDED_CURVE ( )  B_SPLINE_CURVE ( 2, ( #11869, #22083, #43247, #32989, #27329, #54424, #44624, #33666, #6244, #55108, #44278 ),
 .UNSPECIFIED., .F., .F. ) 
 B_SPLINE_CURVE_WITH_KNOTS ( ( 3, 2, 2, 2, 2, 3 ),
 ( 0.7647058823529415683, 0.7705882352941180180, 0.7764705882352943567, 0.7823529411764706953, 0.7882352941176470340, 0.7941176470588233727 ),
 .UNSPECIFIED. ) 
 CURVE ( )  GEOMETRIC_REPRESENTATION_ITEM ( )  RATIONAL_B_SPLINE_CURVE ( ( 0.9999999999999963363, 0.9510565162951571949, 1.000000000000000000, 0.9510565162951535312, 1.000000000000000000, 0.9510565162951535312, 1.000000000000000000, 0.9510565162951535312, 1.000000000000000000, 0.9510565162951544194, 0.9999999999999991118 ) ) 
 REPRESENTATION_ITEM ( '' )  );
#37313 = CARTESIAN_POINT ( 'NONE',  ( -8.102448949553181734, 148.8950000000000102, -5.886773742842749790 ) ) ;
#37314 = CYLINDRICAL_SURFACE ( 'NONE', #4794, 1.000000000000000888 ) ;
#37315 = ORIENTED_EDGE ( 'NONE', *, *, #48140, .T. ) ;
#37316 = STYLED_ITEM ( 'NONE', ( #56211 ), #25190 ) ;
#37317 = CARTESIAN_POINT ( 'NONE',  ( -5.196152422706636465, 1.107695154586737063, 9.000000000000001776 ) ) ;
#37318 = CARTESIAN_POINT ( 'NONE',  ( 8.102448949553181734, 146.1049999999999898, -5.886773742842746238 ) ) ;
#37319 = SURFACE_STYLE_FILL_AREA ( #10884 ) ;
#37320 = EDGE_CURVE ( 'NONE', #2072, #9170, #39225, .T. ) ;
#37321 = DIRECTION ( 'NONE',  ( 0.000000000000000000, 1.000000000000000000, 0.000000000000000000 ) ) ;
#37322 = ORIENTED_EDGE ( 'NONE', *, *, #30807, .F. ) ;
#37323 = CARTESIAN_POINT ( 'NONE',  ( -7.632228543268608334, 129.8429263765338249, 2.479861379858952830 ) ) ;
#37324 = CARTESIAN_POINT ( 'NONE',  ( 72.50000000000000000, 14.49137674618942562, -10.00000000000000000 ) ) ;
#37325 = CARTESIAN_POINT ( 'NONE',  ( 1.999798566743339334, 49.09558629977726696, -2.000000000000000000 ) ) ;
#37326 = AXIS2_PLACEMENT_3D ( 'NONE', #27763, #66468, #59807 ) ;
#37327 = FACE_OUTER_BOUND ( 'NONE', #44092, .T. ) ;
#37328 =( NAMED_UNIT ( * ) SI_UNIT ( $, .STERADIAN. ) SOLID_ANGLE_UNIT ( ) );
#37329 = VERTEX_POINT ( 'NONE', #23353 ) ;
#37330 = DIRECTION ( 'NONE',  ( 0.000000000000000000, -1.000000000000000000, 0.000000000000000000 ) ) ;
#37331 = ORIENTED_EDGE ( 'NONE', *, *, #43039, .F. ) ;
#37332 = CARTESIAN_POINT ( 'NONE',  ( -58.34292637653379643, -9.058813317711329915, 2.943386871421371787 ) ) ;
#37333 = CARTESIAN_POINT ( 'NONE',  ( -6.239160159721279797, 3.193457606803199678, 3.307663659028042824E-15 ) ) ;
#37335 = CARTESIAN_POINT ( 'NONE',  ( -144.8049999999999216, -8.437984349512085203, 5.166775262442717831E-16 ) ) ;
#37334 = CIRCLE ( 'NONE', #6944, 0.5000000000000004441 ) ;
#37336 = CARTESIAN_POINT ( 'NONE',  ( 28.00000000000002842, 38.70020753820971748, 89.00000000000000000 ) ) ;
#37337 = CARTESIAN_POINT ( 'NONE',  ( 7.000000000000017764, 42.74314482547740113, -27.71473342867655987 ) ) ;
#37338 = COLOUR_RGB ( '', 0.66274510, 0.83137255, 0.94901961) ;
#37339 = DIRECTION ( 'NONE',  ( 1.000000000000000000, 1.867193268687763645E-14, 0.000000000000000000 ) ) ;
#37340 = FILL_AREA_STYLE_COLOUR ( '', #65279 ) ;
#37341 = SURFACE_STYLE_USAGE ( .BOTH. , #31660 ) ;
#37342 = ORIENTED_EDGE ( 'NONE', *, *, #27135, .F. ) ;
#37343 = CIRCLE ( 'NONE', #1264, 5.000000000000004441 ) ;
#37344 = ORIENTED_EDGE ( 'NONE', *, *, #32560, .T. ) ;
#37345 = CARTESIAN_POINT ( 'NONE',  ( 22.25000000000000711, 34.24999999999999289, 4.000000000000000000 ) ) ;
#37346 = STYLED_ITEM ( 'NONE', ( #27152 ), #11833 ) ;
#37347 = SPHERICAL_SURFACE ( 'NONE', #63770, 0.2500000000000000000 ) ;
#37348 = CARTESIAN_POINT ( 'NONE',  ( -63.65499999999998693, -7.632228543268600340, -2.479861379858950166 ) ) ;
#37349 = EDGE_LOOP ( 'NONE', ( #59757, #17016, #16195, #68408 ) ) ;
#37350 = DIRECTION ( 'NONE',  ( 0.000000000000000000, 0.000000000000000000, -1.000000000000000000 ) ) ;
#37351 = CARTESIAN_POINT ( 'NONE',  ( -45.91547277936962956, 9.430195807687216103, 6.000000000000000888 ) ) ;
#37352 = CIRCLE ( 'NONE', #26038, 0.2500000000000002220 ) ;
#37353 =( LENGTH_UNIT ( ) NAMED_UNIT ( * ) SI_UNIT ( .MILLI., .METRE. ) );
#37354 = FACE_OUTER_BOUND ( 'NONE', #28196, .T. ) ;
#37355 = CYLINDRICAL_SURFACE ( 'NONE', #1610, 0.2500000000000002220 ) ;
#37356 = ORIENTED_EDGE ( 'NONE', *, *, #63543, .T. ) ;
#37357 = EDGE_CURVE ( 'NONE', #31792, #42973, #10640, .T. ) ;
#37358 = TOROIDAL_SURFACE ( 'NONE', #46330, 9.499999999999996447, 0.5000000000000000000 ) ;
#37359 = DIRECTION ( 'NONE',  ( -0.000000000000000000, -0.000000000000000000, -1.000000000000000000 ) ) ;
#37360 = FILL_AREA_STYLE ('',( #37712 ) ) ;
#37361 = CARTESIAN_POINT ( 'NONE',  ( 61.99999999999998579, 33.99999999999999289, 4.000000000000000000 ) ) ;
#37362 = AXIS2_PLACEMENT_3D ( 'NONE', #19412, #40910, #62328 ) ;
#37363 = AXIS2_PLACEMENT_3D ( 'NONE', #18613, #29121, #49239 ) ;
#37364 = CARTESIAN_POINT ( 'NONE',  ( -113.6949999999999790, -8.437984349512086979, 5.166775262442717831E-16 ) ) ;
#37365 = CARTESIAN_POINT ( 'NONE',  ( 8.102448949553181734, 144.3950000000000102, 5.886773742842750679 ) ) ;
#37366 = CARTESIAN_POINT ( 'NONE',  ( -86.09499999999997044, -2.607480562269071545, -8.024999999999991473 ) ) ;
#37367 = AXIS2_PLACEMENT_3D ( 'NONE', #64018, #15865, #16221 ) ;
#37368 =( LENGTH_UNIT ( ) NAMED_UNIT ( * ) SI_UNIT ( .MILLI., .METRE. ) );
#37369 = CARTESIAN_POINT ( 'NONE',  ( 23.71231517720798010, 117.4999999999999716, 9.500000000000000000 ) ) ;
#37370 =( GEOMETRIC_REPRESENTATION_CONTEXT ( 3 ) GLOBAL_UNCERTAINTY_ASSIGNED_CONTEXT ( ( #44151 ) ) GLOBAL_UNIT_ASSIGNED_CONTEXT ( ( #5018, #3589, #57810 ) ) REPRESENTATION_CONTEXT ( 'NONE', 'WORKASPACE' ) );
#37371 = DIRECTION ( 'NONE',  ( 0.000000000000000000, 0.000000000000000000, -1.000000000000000000 ) ) ;
#37372 = ORIENTED_EDGE ( 'NONE', *, *, #61600, .F. ) ;
#37373 = CARTESIAN_POINT ( 'NONE',  ( -136.9429263765338192, 0.000000000000000000, 9.524999999999991473 ) ) ;
#37374 =( NAMED_UNIT ( * ) PLANE_ANGLE_UNIT ( ) SI_UNIT ( $, .RADIAN. ) );
#37375 = SPHERICAL_SURFACE ( 'NONE', #68065, 0.2500000000000000000 ) ;
#37376 = CARTESIAN_POINT ( 'NONE',  ( -146.0949999999999989, -2.607480562269071545, -8.024999999999991473 ) ) ;
#37377 =( LENGTH_UNIT ( ) NAMED_UNIT ( * ) SI_UNIT ( .MILLI., .METRE. ) );
#37378 = CIRCLE ( 'NONE', #23855, 0.4999999999999994449 ) ;
#37379 = ADVANCED_FACE ( 'NONE', ( #2171 ), #12439, .T. ) ;
#37380 = EDGE_CURVE ( 'NONE', #19151, #2325, #61190, .T. ) ;
#37381 = CARTESIAN_POINT ( 'NONE',  ( -46.94499999999998607, -9.827790563157499189E-16, -8.024999999999991473 ) ) ;
#37382 =( LENGTH_UNIT ( ) NAMED_UNIT ( * ) SI_UNIT ( .MILLI., .METRE. ) );
#37383 = ORIENTED_EDGE ( 'NONE', *, *, #53850, .T. ) ;
#37384 = ORIENTED_EDGE ( 'NONE', *, *, #2748, .T. ) ;
#37385 = MECHANICAL_DESIGN_GEOMETRIC_PRESENTATION_REPRESENTATION (  '', ( #12609 ), #53060 ) ;
#37386 = DIRECTION ( 'NONE',  ( 0.000000000000000000, 0.000000000000000000, 1.000000000000000000 ) ) ;
#37387 = CIRCLE ( 'NONE', #53064, 13.76969600708473074 ) ;
#37388 = EDGE_CURVE ( 'NONE', #6724, #25927, #54402, .T. ) ;
#37389 = DIRECTION ( 'NONE',  ( 1.000000000000000000, 0.000000000000000000, 0.000000000000000000 ) ) ;
#37390 = CARTESIAN_POINT ( 'NONE',  ( -45.72743705490865551, 8.702587636786784486, 6.424237564332099026 ) ) ;
#37391 = CIRCLE ( 'NONE', #14919, 16.94999999999999218 ) ;
#37392 = CARTESIAN_POINT ( 'NONE',  ( -58.01150860321133251, -8.499999999997220002, -0.3572867894539443201 ) ) ;
#37393 = EDGE_LOOP ( 'NONE', ( #25596, #17432, #20292, #51546 ) ) ;
#37394 = CARTESIAN_POINT ( 'NONE',  ( -149.0049999999999386, 6.826472737025115478, 4.959722759717899443 ) ) ;
#37395 = ORIENTED_EDGE ( 'NONE', *, *, #39111, .T. ) ;
#37396 = FILL_AREA_STYLE_COLOUR ( '', #1967 ) ;
#37397 = DIRECTION ( 'NONE',  ( 0.000000000000000000, 0.000000000000000000, 1.000000000000000000 ) ) ;
#37398 = PRESENTATION_LAYER_ASSIGNMENT (  '', '', ( #19356 ) ) ;
#37399 = VERTEX_POINT ( 'NONE', #18087 ) ;
#37400 = EDGE_CURVE ( 'NONE', #9509, #22236, #28579, .T. ) ;
#37401 = SURFACE_SIDE_STYLE ('',( #15921 ) ) ;
#37402 = AXIS2_PLACEMENT_3D ( 'NONE', #62003, #24367, #67645 ) ;
#37403 = CARTESIAN_POINT ( 'NONE',  ( -58.94292637653381206, 0.000000000000000000, 9.524999999999991473 ) ) ;
#37404 = CARTESIAN_POINT ( 'NONE',  ( 5.598654528085809545, 121.1449999999999818, -7.705886871421373741 ) ) ;
#37405 = DIRECTION ( 'NONE',  ( -0.000000000000000000, -0.000000000000000000, 1.000000000000000000 ) ) ;
#37406 =( GEOMETRIC_REPRESENTATION_CONTEXT ( 3 ) GLOBAL_UNCERTAINTY_ASSIGNED_CONTEXT ( ( #5989 ) ) GLOBAL_UNIT_ASSIGNED_CONTEXT ( ( #54474, #6286, #59755 ) ) REPRESENTATION_CONTEXT ( 'NONE', 'WORKASPACE' ) );
#37407 = ORIENTED_EDGE ( 'NONE', *, *, #7213, .F. ) ;
#37408 = CARTESIAN_POINT ( 'NONE',  ( -45.00000000000000000, 10.49999999999998579, 3.000000000000000000 ) ) ;
#37409 = CARTESIAN_POINT ( 'NONE',  ( 5.598654528085805993, 121.3549999999999898, 7.705886871421374629 ) ) ;
#37410 = CARTESIAN_POINT ( 'NONE',  ( -65.15499999999998693, 7.632228543268600340, 2.479861379858949277 ) ) ;
#37412 = STYLED_ITEM ( 'NONE', ( #19949 ), #6906 ) ;
#37411 = CARTESIAN_POINT ( 'NONE',  ( -116.8449999999999847, -7.632228543268599452, 2.479861379858951054 ) ) ;
#37413 = ADVANCED_FACE ( 'NONE', ( #56050 ), #50793, .F. ) ;
#37414 = LINE ( 'NONE', #37763, #12738 ) ;
#37415 = ORIENTED_EDGE ( 'NONE', *, *, #11363, .T. ) ;
#37416 = CARTESIAN_POINT ( 'NONE',  ( 9.058813317711337021, 148.6549999999999727, 2.943386871421375783 ) ) ;
#37417 = PRESENTATION_STYLE_ASSIGNMENT (( #9337 ) ) ;
#37418 =( LENGTH_UNIT ( ) NAMED_UNIT ( * ) SI_UNIT ( .MILLI., .METRE. ) );
#37419 = TOROIDAL_SURFACE ( 'NONE', #8153, 1.000000000000000000, 0.5000000000000000000 ) ;
#37420 = FILL_AREA_STYLE_COLOUR ( '', #42963 ) ;
#37421 = FACE_BOUND ( 'NONE', #40165, .T. ) ;
#37422 = MECHANICAL_DESIGN_GEOMETRIC_PRESENTATION_REPRESENTATION (  '', ( #62044 ), #19383 ) ;
#37423 = CARTESIAN_POINT ( 'NONE',  ( -75.50000000000000000, -8.499999999999991118, 3.000000000000000000 ) ) ;
#37424 = ORIENTED_EDGE ( 'NONE', *, *, #25278, .F. ) ;
#37425 = LINE ( 'NONE', #4276, #22103 ) ;
#37426 = CARTESIAN_POINT ( 'NONE',  ( -180.3549999999999898, -4.716976649647093289, -6.492361379858945902 ) ) ;
#37427 = ORIENTED_EDGE ( 'NONE', *, *, #1701, .F. ) ;
#37428 = CYLINDRICAL_SURFACE ( 'NONE', #36251, 0.5000000000000004441 ) ;
#37429 =( BOUNDED_CURVE ( )  B_SPLINE_CURVE ( 2, ( #46917, #52514, #14170, #46207, #67629, #51115, #4259, #14873, #2859, #3195, #30304 ),
 .UNSPECIFIED., .F., .F. ) 
 B_SPLINE_CURVE_WITH_KNOTS ( ( 3, 2, 2, 2, 2, 3 ),
 ( 0.9021739130434782705, 0.9043478260869565188, 0.9065217391304347672, 0.9086956521739130155, 0.9108695652173912638, 0.9130434782608695121 ),
 .UNSPECIFIED. ) 
 CURVE ( )  GEOMETRIC_REPRESENTATION_ITEM ( )  RATIONAL_B_SPLINE_CURVE ( ( 1.000000000000000000, 0.9510565162951535312, 1.000000000000000000, 0.9510565162951535312, 1.000000000000000000, 0.9510565162951535312, 1.000000000000000000, 0.9510565162951535312, 1.000000000000000000, 0.9510565162951535312, 1.000000000000000000 ) ) 
 REPRESENTATION_ITEM ( '' )  );
#37430 = AXIS2_PLACEMENT_3D ( 'NONE', #5348, #26790, #1050 ) ;
#37431 = CARTESIAN_POINT ( 'NONE',  ( -5.196152422706633800, -9.000000000000005329, 7.500000000000000000 ) ) ;
#37432 =( GEOMETRIC_REPRESENTATION_CONTEXT ( 3 ) GLOBAL_UNCERTAINTY_ASSIGNED_CONTEXT ( ( #60696 ) ) GLOBAL_UNIT_ASSIGNED_CONTEXT ( ( #67726, #1896, #50505 ) ) REPRESENTATION_CONTEXT ( 'NONE', 'WORKASPACE' ) );
#37433 = FILL_AREA_STYLE ('',( #63746 ) ) ;
#37434 = CARTESIAN_POINT ( 'NONE',  ( -44.99154893936432842, 9.591540374752312914, 3.105576841506459296 ) ) ;
#37435 = ORIENTED_EDGE ( 'NONE', *, *, #56368, .F. ) ;
#37436 = AXIS2_PLACEMENT_3D ( 'NONE', #3495, #68615, #24996 ) ;
#37437 = PRESENTATION_STYLE_ASSIGNMENT (( #47651 ) ) ;
#37438 = PRESENTATION_STYLE_ASSIGNMENT (( #53889 ) ) ;
#37439 = CARTESIAN_POINT ( 'NONE',  ( -93.20499999999998408, -2.607480562269071545, -8.024999999999991473 ) ) ;
#37440 = EDGE_LOOP ( 'NONE', ( #19955, #28600, #52143, #26919 ) ) ;
#37441 = DIRECTION ( 'NONE',  ( 0.000000000000000000, 0.000000000000000000, -1.000000000000000000 ) ) ;
#37442 = PRESENTATION_STYLE_ASSIGNMENT (( #31744 ) ) ;
#37443 = CARTESIAN_POINT ( 'NONE',  ( -132.5070736234661410, 8.102448949553176405, 5.886773742842740909 ) ) ;
#37444 = PRESENTATION_LAYER_ASSIGNMENT (  '', '', ( #3644 ) ) ;
#37445 = AXIS2_PLACEMENT_3D ( 'NONE', #58966, #16440, #5821 ) ;
#37446 = FILL_AREA_STYLE ('',( #3970 ) ) ;
#37447 = CARTESIAN_POINT ( 'NONE',  ( -64.40707362346617515, 3.094860106618428031, -9.524999999999993250 ) ) ;
#37448 = EDGE_CURVE ( 'NONE', #25818, #67895, #22993, .T. ) ;
#37449 = AXIS2_PLACEMENT_3D ( 'NONE', #4192, #69622, #15503 ) ;
#37450 = DIRECTION ( 'NONE',  ( -0.000000000000000000, 0.000000000000000000, -1.000000000000000000 ) ) ;
#37451 = ORIENTED_EDGE ( 'NONE', *, *, #56368, .T. ) ;
#37453 = FACE_OUTER_BOUND ( 'NONE', #63652, .T. ) ;
#37452 = COLOUR_RGB ( '', 0.09019608, 0.27058824, 0.51372549) ;
#37454 = FILL_AREA_STYLE_COLOUR ( '', #7728 ) ;
#37455 = CARTESIAN_POINT ( 'NONE',  ( -111.3549999999999898, -4.716976649647093289, -6.492361379858945902 ) ) ;
#37456 = CARTESIAN_POINT ( 'NONE',  ( -8.102448949553181734, 122.4949999999999903, 5.886773742842747126 ) ) ;
#37457 = STYLED_ITEM ( 'NONE', ( #47174 ), #22837 ) ;
#37458 = CARTESIAN_POINT ( 'NONE',  ( -116.8449999999999847, -7.632228543268599452, 2.479861379858951054 ) ) ;
#37459 = MECHANICAL_DESIGN_GEOMETRIC_PRESENTATION_REPRESENTATION (  '', ( #25045 ), #7067 ) ;
#37460 = CARTESIAN_POINT ( 'NONE',  ( 48.49999999999999289, 24.74999999999998579, 4.000000000000000000 ) ) ;
#37461 = AXIS2_PLACEMENT_3D ( 'NONE', #60206, #17666, #55623 ) ;
#37463 = FILL_AREA_STYLE ('',( #53579 ) ) ;
#37462 = CARTESIAN_POINT ( 'NONE',  ( 9.250000000000003553, 25.24999999999998934, -4.000000000000000000 ) ) ;
#37464 = EDGE_CURVE ( 'NONE', #56343, #23940, #329, .T. ) ;
#37465 = EDGE_LOOP ( 'NONE', ( #56649, #2263, #66158, #47092 ) ) ;
#37466 = CARTESIAN_POINT ( 'NONE',  ( -158.3929263765338078, 8.102448949553176405, 5.886773742842740909 ) ) ;
#37467 = CARTESIAN_POINT ( 'NONE',  ( -174.5949999999999989, 2.607480562269073321, 8.024999999999991473 ) ) ;
#37468 = AXIS2_PLACEMENT_3D ( 'NONE', #4448, #11128, #48127 ) ;
#37469 = ADVANCED_FACE ( 'NONE', ( #22545 ), #11640, .T. ) ;
#37470 = AXIS2_PLACEMENT_3D ( 'NONE', #60141, #54160, #54508 ) ;
#37471 = EDGE_CURVE ( 'NONE', #42847, #67099, #49633, .T. ) ;
#37472 = CARTESIAN_POINT ( 'NONE',  ( -40.78947368421051323, 108.1536491499103505, 3.000000000000000000 ) ) ;
#37473 = FACE_OUTER_BOUND ( 'NONE', #48703, .T. ) ;
#37474 =( NAMED_UNIT ( * ) PLANE_ANGLE_UNIT ( ) SI_UNIT ( $, .RADIAN. ) );
#37475 = DIRECTION ( 'NONE',  ( 0.000000000000000000, 0.6449798928094537809, 0.7641995406119435064 ) ) ;
#37476 = EDGE_LOOP ( 'NONE', ( #42315, #32498, #66090, #49751 ) ) ;
#37477 = CARTESIAN_POINT ( 'NONE',  ( -80.09292637653379643, 3.094860106618433360, 9.524999999999991473 ) ) ;
#37478 = CARTESIAN_POINT ( 'NONE',  ( -195.0000000000000000, 0.000000000000000000, 0.000000000000000000 ) ) ;
#37479 = PRESENTATION_LAYER_ASSIGNMENT (  '', '', ( #8202 ) ) ;
#37480 = EDGE_CURVE ( 'NONE', #246, #23187, #38429, .T. ) ;
#37481 = FACE_OUTER_BOUND ( 'NONE', #25138, .T. ) ;
#37482 = EDGE_CURVE ( 'NONE', #32568, #6742, #9443, .T. ) ;
#37483 = CARTESIAN_POINT ( 'NONE',  ( -182.7549999999999955, 4.716976649647091513, -6.492361379858946790 ) ) ;
#37484 = EDGE_LOOP ( 'NONE', ( #64785, #68670, #31977, #27787 ) ) ;
#37485 = SURFACE_STYLE_USAGE ( .BOTH. , #15646 ) ;
#37486 = CARTESIAN_POINT ( 'NONE',  ( 71.62068965517239860, 36.41396814395972115, 7.000000000000000000 ) ) ;
#37487 = CARTESIAN_POINT ( 'NONE',  ( -49.12162162162162105, 13.70805908423323238, -10.00000000000000000 ) ) ;
#37488 = VECTOR ( 'NONE', #26512, 1000.000000000000000 ) ;
#37489 = CARTESIAN_POINT ( 'NONE',  ( 0.000000000000000000, 142.0570736234661524, -8.025000000000000355 ) ) ;
#37490 = CIRCLE ( 'NONE', #52012, 0.5000000000000004441 ) ;
#37491 = VERTEX_POINT ( 'NONE', #27786 ) ;
#37492 = DIRECTION ( 'NONE',  ( -1.000000000000000000, 0.000000000000000000, 0.000000000000000000 ) ) ;
#37493 = CARTESIAN_POINT ( 'NONE',  ( -89.60499999999997556, 6.826472737025113702, -4.959722759717902107 ) ) ;
#37494 = DIRECTION ( 'NONE',  ( 0.000000000000000000, 0.7431448254773929118, -0.6691306063588596809 ) ) ;
#37495 = ORIENTED_EDGE ( 'NONE', *, *, #58442, .T. ) ;
#37496 = CARTESIAN_POINT ( 'NONE',  ( 75.00000000000000000, 19.92376017841765545, -7.000000000000002665 ) ) ;
#37497 = EDGE_CURVE ( 'NONE', #28799, #1094, #39852, .T. ) ;
#37498 = CARTESIAN_POINT ( 'NONE',  ( -34.18098754654297267, -10.00147920973261861, -3.272174344843567173 ) ) ;
#37499 = DIRECTION ( 'NONE',  ( 7.703719777548942317E-32, -1.000000000000000000, -0.000000000000000000 ) ) ;
#37500 = EDGE_LOOP ( 'NONE', ( #49389, #10349, #36438, #31397 ) ) ;
#37501 = CIRCLE ( 'NONE', #23931, 4.499999999999976019 ) ;
#37502 = EDGE_CURVE ( 'NONE', #42518, #66900, #60031, .T. ) ;
#37503 = CARTESIAN_POINT ( 'NONE',  ( -69.29499999999995907, -2.607480562269069768, 8.024999999999991473 ) ) ;
#37504 = EDGE_LOOP ( 'NONE', ( #61215, #5551 ) ) ;
#37505 = DIRECTION ( 'NONE',  ( -0.000000000000000000, -0.000000000000000000, 1.000000000000000000 ) ) ;
#37506 = CIRCLE ( 'NONE', #63263, 1.000000000000000888 ) ;
#37507 = DIRECTION ( 'NONE',  ( 0.000000000000000000, 1.000000000000000000, -0.000000000000000000 ) ) ;
#37508 = DIRECTION ( 'NONE',  ( -4.449603764765679692E-17, -0.9396926207859105373, -0.3420201433256630508 ) ) ;
#37509 = AXIS2_PLACEMENT_3D ( 'NONE', #3824, #57676, #58035 ) ;
#37510 = ORIENTED_EDGE ( 'NONE', *, *, #59551, .F. ) ;
#37511 = VECTOR ( 'NONE', #25067, 1000.000000000000000 ) ;
#37512 = VECTOR ( 'NONE', #27437, 1000.000000000000114 ) ;
#37513 = DIRECTION ( 'NONE',  ( 0.000000000000000000, 0.000000000000000000, -1.000000000000000000 ) ) ;
#37514 = CARTESIAN_POINT ( 'NONE',  ( 1.000000000000000000, 0.000000000000000000, 79.00402776293826435 ) ) ;
#37515 = CARTESIAN_POINT ( 'NONE',  ( -125.7550000000000097, 4.716976649647091513, -6.492361379858946790 ) ) ;
#37516 = ORIENTED_EDGE ( 'NONE', *, *, #11768, .T. ) ;
#37517 = ORIENTED_EDGE ( 'NONE', *, *, #61606, .F. ) ;
#37518 = DIRECTION ( 'NONE',  ( 0.000000000000000000, 1.000000000000000000, 0.000000000000000000 ) ) ;
#37519 =( LENGTH_UNIT ( ) NAMED_UNIT ( * ) SI_UNIT ( .MILLI., .METRE. ) );
#37520 = SURFACE_STYLE_USAGE ( .BOTH. , #1139 ) ;
#37521 = CARTESIAN_POINT ( 'NONE',  ( -155.3070736234662093, -10.01517768586948698, 6.132527647946031529E-16 ) ) ;
#37522 = CARTESIAN_POINT ( 'NONE',  ( 5.598654528085809545, 124.1449999999999960, -7.705886871421373741 ) ) ;
#37523 = CARTESIAN_POINT ( 'NONE',  ( -95.45707362346617231, -9.058813317711329915, 2.943386871421371787 ) ) ;
#37524 = AXIS2_PLACEMENT_3D ( 'NONE', #46067, #41840, #4132 ) ;
#37525 = CIRCLE ( 'NONE', #7137, 9.000000000000000000 ) ;
#37526 = CARTESIAN_POINT ( 'NONE',  ( 45.00000000000000000, 9.999999999999980460, -6.999999999999999112 ) ) ;
#37527 = ORIENTED_EDGE ( 'NONE', *, *, #7703, .T. ) ;
#37528 =( NAMED_UNIT ( * ) PLANE_ANGLE_UNIT ( ) SI_UNIT ( $, .RADIAN. ) );
#37530 = DIRECTION ( 'NONE',  ( 0.000000000000000000, -0.000000000000000000, -1.000000000000000000 ) ) ;
#37529 = LINE ( 'NONE', #10408, #51473 ) ;
#37531 = CARTESIAN_POINT ( 'NONE',  ( 15.98999599679679839, 147.4999999999999716, -10.00000000000000000 ) ) ;
#37532 = CIRCLE ( 'NONE', #58820, 0.5000000000000004441 ) ;
#37533 = CARTESIAN_POINT ( 'NONE',  ( -136.4050000000000296, -2.607480562269069768, 8.024999999999991473 ) ) ;
#37534 = CARTESIAN_POINT ( 'NONE',  ( -72.00000000000000000, 35.92875272052971525, 9.500000000000000000 ) ) ;
#37535 = FACE_OUTER_BOUND ( 'NONE', #12343, .T. ) ;
#37536 = FILL_AREA_STYLE ('',( #62893 ) ) ;
#37537 = ADVANCED_FACE ( 'NONE', ( #32383 ), #1373, .F. ) ;
#37538 = CARTESIAN_POINT ( 'NONE',  ( -148.9449999999999932, -9.827790563157499189E-16, -8.024999999999991473 ) ) ;
#37539 = TOROIDAL_SURFACE ( 'NONE', #22933, 1.000000000000000000, 0.5000000000000000000 ) ;
#37540 = CIRCLE ( 'NONE', #20611, 8.000000000000007105 ) ;
#37541 = CARTESIAN_POINT ( 'NONE',  ( -135.8949999999999818, 6.826472737025115478, 4.959722759717899443 ) ) ;
#37542 = ORIENTED_EDGE ( 'NONE', *, *, #56790, .F. ) ;
#37543 = DIRECTION ( 'NONE',  ( 1.000000000000000000, 0.000000000000000000, 0.000000000000000000 ) ) ;
#37544 =( NAMED_UNIT ( * ) SI_UNIT ( $, .STERADIAN. ) SOLID_ANGLE_UNIT ( ) );
#37545 =( GEOMETRIC_REPRESENTATION_CONTEXT ( 3 ) GLOBAL_UNCERTAINTY_ASSIGNED_CONTEXT ( ( #40316 ) ) GLOBAL_UNIT_ASSIGNED_CONTEXT ( ( #55326, #17720, #1097 ) ) REPRESENTATION_CONTEXT ( 'NONE', 'WORKASPACE' ) );
#37546 = ADVANCED_FACE ( 'NONE', ( #11291 ), #52241, .F. ) ;
#37547 = LINE ( 'NONE', #9385, #102 ) ;
#37548 = UNCERTAINTY_MEASURE_WITH_UNIT (LENGTH_MEASURE( 1.000000000000000082E-05 ), #59572, 'distance_accuracy_value', 'NONE');
#37549 = CARTESIAN_POINT ( 'NONE',  ( -54.80499999999999261, -8.437984349512085203, 5.166775262442717831E-16 ) ) ;
#37550 = ADVANCED_FACE ( 'NONE', ( #41689 ), #46641, .T. ) ;
#37551 = TOROIDAL_SURFACE ( 'NONE', #46533, 0.5000000000000000000, 0.2500000000000000000 ) ;
#37552 = CARTESIAN_POINT ( 'NONE',  ( 5.598654528085809545, 161.2549999999999955, -7.705886871421373741 ) ) ;
#37553 = SURFACE_STYLE_USAGE ( .BOTH. , #21297 ) ;
#37554 = SURFACE_STYLE_FILL_AREA ( #37896 ) ;
#37555 = SURFACE_STYLE_USAGE ( .BOTH. , #42137 ) ;
#37556 = PRODUCT_DEFINITION_CONTEXT ( 'detailed design', #32476, 'design' ) ;
#37557 = CARTESIAN_POINT ( 'NONE',  ( -105.1429263765338078, 5.598654528085800663, -7.705886871421367523 ) ) ;
#37558 = CARTESIAN_POINT ( 'NONE',  ( 35.50000000000006395, 50.00000000000002132, 60.00000000000001421 ) ) ;
#37559 = CIRCLE ( 'NONE', #36400, 12.50000000000001066 ) ;
#37560 = CARTESIAN_POINT ( 'NONE',  ( -152.5429263765338135, 9.058813317711329915, 2.943386871421369566 ) ) ;
#37561 =( GEOMETRIC_REPRESENTATION_CONTEXT ( 3 ) GLOBAL_UNCERTAINTY_ASSIGNED_CONTEXT ( ( #68004 ) ) GLOBAL_UNIT_ASSIGNED_CONTEXT ( ( #20803, #31324, #64039 ) ) REPRESENTATION_CONTEXT ( 'NONE', 'WORKASPACE' ) );
#37562 = DIRECTION ( 'NONE',  ( 1.000000000000000000, -0.000000000000000000, 0.000000000000000000 ) ) ;
#37563 = CARTESIAN_POINT ( 'NONE',  ( 0.000000000000000000, 0.000000000000000000, 0.000000000000000000 ) ) ;
#37564 = AXIS2_PLACEMENT_3D ( 'NONE', #4904, #10547, #53777 ) ;
#37565 = EDGE_CURVE ( 'NONE', #48229, #34584, #31321, .T. ) ;
#37566 = DIRECTION ( 'NONE',  ( -1.000000000000000000, -1.156482317317866302E-16, 0.000000000000000000 ) ) ;
#37567 = LINE ( 'NONE', #59273, #22869 ) ;
#37568 =( NAMED_UNIT ( * ) SI_UNIT ( $, .STERADIAN. ) SOLID_ANGLE_UNIT ( ) );
#37569 = ORIENTED_EDGE ( 'NONE', *, *, #6039, .F. ) ;
#37570 = PRESENTATION_STYLE_ASSIGNMENT (( #48106 ) ) ;
#37571 = PRESENTATION_LAYER_ASSIGNMENT (  '', '', ( #55481 ) ) ;
#37572 = CARTESIAN_POINT ( 'NONE',  ( 7.632228543268608334, 114.4570736234661581, -2.479861379858951942 ) ) ;
#37573 = AXIS2_PLACEMENT_3D ( 'NONE', #31141, #35410, #41396 ) ;
#37574 = FILL_AREA_STYLE ('',( #44573 ) ) ;
#37575 = CYLINDRICAL_SURFACE ( 'NONE', #13927, 0.5000000000000004441 ) ;
#37576 = EDGE_LOOP ( 'NONE', ( #17804, #49882, #12486, #2296 ) ) ;
#37577 = ORIENTED_EDGE ( 'NONE', *, *, #40930, .F. ) ;
#37578 = DIRECTION ( 'NONE',  ( 0.000000000000000000, -1.000000000000000000, 0.000000000000000000 ) ) ;
#37579 = COLOUR_RGB ( '', 0.66274510, 0.83137255, 0.94901961) ;
#37580 = DIRECTION ( 'NONE',  ( -0.000000000000000000, 1.000000000000000000, -0.000000000000000000 ) ) ;
#37581 = ORIENTED_EDGE ( 'NONE', *, *, #29706, .T. ) ;
#37582 = CARTESIAN_POINT ( 'NONE',  ( -5.598654528085808657, 126.7549999999999812, 7.705886871421373741 ) ) ;
#37583 = ORIENTED_EDGE ( 'NONE', *, *, #49187, .F. ) ;
#37584 =( LENGTH_UNIT ( ) NAMED_UNIT ( * ) SI_UNIT ( .MILLI., .METRE. ) );
#37585 = EDGE_CURVE ( 'NONE', #5467, #1094, #13889, .T. ) ;
#37586 = CARTESIAN_POINT ( 'NONE',  ( -99.14499999999998181, -4.716976649647092401, 6.492361379858946790 ) ) ;
#37587 = ORIENTED_EDGE ( 'NONE', *, *, #14378, .F. ) ;
#37588 = DIRECTION ( 'NONE',  ( 1.000000000000000000, 0.000000000000000000, 0.000000000000000000 ) ) ;
#37589 = CARTESIAN_POINT ( 'NONE',  ( 11.00000000000001776, 42.00000000000000000, 29.69000000000000128 ) ) ;
#37590 = ORIENTED_EDGE ( 'NONE', *, *, #42966, .F. ) ;
#37591 = CARTESIAN_POINT ( 'NONE',  ( 2.607480562269071989, 154.5929263765338249, 8.025000000000002132 ) ) ;
#37592 = DIRECTION ( 'NONE',  ( -1.000000000000000000, 0.000000000000000000, 1.300977106640434891E-16 ) ) ;
#37593 = CARTESIAN_POINT ( 'NONE',  ( -62.60707362346615668, -8.102448949553174629, 5.886773742842742685 ) ) ;
#37594 = ORIENTED_EDGE ( 'NONE', *, *, #41087, .F. ) ;
#37595 = LINE ( 'NONE', #5490, #11346 ) ;
#37596 = DIRECTION ( 'NONE',  ( 3.717264591378879477E-17, 0.000000000000000000, -1.000000000000000000 ) ) ;
#37597 = DIRECTION ( 'NONE',  ( 0.000000000000000000, 1.000000000000000000, 0.000000000000000000 ) ) ;
#37598 = PRESENTATION_STYLE_ASSIGNMENT (( #16118 ) ) ;
#37599 =( NAMED_UNIT ( * ) PLANE_ANGLE_UNIT ( ) SI_UNIT ( $, .RADIAN. ) );
#37600 = DIRECTION ( 'NONE',  ( 0.000000000000000000, 0.000000000000000000, -1.000000000000000000 ) ) ;
#37601 = CARTESIAN_POINT ( 'NONE',  ( 6.000000000000017764, -60.04052944165106709, 35.50000000000000000 ) ) ;
#37602 = CARTESIAN_POINT ( 'NONE',  ( 2.607480562269098634, 115.5929263765338249, 8.024999999999984368 ) ) ;
#37603 = CARTESIAN_POINT ( 'NONE',  ( -2.139872436712106474, 154.0569316272727178, 8.842724602598590167 ) ) ;
#37604 = EDGE_LOOP ( 'NONE', ( #56345, #1080, #49046, #55320, #47905, #44135, #14910, #5867 ) ) ;
#37605 = EDGE_LOOP ( 'NONE', ( #41892, #29911, #18307 ) ) ;
#37606 = CARTESIAN_POINT ( 'NONE',  ( -28.74999999999999645, -4.000000000000000000, 15.00000000000000178 ) ) ;
#37607 = CARTESIAN_POINT ( 'NONE',  ( -169.5570736234661808, -1.166476076187852838E-15, -9.524999999999991473 ) ) ;
#37608 = CIRCLE ( 'NONE', #17356, 13.99999999999999822 ) ;
#37609 = CARTESIAN_POINT ( 'NONE',  ( -18.25000000000000711, 33.99999999999999289, -3.750000000000000000 ) ) ;
#37610 = ORIENTED_EDGE ( 'NONE', *, *, #30716, .T. ) ;
#37611 = DIRECTION ( 'NONE',  ( 0.000000000000000000, -1.000000000000000000, -0.000000000000000000 ) ) ;
#37612 = CARTESIAN_POINT ( 'NONE',  ( -166.4049999999999727, -2.607480562269069768, 8.024999999999991473 ) ) ;
#37613 = DIRECTION ( 'NONE',  ( 0.000000000000000000, -0.000000000000000000, 1.000000000000000000 ) ) ;
#37614 = CARTESIAN_POINT ( 'NONE',  ( -12.72792206135785165, 115.4999999999999574, -10.00000000000000000 ) ) ;
#37615 = EDGE_CURVE ( 'NONE', #26930, #1355, #17292, .T. ) ;
#37616 = CARTESIAN_POINT ( 'NONE',  ( -182.3950000000000102, -6.826472737025115478, -4.959722759717899443 ) ) ;
#37617 = CARTESIAN_POINT ( 'NONE',  ( -168.2949999999999875, -2.607480562269069768, 8.024999999999991473 ) ) ;
#37618 = ORIENTED_EDGE ( 'NONE', *, *, #40080, .T. ) ;
#37619 = STYLED_ITEM ( 'NONE', ( #52131 ), #27198 ) ;
#37620 = CARTESIAN_POINT ( 'NONE',  ( -15.00000000000000000, 8.000000000000000000, 4.000000000000000000 ) ) ;
#37621 = CIRCLE ( 'NONE', #60053, 1.000000000000000888 ) ;
#37622 = PRESENTATION_STYLE_ASSIGNMENT (( #9815 ) ) ;
#37623 = CARTESIAN_POINT ( 'NONE',  ( -86.00499999999999545, 6.826472737025116366, 4.959722759717898555 ) ) ;
#37624 = DIRECTION ( 'NONE',  ( 0.000000000000000000, -1.000000000000000000, 0.000000000000000000 ) ) ;
#37625 = MECHANICAL_DESIGN_GEOMETRIC_PRESENTATION_REPRESENTATION (  '', ( #45458 ), #64542 ) ;
#37626 = ADVANCED_FACE ( 'NONE', ( #40285 ), #45593, .F. ) ;
#37627 = CARTESIAN_POINT ( 'NONE',  ( -83.54499999999998749, -7.632228543268600340, -2.479861379858950166 ) ) ;
#37628 = CARTESIAN_POINT ( 'NONE',  ( -9.058813317711338797, 138.4549999999999841, 2.943386871421373563 ) ) ;
#37629 = PRESENTATION_LAYER_ASSIGNMENT (  '', '', ( #53353 ) ) ;
#37630 = AXIS2_PLACEMENT_3D ( 'NONE', #46661, #30064, #68080 ) ;
#37631 = DIRECTION ( 'NONE',  ( 0.000000000000000000, 0.000000000000000000, -1.000000000000000000 ) ) ;
#37632 = EDGE_CURVE ( 'NONE', #54750, #24087, #39725, .T. ) ;
#37633 = UNCERTAINTY_MEASURE_WITH_UNIT (LENGTH_MEASURE( 1.000000000000000082E-05 ), #17828, 'distance_accuracy_value', 'NONE');
#37634 = SURFACE_STYLE_FILL_AREA ( #4873 ) ;
#37635 = FILL_AREA_STYLE ('',( #32293 ) ) ;
#37636 = ORIENTED_EDGE ( 'NONE', *, *, #48160, .T. ) ;
#37637 = EDGE_CURVE ( 'NONE', #39801, #48124, #56803, .T. ) ;
#37638 = CARTESIAN_POINT ( 'NONE',  ( -6.826472737025120807, 132.9929263765338021, 4.959722759717906548 ) ) ;
#37639 = VECTOR ( 'NONE', #62458, 1000.000000000000000 ) ;
#37640 = EDGE_CURVE ( 'NONE', #43100, #41477, #53593, .T. ) ;
#37641 = AXIS2_PLACEMENT_3D ( 'NONE', #6103, #43102, #31793 ) ;
#37642 =( LENGTH_UNIT ( ) NAMED_UNIT ( * ) SI_UNIT ( .MILLI., .METRE. ) );
#37643 = CARTESIAN_POINT ( 'NONE',  ( 45.00000000000000000, 10.69371294336137801, -6.000000000000000000 ) ) ;
#37644 = CARTESIAN_POINT ( 'NONE',  ( 0.000000000000000000, 0.000000000000000000, 0.7500000000000000000 ) ) ;
#37645 = VERTEX_POINT ( 'NONE', #32137 ) ;
#37646 = ORIENTED_EDGE ( 'NONE', *, *, #69661, .T. ) ;
#37647 = STYLED_ITEM ( 'NONE', ( #6144 ), #37215 ) ;
#37648 = CARTESIAN_POINT ( 'NONE',  ( 71.49999999999998579, 99.99999999999998579, 7.500000000000000000 ) ) ;
#37649 = MECHANICAL_DESIGN_GEOMETRIC_PRESENTATION_REPRESENTATION (  '', ( #3883 ), #9501 ) ;
#37650 = CIRCLE ( 'NONE', #58987, 0.5000000000000004441 ) ;
#37651 = CARTESIAN_POINT ( 'NONE',  ( -8.437984349512095861, 147.6929263765338192, -5.166775262442723748E-16 ) ) ;
#37652 =( NAMED_UNIT ( * ) PLANE_ANGLE_UNIT ( ) SI_UNIT ( $, .RADIAN. ) );
#37653 = FACE_OUTER_BOUND ( 'NONE', #51701, .T. ) ;
#37654 = LINE ( 'NONE', #69600, #44253 ) ;
#37655 = ORIENTED_EDGE ( 'NONE', *, *, #9112, .F. ) ;
#37656 = CARTESIAN_POINT ( 'NONE',  ( -125.6049999999999898, 6.826472737025113702, -4.959722759717902107 ) ) ;
#37657 = ORIENTED_EDGE ( 'NONE', *, *, #30461, .T. ) ;
#37658 = CARTESIAN_POINT ( 'NONE',  ( -34.99999999999999289, 99.99999999999998579, -7.000000000000000000 ) ) ;
#37659 = CARTESIAN_POINT ( 'NONE',  ( -75.00000000000000000, -2.215169945516535778E-14, 10.00000000000000000 ) ) ;
#37660 = ORIENTED_EDGE ( 'NONE', *, *, #58608, .F. ) ;
#37661 =( NAMED_UNIT ( * ) SI_UNIT ( $, .STERADIAN. ) SOLID_ANGLE_UNIT ( ) );
#37662 = CARTESIAN_POINT ( 'NONE',  ( -83.09292637653379643, 3.094860106618433360, 9.524999999999991473 ) ) ;
#37663 = VERTEX_POINT ( 'NONE', #48357 ) ;
#37664 = DIRECTION ( 'NONE',  ( -0.000000000000000000, -1.000000000000000000, -0.000000000000000000 ) ) ;
#37665 = CARTESIAN_POINT ( 'NONE',  ( 8.102448949553183510, 147.9949999999999761, -5.886773742842746238 ) ) ;
#37666 = SURFACE_STYLE_USAGE ( .BOTH. , #21421 ) ;
#37667 = ORIENTED_EDGE ( 'NONE', *, *, #24318, .T. ) ;
#37668 =( NAMED_UNIT ( * ) PLANE_ANGLE_UNIT ( ) SI_UNIT ( $, .RADIAN. ) );
#37669 = SURFACE_STYLE_USAGE ( .BOTH. , #43302 ) ;
#37670 = CARTESIAN_POINT ( 'NONE',  ( 4.682380833558961619, 2.003239292658529624, 5.889878495889163901 ) ) ;
#37671 = ORIENTED_EDGE ( 'NONE', *, *, #17580, .F. ) ;
#37672 = CARTESIAN_POINT ( 'NONE',  ( 2.607480562269071989, 127.5929263765338249, 8.025000000000002132 ) ) ;
#37673 = FACE_OUTER_BOUND ( 'NONE', #44384, .T. ) ;
#37674 = SURFACE_SIDE_STYLE ('',( #21795 ) ) ;
#37675 = CIRCLE ( 'NONE', #34257, 0.5000000000000004441 ) ;
#37676 = CARTESIAN_POINT ( 'NONE',  ( -104.5429263765337993, 9.058813317711329915, 2.943386871421369566 ) ) ;
#37677 = DIRECTION ( 'NONE',  ( 0.000000000000000000, 0.2503800040544373884, 0.9681476403781088536 ) ) ;
#37678 = VERTEX_POINT ( 'NONE', #4328 ) ;
#37679 = CARTESIAN_POINT ( 'NONE',  ( 5.710692600061826774, -4.108790270285303414, 4.269046054161672230E-16 ) ) ;
#37680 = VERTEX_POINT ( 'NONE', #58880 ) ;
#37681 = CARTESIAN_POINT ( 'NONE',  ( -34.99999999999992895, 110.4999999999999858, 9.500000000000000000 ) ) ;
#37682 = CONICAL_SURFACE ( 'NONE', #19649, 9.000000000000000000, 0.7853981633974500554 ) ;
#37683 = FILL_AREA_STYLE ('',( #11932 ) ) ;
#37684 = DIRECTION ( 'NONE',  ( -1.000000000000000000, 0.000000000000000000, 0.000000000000000000 ) ) ;
#37685 = CARTESIAN_POINT ( 'NONE',  ( -141.0549999999999784, -9.827790563157499189E-16, -8.024999999999991473 ) ) ;
#37686 = DIRECTION ( 'NONE',  ( -1.189524669241239855E-16, -1.000000000000000000, 0.000000000000000000 ) ) ;
#37687 = SURFACE_SIDE_STYLE ('',( #22145 ) ) ;
#37688 = UNCERTAINTY_MEASURE_WITH_UNIT (LENGTH_MEASURE( 1.000000000000000082E-05 ), #12808, 'distance_accuracy_value', 'NONE');
#37689 = CARTESIAN_POINT ( 'NONE',  ( 6.735557395310448926E-16, -2.500000000000000000, 5.500000000000005329 ) ) ;
#37690 = SURFACE_SIDE_STYLE ('',( #10905 ) ) ;
#37691 =( NAMED_UNIT ( * ) PLANE_ANGLE_UNIT ( ) SI_UNIT ( $, .RADIAN. ) );
#37692 =( NAMED_UNIT ( * ) PLANE_ANGLE_UNIT ( ) SI_UNIT ( $, .RADIAN. ) );
#37693 = VERTEX_POINT ( 'NONE', #5377 ) ;
#37694 = VERTEX_POINT ( 'NONE', #47 ) ;
#37695 = LINE ( 'NONE', #38025, #59747 ) ;
#37696 = DIRECTION ( 'NONE',  ( 0.000000000000000000, 0.000000000000000000, 1.000000000000000000 ) ) ;
#37697 = CARTESIAN_POINT ( 'NONE',  ( -58.55499999999999261, 0.000000000000000000, 8.024999999999991473 ) ) ;
#37699 = ORIENTED_EDGE ( 'NONE', *, *, #33349, .T. ) ;
#37698 = MECHANICAL_DESIGN_GEOMETRIC_PRESENTATION_REPRESENTATION (  '', ( #12917 ), #50059 ) ;
#37700 = DIRECTION ( 'NONE',  ( 1.000000000000000000, 0.000000000000000000, 0.000000000000000000 ) ) ;
#37701 = FACE_OUTER_BOUND ( 'NONE', #38242, .T. ) ;
#37702 = CARTESIAN_POINT ( 'NONE',  ( 45.00000000000000000, 10.69371294336137801, 6.000000000000000888 ) ) ;
#37703 = PRESENTATION_STYLE_ASSIGNMENT (( #49249 ) ) ;
#37704 = VECTOR ( 'NONE', #2873, 1000.000000000000000 ) ;
#37705 = EDGE_CURVE ( 'NONE', #7479, #16380, #43115, .T. ) ;
#37706 = CARTESIAN_POINT ( 'NONE',  ( 44.99999999999977973, 146.9999999999999716, -7.500000000000000000 ) ) ;
#37707 = PRESENTATION_LAYER_ASSIGNMENT (  '', '', ( #39946 ) ) ;
#37709 = EDGE_CURVE ( 'NONE', #23604, #41301, #22894, .T. ) ;
#37708 = ORIENTED_EDGE ( 'NONE', *, *, #8895, .F. ) ;
#37710 = FILL_AREA_STYLE ('',( #32709 ) ) ;
#37711 = CIRCLE ( 'NONE', #46643, 5.499999999999976907 ) ;
#37712 = FILL_AREA_STYLE_COLOUR ( '', #53012 ) ;
#37714 = DIRECTION ( 'NONE',  ( 1.000000000000000000, 0.000000000000000000, 0.000000000000000000 ) ) ;
#37713 =( BOUNDED_CURVE ( )  B_SPLINE_CURVE ( 2, ( #65164, #43443, #49044, #734, #22265, #52908, #37812, #64134, #64827, #63787, #16673 ),
 .UNSPECIFIED., .F., .F. ) 
 B_SPLINE_CURVE_WITH_KNOTS ( ( 3, 2, 2, 2, 2, 3 ),
 ( 0.7647058823529410132, 0.7705882352941175739, 0.7764705882352940236, 0.7823529411764704733, 0.7882352941176469230, 0.7941176470588233727 ),
 .UNSPECIFIED. ) 
 CURVE ( )  GEOMETRIC_REPRESENTATION_ITEM ( )  RATIONAL_B_SPLINE_CURVE ( ( 1.000000000000000888, 0.9510565162951526430, 1.000000000000000000, 0.9510565162951535312, 1.000000000000000000, 0.9510565162951535312, 1.000000000000000000, 0.9510565162951535312, 1.000000000000000000, 0.9510565162951544194, 0.9999999999999991118 ) ) 
 REPRESENTATION_ITEM ( '' )  );
#37715 = ADVANCED_FACE ( 'NONE', ( #10353, #63793, #5054 ), #53927, .T. ) ;
#37716 = CARTESIAN_POINT ( 'NONE',  ( -105.5949999999999989, 2.607480562269072433, 8.024999999999991473 ) ) ;
#37717 = CARTESIAN_POINT ( 'NONE',  ( -9.058813317711338797, 111.4549999999999841, 2.943386871421373563 ) ) ;
#37718 = CARTESIAN_POINT ( 'NONE',  ( -85.64499999999998181, 4.716976649647091513, -6.492361379858946790 ) ) ;
#37719 = EDGE_CURVE ( 'NONE', #47990, #49817, #20543, .T. ) ;
#37720 = CARTESIAN_POINT ( 'NONE',  ( 1.908195823574488119E-14, 24.75000000000002487, 3.750000000000000000 ) ) ;
#37721 = CYLINDRICAL_SURFACE ( 'NONE', #52826, 0.2500000000000002220 ) ;
#37722 = CARTESIAN_POINT ( 'NONE',  ( 0.000000000000000000, 0.000000000000000000, 0.000000000000000000 ) ) ;
#37723 = UNCERTAINTY_MEASURE_WITH_UNIT (LENGTH_MEASURE( 1.000000000000000082E-05 ), #14252, 'distance_accuracy_value', 'NONE');
#37724 = DIRECTION ( 'NONE',  ( -0.000000000000000000, -1.000000000000000000, -0.000000000000000000 ) ) ;
#37725 = COLOUR_RGB ( '', 0.31764706, 0.68627451, 0.89019608) ;
#37726 = ORIENTED_EDGE ( 'NONE', *, *, #25115, .T. ) ;
#37727 = EDGE_CURVE ( 'NONE', #69365, #40929, #31421, .T. ) ;
#37728 = CARTESIAN_POINT ( 'NONE',  ( -134.0929263765338249, 3.094860106618433360, 9.524999999999991473 ) ) ;
#37729 =( LENGTH_UNIT ( ) NAMED_UNIT ( * ) SI_UNIT ( .MILLI., .METRE. ) );
#37730 = CARTESIAN_POINT ( 'NONE',  ( -144.4449999999999932, 0.000000000000000000, 8.024999999999991473 ) ) ;
#37731 = SURFACE_STYLE_USAGE ( .BOTH. , #59815 ) ;
#37732 = DIRECTION ( 'NONE',  ( 1.000000000000000000, 1.084202172485503448E-16, 0.000000000000000000 ) ) ;
#37733 = VECTOR ( 'NONE', #61381, 1000.000000000000000 ) ;
#37734 = DIRECTION ( 'NONE',  ( -1.000000000000000000, -0.000000000000000000, -0.000000000000000000 ) ) ;
#37735 = ORIENTED_EDGE ( 'NONE', *, *, #42538, .T. ) ;
#37736 = ORIENTED_EDGE ( 'NONE', *, *, #40060, .T. ) ;
#37737 =( BOUNDED_CURVE ( )  B_SPLINE_CURVE ( 3, ( #46397, #29824, #19952, #41115 ),
 .UNSPECIFIED., .F., .F. ) 
 B_SPLINE_CURVE_WITH_KNOTS ( ( 4, 4 ),
 ( 0.000000000000000000, 1.570796326794896558 ),
 .UNSPECIFIED. ) 
 CURVE ( )  GEOMETRIC_REPRESENTATION_ITEM ( )  RATIONAL_B_SPLINE_CURVE ( ( 1.000000000000000000, 0.8047378541243649375, 0.8047378541243649375, 1.000000000000000000 ) ) 
 REPRESENTATION_ITEM ( '' )  );
#37738 = CARTESIAN_POINT ( 'NONE',  ( 0.000000000000000000, 152.9999999999999716, 0.000000000000000000 ) ) ;
#37739 = CARTESIAN_POINT ( 'NONE',  ( -155.3929263765337794, 8.102448949553176405, 5.886773742842740909 ) ) ;
#37740 = CARTESIAN_POINT ( 'NONE',  ( -45.00000000000000000, 9.675769070491668344, 6.195678411461557289 ) ) ;
#37741 = CARTESIAN_POINT ( 'NONE',  ( -59.09292637653378932, 3.094860106618433360, 9.524999999999991473 ) ) ;
#37742 = CARTESIAN_POINT ( 'NONE',  ( -116.6929263765337907, 10.01517768586948698, -1.839758294383808966E-15 ) ) ;
#37743 = CARTESIAN_POINT ( 'NONE',  ( -151.7929263765341830, -3.094860106611539319, 9.525000000005000800 ) ) ;
#37744 = VERTEX_POINT ( 'NONE', #52914 ) ;
#37745 = CARTESIAN_POINT ( 'NONE',  ( -146.7549999999999955, 4.716976649647091513, -6.492361379858946790 ) ) ;
#37746 = CIRCLE ( 'NONE', #14102, 7.499999999999992895 ) ;
#37747 = ORIENTED_EDGE ( 'NONE', *, *, #57503, .T. ) ;
#37748 = CARTESIAN_POINT ( 'NONE',  ( 5.705565085145811288, 4.117671386636414077, 0.02778322089669325520 ) ) ;
#37749 = DIRECTION ( 'NONE',  ( 0.000000000000000000, 0.000000000000000000, 1.000000000000000000 ) ) ;
#37750 = ORIENTED_EDGE ( 'NONE', *, *, #50744, .F. ) ;
#37751 = CIRCLE ( 'NONE', #19715, 0.5000000000000004441 ) ;
#37752 = CARTESIAN_POINT ( 'NONE',  ( -5.196152422706636465, 1.107695154586736175, -9.000000000000003553 ) ) ;
#37753 = DIRECTION ( 'NONE',  ( -1.000000000000000000, 0.000000000000000000, 0.000000000000000000 ) ) ;
#37754 = CARTESIAN_POINT ( 'NONE',  ( -8.102448949553181734, 124.8949999999999960, -5.886773742842749790 ) ) ;
#37755 =( LENGTH_UNIT ( ) NAMED_UNIT ( * ) SI_UNIT ( .MILLI., .METRE. ) );
#37756 = AXIS2_PLACEMENT_3D ( 'NONE', #28135, #23581, #60186 ) ;
#37757 = EDGE_CURVE ( 'NONE', #27240, #39729, #316, .T. ) ;
#37758 = ORIENTED_EDGE ( 'NONE', *, *, #34966, .F. ) ;
#37759 = DIRECTION ( 'NONE',  ( -1.000000000000000000, 0.000000000000000000, 0.000000000000000000 ) ) ;
#37760 = CARTESIAN_POINT ( 'NONE',  ( -3.094860106618434248, 132.9050000000000011, 9.525000000000000355 ) ) ;
#37761 = CARTESIAN_POINT ( 'NONE',  ( -69.20499999999998408, -2.607480562269071545, -8.024999999999991473 ) ) ;
#37762 = CARTESIAN_POINT ( 'NONE',  ( -124.9450000000000074, -9.827790563157499189E-16, -8.024999999999991473 ) ) ;
#37763 = CARTESIAN_POINT ( 'NONE',  ( -71.99999999999998579, 119.9999999999997868, 7.500000000000000000 ) ) ;
#37764 = EDGE_LOOP ( 'NONE', ( #55520, #34196, #62622, #54420 ) ) ;
#37765 = CARTESIAN_POINT ( 'NONE',  ( -9.058813317711337021, 144.1549999999999727, -2.943386871421374895 ) ) ;
#37766 = DIRECTION ( 'NONE',  ( -0.000000000000000000, 0.000000000000000000, 1.000000000000000000 ) ) ;
#37767 = UNCERTAINTY_MEASURE_WITH_UNIT (LENGTH_MEASURE( 1.000000000000000082E-05 ), #39524, 'distance_accuracy_value', 'NONE');
#37768 = CYLINDRICAL_SURFACE ( 'NONE', #55622, 3.000000000000000444 ) ;
#37769 = CARTESIAN_POINT ( 'NONE',  ( 8.750000000000001776, 24.74999999999998579, 3.750000000000000000 ) ) ;
#37770 = ORIENTED_EDGE ( 'NONE', *, *, #53158, .T. ) ;
#37771 = CARTESIAN_POINT ( 'NONE',  ( 19.89974874213240597, 115.4999999999999574, 10.50000000000000000 ) ) ;
#37772 = CARTESIAN_POINT ( 'NONE',  ( -169.2549999999999955, -4.716976649647092401, 6.492361379858946790 ) ) ;
#37773 = ORIENTED_EDGE ( 'NONE', *, *, #37976, .T. ) ;
#37774 = DIRECTION ( 'NONE',  ( -0.000000000000000000, -1.000000000000000000, -0.000000000000000000 ) ) ;
#37775 = UNCERTAINTY_MEASURE_WITH_UNIT (LENGTH_MEASURE( 1.000000000000000082E-05 ), #23177, 'distance_accuracy_value', 'NONE');
#37776 = COLOUR_RGB ( '', 0.08235294, 0.09019608, 0.10196078) ;
#37777 =( NAMED_UNIT ( * ) PLANE_ANGLE_UNIT ( ) SI_UNIT ( $, .RADIAN. ) );
#37778 = FILL_AREA_STYLE_COLOUR ( '', #57673 ) ;
#37779 = FILL_AREA_STYLE_COLOUR ( '', #18584 ) ;
#37780 = DIRECTION ( 'NONE',  ( 1.156482317317873451E-16, 1.000000000000000000, -0.000000000000000000 ) ) ;
#37781 = ORIENTED_EDGE ( 'NONE', *, *, #69514, .F. ) ;
#37782 = FACE_OUTER_BOUND ( 'NONE', #11249, .T. ) ;
#37783 = EDGE_CURVE ( 'NONE', #54061, #29745, #20897, .T. ) ;
#37784 = PRESENTATION_LAYER_ASSIGNMENT (  '', '', ( #5120 ) ) ;
#37785 = SURFACE_STYLE_FILL_AREA ( #54237 ) ;
#37786 = CARTESIAN_POINT ( 'NONE',  ( -87.05499999999999261, -9.827790563157499189E-16, -8.024999999999991473 ) ) ;
#37787 = ORIENTED_EDGE ( 'NONE', *, *, #27614, .T. ) ;
#37788 = EDGE_CURVE ( 'NONE', #2804, #65448, #5997, .T. ) ;
#37789 = SURFACE_STYLE_FILL_AREA ( #5020 ) ;
#37790 =( GEOMETRIC_REPRESENTATION_CONTEXT ( 3 ) GLOBAL_UNCERTAINTY_ASSIGNED_CONTEXT ( ( #48254 ) ) GLOBAL_UNIT_ASSIGNED_CONTEXT ( ( #27628, #64926, #65973 ) ) REPRESENTATION_CONTEXT ( 'NONE', 'WORKASPACE' ) );
#37791 = FACE_OUTER_BOUND ( 'NONE', #7424, .T. ) ;
#37792 = PRESENTATION_STYLE_ASSIGNMENT (( #49333 ) ) ;
#37793 = CARTESIAN_POINT ( 'NONE',  ( -67.85707362346617799, -5.598654528085803328, -7.705886871421366635 ) ) ;
#37794 = EDGE_CURVE ( 'NONE', #52209, #59509, #21942, .T. ) ;
#37795 = ORIENTED_EDGE ( 'NONE', *, *, #27688, .F. ) ;
#37796 = DIRECTION ( 'NONE',  ( 4.625929269271505635E-16, -0.000000000000000000, 1.000000000000000000 ) ) ;
#37797 = LINE ( 'NONE', #43072, #63914 ) ;
#37798 = FILL_AREA_STYLE_COLOUR ( '', #35864 ) ;
#37799 = AXIS2_PLACEMENT_3D ( 'NONE', #65092, #1736, #16947 ) ;
#37800 = CARTESIAN_POINT ( 'NONE',  ( -115.2549999999999955, -4.716976649647092401, 6.492361379858946790 ) ) ;
#37801 = CARTESIAN_POINT ( 'NONE',  ( -3.094860106618434248, 131.7950000000000159, 9.525000000000000355 ) ) ;
#37802 = CARTESIAN_POINT ( 'NONE',  ( -117.8949999999999676, 6.826472737025116366, 4.959722759717898555 ) ) ;
#37803 = VECTOR ( 'NONE', #12248, 1000.000000000000000 ) ;
#37804 = EDGE_CURVE ( 'NONE', #66680, #52777, #62176, .T. ) ;
#37805 = CIRCLE ( 'NONE', #62442, 0.5000000000000004441 ) ;
#37806 = CYLINDRICAL_SURFACE ( 'NONE', #66194, 1.000000000000000888 ) ;
#37808 = FILL_AREA_STYLE_COLOUR ( '', #53885 ) ;
#37807 = CARTESIAN_POINT ( 'NONE',  ( -33.12716783835527679, -9.131344072917100263, -2.873593582817198566 ) ) ;
#37809 = ADVANCED_FACE ( 'NONE', ( #25811 ), #47324, .T. ) ;
#37810 = CARTESIAN_POINT ( 'NONE',  ( -164.0929263765337680, 3.094860106618433360, 9.524999999999991473 ) ) ;
#37811 = CARTESIAN_POINT ( 'NONE',  ( -179.0949999999999704, -2.607480562269071545, -8.024999999999991473 ) ) ;
#37812 = CARTESIAN_POINT ( 'NONE',  ( -7.632228543268608334, 148.9570736234661581, 2.479861379858952830 ) ) ;
#37813 = CARTESIAN_POINT ( 'NONE',  ( -40.04190075645216496, -13.49999999999999822, 0.8979962945199001512 ) ) ;
#37814 = CARTESIAN_POINT ( 'NONE',  ( -61.64292637653380780, -5.598654528085801552, 7.705886871421367523 ) ) ;
#37815 = FILL_AREA_STYLE ('',( #53266 ) ) ;
#37816 = ORIENTED_EDGE ( 'NONE', *, *, #1377, .T. ) ;
#37817 = CARTESIAN_POINT ( 'NONE',  ( -78.74292637653380211, -5.598654528085803328, -7.705886871421366635 ) ) ;
#37818 = ITEM_DEFINED_TRANSFORMATION ( 'NONE', 'NONE', #68618,  #42840 ) ;
#37819 = DIRECTION ( 'NONE',  ( 0.000000000000000000, 1.000000000000000000, 0.000000000000000000 ) ) ;
#37820 = CARTESIAN_POINT ( 'NONE',  ( -19.49999999999999645, 8.000000000000000000, 4.000000000000000000 ) ) ;
#37821 = CARTESIAN_POINT ( 'NONE',  ( 4.716976649647096842, 151.7429263765338021, 6.492361379858953896 ) ) ;
#37822 = DIRECTION ( 'NONE',  ( 0.000000000000000000, 0.000000000000000000, -1.000000000000000000 ) ) ;
#37823 = DIRECTION ( 'NONE',  ( 0.000000000000000000, 0.000000000000000000, 1.000000000000000000 ) ) ;
#37824 = CIRCLE ( 'NONE', #34397, 0.5000000000000004441 ) ;
#37825 = CARTESIAN_POINT ( 'NONE',  ( -178.8549999999999898, 4.716976649647094177, 6.492361379858945902 ) ) ;
#37826 = COLOUR_RGB ( '', 0.31764706, 0.68627451, 0.89019608) ;
#37827 = ORIENTED_EDGE ( 'NONE', *, *, #34019, .F. ) ;
#37828 =( LENGTH_UNIT ( ) NAMED_UNIT ( * ) SI_UNIT ( .MILLI., .METRE. ) );
#37829 = SURFACE_SIDE_STYLE ('',( #47701 ) ) ;
#37830 = CARTESIAN_POINT ( 'NONE',  ( -73.55707362346616662, -1.166476076187852838E-15, -9.524999999999991473 ) ) ;
#37831 = FACE_OUTER_BOUND ( 'NONE', #466, .T. ) ;
#37832 = CARTESIAN_POINT ( 'NONE',  ( -2.607480562269073765, 139.2070736234661581, -8.025000000000000355 ) ) ;
#37833 =( BOUNDED_CURVE ( )  B_SPLINE_CURVE ( 2, ( #41494, #35154, #56247, #13694, #19665, #41856, #25617, #40810, #14380, #35851, #41160 ),
 .UNSPECIFIED., .F., .F. ) 
 B_SPLINE_CURVE_WITH_KNOTS ( ( 3, 2, 2, 2, 2, 3 ),
 ( 0.9130434782608695121, 0.9152173913043478715, 0.9173913043478261198, 0.9195652173913043681, 0.9217391304347826164, 0.9239130434782608647 ),
 .UNSPECIFIED. ) 
 CURVE ( )  GEOMETRIC_REPRESENTATION_ITEM ( )  RATIONAL_B_SPLINE_CURVE ( ( 1.000000000000000000, 0.9510565162951535312, 1.000000000000000000, 0.9510565162951535312, 1.000000000000000000, 0.9510565162951535312, 1.000000000000000000, 0.9510565162951535312, 1.000000000000000000, 0.9510565162951535312, 1.000000000000000000 ) ) 
 REPRESENTATION_ITEM ( '' )  );
#37834 = ADVANCED_FACE ( 'NONE', ( #37117 ), #47691, .T. ) ;
#37835 = EDGE_LOOP ( 'NONE', ( #11773, #28077, #43891, #68849 ) ) ;
#37836 = CARTESIAN_POINT ( 'NONE',  ( -101.1570736234661609, -9.058813317711329915, -2.943386871421370898 ) ) ;
#37837 = CARTESIAN_POINT ( 'NONE',  ( -90.65499999999998693, -7.632228543268600340, -2.479861379858950166 ) ) ;
#37838 = UNCERTAINTY_MEASURE_WITH_UNIT (LENGTH_MEASURE( 1.000000000000000082E-05 ), #65126, 'distance_accuracy_value', 'NONE');
#37839 = DIRECTION ( 'NONE',  ( -1.000000000000000000, -0.000000000000000000, 1.300977106640434891E-16 ) ) ;
#37840 = VERTEX_POINT ( 'NONE', #21220 ) ;
#37841 = TOROIDAL_SURFACE ( 'NONE', #69233, 2.000000000000000000, 1.000000000000000000 ) ;
#37842 = CARTESIAN_POINT ( 'NONE',  ( 22.99999999999996447, 5.000000000000000000, 29.00402776293825369 ) ) ;
#37843 = LINE ( 'NONE', #38866, #42379 ) ;
#37844 = DIRECTION ( 'NONE',  ( 0.000000000000000000, 0.000000000000000000, 1.000000000000000000 ) ) ;
#37845 = ORIENTED_EDGE ( 'NONE', *, *, #17046, .F. ) ;
#37846 = SURFACE_STYLE_USAGE ( .BOTH. , #6805 ) ;
#37847 = CARTESIAN_POINT ( 'NONE',  ( -66.74499999999999034, 4.716976649647094177, 6.492361379858945902 ) ) ;
#37848 = ORIENTED_EDGE ( 'NONE', *, *, #58912, .T. ) ;
#37849 = DIRECTION ( 'NONE',  ( 1.000000000000000000, -0.000000000000000000, 0.000000000000000000 ) ) ;
#37850 = EDGE_CURVE ( 'NONE', #7517, #1721, #36391, .T. ) ;
#37851 = CARTESIAN_POINT ( 'NONE',  ( -13.75000000000000533, 30.74999999999999289, 4.000000000000000000 ) ) ;
#37852 = CARTESIAN_POINT ( 'NONE',  ( -15.75000000000000000, -4.000000000000000000, 20.00000000000000000 ) ) ;
#37853 = EDGE_CURVE ( 'NONE', #42295, #44642, #29604, .T. ) ;
#37854 = EDGE_LOOP ( 'NONE', ( #36349, #12063, #53444, #37424 ) ) ;
#37855 = CARTESIAN_POINT ( 'NONE',  ( 1.000000000000000000, 0.9999999999999991118, 79.00402776293826435 ) ) ;
#37856 = LINE ( 'NONE', #33891, #34810 ) ;
#37857 = ORIENTED_EDGE ( 'NONE', *, *, #5570, .T. ) ;
#37858 = EDGE_CURVE ( 'NONE', #26152, #23161, #22120, .T. ) ;
#37859 =( LENGTH_UNIT ( ) NAMED_UNIT ( * ) SI_UNIT ( .MILLI., .METRE. ) );
#37860 = LINE ( 'NONE', #69467, #55955 ) ;
#37861 = CARTESIAN_POINT ( 'NONE',  ( -124.4049999999999869, -2.607480562269069768, 8.024999999999991473 ) ) ;
#37862 = ORIENTED_EDGE ( 'NONE', *, *, #54494, .F. ) ;
#37863 = EDGE_CURVE ( 'NONE', #3256, #14756, #2591, .T. ) ;
#37864 = VERTEX_POINT ( 'NONE', #7482 ) ;
#37865 = CARTESIAN_POINT ( 'NONE',  ( -41.49999999999998579, 108.0000000000000000, 3.500000000000000000 ) ) ;
#37866 = CARTESIAN_POINT ( 'NONE',  ( 52.49999999999998579, 2.746146170318484607E-15, -12.00000000000000000 ) ) ;
#37867 = CARTESIAN_POINT ( 'NONE',  ( 24.00000000000000000, 1.000000000000000000, -3.000000000000000000 ) ) ;
#37868 = CARTESIAN_POINT ( 'NONE',  ( -161.3070736234661808, -10.01517768586948698, 6.132527647946031529E-16 ) ) ;
#37869 = CARTESIAN_POINT ( 'NONE',  ( -3.094860106618432471, 133.5949999999999989, -9.525000000000000355 ) ) ;
#37870 = CARTESIAN_POINT ( 'NONE',  ( -95.15707362346617515, -9.058813317711329915, -2.943386871421370898 ) ) ;
#37871 = EDGE_CURVE ( 'NONE', #59688, #54235, #22623, .T. ) ;
#37872 = CARTESIAN_POINT ( 'NONE',  ( 40.49999999999998579, 107.7459666924148252, 3.000000000000000000 ) ) ;
#37873 = PRODUCT ( '15. Washer M6', '15. Washer M6', '', ( #55041 ) ) ;
#37874 = EDGE_LOOP ( 'NONE', ( #3220, #10102, #41357, #64331, #41812, #44780 ) ) ;
#37875 = FACE_OUTER_BOUND ( 'NONE', #23246, .T. ) ;
#37876 = EDGE_CURVE ( 'NONE', #48050, #10014, #66573, .T. ) ;
#37878 = DIRECTION ( 'NONE',  ( -1.000000000000000000, 0.000000000000000000, 0.000000000000000000 ) ) ;
#37877 = CARTESIAN_POINT ( 'NONE',  ( -60.70461754965443646, -8.499999999999992895, 1.000000000000000000 ) ) ;
#37880 = CARTESIAN_POINT ( 'NONE',  ( 1.000000000000000888, 14.00000000000000533, -35.50000000000000000 ) ) ;
#37879 = CIRCLE ( 'NONE', #1802, 12.50000000000001066 ) ;
#37881 = CARTESIAN_POINT ( 'NONE',  ( -142.7049999999999557, 2.607480562269073321, 8.024999999999991473 ) ) ;
#37882 = CONICAL_SURFACE ( 'NONE', #59146, 3.599999999999992095, 0.7853981633974375098 ) ;
#37883 = CARTESIAN_POINT ( 'NONE',  ( 75.00000000000000000, 19.92376017841764479, 7.000000000000000000 ) ) ;
#37884 = CARTESIAN_POINT ( 'NONE',  ( 41.84210526315788314, 107.2928455055531600, 4.000000000000000000 ) ) ;
#37885 = CARTESIAN_POINT ( 'NONE',  ( -146.8449999999999989, -7.632228543268599452, 2.479861379858951054 ) ) ;
#37886 = CIRCLE ( 'NONE', #27649, 23.00000000000000355 ) ;
#37887 = CARTESIAN_POINT ( 'NONE',  ( -143.0949999999999704, -2.607480562269071545, -8.024999999999991473 ) ) ;
#37888 = EDGE_LOOP ( 'NONE', ( #67551, #56028, #68584, #18229 ) ) ;
#37889 = SURFACE_SIDE_STYLE ('',( #53995 ) ) ;
#37890 = SURFACE_STYLE_USAGE ( .BOTH. , #32207 ) ;
#37891 = CARTESIAN_POINT ( 'NONE',  ( -53.60499999999998977, 6.826472737025113702, -4.959722759717902107 ) ) ;
#37892 = CARTESIAN_POINT ( 'NONE',  ( -54.74499999999999034, 4.716976649647094177, 6.492361379858945902 ) ) ;
#37893 = CIRCLE ( 'NONE', #18712, 0.2500000000000002220 ) ;
#37894 = CARTESIAN_POINT ( 'NONE',  ( 26.00000000000001066, 19.24999999999997868, -4.000000000000000000 ) ) ;
#37895 = FILL_AREA_STYLE_COLOUR ( '', #31317 ) ;
#37896 = FILL_AREA_STYLE ('',( #48783 ) ) ;
#37897 = LINE ( 'NONE', #22354, #62654 ) ;
#37898 = ADVANCED_FACE ( 'NONE', ( #28201 ), #44807, .F. ) ;
#37899 = CARTESIAN_POINT ( 'NONE',  ( -106.3429263765338106, -9.058813317711329915, 2.943386871421371787 ) ) ;
#37900 = DIRECTION ( 'NONE',  ( -9.279055218099539736E-17, -0.3711537444790455886, 0.9285714285714283811 ) ) ;
#37901 = DIRECTION ( 'NONE',  ( 0.000000000000000000, -1.000000000000000000, 0.000000000000000000 ) ) ;
#37902 = AXIS2_PLACEMENT_3D ( 'NONE', #48464, #23086, #21688 ) ;
#37903 = CARTESIAN_POINT ( 'NONE',  ( -74.99999999999998579, 50.00000000000000000, 7.500000000000000000 ) ) ;
#37904 = DIRECTION ( 'NONE',  ( -0.000000000000000000, -1.000000000000000000, -0.000000000000000000 ) ) ;
#37905 = CARTESIAN_POINT ( 'NONE',  ( 10.00000000000001954, 50.00000000000000000, 60.00000000000000000 ) ) ;
#37906 = ORIENTED_EDGE ( 'NONE', *, *, #54926, .F. ) ;
#37907 = CARTESIAN_POINT ( 'NONE',  ( 60.00000000000000000, 115.4999999999999574, -10.00000000000000000 ) ) ;
#37908 = ORIENTED_EDGE ( 'NONE', *, *, #26363, .T. ) ;
#37909 = CARTESIAN_POINT ( 'NONE',  ( 2.607480562269071989, 113.7070736234661439, 8.025000000000002132 ) ) ;
#37910 = CARTESIAN_POINT ( 'NONE',  ( -20.22778885548742522, 114.9430298377684210, 10.39013442403998866 ) ) ;
#37911 = CARTESIAN_POINT ( 'NONE',  ( 22.50000000000000711, 37.00000000000000000, 3.750000000000000000 ) ) ;
#37912 = VERTEX_POINT ( 'NONE', #17710 ) ;
#37913 = VERTEX_POINT ( 'NONE', #18034 ) ;
#37914 = AXIS2_PLACEMENT_3D ( 'NONE', #47918, #21457, #21113 ) ;
#37915 = CARTESIAN_POINT ( 'NONE',  ( -116.0070736234661553, -8.102448949553174629, -5.886773742842741797 ) ) ;
#37916 = FACE_OUTER_BOUND ( 'NONE', #23950, .T. ) ;
#37917 = ORIENTED_EDGE ( 'NONE', *, *, #29370, .T. ) ;
#37918 = CARTESIAN_POINT ( 'NONE',  ( -9.058813317711337021, 132.1550000000000011, -2.943386871421374895 ) ) ;
#37919 = DIRECTION ( 'NONE',  ( -1.000000000000000000, 0.000000000000000000, 0.000000000000000000 ) ) ;
#37920 =( GEOMETRIC_REPRESENTATION_CONTEXT ( 3 ) GLOBAL_UNCERTAINTY_ASSIGNED_CONTEXT ( ( #68425 ) ) GLOBAL_UNIT_ASSIGNED_CONTEXT ( ( #34656, #22742, #52870 ) ) REPRESENTATION_CONTEXT ( 'NONE', 'WORKASPACE' ) );
#37921 = CIRCLE ( 'NONE', #41273, 0.2500000000000002220 ) ;
#37922 = CYLINDRICAL_SURFACE ( 'NONE', #6953, 0.2500000000000002220 ) ;
#37923 = CARTESIAN_POINT ( 'NONE',  ( -101.5449999999999875, -7.632228543268600340, -2.479861379858950166 ) ) ;
#37924 = ORIENTED_EDGE ( 'NONE', *, *, #40632, .T. ) ;
#37925 = SURFACE_SIDE_STYLE ('',( #5483 ) ) ;
#37926 = EDGE_CURVE ( 'NONE', #65056, #28347, #39518, .T. ) ;
#37927 = SURFACE_SIDE_STYLE ('',( #59301 ) ) ;
#37928 = EDGE_LOOP ( 'NONE', ( #15215, #26191, #1120 ) ) ;
#37929 = LINE ( 'NONE', #32956, #32451 ) ;
#37930 = FILL_AREA_STYLE_COLOUR ( '', #25777 ) ;
#37931 = DIRECTION ( 'NONE',  ( 0.000000000000000000, -1.000000000000000000, 0.000000000000000000 ) ) ;
#37932 = VECTOR ( 'NONE', #1021, 1000.000000000000000 ) ;
#37933 = EDGE_CURVE ( 'NONE', #14708, #67110, #55406, .T. ) ;
#37934 = VERTEX_POINT ( 'NONE', #65530 ) ;
#37935 = DIRECTION ( 'NONE',  ( 0.000000000000000000, 0.000000000000000000, 1.000000000000000000 ) ) ;
#37936 = ORIENTED_EDGE ( 'NONE', *, *, #6833, .T. ) ;
#37937 = CARTESIAN_POINT ( 'NONE',  ( -79.94292637653380496, 0.000000000000000000, 9.524999999999991473 ) ) ;
#37938 =( NAMED_UNIT ( * ) PLANE_ANGLE_UNIT ( ) SI_UNIT ( $, .RADIAN. ) );
#37939 = FACE_OUTER_BOUND ( 'NONE', #45700, .T. ) ;
#37940 = FILL_AREA_STYLE ('',( #48483 ) ) ;
#37941 = DIRECTION ( 'NONE',  ( -0.000000000000000000, -1.000000000000000000, -0.000000000000000000 ) ) ;
#37942 = CARTESIAN_POINT ( 'NONE',  ( 0.000000000000000000, 9.000000000000007105, 0.000000000000000000 ) ) ;
#37943 = DIRECTION ( 'NONE',  ( 0.000000000000000000, -0.000000000000000000, -1.000000000000000000 ) ) ;
#37944 = CARTESIAN_POINT ( 'NONE',  ( 8.437984349512095861, 116.1929263765338192, 1.550032578732816828E-15 ) ) ;
#37945 = DIRECTION ( 'NONE',  ( 1.000000000000000000, 0.000000000000000000, 0.000000000000000000 ) ) ;
#37946 = VERTEX_POINT ( 'NONE', #2121 ) ;
#37947 = ORIENTED_EDGE ( 'NONE', *, *, #35216, .T. ) ;
#37948 =( NAMED_UNIT ( * ) SI_UNIT ( $, .STERADIAN. ) SOLID_ANGLE_UNIT ( ) );
#37949 = PLANE ( 'NONE',  #2877 ) ;
#37950 = EDGE_CURVE ( 'NONE', #51702, #48200, #25092, .T. ) ;
#37951 = DIRECTION ( 'NONE',  ( -1.000000000000000000, 0.000000000000000000, 0.000000000000000000 ) ) ;
#37952 = FILL_AREA_STYLE ('',( #48497 ) ) ;
#37953 = ORIENTED_EDGE ( 'NONE', *, *, #55798, .T. ) ;
#37954 = DIRECTION ( 'NONE',  ( 0.000000000000000000, 0.000000000000000000, -1.000000000000000000 ) ) ;
#37955 = CARTESIAN_POINT ( 'NONE',  ( -173.4549999999999841, 7.632228543268599452, -2.479861379858951942 ) ) ;
#37956 = LINE ( 'NONE', #10490, #67796 ) ;
#37957 = DIRECTION ( 'NONE',  ( 1.000000000000000000, 0.000000000000000000, 0.000000000000000000 ) ) ;
#37958 = CARTESIAN_POINT ( 'NONE',  ( -175.0450000000000159, 7.632228543268600340, 2.479861379858949277 ) ) ;
#37959 = CARTESIAN_POINT ( 'NONE',  ( -162.5949999999999704, 2.607480562269072433, 8.024999999999991473 ) ) ;
#37960 = ORIENTED_EDGE ( 'NONE', *, *, #23356, .T. ) ;
#37961 = FACE_OUTER_BOUND ( 'NONE', #24074, .T. ) ;
#37962 = SURFACE_STYLE_FILL_AREA ( #20705 ) ;
#37963 = SURFACE_SIDE_STYLE ('',( #34012 ) ) ;
#37964 = CARTESIAN_POINT ( 'NONE',  ( -82.70499999999999829, 2.607480562269073321, 8.024999999999991473 ) ) ;
#37965 = FACE_OUTER_BOUND ( 'NONE', #7646, .T. ) ;
#37966 =( LENGTH_UNIT ( ) NAMED_UNIT ( * ) SI_UNIT ( .MILLI., .METRE. ) );
#37967 = CARTESIAN_POINT ( 'NONE',  ( 7.999999999999989342, 0.000000000000000000, 37.00402776293825724 ) ) ;
#37968 =( GEOMETRIC_REPRESENTATION_CONTEXT ( 3 ) GLOBAL_UNCERTAINTY_ASSIGNED_CONTEXT ( ( #60831 ) ) GLOBAL_UNIT_ASSIGNED_CONTEXT ( ( #47089, #50947, #45706 ) ) REPRESENTATION_CONTEXT ( 'NONE', 'WORKASPACE' ) );
#37969 = CARTESIAN_POINT ( 'NONE',  ( -80.39499999999998181, -6.826472737025113702, -4.959722759717900331 ) ) ;
#37970 = CARTESIAN_POINT ( 'NONE',  ( 8.102448949553181734, 136.5049999999999386, 5.886773742842750679 ) ) ;
#37971 = STYLED_ITEM ( 'NONE', ( #6998 ), #3964 ) ;
#37972 = ADVANCED_FACE ( 'NONE', ( #54618 ), #47698, .F. ) ;
#37973 = CARTESIAN_POINT ( 'NONE',  ( -7.632228543268608334, 126.8429263765338249, 2.479861379858952830 ) ) ;
#37974 = CARTESIAN_POINT ( 'NONE',  ( -4.000000000000000000, -3.499999999999999556, 24.00000000000000000 ) ) ;
#37975 = CARTESIAN_POINT ( 'NONE',  ( -74.99999999999998579, 36.00000000000000711, 9.500000000000001776 ) ) ;
#37976 = EDGE_CURVE ( 'NONE', #16826, #8613, #67823, .T. ) ;
#37977 = CARTESIAN_POINT ( 'NONE',  ( 74.50000000000000000, 20.36037961002804408, 6.000000000000000888 ) ) ;
#37978 = FILL_AREA_STYLE_COLOUR ( '', #23621 ) ;
#37979 = ORIENTED_EDGE ( 'NONE', *, *, #23978, .F. ) ;
#37980 = CARTESIAN_POINT ( 'NONE',  ( -2.607480562269032909, 133.2929263765337851, 8.025000000000032330 ) ) ;
#37981 = CIRCLE ( 'NONE', #34554, 5.249999999999991118 ) ;
#37982 = VECTOR ( 'NONE', #34066, 1000.000000000000000 ) ;
#37983 = FACE_OUTER_BOUND ( 'NONE', #66976, .T. ) ;
#37984 = PRESENTATION_STYLE_ASSIGNMENT (( #581 ) ) ;
#37985 = ORIENTED_EDGE ( 'NONE', *, *, #64581, .F. ) ;
#37986 = VERTEX_POINT ( 'NONE', #40913 ) ;
#37987 = FACE_OUTER_BOUND ( 'NONE', #46683, .T. ) ;
#37988 = CARTESIAN_POINT ( 'NONE',  ( -127.9429263765338192, 0.000000000000000000, 9.524999999999991473 ) ) ;
#37989 = VERTEX_POINT ( 'NONE', #51433 ) ;
#37990 = CARTESIAN_POINT ( 'NONE',  ( -110.0050000000000097, 6.826472737025115478, 4.959722759717899443 ) ) ;
#37991 = VERTEX_POINT ( 'NONE', #67981 ) ;
#37992 = CARTESIAN_POINT ( 'NONE',  ( -80.49999999999995737, 50.00000000000000000, -12.00000000000000000 ) ) ;
#37993 = ORIENTED_EDGE ( 'NONE', *, *, #1855, .F. ) ;
#37994 = DIRECTION ( 'NONE',  ( 0.000000000000000000, 1.000000000000000000, 0.000000000000000000 ) ) ;
#37995 = EDGE_LOOP ( 'NONE', ( #42448, #12865, #192, #69515 ) ) ;
#37996 = ADVANCED_FACE ( 'NONE', ( #13089 ), #46193, .T. ) ;
#37997 = VERTEX_POINT ( 'NONE', #29970 ) ;
#37998 = ORIENTED_EDGE ( 'NONE', *, *, #49174, .T. ) ;
#37999 = CARTESIAN_POINT ( 'NONE',  ( -14.66964813207146889, -10.90871211463571200, 5.000000000000000888 ) ) ;
#38000 = COLOUR_RGB ( '', 0.40784314, 0.44705882, 0.49803922) ;
#38001 = CARTESIAN_POINT ( 'NONE',  ( 22.99999999999995026, 5.000000000000000000, -32.00402776293824303 ) ) ;
#38002 = ORIENTED_EDGE ( 'NONE', *, *, #64247, .T. ) ;
#38003 = CARTESIAN_POINT ( 'NONE',  ( 4.716976649647099507, 134.6429263765338362, -6.492361379858953008 ) ) ;
#38004 = VECTOR ( 'NONE', #37507, 1000.000000000000000 ) ;
#38005 = CIRCLE ( 'NONE', #14399, 0.2500000000000002220 ) ;
#38006 = DIRECTION ( 'NONE',  ( 1.000000000000000000, 0.000000000000000000, 0.000000000000000000 ) ) ;
#38007 = EDGE_CURVE ( 'NONE', #49241, #25507, #27363, .T. ) ;
#38008 = CARTESIAN_POINT ( 'NONE',  ( 0.000000000000000000, 110.7489631882669130, -8.775000000000002132 ) ) ;
#38009 = EDGE_LOOP ( 'NONE', ( #50489, #10125, #37168, #35667 ) ) ;
#38010 = LINE ( 'NONE', #4195, #48693 ) ;
#38011 = EDGE_LOOP ( 'NONE', ( #39751, #66245, #16400, #26365 ) ) ;
#38012 = DIRECTION ( 'NONE',  ( 0.000000000000000000, 1.000000000000000000, 0.000000000000000000 ) ) ;
#38013 = FILL_AREA_STYLE ('',( #11576 ) ) ;
#38015 = PRESENTATION_LAYER_ASSIGNMENT (  '', '', ( #18865 ) ) ;
#38014 =( NAMED_UNIT ( * ) SI_UNIT ( $, .STERADIAN. ) SOLID_ANGLE_UNIT ( ) );
#38016 = CARTESIAN_POINT ( 'NONE',  ( -139.7049999999999841, 2.607480562269073321, 8.024999999999991473 ) ) ;
#38017 = ADVANCED_FACE ( 'NONE', ( #30650 ), #37551, .T. ) ;
#38018 = CARTESIAN_POINT ( 'NONE',  ( -176.6070736234661354, -8.102448949553174629, 5.886773742842742685 ) ) ;
#38019 = CARTESIAN_POINT ( 'NONE',  ( -40.04190075645215785, -13.49999999999999822, 0.8979962945199000401 ) ) ;
#38020 = SURFACE_SIDE_STYLE ('',( #64013 ) ) ;
#38021 = CARTESIAN_POINT ( 'NONE',  ( 40.78947368421051323, 108.1536491499103363, 2.999999999999999112 ) ) ;
#38022 = ORIENTED_EDGE ( 'NONE', *, *, #8185, .T. ) ;
#38023 = CIRCLE ( 'NONE', #47016, 5.000000000000000000 ) ;
#38024 = EDGE_LOOP ( 'NONE', ( #15331, #33795, #52127, #50865, #15920, #17589, #13367, #39074 ) ) ;
#38025 = CARTESIAN_POINT ( 'NONE',  ( 31.00000000000001421, 43.00000000000000000, 35.50000000000000000 ) ) ;
#38026 = EDGE_CURVE ( 'NONE', #46816, #47020, #39786, .T. ) ;
#38027 = CARTESIAN_POINT ( 'NONE',  ( 0.000000000000000000, 0.000000000000000000, 7.500000000000000000 ) ) ;
#38028 = CARTESIAN_POINT ( 'NONE',  ( -53.45499999999997698, 7.632228543268599452, -2.479861379858951942 ) ) ;
#38029 = ORIENTED_EDGE ( 'NONE', *, *, #24686, .F. ) ;
#38030 = FACE_OUTER_BOUND ( 'NONE', #33396, .T. ) ;
#38031 = DIRECTION ( 'NONE',  ( -1.000000000000000000, -0.000000000000000000, -0.000000000000000000 ) ) ;
#38032 = CYLINDRICAL_SURFACE ( 'NONE', #31775, 0.5000000000000004441 ) ;
#38033 = SPHERICAL_SURFACE ( 'NONE', #63439, 1.000000000000000000 ) ;
#38034 = ORIENTED_EDGE ( 'NONE', *, *, #7085, .T. ) ;
#38035 = CARTESIAN_POINT ( 'NONE',  ( -1.000000000000028644, 1.469576158976823553E-15, -11.99999999999999645 ) ) ;
#38036 =( NAMED_UNIT ( * ) SI_UNIT ( $, .STERADIAN. ) SOLID_ANGLE_UNIT ( ) );
#38037 = SURFACE_STYLE_FILL_AREA ( #58168 ) ;
#38038 = FILL_AREA_STYLE_COLOUR ( '', #5552 ) ;
#38039 = CARTESIAN_POINT ( 'NONE',  ( -113.9949999999999903, -6.826472737025113702, 4.959722759717902107 ) ) ;
#38040 = CARTESIAN_POINT ( 'NONE',  ( 9.058813317711338797, 112.9549999999999841, -2.943386871421372675 ) ) ;
#38041 = CARTESIAN_POINT ( 'NONE',  ( -85.04499999999998749, 7.632228543268600340, 2.479861379858949277 ) ) ;
#38042 = CARTESIAN_POINT ( 'NONE',  ( -7.632228543268608334, 112.9570736234661581, 2.479861379858952830 ) ) ;
#38043 = VECTOR ( 'NONE', #9932, 1000.000000000000000 ) ;
#38044 = DIRECTION ( 'NONE',  ( 0.000000000000000000, -1.000000000000000000, 0.000000000000000000 ) ) ;
#38045 = DIRECTION ( 'NONE',  ( -0.000000000000000000, 0.000000000000000000, -1.000000000000000000 ) ) ;
#38046 = CARTESIAN_POINT ( 'NONE',  ( -167.7570736234661695, -5.598654528085801552, 7.705886871421367523 ) ) ;
#38047 = CARTESIAN_POINT ( 'NONE',  ( 16.00000000000001776, 42.00000000000000000, 35.68999999999999062 ) ) ;
#38048 = ORIENTED_EDGE ( 'NONE', *, *, #13979, .T. ) ;
#38049 = CARTESIAN_POINT ( 'NONE',  ( -122.6929263765337907, 10.01517768586948698, -1.839758294383808571E-15 ) ) ;
#38050 = SURFACE_STYLE_FILL_AREA ( #48960 ) ;
#38051 = CARTESIAN_POINT ( 'NONE',  ( -147.4449999999999932, 0.000000000000000000, 8.024999999999991473 ) ) ;
#38052 = CYLINDRICAL_SURFACE ( 'NONE', #63958, 9.524999999999991473 ) ;
#38053 = AXIS2_PLACEMENT_3D ( 'NONE', #40951, #23689, #29301 ) ;
#38054 =( GEOMETRIC_REPRESENTATION_CONTEXT ( 3 ) GLOBAL_UNCERTAINTY_ASSIGNED_CONTEXT ( ( #10080 ) ) GLOBAL_UNIT_ASSIGNED_CONTEXT ( ( #7202, #59960, #60635 ) ) REPRESENTATION_CONTEXT ( 'NONE', 'WORKASPACE' ) );
#38055 = CARTESIAN_POINT ( 'NONE',  ( -67.10707362346616378, 8.102448949553172852, -5.886773742842744461 ) ) ;
#38056 = ORIENTED_EDGE ( 'NONE', *, *, #3300, .F. ) ;
#38057 = STYLED_ITEM ( 'NONE', ( #38141 ), #14526 ) ;
#38058 = EDGE_LOOP ( 'NONE', ( #16017, #32488, #59130, #10000 ) ) ;
#38059 = CARTESIAN_POINT ( 'NONE',  ( -16.75000000000000000, 4.336808689942018722E-16, 20.00000000000000000 ) ) ;
#38060 = LINE ( 'NONE', #16599, #31956 ) ;
#38061 = MECHANICAL_DESIGN_GEOMETRIC_PRESENTATION_REPRESENTATION (  '', ( #40299 ), #66080 ) ;
#38062 = CARTESIAN_POINT ( 'NONE',  ( -132.8070736234661524, 10.01517768586948698, -1.839758294383808966E-15 ) ) ;
#38063 = LINE ( 'NONE', #22904, #32720 ) ;
#38064 = LINE ( 'NONE', #69015, #66263 ) ;
#38065 = VECTOR ( 'NONE', #14734, 1000.000000000000000 ) ;
#38066 = CARTESIAN_POINT ( 'NONE',  ( -50.75707362346618368, -5.598654528085801552, 7.705886871421367523 ) ) ;
#38067 = DIRECTION ( 'NONE',  ( -0.000000000000000000, -1.000000000000000000, -0.000000000000000000 ) ) ;
#38068 = VERTEX_POINT ( 'NONE', #25046 ) ;
#38069 = CARTESIAN_POINT ( 'NONE',  ( -137.6049999999999613, 6.826472737025113702, -4.959722759717902107 ) ) ;
#38070 = ORIENTED_EDGE ( 'NONE', *, *, #64937, .T. ) ;
#38071 = ORIENTED_EDGE ( 'NONE', *, *, #35355, .F. ) ;
#38072 = LINE ( 'NONE', #38770, #4275 ) ;
#38073 = CYLINDRICAL_SURFACE ( 'NONE', #47853, 8.025000000000000355 ) ;
#38074 = ORIENTED_EDGE ( 'NONE', *, *, #31000, .F. ) ;
#38075 = EDGE_CURVE ( 'NONE', #42335, #37934, #56618, .T. ) ;
#38076 = CARTESIAN_POINT ( 'NONE',  ( -20.08870137916957788, 4.181554945440833393, -12.05901974869650850 ) ) ;
#38077 = CARTESIAN_POINT ( 'NONE',  ( -8.102448949553181734, 134.4949999999999477, 5.886773742842747126 ) ) ;
#38078 = CARTESIAN_POINT ( 'NONE',  ( 12.00000000000001776, 14.00000000000000000, 29.68999999999999417 ) ) ;
#38079 = ADVANCED_FACE ( 'NONE', ( #24002 ), #51100, .T. ) ;
#38080 = ORIENTED_EDGE ( 'NONE', *, *, #24228, .F. ) ;
#38081 = ADVANCED_FACE ( 'NONE', ( #37031 ), #52841, .T. ) ;
#38082 = CARTESIAN_POINT ( 'NONE',  ( -95.75707362346618368, -5.598654528085801552, 7.705886871421367523 ) ) ;
#38083 = CARTESIAN_POINT ( 'NONE',  ( 5.598654528085809545, 134.2549999999999955, -7.705886871421373741 ) ) ;
#38084 = CARTESIAN_POINT ( 'NONE',  ( -62.90499999999997272, 2.607480562269069324, -8.024999999999993250 ) ) ;
#38085 = CIRCLE ( 'NONE', #33520, 15.00000000000000000 ) ;
#38086 = CARTESIAN_POINT ( 'NONE',  ( -118.4949999999999903, 6.826472737025113702, -4.959722759717902107 ) ) ;
#38087 = LINE ( 'NONE', #5324, #39746 ) ;
#38088 = ORIENTED_EDGE ( 'NONE', *, *, #23423, .T. ) ;
#38089 = CARTESIAN_POINT ( 'NONE',  ( 8.102448949553181734, 148.5049999999999955, 5.886773742842750679 ) ) ;
#38090 = CARTESIAN_POINT ( 'NONE',  ( -71.50000000000000000, 35.92875272052971525, -9.500000000000000000 ) ) ;
#38091 = DIRECTION ( 'NONE',  ( -0.000000000000000000, -1.000000000000000000, -0.000000000000000000 ) ) ;
#38092 = EDGE_CURVE ( 'NONE', #1094, #42518, #4617, .T. ) ;
#38093 = SURFACE_STYLE_USAGE ( .BOTH. , #27123 ) ;
#38094 = EDGE_CURVE ( 'NONE', #39120, #34141, #21144, .T. ) ;
#38095 = AXIS2_PLACEMENT_3D ( 'NONE', #7702, #62550, #8425 ) ;
#38096 = CARTESIAN_POINT ( 'NONE',  ( 48.74999999999999289, 24.74999999999998579, 3.750000000000000000 ) ) ;
#38097 = ORIENTED_EDGE ( 'NONE', *, *, #28886, .F. ) ;
#38098 = COLOUR_RGB ( '', 0.08235294, 0.09019608, 0.10196078) ;
#38099 = CARTESIAN_POINT ( 'NONE',  ( -33.89861118948983432, -9.947368421052630083, -2.000000000000000000 ) ) ;
#38100 = CARTESIAN_POINT ( 'NONE',  ( -169.7050000000000125, 2.607480562269073321, 8.024999999999991473 ) ) ;
#38102 = ORIENTED_EDGE ( 'NONE', *, *, #8280, .F. ) ;
#38101 = EDGE_CURVE ( 'NONE', #55126, #7860, #20821, .T. ) ;
#38103 = SURFACE_STYLE_USAGE ( .BOTH. , #64796 ) ;
#38104 = AXIS2_PLACEMENT_3D ( 'NONE', #13924, #35393, #47365 ) ;
#38105 = SURFACE_STYLE_FILL_AREA ( #33146 ) ;
#38106 = ADVANCED_FACE ( 'NONE', ( #63710 ), #12771, .T. ) ;
#38107 = FACE_OUTER_BOUND ( 'NONE', #2528, .T. ) ;
#38108 = SURFACE_STYLE_USAGE ( .BOTH. , #58486 ) ;
#38109 = PLANE ( 'NONE',  #61330 ) ;
#38110 =( BOUNDED_CURVE ( )  B_SPLINE_CURVE ( 2, ( #39072, #60463, #18626, #44703, #66094, #50286, #60807, #40104, #12630, #2009, #23530, #45042, #19651, #14365, #35834, #13677, #67855, #9813, #31223, #9461, #15107, #52716, #46071, #4135, #41145, #57280, #67487, #62547, #20701, #46795, #25952, #68901, #19285, #40792, #9111, #30527, #36581, #52029, #25602, #30180, #62209, #47478, #68198, #3785, #3066, #14035, #25274, #19977, #4485, #8422, #41475, #61848, #62892, #35494, #35137, #24914, #14736, #36211, #57638, #41844, #30889, #56591, #52387, #47118, #58000, #68542, #20340, #63260, #29855, #51321, #24556, #56940, #8755, #51668, #3420, #46431, #38296, #58665, #49176, #47844, #54419, #43579, #37264, #877, #69240, #42894, #42213, #53061, #5881, #53412, #64287, #16140, #59695, #15446, #11514, #32985, #48854, #63601, #21369, #27323, #4854, #37617, #54073, #26300, #42535, #22079, #59334, #36911, #6240, #64971, #5191, #553, #21035, #63933, #32275, #58322, #10495, #11162, #15781, #59021, #16823, #26633, #27667, #31933, #48156, #53725, #21729, #69565, #32608, #43242, #10833, #10146, #5516, #16495, #26969, #31578, #48505, #203, #64649, #37959, #1928, #11865, #45303, #43919, #61085, #23130, #33328, #7616, #65330, #13232, #2272, #54749, #23802, #50890, #44952, #66724, #22776, #34691, #6560, #34364, #28356, #22416, #18539, #66359, #6931, #17176, #56145, #18180, #38649, #40029, #60050, #7972, #29418, #61415, #12898, #28005, #55104, #49517, #7290, #1600, #1244, #60384, #49863, #12189, #44619, #50207, #44274, #28719, #65672, #33661, #29052, #17521, #39665, #38993, #66015, #55812, #17843, #39321, #23447, #60724, #12543, #55467, #34007, #50549, #13585, #2650, #4060, #30439, #9380, #63178, #45654, #25191, #40708, #51941, #46708, #52305, #41402, #25526, #67404, #9740, #8335, #15016, #68122, #19902, #20253, #47039, #62120, #62807, #41056, #19199, #57913, #31144, #24826, #67072, #13945, #14290, #36489, #51579, #14649, #35053, #24145, #30804, #67764, #18850, #56501, #56864, #68455, #35413, #40346, #29779, #61755, #36114, #8678, #30104, #3335, #3696, #51242, #57551, #41757, #2985, #24475, #46343, #45979, #19563, #62472, #35755, #57192, #9021, #31845, #37887, #63515, #15696, #37178, #5113, #68818, #47761, #113, #15375, #69487, #59254, #53333, #64567, #36829, #58244, #42815, #32204, #20964, #21644, #53650, #58587, #4397, #10417, #26886, #69156, #16745, #38210, #11078, #21283, #10067, #5438, #42124, #11432, #10756, #43161, #27239, #16413, #42458, #26562, #48083, #64203, #25871, #16059, #476, #22005, #32527, #5793, #64895, #37541, #47389, #31491, #43508, #52974, #58944, #52640, #48424, #59612, #20612, #4770, #26223, #53991, #48774, #63853, #6848, #44872, #1155, #11784, #38571, #22342, #50132, #43836, #65593, #28271, #60642, #50464, #49112, #12458, #23720, #44540, #33246, #45219, #17445, #60314, #23045, #1519, #12817, #38908, #66279, #7210, #54342, #65242, #60999, #49778, #65944, #798, #2191, #33922, #12119, #17094, #61344, #39943, #44193, #1862, #59970, #28973, #34280, #18103, #54684, #6160, #17772, #32909, #55388, #23372, #33583, #6483, #39593, #27591, #66644, #55738, #27924, #7544, #49435, #28638, #18461, #22692, #55020, #39244, #26053, #19116, #8598, #66994, #40620, #67325, #42631, #4953, #8937, #34610, #10246, #13154, #26401, #47932, #37012, #52819, #58420, #45896, #69333, #67680, #62035, #24072, #40265, #56784, #40983, #13863, #62399, #53159, #19477, #56072, #2911, #20800, #21127, #35679, #7886, #29332, #4594, #24402, #50811, #14216, #35330, #31683, #30033, #51493, #3254, #2562, #47587, #42307, #24741, #45576, #18787, #46257, #61670, #29697, #13499, #34971, #56420, #68994, #8254, #57112, #51166, #31320, #63695, #15539, #38400, #5620, #16584, #38039, #11959, #37364, #60150, #33416, #972, #64036, #43346, #49263, #5280, #27072, #48607, #59431, #10587, #59106, #11614, #26725, #11262, #17279, #300, #6328, #48247, #69662, #54172, #43670, #21834, #58770, #53497, #54845, #15880, #38743, #16917, #64741, #22873, #6664, #59803, #32036, #28104, #32717, #49609, #5982, #27759, #32360, #42986, #21476, #64390, #33081, #16238, #27421, #53821, #48949, #647, #22175, #65063, #1343, #54518, #37716, #22522, #44020, #65430, #10925, #12995, #24241, #50298, #8068, #18636, #65778, #55203, #2749, #7712, #40447, #17931, #7026, #44373, #45742, #2376, #50984, #35149, #28815, #61864, #60822, #51332, #49964, #56604, #13331, #39421, #7385, #12642, #23895, #8434, #66828, #40116, #13690, #67159, #34106, #61504, #34450, #55564, #29867, #18945, #17614, #23542, #29520, #28453, #2017, #45052, #66462, #60474, #18286, #34791, #1700, #61186, #3077, #39771, #39080, #55909, #29151, #50637, #45408, #56243, #12282, #33753, #23218, #44712, #66102, #68552, #41156, #58332, #10157, #9822, #41487, #8767, #4143, #14046, #35506, #47489, #46081, #63272, #58012, #62557, #52041, #46805, #68210, #67499, #30540, #42223, #63613, #41851, #68912, #36920, #15457, #52397, #3797, #40805, #53072, #31590, #35846, #15117, #24568, #31232, #62903, #30188, #25613, #56949, #51681, #20710, #19300, #36593, #25283, #3427, #52727, #62220, #24929, #4495, #46442, #25960, #67867, #47126, #19660, #14375, #57290, #9122, #19986, #14747, #36222, #57649, #20349, #9475, #30899, #65339, #564, #26309, #887, #4866, #17187, #38661, #27674, #43591, #53421, #10506, #63945, #22089, #15792, #37627, #42904, #59031, #64297, #32286, #32622, #43929, #59345, #47854, #16149, #11522, #60059, #27335, #69249, #11874, #10842, #38306, #48865, #21048, #37276, #32994, #37969, #22428, #48168, #58674, #42545, #6249, #54084, #54429, #33337, #31944, #64979, #53737, #5892, #16835, #5200, #59709, #69576, #5530, #26981, #49185, #26644, #21381, #48514, #211, #21742, #43253, #64659, #16503, #11175, #40355, #13594, #7300, #28017, #49873, #65683, #17852, #39330, #28728, #1255, #1611, #2282, #17531, #1939, #61424, #55478, #50898, #66369, #44628, #18190, #2661, #23138, #55113, #34700, #23811, #24156, #7983, #60733, #66735, #39001, #60394, #44962, #34373, #66025, #45313, #55821, #12551, #6572, #34017, #29061, #50217, #18862, #61765, #40035, #23456, #6940, #49526, #39676, #54759, #12908, #18550, #29427, #13244, #61098, #7627, #50559, #56156, #22786, #45661, #67077, #44286, #12197, #33671, #28365, #51590, #36126, #24838, #62481, #45989, #46354, #57925, #30450, #63187, #36501, #67413, #19209, #67774, #19574, #4068, #41067, #57561, #8685, #40719, #62129, #2992, #14300, #24482, #13956, #35764, #3707, #68465, #29791, #25202, #41766, #57200, #35424, #15027, #3345, #9032, #51950, #46719, #52315, #68132, #9391, #19911, #41414, #25532, #62817, #14657, #30816, #51251, #56508, #47046, #20261, #35061, #8346, #56874, #30112, #24377, #44847, #35303, #33890, #40597, #66971, #23344, #56762, #55358, #28943, #28239, #39214, #61647, #39565, #50435, #2162, #45871, #1487, #67304, #19091, #34947, #49749, #7519, #13475, #60614, #60968, #12787, #12429, #18766, #66251, #34255, #18078, #56040, #62010, #50784, #2535, #13839, #8227, #55711, #24045, #66617, #23694, #23016, #44512, #45194, #65916, #18432, #7181, #39918, #61322, #13133, #17744, #34585, #45549, #28609, #7854, #56392, #29306, #50106, #40243, #29673, #51141, #1835, #2885, #49278, #26741, #48622, #22895, #1362, #5634, #11629, #10603, #60164, #65446, #6345, #16258, #37381, #32734, #64049 ),
 .UNSPECIFIED., .F., .F. ) 
 B_SPLINE_CURVE_WITH_KNOTS ( ( 3, 2, 2, 2, 2, 2, 2, 2, 2, 2, 2, 2, 2, 2, 2, 2, 2, 2, 2, 2, 2, 2, 2, 2, 2, 2, 2, 2, 2, 2, 2, 2, 2, 2, 2, 2, 2, 2, 2, 2, 2, 2, 2, 2, 2, 2, 2, 2, 2, 2, 2, 2, 2, 2, 2, 2, 2, 2, 2, 2, 2, 2, 2, 2, 2, 2, 2, 2, 2, 2, 2, 2, 2, 2, 2, 2, 2, 2, 2, 2, 2, 2, 2, 2, 2, 2, 2, 2, 2, 2, 2, 2, 2, 2, 2, 2, 2, 2, 2, 2, 2, 2, 2, 2, 2, 2, 2, 2, 2, 2, 2, 2, 2, 2, 2, 2, 2, 2, 2, 2, 2, 2, 2, 2, 2, 2, 2, 2, 2, 2, 2, 2, 2, 2, 2, 2, 2, 2, 2, 2, 2, 2, 2, 2, 2, 2, 2, 2, 2, 2, 2, 2, 2, 2, 2, 2, 2, 2, 2, 2, 2, 2, 2, 2, 2, 2, 2, 2, 2, 2, 2, 2, 2, 2, 2, 2, 2, 2, 2, 2, 2, 2, 2, 2, 2, 2, 2, 2, 2, 2, 2, 2, 2, 2, 2, 2, 2, 2, 2, 2, 2, 2, 2, 2, 2, 2, 2, 2, 2, 2, 2, 2, 2, 2, 2, 2, 2, 2, 2, 2, 2, 2, 2, 2, 2, 2, 2, 2, 2, 2, 2, 2, 2, 2, 2, 2, 2, 2, 2, 2, 2, 2, 2, 2, 2, 2, 2, 2, 2, 2, 2, 2, 2, 2, 2, 2, 2, 2, 2, 2, 2, 2, 2, 2, 2, 2, 2, 2, 2, 2, 2, 2, 2, 2, 2, 2, 2, 2, 2, 2, 2, 2, 2, 2, 2, 2, 2, 2, 2, 2, 2, 2, 2, 2, 2, 2, 2, 2, 2, 2, 2, 2, 2, 2, 2, 2, 2, 2, 2, 2, 2, 2, 2, 2, 2, 2, 2, 2, 2, 2, 2, 2, 2, 2, 2, 2, 2, 2, 2, 2, 2, 2, 2, 2, 2, 2, 2, 2, 2, 2, 2, 2, 2, 2, 2, 2, 2, 2, 2, 2, 2, 2, 2, 2, 2, 2, 2, 2, 2, 2, 2, 2, 2, 2, 2, 2, 2, 2, 2, 2, 2, 2, 2, 2, 2, 2, 2, 2, 2, 2, 2, 2, 2, 2, 2, 2, 2, 2, 2, 2, 2, 2, 2, 2, 2, 2, 2, 2, 2, 2, 2, 2, 2, 2, 2, 2, 2, 2, 2, 2, 2, 2, 2, 2, 2, 2, 2, 2, 2, 2, 2, 2, 2, 2, 2, 2, 2, 2, 2, 2, 2, 2, 2, 2, 2, 2, 2, 2, 2, 2, 2, 2, 2, 2, 2, 2, 2, 2, 2, 2, 2, 2, 2, 2, 2, 2, 3 ),
 ( 0.000000000000000000, 0.002173913043478260896, 0.004347826086956521792, 0.006521739130434782254, 0.008695652173913043584, 0.01086956521739130405, 0.01304347826086956451, 0.01521739130434782671, 0.01739130434782608717, 0.01956521739130434936, 0.02173913043478260809, 0.02391304347826087029, 0.02608695652173912902, 0.02826086956521739121, 0.03043478260869565341, 0.03260869565217391214, 0.03478260869565217434, 0.03695652173913043653, 0.03913043478260869873, 0.04130434782608695399, 0.04347826086956521618, 0.04565217391304347838, 0.04782608695652174058, 0.05000000000000000278, 0.05217391304347825803, 0.05434782608695652023, 0.05652173913043478243, 0.05869565217391304462, 0.06086956521739130682, 0.06304347826086956208, 0.06521739130434782428, 0.06739130434782608647, 0.06956521739130434867, 0.07173913043478261087, 0.07391304347826087306, 0.07608695652173913526, 0.07826086956521739746, 0.08043478260869564578, 0.08260869565217390798, 0.08478260869565217017, 0.08695652173913043237, 0.08913043478260869457, 0.09130434782608695676, 0.09347826086956521896, 0.09565217391304348116, 0.09782608695652174335, 0.1000000000000000056, 0.1021739130434782677, 0.1043478260869565161, 0.1065217391304347783, 0.1086956521739130405, 0.1108695652173913027, 0.1130434782608695649, 0.1152173913043478271, 0.1173913043478260892, 0.1195652173913043514, 0.1217391304347826136, 0.1239130434782608758, 0.1260869565217391242, 0.1282608695652174002, 0.1304347826086956486, 0.1326086956521739246, 0.1347826086956521729, 0.1369565217391304213, 0.1391304347826086973, 0.1413043478260869457, 0.1434782608695652217, 0.1456521739130434701, 0.1478260869565217461, 0.1499999999999999944, 0.1521739130434782705, 0.1543478260869565188, 0.1565217391304347949, 0.1586956521739130432, 0.1608695652173912916, 0.1630434782608695676, 0.1652173913043478160, 0.1673913043478260920, 0.1695652173913043403, 0.1717391304347826164, 0.1739130434782608647, 0.1760869565217391408, 0.1782608695652173891, 0.1804347826086956652, 0.1826086956521739135, 0.1847826086956521618, 0.1869565217391304379, 0.1891304347826086862, 0.1913043478260869623, 0.1934782608695652106, 0.1956521739130434867, 0.1978260869565217350, 0.2000000000000000111, 0.2021739130434782594, 0.2043478260869565355, 0.2065217391304347838, 0.2086956521739130321, 0.2108695652173913082, 0.2130434782608695565, 0.2152173913043478326, 0.2173913043478260809, 0.2195652173913043570, 0.2217391304347826053, 0.2239130434782608814, 0.2260869565217391297, 0.2282608695652173780, 0.2304347826086956541, 0.2326086956521739024, 0.2347826086956521785, 0.2369565217391304268, 0.2391304347826087029, 0.2413043478260869512, 0.2434782608695652273, 0.2456521739130434756, 0.2478260869565217517, 0.2500000000000000000, 0.2521739130434782483, 0.2543478260869564966, 0.2565217391304348005, 0.2586956521739130488, 0.2608695652173912971, 0.2630434782608695454, 0.2652173913043478493, 0.2673913043478260976, 0.2695652173913043459, 0.2717391304347825942, 0.2739130434782608425, 0.2760869565217391464, 0.2782608695652173947, 0.2804347826086956430, 0.2826086956521738913, 0.2847826086956521952, 0.2869565217391304435, 0.2891304347826086918, 0.2913043478260869401, 0.2934782608695652439, 0.2956521739130434923, 0.2978260869565217406, 0.2999999999999999889, 0.3021739130434782372, 0.3043478260869565410, 0.3065217391304347894, 0.3086956521739130377, 0.3108695652173912860, 0.3130434782608695898, 0.3152173913043478382, 0.3173913043478260865, 0.3195652173913043348, 0.3217391304347825831, 0.3239130434782608869, 0.3260869565217391353, 0.3282608695652173836, 0.3304347826086956319, 0.3326086956521739357, 0.3347826086956521840, 0.3369565217391304324, 0.3391304347826086807, 0.3413043478260869290, 0.3434782608695652328, 0.3456521739130434812, 0.3478260869565217295, 0.3499999999999999778, 0.3521739130434782816, 0.3543478260869565299, 0.3565217391304347783, 0.3586956521739130266, 0.3608695652173913304, 0.3630434782608695787, 0.3652173913043478271, 0.3673913043478260754, 0.3695652173913043237, 0.3717391304347826275, 0.3739130434782608758, 0.3760869565217391242, 0.3782608695652173725, 0.3804347826086956763, 0.3826086956521739246, 0.3847826086956521729, 0.3869565217391304213, 0.3891304347826086696, 0.3913043478260869734, 0.3934782608695652217, 0.3956521739130434701, 0.3978260869565217184, 0.4000000000000000222, 0.4021739130434782705, 0.4043478260869565188, 0.4065217391304347672, 0.4086956521739130710, 0.4108695652173913193, 0.4130434782608695676, 0.4152173913043478160, 0.4173913043478260643, 0.4195652173913043681, 0.4217391304347826164, 0.4239130434782608647, 0.4260869565217391131, 0.4282608695652174169, 0.4304347826086956652, 0.4326086956521739135, 0.4347826086956521618, 0.4369565217391304102, 0.4391304347826087140, 0.4413043478260869623, 0.4434782608695652106, 0.4456521739130434590, 0.4478260869565217628, 0.4500000000000000111, 0.4521739130434782594, 0.4543478260869565077, 0.4565217391304347561, 0.4586956521739130599, 0.4608695652173913082, 0.4630434782608695565, 0.4652173913043478048, 0.4673913043478261087, 0.4695652173913043570, 0.4717391304347826053, 0.4739130434782608536, 0.4760869565217391575, 0.4782608695652174058, 0.4804347826086956541, 0.4826086956521739024, 0.4847826086956521507, 0.4869565217391304546, 0.4891304347826087029, 0.4913043478260869512, 0.4934782608695651995, 0.4956521739130435034, 0.4978260869565217517, 0.5000000000000000000, 0.5021739130434782483, 0.5043478260869564966, 0.5065217391304347450, 0.5086956521739129933, 0.5108695652173913526, 0.5130434782608696009, 0.5152173913043478493, 0.5173913043478260976, 0.5195652173913043459, 0.5217391304347825942, 0.5239130434782608425, 0.5260869565217390909, 0.5282608695652173392, 0.5304347826086956985, 0.5326086956521739468, 0.5347826086956521952, 0.5369565217391304435, 0.5391304347826086918, 0.5413043478260869401, 0.5434782608695651884, 0.5456521739130434367, 0.5478260869565216851, 0.5500000000000000444, 0.5521739130434782927, 0.5543478260869565410, 0.5565217391304347894, 0.5586956521739130377, 0.5608695652173912860, 0.5630434782608695343, 0.5652173913043477826, 0.5673913043478261420, 0.5695652173913043903, 0.5717391304347826386, 0.5739130434782608869, 0.5760869565217391353, 0.5782608695652173836, 0.5804347826086956319, 0.5826086956521738802, 0.5847826086956521285, 0.5869565217391304879, 0.5891304347826087362, 0.5913043478260869845, 0.5934782608695652328, 0.5956521739130434812, 0.5978260869565217295, 0.5999999999999999778, 0.6021739130434782261, 0.6043478260869564744, 0.6065217391304348338, 0.6086956521739130821, 0.6108695652173913304, 0.6130434782608695787, 0.6152173913043478271, 0.6173913043478260754, 0.6195652173913043237, 0.6217391304347825720, 0.6239130434782608203, 0.6260869565217391797, 0.6282608695652174280, 0.6304347826086956763, 0.6326086956521739246, 0.6347826086956521729, 0.6369565217391304213, 0.6391304347826086696, 0.6413043478260869179, 0.6434782608695651662, 0.6456521739130435256, 0.6478260869565217739, 0.6500000000000000222, 0.6521739130434782705, 0.6543478260869565188, 0.6565217391304347672, 0.6586956521739130155, 0.6608695652173912638, 0.6630434782608695121, 0.6652173913043478715, 0.6673913043478261198, 0.6695652173913043681, 0.6717391304347826164, 0.6739130434782608647, 0.6760869565217391131, 0.6782608695652173614, 0.6804347826086956097, 0.6826086956521738580, 0.6847826086956522174, 0.6869565217391304657, 0.6891304347826087140, 0.6913043478260869623, 0.6934782608695652106, 0.6956521739130434590, 0.6978260869565217073, 0.6999999999999999556, 0.7021739130434783149, 0.7043478260869565633, 0.7065217391304348116, 0.7086956521739130599, 0.7108695652173913082, 0.7130434782608695565, 0.7152173913043478048, 0.7173913043478260532, 0.7195652173913043015, 0.7217391304347826608, 0.7239130434782609091, 0.7260869565217391575, 0.7282608695652174058, 0.7304347826086956541, 0.7326086956521739024, 0.7347826086956521507, 0.7369565217391303991, 0.7391304347826086474, 0.7413043478260870067, 0.7434782608695652550, 0.7456521739130435034, 0.7478260869565217517, 0.7500000000000000000, 0.7521739130434782483, 0.7543478260869564966, 0.7565217391304347450, 0.7586956521739129933, 0.7608695652173913526, 0.7630434782608696009, 0.7652173913043478493, 0.7673913043478260976, 0.7695652173913043459, 0.7717391304347825942, 0.7739130434782608425, 0.7760869565217390909, 0.7782608695652173392, 0.7804347826086956985, 0.7826086956521739468, 0.7847826086956521952, 0.7869565217391304435, 0.7891304347826086918, 0.7913043478260869401, 0.7934782608695651884, 0.7956521739130434367, 0.7978260869565216851, 0.8000000000000000444, 0.8021739130434782927, 0.8043478260869565410, 0.8065217391304347894, 0.8086956521739130377, 0.8108695652173912860, 0.8130434782608695343, 0.8152173913043477826, 0.8173913043478261420, 0.8195652173913043903, 0.8217391304347826386, 0.8239130434782608869, 0.8260869565217391353, 0.8282608695652173836, 0.8304347826086956319, 0.8326086956521738802, 0.8347826086956521285, 0.8369565217391304879, 0.8391304347826087362, 0.8413043478260869845, 0.8434782608695652328, 0.8456521739130434812, 0.8478260869565217295, 0.8499999999999999778, 0.8521739130434782261, 0.8543478260869564744, 0.8565217391304348338, 0.8586956521739130821, 0.8608695652173913304, 0.8630434782608695787, 0.8652173913043478271, 0.8673913043478260754, 0.8695652173913043237, 0.8717391304347825720, 0.8739130434782608203, 0.8760869565217391797, 0.8782608695652174280, 0.8804347826086956763, 0.8826086956521739246, 0.8847826086956521729, 0.8869565217391304213, 0.8891304347826086696, 0.8913043478260869179, 0.8934782608695651662, 0.8956521739130435256, 0.8978260869565217739, 0.9000000000000000222, 0.9021739130434782705, 0.9043478260869565188, 0.9065217391304347672, 0.9086956521739130155, 0.9108695652173912638, 0.9130434782608695121, 0.9152173913043478715, 0.9173913043478261198, 0.9195652173913043681, 0.9217391304347826164, 0.9239130434782608647, 0.9260869565217391131, 0.9282608695652173614, 0.9304347826086956097, 0.9326086956521738580, 0.9347826086956522174, 0.9369565217391304657, 0.9391304347826087140, 0.9413043478260869623, 0.9434782608695652106, 0.9456521739130434590, 0.9478260869565217073, 0.9499999999999999556, 0.9521739130434783149, 0.9543478260869565633, 0.9565217391304348116, 0.9586956521739130599, 0.9608695652173913082, 0.9630434782608695565, 0.9652173913043478048, 0.9673913043478260532, 0.9695652173913043015, 0.9717391304347826608, 0.9739130434782609091, 0.9760869565217391575, 0.9782608695652174058, 0.9804347826086956541, 0.9826086956521739024, 0.9847826086956521507, 0.9869565217391303991, 0.9891304347826086474, 0.9913043478260870067 ),
 .UNSPECIFIED. ) 
 CURVE ( )  GEOMETRIC_REPRESENTATION_ITEM ( )  RATIONAL_B_SPLINE_CURVE ( ( 1.000000000000000000, 0.9510565162951535312, 1.000000000000000000, 0.9510565162951535312, 1.000000000000000000, 0.9510565162951535312, 1.000000000000000000, 0.9510565162951535312, 1.000000000000000000, 0.9510565162951535312, 1.000000000000000000, 0.9510565162951535312, 1.000000000000000000, 0.9510565162951535312, 1.000000000000000000, 0.9510565162951535312, 1.000000000000000000, 0.9510565162951535312, 1.000000000000000000, 0.9510565162951535312, 1.000000000000000000, 0.9510565162951535312, 1.000000000000000000, 0.9510565162951535312, 1.000000000000000000, 0.9510565162951535312, 1.000000000000000000, 0.9510565162951535312, 1.000000000000000000, 0.9510565162951535312, 1.000000000000000000, 0.9510565162951535312, 1.000000000000000000, 0.9510565162951535312, 1.000000000000000000, 0.9510565162951535312, 1.000000000000000000, 0.9510565162951535312, 1.000000000000000000, 0.9510565162951535312, 1.000000000000000000, 0.9510565162951535312, 1.000000000000000000, 0.9510565162951535312, 1.000000000000000000, 0.9510565162951535312, 1.000000000000000000, 0.9510565162951535312, 1.000000000000000000, 0.9510565162951535312, 1.000000000000000000, 0.9510565162951535312, 1.000000000000000000, 0.9510565162951535312, 1.000000000000000000, 0.9510565162951535312, 1.000000000000000000, 0.9510565162951535312, 1.000000000000000000, 0.9510565162951535312, 1.000000000000000000, 0.9510565162951535312, 1.000000000000000000, 0.9510565162951535312, 1.000000000000000000, 0.9510565162951535312, 1.000000000000000000, 0.9510565162951535312, 1.000000000000000000, 0.9510565162951535312, 1.000000000000000000, 0.9510565162951535312, 1.000000000000000000, 0.9510565162951535312, 1.000000000000000000, 0.9510565162951535312, 1.000000000000000000, 0.9510565162951535312, 1.000000000000000000, 0.9510565162951535312, 1.000000000000000000, 0.9510565162951535312, 1.000000000000000000, 0.9510565162951535312, 1.000000000000000000, 0.9510565162951535312, 1.000000000000000000, 0.9510565162951535312, 1.000000000000000000, 0.9510565162951535312, 1.000000000000000000, 0.9510565162951535312, 1.000000000000000000, 0.9510565162951535312, 1.000000000000000000, 0.9510565162951535312, 1.000000000000000000, 0.9510565162951535312, 1.000000000000000000, 0.9510565162951535312, 1.000000000000000000, 0.9510565162951535312, 1.000000000000000000, 0.9510565162951535312, 1.000000000000000000, 0.9510565162951535312, 1.000000000000000000, 0.9510565162951535312, 1.000000000000000000, 0.9510565162951535312, 1.000000000000000000, 0.9510565162951535312, 1.000000000000000000, 0.9510565162951535312, 1.000000000000000000, 0.9510565162951535312, 1.000000000000000000, 0.9510565162951535312, 1.000000000000000000, 0.9510565162951535312, 1.000000000000000000, 0.9510565162951535312, 1.000000000000000000, 0.9510565162951535312, 1.000000000000000000, 0.9510565162951535312, 1.000000000000000000, 0.9510565162951535312, 1.000000000000000000, 0.9510565162951535312, 1.000000000000000000, 0.9510565162951535312, 1.000000000000000000, 0.9510565162951535312, 1.000000000000000000, 0.9510565162951535312, 1.000000000000000000, 0.9510565162951535312, 1.000000000000000000, 0.9510565162951535312, 1.000000000000000000, 0.9510565162951535312, 1.000000000000000000, 0.9510565162951535312, 1.000000000000000000, 0.9510565162951535312, 1.000000000000000000, 0.9510565162951535312, 1.000000000000000000, 0.9510565162951535312, 1.000000000000000000, 0.9510565162951535312, 1.000000000000000000, 0.9510565162951535312, 1.000000000000000000, 0.9510565162951535312, 1.000000000000000000, 0.9510565162951535312, 1.000000000000000000, 0.9510565162951535312, 1.000000000000000000, 0.9510565162951535312, 1.000000000000000000, 0.9510565162951535312, 1.000000000000000000, 0.9510565162951535312, 1.000000000000000000, 0.9510565162951535312, 1.000000000000000000, 0.9510565162951535312, 1.000000000000000000, 0.9510565162951535312, 1.000000000000000000, 0.9510565162951535312, 1.000000000000000000, 0.9510565162951535312, 1.000000000000000000, 0.9510565162951535312, 1.000000000000000000, 0.9510565162951535312, 1.000000000000000000, 0.9510565162951535312, 1.000000000000000000, 0.9510565162951535312, 1.000000000000000000, 0.9510565162951535312, 1.000000000000000000, 0.9510565162951535312, 1.000000000000000000, 0.9510565162951535312, 1.000000000000000000, 0.9510565162951535312, 1.000000000000000000, 0.9510565162951535312, 1.000000000000000000, 0.9510565162951535312, 1.000000000000000000, 0.9510565162951535312, 1.000000000000000000, 0.9510565162951535312, 1.000000000000000000, 0.9510565162951535312, 1.000000000000000000, 0.9510565162951535312, 1.000000000000000000, 0.9510565162951535312, 1.000000000000000000, 0.9510565162951535312, 1.000000000000000000, 0.9510565162951535312, 1.000000000000000000, 0.9510565162951535312, 1.000000000000000000, 0.9510565162951535312, 1.000000000000000000, 0.9510565162951535312, 1.000000000000000000, 0.9510565162951535312, 1.000000000000000000, 0.9510565162951535312, 1.000000000000000000, 0.9510565162951535312, 1.000000000000000000, 0.9510565162951535312, 1.000000000000000000, 0.9510565162951535312, 1.000000000000000000, 0.9510565162951535312, 1.000000000000000000, 0.9510565162951535312, 1.000000000000000000, 0.9510565162951535312, 1.000000000000000000, 0.9510565162951535312, 1.000000000000000000, 0.9510565162951535312, 1.000000000000000000, 0.9510565162951535312, 1.000000000000000000, 0.9510565162951535312, 1.000000000000000000, 0.9510565162951535312, 1.000000000000000000, 0.9510565162951535312, 1.000000000000000000, 0.9510565162951535312, 1.000000000000000000, 0.9510565162951535312, 1.000000000000000000, 0.9510565162951535312, 1.000000000000000000, 0.9510565162951535312, 1.000000000000000000, 0.9510565162951535312, 1.000000000000000000, 0.9510565162951535312, 1.000000000000000000, 0.9510565162951535312, 1.000000000000000000, 0.9510565162951535312, 1.000000000000000000, 0.9510565162951535312, 1.000000000000000000, 0.9510565162951535312, 1.000000000000000000, 0.9510565162951535312, 1.000000000000000000, 0.9510565162951535312, 1.000000000000000000, 0.9510565162951535312, 1.000000000000000000, 0.9510565162951535312, 1.000000000000000000, 0.9510565162951535312, 1.000000000000000000, 0.9510565162951535312, 1.000000000000000000, 0.9510565162951535312, 1.000000000000000000, 0.9510565162951535312, 1.000000000000000000, 0.9510565162951535312, 1.000000000000000000, 0.9510565162951535312, 1.000000000000000000, 0.9510565162951535312, 1.000000000000000000, 0.9510565162951535312, 1.000000000000000000, 0.9510565162951535312, 1.000000000000000000, 0.9510565162951535312, 1.000000000000000000, 0.9510565162951535312, 1.000000000000000000, 0.9510565162951535312, 1.000000000000000000, 0.9510565162951535312, 1.000000000000000000, 0.9510565162951535312, 1.000000000000000000, 0.9510565162951535312, 1.000000000000000000, 0.9510565162951535312, 1.000000000000000000, 0.9510565162951535312, 1.000000000000000000, 0.9510565162951535312, 1.000000000000000000, 0.9510565162951535312, 1.000000000000000000, 0.9510565162951535312, 1.000000000000000000, 0.9510565162951535312, 1.000000000000000000, 0.9510565162951535312, 1.000000000000000000, 0.9510565162951535312, 1.000000000000000000, 0.9510565162951535312, 1.000000000000000000, 0.9510565162951535312, 1.000000000000000000, 0.9510565162951535312, 1.000000000000000000, 0.9510565162951535312, 1.000000000000000000, 0.9510565162951535312, 1.000000000000000000, 0.9510565162951535312, 1.000000000000000000, 0.9510565162951535312, 1.000000000000000000, 0.9510565162951535312, 1.000000000000000000, 0.9510565162951535312, 1.000000000000000000, 0.9510565162951535312, 1.000000000000000000, 0.9510565162951535312, 1.000000000000000000, 0.9510565162951535312, 1.000000000000000000, 0.9510565162951535312, 1.000000000000000000, 0.9510565162951535312, 1.000000000000000000, 0.9510565162951535312, 1.000000000000000000, 0.9510565162951535312, 1.000000000000000000, 0.9510565162951535312, 1.000000000000000000, 0.9510565162951535312, 1.000000000000000000, 0.9510565162951535312, 1.000000000000000000, 0.9510565162951535312, 1.000000000000000000, 0.9510565162951535312, 1.000000000000000000, 0.9510565162951535312, 1.000000000000000000, 0.9510565162951535312, 1.000000000000000000, 0.9510565162951535312, 1.000000000000000000, 0.9510565162951535312, 1.000000000000000000, 0.9510565162951535312, 1.000000000000000000, 0.9510565162951535312, 1.000000000000000000, 0.9510565162951535312, 1.000000000000000000, 0.9510565162951535312, 1.000000000000000000, 0.9510565162951535312, 1.000000000000000000, 0.9510565162951535312, 1.000000000000000000, 0.9510565162951535312, 1.000000000000000000, 0.9510565162951535312, 1.000000000000000000, 0.9510565162951535312, 1.000000000000000000, 0.9510565162951535312, 1.000000000000000000, 0.9510565162951535312, 1.000000000000000000, 0.9510565162951535312, 1.000000000000000000, 0.9510565162951535312, 1.000000000000000000, 0.9510565162951535312, 1.000000000000000000, 0.9510565162951535312, 1.000000000000000000, 0.9510565162951535312, 1.000000000000000000, 0.9510565162951535312, 1.000000000000000000, 0.9510565162951535312, 1.000000000000000000, 0.9510565162951535312, 1.000000000000000000, 0.9510565162951535312, 1.000000000000000000, 0.9510565162951535312, 1.000000000000000000, 0.9510565162951535312, 1.000000000000000000, 0.9510565162951535312, 1.000000000000000000, 0.9510565162951535312, 1.000000000000000000, 0.9510565162951535312, 1.000000000000000000, 0.9510565162951535312, 1.000000000000000000, 0.9510565162951535312, 1.000000000000000000, 0.9510565162951535312, 1.000000000000000000, 0.9510565162951535312, 1.000000000000000000, 0.9510565162951535312, 1.000000000000000000, 0.9510565162951535312, 1.000000000000000000, 0.9510565162951535312, 1.000000000000000000, 0.9510565162951535312, 1.000000000000000000, 0.9510565162951535312, 1.000000000000000000, 0.9510565162951535312, 1.000000000000000000, 0.9510565162951535312, 1.000000000000000000, 0.9510565162951535312, 1.000000000000000000, 0.9510565162951535312, 1.000000000000000000, 0.9510565162951535312, 1.000000000000000000, 0.9510565162951535312, 1.000000000000000000, 0.9510565162951535312, 1.000000000000000000, 0.9510565162951535312, 1.000000000000000000, 0.9510565162951535312, 1.000000000000000000, 0.9510565162951535312, 1.000000000000000000, 0.9510565162951535312, 1.000000000000000000, 0.9510565162951535312, 1.000000000000000000, 0.9510565162951535312, 1.000000000000000000, 0.9510565162951535312, 1.000000000000000000, 0.9510565162951535312, 1.000000000000000000, 0.9510565162951535312, 1.000000000000000000, 0.9510565162951535312, 1.000000000000000000, 0.9510565162951535312, 1.000000000000000000, 0.9510565162951535312, 1.000000000000000000, 0.9510565162951535312, 1.000000000000000000, 0.9510565162951535312, 1.000000000000000000, 0.9510565162951535312, 1.000000000000000000, 0.9510565162951535312, 1.000000000000000000, 0.9510565162951535312, 1.000000000000000000, 0.9510565162951535312, 1.000000000000000000, 0.9510565162951535312, 1.000000000000000000, 0.9510565162951535312, 1.000000000000000000, 0.9510565162951535312, 1.000000000000000000, 0.9510565162951535312, 1.000000000000000000, 0.9510565162951535312, 1.000000000000000000, 0.9510565162951535312, 1.000000000000000000, 0.9510565162951535312, 1.000000000000000000, 0.9510565162951535312, 1.000000000000000000, 0.9510565162951535312, 1.000000000000000000, 0.9510565162951535312, 1.000000000000000000, 0.9510565162951535312, 1.000000000000000000, 0.9510565162951535312, 1.000000000000000000, 0.9510565162951535312, 1.000000000000000000, 0.9510565162951535312, 1.000000000000000000, 0.9510565162951535312, 1.000000000000000000, 0.9510565162951535312, 1.000000000000000000, 0.9510565162951535312, 1.000000000000000000, 0.9510565162951535312, 1.000000000000000000, 0.9510565162951535312, 1.000000000000000000, 0.9510565162951535312, 1.000000000000000000, 0.9510565162951535312, 1.000000000000000000, 0.9510565162951535312, 1.000000000000000000, 0.9510565162951535312, 1.000000000000000000, 0.9510565162951535312, 1.000000000000000000, 0.9510565162951535312, 1.000000000000000000, 0.9510565162951535312, 1.000000000000000000, 0.9510565162951535312, 1.000000000000000000, 0.9510565162951535312, 1.000000000000000000, 0.9510565162951535312, 1.000000000000000000, 0.9510565162951535312, 1.000000000000000000, 0.9510565162951535312, 1.000000000000000000, 0.9510565162951535312, 1.000000000000000000, 0.9510565162951535312, 1.000000000000000000, 0.9510565162951535312, 1.000000000000000000, 0.9510565162951535312, 1.000000000000000000, 0.9510565162951535312, 1.000000000000000000, 0.9510565162951535312, 1.000000000000000000, 0.9510565162951535312, 1.000000000000000000, 0.9510565162951535312, 1.000000000000000000, 0.9510565162951535312, 1.000000000000000000, 0.9510565162951535312, 1.000000000000000000, 0.9510565162951535312, 1.000000000000000000, 0.9510565162951535312, 1.000000000000000000, 0.9510565162951535312, 1.000000000000000000, 0.9510565162951535312, 1.000000000000000000, 0.9510565162951535312, 1.000000000000000000, 0.9510565162951535312, 1.000000000000000000, 0.9510565162951535312, 1.000000000000000000, 0.9510565162951535312, 1.000000000000000000, 0.9510565162951535312, 1.000000000000000000, 0.9510565162951535312, 1.000000000000000000, 0.9510565162951535312, 1.000000000000000000, 0.9510565162951535312, 1.000000000000000000, 0.9510565162951535312, 1.000000000000000000, 0.9510565162951535312, 1.000000000000000000, 0.9510565162951535312, 1.000000000000000000, 0.9510565162951535312, 1.000000000000000000, 0.9510565162951535312, 1.000000000000000000, 0.9510565162951535312, 1.000000000000000000, 0.9510565162951535312, 1.000000000000000000, 0.9510565162951535312, 1.000000000000000000, 0.9510565162951535312, 1.000000000000000000, 0.9510565162951535312, 1.000000000000000000, 0.9510565162951535312, 1.000000000000000000, 0.9510565162951535312, 1.000000000000000000, 0.9510565162951535312, 1.000000000000000000, 0.9510565162951535312, 1.000000000000000000, 0.9510565162951535312, 1.000000000000000000, 0.9510565162951535312, 1.000000000000000000, 0.9510565162951535312, 1.000000000000000000, 0.9510565162951535312, 1.000000000000000000, 0.9510565162951535312, 1.000000000000000000, 0.9510565162951535312, 1.000000000000000000, 0.9510565162951535312, 1.000000000000000000, 0.9510565162951535312, 1.000000000000000000, 0.9510565162951535312, 1.000000000000000000, 0.9510565162951535312, 1.000000000000000000, 0.9510565162951535312, 1.000000000000000000, 0.9510565162951535312, 1.000000000000000000, 0.9510565162951535312, 1.000000000000000000, 0.9510565162951535312, 1.000000000000000000, 0.9510565162951535312, 1.000000000000000000, 0.9510565162951535312, 1.000000000000000000, 0.9510565162951535312, 1.000000000000000000, 0.9510565162951535312, 1.000000000000000000, 0.9510565162951535312, 1.000000000000000000, 0.9510565162951535312, 1.000000000000000000, 0.9510565162951535312, 1.000000000000000000, 0.9510565162951535312, 1.000000000000000000, 0.9510565162951535312, 1.000000000000000000, 0.9510565162951535312, 1.000000000000000000, 0.9510565162951535312, 1.000000000000000000, 0.9510565162951535312, 1.000000000000000000, 0.9510565162951535312, 1.000000000000000000, 0.9510565162951535312, 1.000000000000000000, 0.9510565162951535312, 1.000000000000000000, 0.9510565162951535312, 1.000000000000000000, 0.9510565162951535312, 1.000000000000000000, 0.9510565162951535312, 1.000000000000000000, 0.9510565162951535312, 1.000000000000000000, 0.9510565162951535312, 1.000000000000000000, 0.9510565162951535312, 1.000000000000000000, 0.9510565162951535312, 1.000000000000000000, 0.9510565162951535312, 1.000000000000000000, 0.9510565162951535312, 1.000000000000000000, 0.9510565162951535312, 1.000000000000000000, 0.9510565162951535312, 1.000000000000000000, 0.9510565162951535312, 1.000000000000000000, 0.9510565162951535312, 1.000000000000000000, 0.9510565162951535312, 1.000000000000000000, 0.9510565162951535312, 1.000000000000000000, 0.9510565162951535312, 1.000000000000000000, 0.9510565162951535312, 1.000000000000000000, 0.9510565162951535312, 1.000000000000000000, 0.9510565162951535312, 1.000000000000000000, 0.9510565162951535312, 1.000000000000000000, 0.9510565162951535312, 1.000000000000000000, 0.9510565162951535312, 1.000000000000000000, 0.9510565162951535312, 1.000000000000000000, 0.9510565162951535312, 1.000000000000000000, 0.9510565162951535312, 1.000000000000000000, 0.9510565162951535312, 1.000000000000000000, 0.9510565162951535312, 1.000000000000000000, 0.9510565162951535312, 1.000000000000000000, 0.9510565162951535312, 1.000000000000000000, 0.9510565162951535312, 1.000000000000000000, 0.9510565162951535312, 1.000000000000000000, 0.9510565162951535312, 1.000000000000000000, 0.9510565162951535312, 1.000000000000000000, 0.9510565162951535312, 1.000000000000000000, 0.9510565162951535312, 1.000000000000000000, 0.9510565162951535312, 1.000000000000000000, 0.9510565162951535312, 1.000000000000000000, 0.9510565162951535312, 1.000000000000000000, 0.9510565162951535312, 1.000000000000000000, 0.9510565162951535312, 1.000000000000000000, 0.9510565162951535312, 1.000000000000000000, 0.9510565162951535312, 1.000000000000000000, 0.9510565162951535312, 1.000000000000000000, 0.9510565162951535312, 1.000000000000000000, 0.9510565162951535312, 1.000000000000000000, 0.9510565162951535312, 1.000000000000000000, 0.9510565162951535312, 1.000000000000000000, 0.9510565162951535312, 1.000000000000000000, 0.9510565162951535312, 1.000000000000000000, 0.9510565162951535312, 1.000000000000000000, 0.9510565162951535312, 1.000000000000000000, 0.9510565162951535312, 1.000000000000000000, 0.9510565162951535312, 1.000000000000000000, 0.9510565162951535312, 1.000000000000000000, 0.9510565162951535312, 1.000000000000000000, 0.9510565162951535312, 1.000000000000000000, 0.9510565162951535312, 1.000000000000000000, 0.9510565162951535312, 1.000000000000000000, 0.9510565162951535312, 1.000000000000000000, 0.9510565162951535312, 1.000000000000000000, 0.9510565162951535312, 1.000000000000000000, 0.9510565162951535312, 1.000000000000000000, 0.9510565162951535312, 1.000000000000000000, 0.9510565162951535312, 1.000000000000000000, 0.9510565162951535312, 1.000000000000000000, 0.9510565162951535312, 1.000000000000000000, 0.9510565162951535312, 1.000000000000000000, 0.9510565162951535312, 1.000000000000000000, 0.9510565162951535312, 1.000000000000000000, 0.9510565162951535312, 1.000000000000000000, 0.9510565162951535312, 1.000000000000000000, 0.9510565162951535312, 1.000000000000000000, 0.9510565162951535312, 1.000000000000000000, 0.9510565162951535312, 1.000000000000000000, 0.9510565162951535312, 1.000000000000000000, 0.9510565162951535312, 1.000000000000000000, 0.9510565162951535312, 1.000000000000000000, 0.9510565162951535312, 1.000000000000000000, 0.9510565162951535312, 1.000000000000000000, 0.9510565162951535312, 1.000000000000000000, 0.9510565162951535312, 1.000000000000000000, 0.9510565162951535312, 1.000000000000000000, 0.9510565162951535312, 1.000000000000000000, 0.9510565162951535312, 1.000000000000000000, 0.9510565162951535312, 1.000000000000000000, 0.9510565162951535312, 1.000000000000000000, 0.9510565162951535312, 1.000000000000000000, 0.9510565162951535312, 1.000000000000000000, 0.9510565162951535312, 1.000000000000000000, 0.9510565162951535312, 1.000000000000000000, 0.9510565162951535312, 1.000000000000000000, 0.9510565162951535312, 1.000000000000000000, 0.9510565162951535312, 1.000000000000000000, 0.9510565162951535312, 1.000000000000000000, 0.9510565162951535312, 1.000000000000000000, 0.9510565162951535312, 1.000000000000000000, 0.9510565162951535312, 1.000000000000000000, 0.9510565162951535312, 1.000000000000000000, 0.9510565162951535312, 1.000000000000000000, 0.9510565162951535312, 1.000000000000000000, 0.9510565162951535312, 1.000000000000000000, 0.9510565162951535312, 1.000000000000000000, 0.9510565162951535312, 1.000000000000000000, 0.9510565162951535312, 1.000000000000000000, 0.9510565162951535312, 1.000000000000000000, 0.9510565162951535312, 1.000000000000000000, 0.9510565162951535312, 1.000000000000000000, 0.9510565162951535312, 1.000000000000000000, 0.9510565162951535312, 1.000000000000000000, 0.9510565162951535312, 1.000000000000000000, 0.9510565162951535312, 1.000000000000000000, 0.9510565162951535312, 1.000000000000000000, 0.9510565162951535312, 1.000000000000000000, 0.9510565162951535312, 1.000000000000000000, 0.9510565162951535312, 1.000000000000000000, 0.9510565162951535312, 1.000000000000000000, 0.9510565162951535312, 1.000000000000000000 ) ) 
 REPRESENTATION_ITEM ( '' )  );
#38111 = ORIENTED_EDGE ( 'NONE', *, *, #48601, .T. ) ;
#38112 = CIRCLE ( 'NONE', #53819, 4.999999999999997335 ) ;
#38113 =( GEOMETRIC_REPRESENTATION_CONTEXT ( 3 ) GLOBAL_UNCERTAINTY_ASSIGNED_CONTEXT ( ( #36131 ) ) GLOBAL_UNIT_ASSIGNED_CONTEXT ( ( #53572, #5358, #26799 ) ) REPRESENTATION_CONTEXT ( 'NONE', 'WORKASPACE' ) );
#38114 = SURFACE_STYLE_USAGE ( .BOTH. , #32105 ) ;
#38115 = CARTESIAN_POINT ( 'NONE',  ( -89.60499999999997556, 6.826472737025113702, -4.959722759717902107 ) ) ;
#38116 = VERTEX_POINT ( 'NONE', #15559 ) ;
#38117 = CYLINDRICAL_SURFACE ( 'NONE', #4773, 5.000000000000004441 ) ;
#38118 = DIRECTION ( 'NONE',  ( 1.000000000000000000, 0.000000000000000000, 0.000000000000000000 ) ) ;
#38119 =( GEOMETRIC_REPRESENTATION_CONTEXT ( 3 ) GLOBAL_UNCERTAINTY_ASSIGNED_CONTEXT ( ( #21445 ) ) GLOBAL_UNIT_ASSIGNED_CONTEXT ( ( #59607, #48768, #468 ) ) REPRESENTATION_CONTEXT ( 'NONE', 'WORKASPACE' ) );
#38120 = DIRECTION ( 'NONE',  ( 0.000000000000000000, 0.000000000000000000, -1.000000000000000000 ) ) ;
#38121 = DIRECTION ( 'NONE',  ( -1.000000000000000000, 0.000000000000000000, 0.000000000000000000 ) ) ;
#38122 = CARTESIAN_POINT ( 'NONE',  ( -66.20707362346615810, 3.094860106618433360, 9.524999999999991473 ) ) ;
#38123 = COLOUR_RGB ( '', 0.09019608, 0.27058824, 0.51372549) ;
#38124 = FACE_OUTER_BOUND ( 'NONE', #67098, .T. ) ;
#38125 = VERTEX_POINT ( 'NONE', #47242 ) ;
#38126 = DIRECTION ( 'NONE',  ( 0.000000000000000000, 0.000000000000000000, -1.000000000000000000 ) ) ;
#38127 = COLOUR_RGB ( '', 0.66274510, 0.83137255, 0.94901961) ;
#38128 = CARTESIAN_POINT ( 'NONE',  ( -102.8049999999999784, -8.437984349512085203, 5.166775262442717831E-16 ) ) ;
#38129 = CARTESIAN_POINT ( 'NONE',  ( -5.598654528085806881, 133.7450000000000045, -7.705886871421374629 ) ) ;
#38130 = CARTESIAN_POINT ( 'NONE',  ( -111.8949999999999960, 6.826472737025116366, 4.959722759717898555 ) ) ;
#38131 = DIRECTION ( 'NONE',  ( 0.000000000000000000, 1.000000000000000000, 0.000000000000000000 ) ) ;
#38132 = CARTESIAN_POINT ( 'NONE',  ( 40.99999999999997868, 9.999999999999978684, -3.500000000000000000 ) ) ;
#38133 = PRESENTATION_LAYER_ASSIGNMENT (  '', '', ( #62775 ) ) ;
#38134 = CARTESIAN_POINT ( 'NONE',  ( -156.5929263765337964, -3.094860106618431139, -9.524999999999991473 ) ) ;
#38135 = CARTESIAN_POINT ( 'NONE',  ( -172.9449999999999932, -9.827790563157499189E-16, -8.024999999999991473 ) ) ;
#38136 = VECTOR ( 'NONE', #41388, 1000.000000000000000 ) ;
#38137 = CARTESIAN_POINT ( 'NONE',  ( 4.250000000000001776, 21.74999999999998579, 3.750000000000000000 ) ) ;
#38138 = CIRCLE ( 'NONE', #26862, 0.5000000000000004441 ) ;
#38139 = CARTESIAN_POINT ( 'NONE',  ( 60.00000000000000000, 1.797044900979284448E-15, 6.999999999999999112 ) ) ;
#38140 = ORIENTED_EDGE ( 'NONE', *, *, #36363, .T. ) ;
#38141 = PRESENTATION_STYLE_ASSIGNMENT (( #54267 ) ) ;
#38142 = VERTEX_POINT ( 'NONE', #32056 ) ;
#38143 = CARTESIAN_POINT ( 'NONE',  ( -80.54292637653379927, 9.058813317711329915, 2.943386871421369566 ) ) ;
#38144 = VECTOR ( 'NONE', #60744, 1000.000000000000000 ) ;
#38145 = CARTESIAN_POINT ( 'NONE',  ( -11.99999999999999822, -6.499999999999999112, 21.00000000000000000 ) ) ;
#38146 = CYLINDRICAL_SURFACE ( 'NONE', #58457, 16.99999999999998579 ) ;
#38147 = DIRECTION ( 'NONE',  ( 0.000000000000000000, -1.000000000000000000, 0.000000000000000000 ) ) ;
#38148 = DIRECTION ( 'NONE',  ( -0.07898106964430656740, -0.9968761159932768567, -0.000000000000000000 ) ) ;
#38149 = AXIS2_PLACEMENT_3D ( 'NONE', #66118, #50311, #18647 ) ;
#38150 = EDGE_LOOP ( 'NONE', ( #38255, #54831, #66787, #61440 ) ) ;
#38151 = CARTESIAN_POINT ( 'NONE',  ( -174.0549999999999784, -9.827790563157499189E-16, -8.024999999999991473 ) ) ;
#38152 = ADVANCED_FACE ( 'NONE', ( #41599 ), #36437, .F. ) ;
#38153 = VERTEX_POINT ( 'NONE', #58791 ) ;
#38154 = CARTESIAN_POINT ( 'NONE',  ( -75.50000000000000000, -6.499999999999992006, 3.000000000000000000 ) ) ;
#38155 = SURFACE_STYLE_FILL_AREA ( #36780 ) ;
#38156 = EDGE_CURVE ( 'NONE', #42076, #21155, #20461, .T. ) ;
#38157 = DIRECTION ( 'NONE',  ( 0.000000000000000000, 0.000000000000000000, 1.000000000000000000 ) ) ;
#38158 = CARTESIAN_POINT ( 'NONE',  ( -182.3070736234661808, -10.01517768586948698, 6.132527647946031529E-16 ) ) ;
#38159 = CARTESIAN_POINT ( 'NONE',  ( 4.716976649647099507, 156.7570736234661695, -6.492361379858953008 ) ) ;
#38160 = CIRCLE ( 'NONE', #65070, 16.99999999999998579 ) ;
#38161 = ADVANCED_FACE ( 'NONE', ( #10941 ), #48267, .F. ) ;
#38162 = ORIENTED_EDGE ( 'NONE', *, *, #26119, .F. ) ;
#38163 = CARTESIAN_POINT ( 'NONE',  ( 4.716976649647096842, 136.7429263765338305, 6.492361379858953896 ) ) ;
#38164 = CARTESIAN_POINT ( 'NONE',  ( -94.10499999999997556, -6.826472737025113702, 4.959722759717902107 ) ) ;
#38165 = VECTOR ( 'NONE', #44017, 1000.000000000000000 ) ;
#38166 = DIRECTION ( 'NONE',  ( 1.000000000000000000, 9.811390859391774840E-17, 0.000000000000000000 ) ) ;
#38167 = ORIENTED_EDGE ( 'NONE', *, *, #43665, .F. ) ;
#38168 =( NAMED_UNIT ( * ) PLANE_ANGLE_UNIT ( ) SI_UNIT ( $, .RADIAN. ) );
#38169 = PRESENTATION_STYLE_ASSIGNMENT (( #64855 ) ) ;
#38170 = CARTESIAN_POINT ( 'NONE',  ( -33.89861118948982721, -9.947368421052624754, -2.000000000000000000 ) ) ;
#38171 = EDGE_CURVE ( 'NONE', #44039, #8600, #6059, .T. ) ;
#38172 =( NAMED_UNIT ( * ) SI_UNIT ( $, .STERADIAN. ) SOLID_ANGLE_UNIT ( ) );
#38173 = ORIENTED_EDGE ( 'NONE', *, *, #12769, .F. ) ;
#38174 =( NAMED_UNIT ( * ) PLANE_ANGLE_UNIT ( ) SI_UNIT ( $, .RADIAN. ) );
#38176 = CARTESIAN_POINT ( 'NONE',  ( -64.64499999999998181, 4.716976649647091513, -6.492361379858946790 ) ) ;
#38175 = AXIS2_PLACEMENT_3D ( 'NONE', #62451, #14266, #8998 ) ;
#38177 = ORIENTED_EDGE ( 'NONE', *, *, #65202, .T. ) ;
#38178 = DIRECTION ( 'NONE',  ( -0.4468085106382997385, -0.000000000000000000, -0.8946296187927071930 ) ) ;
#38179 =( NAMED_UNIT ( * ) SI_UNIT ( $, .STERADIAN. ) SOLID_ANGLE_UNIT ( ) );
#38180 = CARTESIAN_POINT ( 'NONE',  ( -45.84227902758264150, 9.150846973920693017, -6.292314909081791363 ) ) ;
#38181 = ADVANCED_FACE ( 'NONE', ( #69351 ), #5297, .T. ) ;
#38182 = EDGE_LOOP ( 'NONE', ( #67429, #7731, #14616, #47073 ) ) ;
#38183 = SURFACE_SIDE_STYLE ('',( #54658 ) ) ;
#38184 = ORIENTED_EDGE ( 'NONE', *, *, #38491, .F. ) ;
#38185 = LINE ( 'NONE', #15516, #42756 ) ;
#38186 = CARTESIAN_POINT ( 'NONE',  ( -111.8049999999999784, -8.437984349512085203, 5.166775262442717831E-16 ) ) ;
#38187 = ORIENTED_EDGE ( 'NONE', *, *, #50693, .T. ) ;
#38188 = CARTESIAN_POINT ( 'NONE',  ( 3.000000000000030198, 43.00000000000000000, 90.00000000000000000 ) ) ;
#38189 = FACE_OUTER_BOUND ( 'NONE', #23955, .T. ) ;
#38190 = AXIS2_PLACEMENT_3D ( 'NONE', #40509, #56664, #8491 ) ;
#38191 = CARTESIAN_POINT ( 'NONE',  ( 0.000000000000000000, 0.000000000000000000, 0.000000000000000000 ) ) ;
#38192 = LINE ( 'NONE', #48404, #63714 ) ;
#38193 = TOROIDAL_SURFACE ( 'NONE', #31407, 7.500000000000011546, 0.5000000000000000000 ) ;
#38194 = CARTESIAN_POINT ( 'NONE',  ( -161.1570736234661751, -9.058813317711329915, -2.943386871421370898 ) ) ;
#38195 = CARTESIAN_POINT ( 'NONE',  ( -1.166476076187854022E-15, 128.9449999999999648, 9.525000000000000355 ) ) ;
#38196 = COLOUR_RGB ( '', 0.40784314, 0.44705882, 0.49803922) ;
#38197 = CARTESIAN_POINT ( 'NONE',  ( -96.05707362346618083, 0.000000000000000000, 9.524999999999991473 ) ) ;
#38198 = VECTOR ( 'NONE', #1806, 1000.000000000000000 ) ;
#38199 = PRESENTATION_LAYER_ASSIGNMENT (  '', '', ( #61726 ) ) ;
#38200 = CARTESIAN_POINT ( 'NONE',  ( -15.48999599679679662, 146.9999999999999716, -7.500000000000000000 ) ) ;
#38201 = ORIENTED_EDGE ( 'NONE', *, *, #8498, .T. ) ;
#38202 = CIRCLE ( 'NONE', #55008, 1.000000000000000888 ) ;
#38203 = DIRECTION ( 'NONE',  ( -1.000000000000000000, 0.000000000000000000, 0.000000000000000000 ) ) ;
#38204 = DIRECTION ( 'NONE',  ( -0.000000000000000000, -0.000000000000000000, -1.000000000000000000 ) ) ;
#38205 = CARTESIAN_POINT ( 'NONE',  ( -130.8549999999999898, 4.716976649647094177, 6.492361379858945902 ) ) ;
#38206 = SURFACE_SIDE_STYLE ('',( #37175 ) ) ;
#38207 = SURFACE_STYLE_FILL_AREA ( #60996 ) ;
#38208 = CARTESIAN_POINT ( 'NONE',  ( -143.9950000000000045, -6.826472737025115478, 4.959722759717900331 ) ) ;
#38209 = VECTOR ( 'NONE', #34198, 1000.000000000000000 ) ;
#38210 = CARTESIAN_POINT ( 'NONE',  ( -139.1949999999999932, 8.437984349512086979, -1.550032578732815448E-15 ) ) ;
#38211 = EDGE_LOOP ( 'NONE', ( #11540, #52761, #25162, #24171, #33247, #57706, #41511, #59811, #61203, #1590 ) ) ;
#38212 = VECTOR ( 'NONE', #17004, 1000.000000000000000 ) ;
#38213 = EDGE_CURVE ( 'NONE', #25093, #49290, #38851, .T. ) ;
#38214 = CARTESIAN_POINT ( 'NONE',  ( -192.5249999999998636, 0.000000000000000000, 0.000000000000000000 ) ) ;
#38215 = FILL_AREA_STYLE_COLOUR ( '', #36858 ) ;
#38216 = DIRECTION ( 'NONE',  ( 1.000000000000000000, -0.000000000000000000, -1.300977106640434644E-16 ) ) ;
#38217 = UNCERTAINTY_MEASURE_WITH_UNIT (LENGTH_MEASURE( 1.000000000000000082E-05 ), #8485, 'distance_accuracy_value', 'NONE');
#38218 = CARTESIAN_POINT ( 'NONE',  ( -58.55499999999999261, 0.000000000000000000, 8.024999999999991473 ) ) ;
#38219 =( LENGTH_UNIT ( ) NAMED_UNIT ( * ) SI_UNIT ( .MILLI., .METRE. ) );
#38220 = VECTOR ( 'NONE', #34104, 1000.000000000000000 ) ;
#38221 = CARTESIAN_POINT ( 'NONE',  ( -60.14499999999998892, -4.716976649647092401, 6.492361379858946790 ) ) ;
#38222 = FACE_OUTER_BOUND ( 'NONE', #54502, .T. ) ;
#38223 = CARTESIAN_POINT ( 'NONE',  ( -102.5070736234661695, 8.102448949553176405, 5.886773742842740909 ) ) ;
#38224 =( NAMED_UNIT ( * ) PLANE_ANGLE_UNIT ( ) SI_UNIT ( $, .RADIAN. ) );
#38225 = CYLINDRICAL_SURFACE ( 'NONE', #22645, 8.999999999999994671 ) ;
#38226 = MECHANICAL_DESIGN_GEOMETRIC_PRESENTATION_REPRESENTATION (  '', ( #20196 ), #5569 ) ;
#38227 = COLOUR_RGB ( '', 0.31764706, 0.68627451, 0.89019608) ;
#38228 = CARTESIAN_POINT ( 'NONE',  ( -102.1429263765337936, 5.598654528085800663, -7.705886871421367523 ) ) ;
#38229 = DIRECTION ( 'NONE',  ( 4.528264053928433857E-17, -5.775339657480442461E-17, 1.000000000000000000 ) ) ;
#38230 =( BOUNDED_CURVE ( )  B_SPLINE_CURVE ( 2, ( #11147, #32594, #54058, #22066, #32972, #64956, #6545, #49501, #27994, #22761, #44260 ),
 .UNSPECIFIED., .F., .F. ) 
 B_SPLINE_CURVE_WITH_KNOTS ( ( 3, 2, 2, 2, 2, 3 ),
 ( 0.8369565217391304879, 0.8391304347826087362, 0.8413043478260869845, 0.8434782608695652328, 0.8456521739130434812, 0.8478260869565217295 ),
 .UNSPECIFIED. ) 
 CURVE ( )  GEOMETRIC_REPRESENTATION_ITEM ( )  RATIONAL_B_SPLINE_CURVE ( ( 1.000000000000000000, 0.9510565162951535312, 1.000000000000000000, 0.9510565162951535312, 1.000000000000000000, 0.9510565162951535312, 1.000000000000000000, 0.9510565162951535312, 1.000000000000000000, 0.9510565162951535312, 1.000000000000000000 ) ) 
 REPRESENTATION_ITEM ( '' )  );
#38231 = CARTESIAN_POINT ( 'NONE',  ( -162.8070736234661808, 10.01517768586948698, -1.839758294383808966E-15 ) ) ;
#38232 = AXIS2_PLACEMENT_3D ( 'NONE', #11268, #653, #64396 ) ;
#38233 = PRESENTATION_STYLE_ASSIGNMENT (( #17119 ) ) ;
#38234 = ADVANCED_FACE ( 'NONE', ( #4971 ), #28473, .F. ) ;
#38235 = CARTESIAN_POINT ( 'NONE',  ( 0.000000000000000000, 0.000000000000000000, 0.000000000000000000 ) ) ;
#38236 = ADVANCED_FACE ( 'NONE', ( #64413 ), #65801, .F. ) ;
#38237 = ORIENTED_EDGE ( 'NONE', *, *, #45705, .T. ) ;
#38238 = DIRECTION ( 'NONE',  ( 0.000000000000000000, 0.000000000000000000, -1.000000000000000000 ) ) ;
#38239 = COLOUR_RGB ( '', 0.40784314, 0.44705882, 0.49803922) ;
#38240 = PRESENTATION_STYLE_ASSIGNMENT (( #64916 ) ) ;
#38241 = AXIS2_PLACEMENT_3D ( 'NONE', #44697, #38386, #33403 ) ;
#38242 = EDGE_LOOP ( 'NONE', ( #67631, #6598, #39024, #9800 ) ) ;
#38243 = CARTESIAN_POINT ( 'NONE',  ( -8.437984349512095861, 115.8070736234661524, -5.166775262442723748E-16 ) ) ;
#38244 = EDGE_CURVE ( 'NONE', #1837, #16875, #31008, .T. ) ;
#38245 = DIRECTION ( 'NONE',  ( 0.000000000000000000, 0.000000000000000000, 1.000000000000000000 ) ) ;
#38246 = CARTESIAN_POINT ( 'NONE',  ( -60.00000000000000000, -2.024042244987997205E-14, 12.00000000000000000 ) ) ;
#38247 = STYLED_ITEM ( 'NONE', ( #45598 ), #52290 ) ;
#38248 = SURFACE_SIDE_STYLE ('',( #10447 ) ) ;
#38249 = ADVANCED_FACE ( 'NONE', ( #44731 ), #39848, .F. ) ;
#38250 = ORIENTED_EDGE ( 'NONE', *, *, #26577, .T. ) ;
#38251 = EDGE_LOOP ( 'NONE', ( #12581, #11625 ) ) ;
#38252 = CARTESIAN_POINT ( 'NONE',  ( -116.1570736234661751, -9.058813317711329915, -2.943386871421370898 ) ) ;
#38253 = LINE ( 'NONE', #34568, #29741 ) ;
#38254 = LINE ( 'NONE', #22039, #40627 ) ;
#38255 = ORIENTED_EDGE ( 'NONE', *, *, #28165, .F. ) ;
#38256 = CARTESIAN_POINT ( 'NONE',  ( -183.0769827045555473, 0.000000000000000000, 9.448017295444435248 ) ) ;
#38257 = ADVANCED_FACE ( 'NONE', ( #33435 ), #16937, .F. ) ;
#38258 = PRESENTATION_LAYER_ASSIGNMENT (  '', '', ( #46139 ) ) ;
#38259 = CARTESIAN_POINT ( 'NONE',  ( 2.607480562269155921, 148.5929263765338249, 8.024999999999941735 ) ) ;
#38260 = CARTESIAN_POINT ( 'NONE',  ( -90.74499999999999034, 4.716976649647094177, 6.492361379858945902 ) ) ;
#38261 = ORIENTED_EDGE ( 'NONE', *, *, #36666, .F. ) ;
#38262 = AXIS2_PLACEMENT_3D ( 'NONE', #64399, #54179, #59112 ) ;
#38263 = COLOUR_RGB ( '', 0.66274510, 0.83137255, 0.94901961) ;
#38264 = CARTESIAN_POINT ( 'NONE',  ( 7.295185304185720199, 153.7998498338025684, -4.982187544324071737 ) ) ;
#38265 = CARTESIAN_POINT ( 'NONE',  ( -22.75000000000000711, 34.24999999999999289, -3.750000000000000000 ) ) ;
#38266 = DIRECTION ( 'NONE',  ( -1.000000000000000000, -1.224646799147353207E-16, 0.000000000000000000 ) ) ;
#38267 = EDGE_CURVE ( 'NONE', #32231, #41879, #49906, .T. ) ;
#38268 = UNCERTAINTY_MEASURE_WITH_UNIT (LENGTH_MEASURE( 1.000000000000000082E-05 ), #67368, 'distance_accuracy_value', 'NONE');
#38269 = ORIENTED_EDGE ( 'NONE', *, *, #45481, .T. ) ;
#38270 = CARTESIAN_POINT ( 'NONE',  ( 7.632228543268608334, 161.3429263765338249, -2.479861379858951942 ) ) ;
#38271 = SURFACE_STYLE_USAGE ( .BOTH. , #1903 ) ;
#38272 = AXIS2_PLACEMENT_3D ( 'NONE', #23453, #66731, #22783 ) ;
#38273 = SURFACE_STYLE_USAGE ( .BOTH. , #21340 ) ;
#38274 = PLANE ( 'NONE',  #16825 ) ;
#38275 = ORIENTED_EDGE ( 'NONE', *, *, #12151, .T. ) ;
#38276 = DIRECTION ( 'NONE',  ( -1.000000000000000000, -1.224646799147353454E-16, 0.000000000000000000 ) ) ;
#38277 = ORIENTED_EDGE ( 'NONE', *, *, #33998, .F. ) ;
#38278 = CYLINDRICAL_SURFACE ( 'NONE', #15898, 9.524999999999991473 ) ;
#38279 = FACE_OUTER_BOUND ( 'NONE', #11716, .T. ) ;
#38280 = DIRECTION ( 'NONE',  ( 1.000000000000000000, 0.000000000000000000, 0.000000000000000000 ) ) ;
#38281 = DIRECTION ( 'NONE',  ( 0.000000000000000000, 1.000000000000000000, 0.000000000000000000 ) ) ;
#38282 = AXIS2_PLACEMENT_3D ( 'NONE', #25260, #68187, #30514 ) ;
#38283 = CARTESIAN_POINT ( 'NONE',  ( 4.000000000000030198, 38.70020753820971748, 89.00000000000000000 ) ) ;
#38284 = COLOUR_RGB ( '', 0.40784314, 0.44705882, 0.49803922) ;
#38285 = CARTESIAN_POINT ( 'NONE',  ( -4.377616827404060551, 9.000000000000010658, 1.000745235317163528 ) ) ;
#38286 = CARTESIAN_POINT ( 'NONE',  ( -7.863253753129167301, 153.7221554051249370, 3.841316429231163010 ) ) ;
#38287 = EDGE_LOOP ( 'NONE', ( #17678, #14725, #37061, #54464 ) ) ;
#38288 = CARTESIAN_POINT ( 'NONE',  ( -49.10707362346617089, 8.102448949553172852, -5.886773742842744461 ) ) ;
#38289 = DIRECTION ( 'NONE',  ( 1.000000000000000000, 0.000000000000000000, 0.000000000000000000 ) ) ;
#38290 = VERTEX_POINT ( 'NONE', #54869 ) ;
#38291 = CARTESIAN_POINT ( 'NONE',  ( -167.6050000000000182, 6.826472737025113702, -4.959722759717902107 ) ) ;
#38292 = FACE_OUTER_BOUND ( 'NONE', #46511, .T. ) ;
#38293 = CARTESIAN_POINT ( 'NONE',  ( 30.25000000000001066, 16.24999999999997513, 4.000000000000000000 ) ) ;
#38294 = CARTESIAN_POINT ( 'NONE',  ( -177.8949999999999818, 6.826472737025116366, 4.959722759717898555 ) ) ;
#38295 = COLOUR_RGB ( '', 0.09019608, 0.27058824, 0.51372549) ;
#38296 = CARTESIAN_POINT ( 'NONE',  ( -172.0450000000000159, 7.632228543268600340, 2.479861379858949277 ) ) ;
#38297 = ORIENTED_EDGE ( 'NONE', *, *, #40417, .F. ) ;
#38298 = EDGE_CURVE ( 'NONE', #69624, #66051, #6690, .T. ) ;
#38299 = DIRECTION ( 'NONE',  ( 0.000000000000000000, 0.000000000000000000, 1.000000000000000000 ) ) ;
#38300 = SURFACE_STYLE_USAGE ( .BOTH. , #60387 ) ;
#38301 = DIRECTION ( 'NONE',  ( 0.000000000000000000, 0.000000000000000000, 1.000000000000000000 ) ) ;
#38302 = COLOUR_RGB ( '', 0.31764706, 0.68627451, 0.89019608) ;
#38303 = CARTESIAN_POINT ( 'NONE',  ( -87.05499999999999261, -9.827790563157499189E-16, -8.024999999999991473 ) ) ;
#38304 = CIRCLE ( 'NONE', #40550, 0.2500000000000002220 ) ;
#38305 = CARTESIAN_POINT ( 'NONE',  ( 3.046771365092978190, 72.00000000000001421, 6.349999999999997868 ) ) ;
#38306 = CARTESIAN_POINT ( 'NONE',  ( -81.14499999999998181, -4.716976649647092401, 6.492361379858946790 ) ) ;
#38307 = CARTESIAN_POINT ( 'NONE',  ( -5.598654528085808657, 132.7549999999999955, 7.705886871421373741 ) ) ;
#38308 = CARTESIAN_POINT ( 'NONE',  ( 71.18918918918917882, 14.09971791521133255, 7.500000000000000000 ) ) ;
#38309 = COLOUR_RGB ( '', 0.40784314, 0.44705882, 0.49803922) ;
#38310 = UNCERTAINTY_MEASURE_WITH_UNIT (LENGTH_MEASURE( 1.000000000000000082E-05 ), #36946, 'distance_accuracy_value', 'NONE');
#38311 = CIRCLE ( 'NONE', #24743, 0.2500000000000002220 ) ;
#38313 = SURFACE_STYLE_USAGE ( .BOTH. , #49879 ) ;
#38312 = AXIS2_PLACEMENT_3D ( 'NONE', #59983, #15714, #26240 ) ;
#38314 = ORIENTED_EDGE ( 'NONE', *, *, #37705, .F. ) ;
#38315 = EDGE_CURVE ( 'NONE', #48372, #56046, #38060, .T. ) ;
#38316 = CARTESIAN_POINT ( 'NONE',  ( 6.239160159721271803, -2.500000000000000000, -3.193457606803198789 ) ) ;
#38317 = ADVANCED_FACE ( 'NONE', ( #65081 ), #26320, .F. ) ;
#38318 = PLANE ( 'NONE',  #28176 ) ;
#38319 = EDGE_CURVE ( 'NONE', #65448, #61448, #54394, .T. ) ;
#38320 = CARTESIAN_POINT ( 'NONE',  ( 34.99999999999992895, 112.9999999999999858, -7.000000000000000000 ) ) ;
#38321 = ORIENTED_EDGE ( 'NONE', *, *, #31942, .T. ) ;
#38322 = EDGE_LOOP ( 'NONE', ( #20429, #22886, #57593, #51715 ) ) ;
#38323 = LINE ( 'NONE', #17867, #65592 ) ;
#38324 = CARTESIAN_POINT ( 'NONE',  ( -40.99999999999997868, 10.49999999999998224, 3.500000000000000000 ) ) ;
#38325 = COLOUR_RGB ( '', 0.66274510, 0.83137255, 0.94901961) ;
#38326 = EDGE_CURVE ( 'NONE', #57943, #11591, #51065, .T. ) ;
#38327 = VECTOR ( 'NONE', #42625, 1000.000000000000000 ) ;
#38328 = CARTESIAN_POINT ( 'NONE',  ( -45.48309787872866394, 9.683080749504641815, 3.000000000000000000 ) ) ;
#38329 = DIRECTION ( 'NONE',  ( 0.000000000000000000, 0.000000000000000000, -1.000000000000000000 ) ) ;
#38330 = DIRECTION ( 'NONE',  ( 0.000000000000000000, 0.000000000000000000, 1.000000000000000000 ) ) ;
#38331 = CARTESIAN_POINT ( 'NONE',  ( 2.607480562268992941, 140.7929263765338419, -8.025000000000060751 ) ) ;
#38332 = ADVANCED_FACE ( 'NONE', ( #30211 ), #6099, .T. ) ;
#38333 = EDGE_LOOP ( 'NONE', ( #56984, #33867, #50032, #47762, #30403, #30733, #12587, #16354 ) ) ;
#38334 = CIRCLE ( 'NONE', #12470, 5.000000000000004441 ) ;
#38335 = CARTESIAN_POINT ( 'NONE',  ( -115.1049999999999756, -6.826472737025113702, 4.959722759717902107 ) ) ;
#38336 = ORIENTED_EDGE ( 'NONE', *, *, #19994, .F. ) ;
#38337 = FACE_OUTER_BOUND ( 'NONE', #68166, .T. ) ;
#38338 = DIRECTION ( 'NONE',  ( 0.000000000000000000, 0.000000000000000000, 1.000000000000000000 ) ) ;
#38339 = ORIENTED_EDGE ( 'NONE', *, *, #8515, .T. ) ;
#38340 = CARTESIAN_POINT ( 'NONE',  ( 26.25000000000001066, 18.74999999999997868, 3.750000000000000000 ) ) ;
#38341 = CARTESIAN_POINT ( 'NONE',  ( 179.4361977533490347, 0.000000000000000000, 103.7004518695263044 ) ) ;
#38342 = EDGE_LOOP ( 'NONE', ( #1202, #53053 ) ) ;
#38343 = AXIS2_PLACEMENT_3D ( 'NONE', #45080, #16600, #27781 ) ;
#38344 = SURFACE_STYLE_USAGE ( .BOTH. , #28401 ) ;
#38345 = MECHANICAL_DESIGN_GEOMETRIC_PRESENTATION_REPRESENTATION (  '', ( #48440 ), #55105 ) ;
#38346 = CARTESIAN_POINT ( 'NONE',  ( -10.01517768586949231, 158.1949999999999932, -6.132527647946036459E-16 ) ) ;
#38347 = DIRECTION ( 'NONE',  ( 1.000000000000000000, 0.000000000000000000, 0.000000000000000000 ) ) ;
#38348 = ORIENTED_EDGE ( 'NONE', *, *, #12206, .F. ) ;
#38349 = AXIS2_PLACEMENT_3D ( 'NONE', #33347, #2673, #28029 ) ;
#38350 = VERTEX_POINT ( 'NONE', #41178 ) ;
#38351 = CARTESIAN_POINT ( 'NONE',  ( -118.1070736234661780, 8.102448949553172852, -5.886773742842744461 ) ) ;
#38352 =( LENGTH_UNIT ( ) NAMED_UNIT ( * ) SI_UNIT ( .MILLI., .METRE. ) );
#38353 = CARTESIAN_POINT ( 'NONE',  ( -4.750000000000002665, 24.74999999999998579, -3.750000000000000000 ) ) ;
#38354 = LINE ( 'NONE', #31638, #61096 ) ;
#38355 = ORIENTED_EDGE ( 'NONE', *, *, #38497, .F. ) ;
#38356 = CARTESIAN_POINT ( 'NONE',  ( 4.716976649647096842, 136.7429263765338305, 6.492361379858953896 ) ) ;
#38357 = DIRECTION ( 'NONE',  ( 1.000000000000000000, 0.000000000000000000, 0.000000000000000000 ) ) ;
#38358 = DIRECTION ( 'NONE',  ( -0.000000000000000000, 0.000000000000000000, -1.000000000000000000 ) ) ;
#38359 = CARTESIAN_POINT ( 'NONE',  ( -20.71231517720798010, 146.9999999999999716, 7.500000000000000000 ) ) ;
#38360 =( LENGTH_UNIT ( ) NAMED_UNIT ( * ) SI_UNIT ( .MILLI., .METRE. ) );
#38361 = EDGE_CURVE ( 'NONE', #28358, #47977, #58887, .T. ) ;
#38362 = ORIENTED_EDGE ( 'NONE', *, *, #44451, .T. ) ;
#38363 = CONICAL_SURFACE ( 'NONE', #36129, 5.000000000000000000, 0.7853981633974415066 ) ;
#38364 = SURFACE_SIDE_STYLE ('',( #22485 ) ) ;
#38365 = ORIENTED_EDGE ( 'NONE', *, *, #5886, .T. ) ;
#38366 = CARTESIAN_POINT ( 'NONE',  ( -49.19292637653380496, -10.01517768586948698, 6.132527647946031529E-16 ) ) ;
#38367 = SURFACE_SIDE_STYLE ('',( #48572 ) ) ;
#38368 = CARTESIAN_POINT ( 'NONE',  ( 26.00000000000001776, 15.00000000000000000, 29.68999999999999417 ) ) ;
#38369 = DIRECTION ( 'NONE',  ( 0.000000000000000000, 1.000000000000000000, 0.000000000000000000 ) ) ;
#38370 = CARTESIAN_POINT ( 'NONE',  ( -139.2549999999999955, -4.716976649647092401, 6.492361379858946790 ) ) ;
#38371 = DIRECTION ( 'NONE',  ( 0.000000000000000000, -0.000000000000000000, 1.000000000000000000 ) ) ;
#38372 = EDGE_CURVE ( 'NONE', #12708, #36632, #62006, .T. ) ;
#38373 = UNCERTAINTY_MEASURE_WITH_UNIT (LENGTH_MEASURE( 1.000000000000000082E-05 ), #61862, 'distance_accuracy_value', 'NONE');
#38374 = ORIENTED_EDGE ( 'NONE', *, *, #53152, .F. ) ;
#38375 =( GEOMETRIC_REPRESENTATION_CONTEXT ( 3 ) GLOBAL_UNCERTAINTY_ASSIGNED_CONTEXT ( ( #59361 ) ) GLOBAL_UNIT_ASSIGNED_CONTEXT ( ( #10081, #20628, #42140 ) ) REPRESENTATION_CONTEXT ( 'NONE', 'WORKASPACE' ) );
#38376 = DIRECTION ( 'NONE',  ( 0.000000000000000000, 1.000000000000000000, 0.000000000000000000 ) ) ;
#38377 = CARTESIAN_POINT ( 'NONE',  ( -74.99999999999998579, 118.4999999999999716, 7.000000000000000000 ) ) ;
#38378 = CARTESIAN_POINT ( 'NONE',  ( 40.99999999999998579, 108.0041655821620026, 3.000000000000000000 ) ) ;
#38379 = ORIENTED_EDGE ( 'NONE', *, *, #41484, .F. ) ;
#38380 = STYLED_ITEM ( 'NONE', ( #13790 ), #13706 ) ;
#38381 = EDGE_LOOP ( 'NONE', ( #58827, #8725, #57039, #18159 ) ) ;
#38382 = CARTESIAN_POINT ( 'NONE',  ( 44.00000000000000000, 19.24999999999998224, -3.750000000000000000 ) ) ;
#38383 = CARTESIAN_POINT ( 'NONE',  ( -109.9429263765338050, 0.000000000000000000, 9.524999999999991473 ) ) ;
#38384 = CARTESIAN_POINT ( 'NONE',  ( -60.65499999999998693, -7.632228543268600340, -2.479861379858950166 ) ) ;
#38385 = ORIENTED_EDGE ( 'NONE', *, *, #61308, .F. ) ;
#38386 = DIRECTION ( 'NONE',  ( 1.224646799147353207E-16, 1.000000000000000000, -0.000000000000000000 ) ) ;
#38387 = PRESENTATION_STYLE_ASSIGNMENT (( #42975 ) ) ;
#38388 = DIRECTION ( 'NONE',  ( 1.000000000000000000, 7.709882115452469292E-16, 0.000000000000000000 ) ) ;
#38389 = FACE_OUTER_BOUND ( 'NONE', #23345, .T. ) ;
#38390 = CIRCLE ( 'NONE', #5774, 0.5000000000000004441 ) ;
#38391 = DIRECTION ( 'NONE',  ( -1.000000000000000000, 0.000000000000000000, 0.000000000000000000 ) ) ;
#38392 = DIRECTION ( 'NONE',  ( 0.000000000000000000, 0.000000000000000000, 1.000000000000000000 ) ) ;
#38393 = EDGE_LOOP ( 'NONE', ( #28582, #56766, #15017, #22151 ) ) ;
#38394 = AXIS2_PLACEMENT_3D ( 'NONE', #18980, #52341, #50002 ) ;
#38395 =( GEOMETRIC_REPRESENTATION_CONTEXT ( 3 ) GLOBAL_UNCERTAINTY_ASSIGNED_CONTEXT ( ( #35570 ) ) GLOBAL_UNIT_ASSIGNED_CONTEXT ( ( #7978, #2989, #24831 ) ) REPRESENTATION_CONTEXT ( 'NONE', 'WORKASPACE' ) );
#38396 = CARTESIAN_POINT ( 'NONE',  ( -145.5570736234661808, -1.166476076187852838E-15, -9.524999999999991473 ) ) ;
#38397 = CARTESIAN_POINT ( 'NONE',  ( -41.49999999999997868, 9.999999999999978684, -3.000000000000000444 ) ) ;
#38398 = FILL_AREA_STYLE ('',( #16916 ) ) ;
#38399 = PRESENTATION_LAYER_ASSIGNMENT (  '', '', ( #40631 ) ) ;
#38400 = CARTESIAN_POINT ( 'NONE',  ( -114.4449999999999932, 0.000000000000000000, 8.024999999999991473 ) ) ;
#38401 = CARTESIAN_POINT ( 'NONE',  ( -3.094860106618432471, 110.7049999999999983, -9.525000000000000355 ) ) ;
#38402 = CARTESIAN_POINT ( 'NONE',  ( -90.74499999999999034, 4.716976649647094177, 6.492361379858945902 ) ) ;
#38403 = EDGE_CURVE ( 'NONE', #31418, #1731, #45760, .T. ) ;
#38404 = AXIS2_PLACEMENT_3D ( 'NONE', #55227, #17301, #38761 ) ;
#38405 =( NAMED_UNIT ( * ) SI_UNIT ( $, .STERADIAN. ) SOLID_ANGLE_UNIT ( ) );
#38406 = CARTESIAN_POINT ( 'NONE',  ( 52.99999999999999289, 27.99999999999998579, 4.000000000000000000 ) ) ;
#38407 = AXIS2_PLACEMENT_3D ( 'NONE', #24105, #67027, #18819 ) ;
#38408 = DIRECTION ( 'NONE',  ( -0.000000000000000000, 0.000000000000000000, 1.000000000000000000 ) ) ;
#38409 = UNCERTAINTY_MEASURE_WITH_UNIT (LENGTH_MEASURE( 1.000000000000000082E-05 ), #13108, 'distance_accuracy_value', 'NONE');
#38410 = APPLICATION_CONTEXT ( 'automotive_design' ) ;
#38411 = ORIENTED_EDGE ( 'NONE', *, *, #14128, .F. ) ;
#38412 = EDGE_CURVE ( 'NONE', #54537, #44052, #53327, .T. ) ;
#38413 = CARTESIAN_POINT ( 'NONE',  ( -128.8429263765337964, 9.058813317711329915, -2.943386871421373119 ) ) ;
#38414 = SURFACE_STYLE_FILL_AREA ( #44033 ) ;
#38415 = CARTESIAN_POINT ( 'NONE',  ( -151.9449999999999932, -9.827790563157499189E-16, -8.024999999999991473 ) ) ;
#38416 = CARTESIAN_POINT ( 'NONE',  ( 16.75000000000000711, 25.24999999999998224, -4.000000000000000000 ) ) ;
#38417 = EDGE_CURVE ( 'NONE', #52608, #21468, #29539, .T. ) ;
#38418 = AXIS2_PLACEMENT_3D ( 'NONE', #60368, #65997, #33986 ) ;
#38419 = PRESENTATION_STYLE_ASSIGNMENT (( #65076 ) ) ;
#38420 = ORIENTED_EDGE ( 'NONE', *, *, #57205, .T. ) ;
#38421 = ORIENTED_EDGE ( 'NONE', *, *, #48686, .F. ) ;
#38422 = STYLED_ITEM ( 'NONE', ( #41690 ), #17186 ) ;
#38423 = DIRECTION ( 'NONE',  ( 1.000000000000000000, 0.000000000000000000, -0.000000000000000000 ) ) ;
#38424 = DIRECTION ( 'NONE',  ( -1.000000000000000000, 0.000000000000000000, 0.000000000000000000 ) ) ;
#38425 =( NAMED_UNIT ( * ) SI_UNIT ( $, .STERADIAN. ) SOLID_ANGLE_UNIT ( ) );
#38426 = CARTESIAN_POINT ( 'NONE',  ( -60.29292637653380638, 3.094860106618428031, -9.524999999999993250 ) ) ;
#38427 = AXIS2_PLACEMENT_3D ( 'NONE', #69311, #59779, #53138 ) ;
#38428 = SURFACE_STYLE_FILL_AREA ( #38763 ) ;
#38430 = ADVANCED_FACE ( 'NONE', ( #7735 ), #56627, .T. ) ;
#38429 = LINE ( 'NONE', #44047, #31962 ) ;
#38431 = ORIENTED_EDGE ( 'NONE', *, *, #5383, .F. ) ;
#38432 = CARTESIAN_POINT ( 'NONE',  ( -139.2549999999999955, -4.716976649647092401, 6.492361379858946790 ) ) ;
#38433 = EDGE_LOOP ( 'NONE', ( #41730, #9691, #64759, #51244 ) ) ;
#38434 = VERTEX_POINT ( 'NONE', #19324 ) ;
#38435 = LINE ( 'NONE', #65091, #22283 ) ;
#38436 =( LENGTH_UNIT ( ) NAMED_UNIT ( * ) SI_UNIT ( .MILLI., .METRE. ) );
#38437 = ORIENTED_EDGE ( 'NONE', *, *, #1145, .T. ) ;
#38438 = CARTESIAN_POINT ( 'NONE',  ( -56.25313552506686676, -8.558999539123545830, -0.5698282025367524817 ) ) ;
#38439 = DIRECTION ( 'NONE',  ( 0.000000000000000000, 0.000000000000000000, 1.000000000000000000 ) ) ;
#38440 = CARTESIAN_POINT ( 'NONE',  ( 8.102448949553183510, 132.9949999999999477, -5.886773742842746238 ) ) ;
#38441 =( BOUNDED_CURVE ( )  B_SPLINE_CURVE ( 3, ( #69182, #36850, #64225, #26580 ),
 .UNSPECIFIED., .F., .F. ) 
 B_SPLINE_CURVE_WITH_KNOTS ( ( 4, 4 ),
 ( 3.919743979054040484, 4.712388980384689674 ),
 .UNSPECIFIED. ) 
 CURVE ( )  GEOMETRIC_REPRESENTATION_ITEM ( )  RATIONAL_B_SPLINE_CURVE ( ( 1.000000000000000000, 0.9483245655077794378, 0.9483245655077794378, 1.000000000000000000 ) ) 
 REPRESENTATION_ITEM ( '' )  );
#38442 = VERTEX_POINT ( 'NONE', #66849 ) ;
#38443 = AXIS2_PLACEMENT_3D ( 'NONE', #26841, #69118, #20927 ) ;
#38444 = CARTESIAN_POINT ( 'NONE',  ( -95.00707362346616947, -8.102448949553174629, -5.886773742842741797 ) ) ;
#38445 = CARTESIAN_POINT ( 'NONE',  ( 3.094860106618435136, 131.4050000000000011, -9.525000000000000355 ) ) ;
#38446 = AXIS2_PLACEMENT_3D ( 'NONE', #68377, #5626, #27078 ) ;
#38447 = CARTESIAN_POINT ( 'NONE',  ( -52.10499999999997556, -6.826472737025113702, 4.959722759717902107 ) ) ;
#38448 = CARTESIAN_POINT ( 'NONE',  ( -116.3949999999999960, -6.826472737025115478, -4.959722759717899443 ) ) ;
#38449 = DIRECTION ( 'NONE',  ( 1.000000000000000000, -0.000000000000000000, -1.300977106640434891E-16 ) ) ;
#38450 = ORIENTED_EDGE ( 'NONE', *, *, #65668, .F. ) ;
#38451 = CARTESIAN_POINT ( 'NONE',  ( -9.058813317711337021, 159.1550000000000011, -2.943386871421374895 ) ) ;
#38452 = CARTESIAN_POINT ( 'NONE',  ( 9.827790563157511022E-16, 87.30187232391182306, -8.025000000000000355 ) ) ;
#38453 = UNCERTAINTY_MEASURE_WITH_UNIT (LENGTH_MEASURE( 1.000000000000000082E-05 ), #57078, 'distance_accuracy_value', 'NONE');
#38454 = MECHANICAL_DESIGN_GEOMETRIC_PRESENTATION_REPRESENTATION (  '', ( #51914 ), #11421 ) ;
#38455 = AXIS2_PLACEMENT_3D ( 'NONE', #48242, #53817, #4588 ) ;
#38456 = CARTESIAN_POINT ( 'NONE',  ( 0.000000000000000000, 0.000000000000000000, 0.000000000000000000 ) ) ;
#38457 = COLOUR_RGB ( '', 0.31764706, 0.68627451, 0.89019608) ;
#38458 = FACE_OUTER_BOUND ( 'NONE', #34336, .T. ) ;
#38459 = EDGE_LOOP ( 'NONE', ( #68841, #6217, #13829, #5014 ) ) ;
#38460 = CARTESIAN_POINT ( 'NONE',  ( 8.250000000000001776, 30.99999999999998579, 4.000000000000000000 ) ) ;
#38461 = CARTESIAN_POINT ( 'NONE',  ( -168.9549999999999841, -7.632228543268599452, 2.479861379858951054 ) ) ;
#38462 = ORIENTED_EDGE ( 'NONE', *, *, #40356, .F. ) ;
#38463 = UNCERTAINTY_MEASURE_WITH_UNIT (LENGTH_MEASURE( 1.000000000000000082E-05 ), #29674, 'distance_accuracy_value', 'NONE');
#38464 = MECHANICAL_DESIGN_GEOMETRIC_PRESENTATION_REPRESENTATION (  '', ( #20438 ), #24877 ) ;
#38465 = DIRECTION ( 'NONE',  ( 1.000000000000000000, 0.000000000000000000, 0.000000000000000000 ) ) ;
#38466 =( LENGTH_UNIT ( ) NAMED_UNIT ( * ) SI_UNIT ( .MILLI., .METRE. ) );
#38467 = B_SPLINE_CURVE_WITH_KNOTS ( 'NONE', 3,
 ( #103, #49098, #21269, #20951 ),
 .UNSPECIFIED., .F., .F.,
 ( 4, 4 ),
 ( 0.01934061289150207363, 0.02044444614850437353 ),
 .UNSPECIFIED. ) ;
#38468 = CARTESIAN_POINT ( 'NONE',  ( 47.50000000000000000, 14.49137674618942562, 10.00000000000000000 ) ) ;
#38469 = DIRECTION ( 'NONE',  ( -0.000000000000000000, -0.000000000000000000, -1.000000000000000000 ) ) ;
#38470 = AXIS2_PLACEMENT_3D ( 'NONE', #407, #1443, #65169 ) ;
#38471 = ORIENTED_EDGE ( 'NONE', *, *, #60809, .F. ) ;
#38472 = CARTESIAN_POINT ( 'NONE',  ( -45.50000000000000000, 7.768687147774684831, -6.999999999999999112 ) ) ;
#38473 = VECTOR ( 'NONE', #32262, 1000.000000000000000 ) ;
#38474 = CARTESIAN_POINT ( 'NONE',  ( -85.70499999999999829, 2.607480562269073321, 8.024999999999991473 ) ) ;
#38475 = EDGE_LOOP ( 'NONE', ( #11943, #59336, #57790, #41925 ) ) ;
#38476 = SURFACE_STYLE_USAGE ( .BOTH. , #16986 ) ;
#38477 = AXIS2_PLACEMENT_3D ( 'NONE', #32013, #25682, #20784 ) ;
#38478 = CYLINDRICAL_SURFACE ( 'NONE', #19379, 0.2500000000000002220 ) ;
#38479 = CARTESIAN_POINT ( 'NONE',  ( 74.99999999999998579, 50.00000000000000000, 9.500000000000000000 ) ) ;
#38480 = CARTESIAN_POINT ( 'NONE',  ( -67.25707362346616947, 5.598654528085800663, -7.705886871421367523 ) ) ;
#38481 = AXIS2_PLACEMENT_3D ( 'NONE', #51477, #66977, #18772 ) ;
#38482 =( LENGTH_UNIT ( ) NAMED_UNIT ( * ) SI_UNIT ( .MILLI., .METRE. ) );
#38483 = ORIENTED_EDGE ( 'NONE', *, *, #41727, .T. ) ;
#38484 = DIRECTION ( 'NONE',  ( 0.000000000000000000, 0.000000000000000000, -1.000000000000000000 ) ) ;
#38485 = CIRCLE ( 'NONE', #41832, 4.999999999999997335 ) ;
#38487 = CYLINDRICAL_SURFACE ( 'NONE', #1030, 5.000000000000004441 ) ;
#38486 =( NAMED_UNIT ( * ) SI_UNIT ( $, .STERADIAN. ) SOLID_ANGLE_UNIT ( ) );
#38488 = CARTESIAN_POINT ( 'NONE',  ( -99.50499999999996703, -6.826472737025115478, -4.959722759717899443 ) ) ;
#38489 = CARTESIAN_POINT ( 'NONE',  ( -1.166476076187854022E-15, 125.9449999999999790, 9.525000000000000355 ) ) ;
#38490 = CARTESIAN_POINT ( 'NONE',  ( -115.6449999999999818, 4.716976649647091513, -6.492361379858946790 ) ) ;
#38491 = EDGE_CURVE ( 'NONE', #21751, #30491, #61206, .T. ) ;
#38492 = MECHANICAL_DESIGN_GEOMETRIC_PRESENTATION_REPRESENTATION (  '', ( #40722 ), #44112 ) ;
#38494 = DIRECTION ( 'NONE',  ( -0.000000000000000000, 0.000000000000000000, -1.000000000000000000 ) ) ;
#38493 = CARTESIAN_POINT ( 'NONE',  ( -34.31243252642629926, -10.02680648607947589, -3.499999999999429789 ) ) ;
#38495 = CARTESIAN_POINT ( 'NONE',  ( -149.5429263765338135, 9.058813317711329915, 2.943386871421369566 ) ) ;
#38496 = CARTESIAN_POINT ( 'NONE',  ( -177.8949999999999818, 6.826472737025116366, 4.959722759717898555 ) ) ;
#38497 = EDGE_CURVE ( 'NONE', #8099, #48634, #24953, .T. ) ;
#38498 = SURFACE_STYLE_USAGE ( .BOTH. , #66198 ) ;
#38499 = EDGE_CURVE ( 'NONE', #55142, #30954, #66491, .T. ) ;
#38500 = CARTESIAN_POINT ( 'NONE',  ( 7.794228634059952476, 4.500000000000003553, 0.000000000000000000 ) ) ;
#38501 = VERTEX_POINT ( 'NONE', #62581 ) ;
#38502 = DIRECTION ( 'NONE',  ( -1.000000000000000000, 0.000000000000000000, 0.000000000000000000 ) ) ;
#38503 =( LENGTH_UNIT ( ) NAMED_UNIT ( * ) SI_UNIT ( .MILLI., .METRE. ) );
#38504 = ORIENTED_EDGE ( 'NONE', *, *, #52980, .F. ) ;
#38505 = EDGE_CURVE ( 'NONE', #6097, #52429, #49963, .T. ) ;
#38506 = CARTESIAN_POINT ( 'NONE',  ( -68.99292637653380211, 8.102448949553171076, -5.886773742842744461 ) ) ;
#38507 = CARTESIAN_POINT ( 'NONE',  ( -45.64543621907380100, 8.376853334107021709, 6.482973932537276163 ) ) ;
#38508 = STYLED_ITEM ( 'NONE', ( #18754 ), #54771 ) ;
#38509 = EDGE_CURVE ( 'NONE', #15308, #21029, #14067, .T. ) ;
#38510 = LINE ( 'NONE', #59903, #53960 ) ;
#38511 = CARTESIAN_POINT ( 'NONE',  ( -60.00000000000000000, -2.024042244987997205E-14, -10.49999999999999822 ) ) ;
#38512 = CARTESIAN_POINT ( 'NONE',  ( -60.00000000000000000, -2.024042244987997205E-14, -12.00000000000000000 ) ) ;
#38513 = DIRECTION ( 'NONE',  ( 0.9486832980505138790, 0.3162277660168378857, -0.000000000000000000 ) ) ;
#38514 = ADVANCED_FACE ( 'NONE', ( #18311 ), #34473, .F. ) ;
#38515 = ORIENTED_EDGE ( 'NONE', *, *, #6287, .T. ) ;
#38516 = CARTESIAN_POINT ( 'NONE',  ( -171.0549999999999784, -9.827790563157499189E-16, -8.024999999999991473 ) ) ;
#38517 = ORIENTED_EDGE ( 'NONE', *, *, #42722, .F. ) ;
#38518 = MECHANICAL_DESIGN_GEOMETRIC_PRESENTATION_REPRESENTATION (  '', ( #31727 ), #26100 ) ;
#38519 = PRESENTATION_STYLE_ASSIGNMENT (( #60263 ) ) ;
#38520 =( NAMED_UNIT ( * ) SI_UNIT ( $, .STERADIAN. ) SOLID_ANGLE_UNIT ( ) );
#38521 = FACE_OUTER_BOUND ( 'NONE', #40746, .T. ) ;
#38522 = LINE ( 'NONE', #64152, #43280 ) ;
#38523 = CARTESIAN_POINT ( 'NONE',  ( -2.607480562269073765, 154.2070736234661865, -8.025000000000000355 ) ) ;
#38524 = AXIS2_PLACEMENT_3D ( 'NONE', #29233, #67229, #45482 ) ;
#38525 = ORIENTED_EDGE ( 'NONE', *, *, #20988, .F. ) ;
#38526 = CARTESIAN_POINT ( 'NONE',  ( 22.00000000000002132, 50.00000000000000000, 59.99999999999999289 ) ) ;
#38527 = CARTESIAN_POINT ( 'NONE',  ( -80.30499999999999261, 8.437984349512086979, -1.550032578732815448E-15 ) ) ;
#38528 = UNCERTAINTY_MEASURE_WITH_UNIT (LENGTH_MEASURE( 1.000000000000000082E-05 ), #6453, 'distance_accuracy_value', 'NONE');
#38529 = VECTOR ( 'NONE', #44084, 1000.000000000000000 ) ;
#38530 = CARTESIAN_POINT ( 'NONE',  ( 4.716976649647099507, 132.7570736234661695, -6.492361379858953008 ) ) ;
#38531 =( NAMED_UNIT ( * ) SI_UNIT ( $, .STERADIAN. ) SOLID_ANGLE_UNIT ( ) );
#38532 = CARTESIAN_POINT ( 'NONE',  ( -168.4429263765337907, -1.166476076187852838E-15, -9.524999999999991473 ) ) ;
#38533 = CARTESIAN_POINT ( 'NONE',  ( 2.000000000000008882, 50.00000000000000000, -59.99999999999999289 ) ) ;
#38534 = VERTEX_POINT ( 'NONE', #68929 ) ;
#38535 = PRESENTATION_LAYER_ASSIGNMENT (  '', '', ( #18408 ) ) ;
#38536 = VECTOR ( 'NONE', #31519, 1000.000000000000000 ) ;
#38537 = DIRECTION ( 'NONE',  ( 0.000000000000000000, 0.000000000000000000, -1.000000000000000000 ) ) ;
#38538 = CARTESIAN_POINT ( 'NONE',  ( -61.79499999999998039, 2.607480562269068880, -8.024999999999993250 ) ) ;
#38539 = ORIENTED_EDGE ( 'NONE', *, *, #47313, .F. ) ;
#38540 = LINE ( 'NONE', #54654, #14353 ) ;
#38541 = CARTESIAN_POINT ( 'NONE',  ( -44.99999999999999289, 8.674606743306377155, -5.942398972768217824 ) ) ;
#38542 = ORIENTED_EDGE ( 'NONE', *, *, #53086, .T. ) ;
#38543 = FACE_OUTER_BOUND ( 'NONE', #10379, .T. ) ;
#38544 =( LENGTH_UNIT ( ) NAMED_UNIT ( * ) SI_UNIT ( .MILLI., .METRE. ) );
#38545 = ORIENTED_EDGE ( 'NONE', *, *, #38580, .T. ) ;
#38546 = CARTESIAN_POINT ( 'NONE',  ( 45.00000000000000000, 10.00436330937237095, -6.147562757271016309 ) ) ;
#38547 = CARTESIAN_POINT ( 'NONE',  ( -75.00000000000000000, 8.162286782231385374, 6.987283332039738504 ) ) ;
#38548 = CARTESIAN_POINT ( 'NONE',  ( -113.7549999999999955, 4.716976649647091513, -6.492361379858946790 ) ) ;
#38549 = ORIENTED_EDGE ( 'NONE', *, *, #7588, .F. ) ;
#38551 = STYLED_ITEM ( 'NONE', ( #39119 ), #22661 ) ;
#38550 = CARTESIAN_POINT ( 'NONE',  ( 3.728455551740339047, 1.573594397638760300, -7.000000000000004441 ) ) ;
#38552 = CYLINDRICAL_SURFACE ( 'NONE', #7275, 0.5000000000000004441 ) ;
#38553 = CARTESIAN_POINT ( 'NONE',  ( 16.00000000000001776, 43.00000000000000000, -29.68999999999999417 ) ) ;
#38554 = CARTESIAN_POINT ( 'NONE',  ( -71.50000000000000000, 14.49137674618942562, -9.500000000000000000 ) ) ;
#38555 = CARTESIAN_POINT ( 'NONE',  ( -147.3570736234661638, 5.598654528085804216, 7.705886871421366635 ) ) ;
#38556 = COLOUR_RGB ( '', 0.08235294, 0.09019608, 0.10196078) ;
#38557 = CARTESIAN_POINT ( 'NONE',  ( 10.01517768586949408, 135.6949999999999932, 1.839758294383810543E-15 ) ) ;
#38558 = CARTESIAN_POINT ( 'NONE',  ( -93.80707362346618083, 10.01517768586948698, -1.839758294383808571E-15 ) ) ;
#38559 =( NAMED_UNIT ( * ) SI_UNIT ( $, .STERADIAN. ) SOLID_ANGLE_UNIT ( ) );
#38560 = ORIENTED_EDGE ( 'NONE', *, *, #14374, .F. ) ;
#38562 = SURFACE_STYLE_USAGE ( .BOTH. , #22333 ) ;
#38561 = CARTESIAN_POINT ( 'NONE',  ( -7.647808743681030030, 110.5000000000002984, 5.677732506914710875 ) ) ;
#38563 = CARTESIAN_POINT ( 'NONE',  ( -72.49999999999998579, 64.07124727947029896, 9.500000000000000000 ) ) ;
#38564 = VECTOR ( 'NONE', #58410, 1000.000000000000227 ) ;
#38565 = CARTESIAN_POINT ( 'NONE',  ( -134.1550000000000011, 7.632228543268600340, 2.479861379858949277 ) ) ;
#38566 = DIRECTION ( 'NONE',  ( -0.000000000000000000, -1.000000000000000000, -0.000000000000000000 ) ) ;
#38567 = CARTESIAN_POINT ( 'NONE',  ( -45.50000000000000000, -2.024042244987997205E-14, -9.500000000000000000 ) ) ;
#38568 = CARTESIAN_POINT ( 'NONE',  ( -55.04292637653379927, -9.058813317711329915, -2.943386871421370898 ) ) ;
#38569 = CARTESIAN_POINT ( 'NONE',  ( -146.6949999999999932, -8.437984349512085203, 5.166775262442717831E-16 ) ) ;
#38570 = EDGE_CURVE ( 'NONE', #13067, #37066, #16247, .T. ) ;
#38571 = CARTESIAN_POINT ( 'NONE',  ( -133.0449999999999875, 7.632228543268600340, 2.479861379858949277 ) ) ;
#38572 = VERTEX_POINT ( 'NONE', #25633 ) ;
#38573 = SURFACE_SIDE_STYLE ('',( #3522 ) ) ;
#38574 = EDGE_CURVE ( 'NONE', #41595, #52470, #40471, .T. ) ;
#38575 = DIRECTION ( 'NONE',  ( -0.7071067811865426878, 0.000000000000000000, -0.7071067811865524577 ) ) ;
#38576 = CARTESIAN_POINT ( 'NONE',  ( -48.20499999999999829, -2.607480562269071545, -8.024999999999991473 ) ) ;
#38577 = SURFACE_STYLE_FILL_AREA ( #44881 ) ;
#38578 = AXIS2_PLACEMENT_3D ( 'NONE', #29217, #55630, #12344 ) ;
#38579 = CARTESIAN_POINT ( 'NONE',  ( -61.64499999999998892, 4.716976649647091513, -6.492361379858946790 ) ) ;
#38580 = EDGE_CURVE ( 'NONE', #61196, #31124, #69271, .T. ) ;
#38581 = CARTESIAN_POINT ( 'NONE',  ( -139.0429263765338135, -9.058813317711329915, -2.943386871421370898 ) ) ;
#38582 = CARTESIAN_POINT ( 'NONE',  ( -195.0000000000000000, 0.000000000000000000, 9.524999999999991473 ) ) ;
#38583 = EDGE_CURVE ( 'NONE', #27901, #60674, #54799, .T. ) ;
#38584 = MECHANICAL_DESIGN_GEOMETRIC_PRESENTATION_REPRESENTATION (  '', ( #3644 ), #16070 ) ;
#38585 = COLOUR_RGB ( '', 0.09019608, 0.27058824, 0.51372549) ;
#38586 = SURFACE_STYLE_USAGE ( .BOTH. , #54354 ) ;
#38587 = CARTESIAN_POINT ( 'NONE',  ( -76.55707362346616662, -1.166476076187852838E-15, -9.524999999999991473 ) ) ;
#38588 = CARTESIAN_POINT ( 'NONE',  ( -92.99292637653381632, 8.102448949553171076, -5.886773742842744461 ) ) ;
#38589 = DIRECTION ( 'NONE',  ( -1.000000000000000000, -1.162264728904460753E-15, -1.387778780781445676E-16 ) ) ;
#38590 = CARTESIAN_POINT ( 'NONE',  ( -195.0000000000000000, 1.166476076187852838E-15, -9.524999999999991473 ) ) ;
#38591 = AXIS2_PLACEMENT_3D ( 'NONE', #63903, #31551, #41815 ) ;
#38592 = EDGE_CURVE ( 'NONE', #25561, #51395, #12825, .T. ) ;
#38593 = CARTESIAN_POINT ( 'NONE',  ( 0.000000000000000000, 87.30187232391182306, 0.000000000000000000 ) ) ;
#38594 =( LENGTH_UNIT ( ) NAMED_UNIT ( * ) SI_UNIT ( .MILLI., .METRE. ) );
#38595 = ORIENTED_EDGE ( 'NONE', *, *, #29621, .F. ) ;
#38596 = FACE_OUTER_BOUND ( 'NONE', #35016, .T. ) ;
#38597 = CARTESIAN_POINT ( 'NONE',  ( 71.50000000000000000, 14.49137674618942562, -7.500000000000000000 ) ) ;
#38598 = ORIENTED_EDGE ( 'NONE', *, *, #39982, .F. ) ;
#38599 = VECTOR ( 'NONE', #21100, 1000.000000000000000 ) ;
#38600 = CARTESIAN_POINT ( 'NONE',  ( -7.632228543268607446, 121.6570736234661609, -2.479861379858953718 ) ) ;
#38601 = CARTESIAN_POINT ( 'NONE',  ( 61.74999999999998579, 31.24999999999999289, 4.000000000000000000 ) ) ;
#38602 = CIRCLE ( 'NONE', #51077, 13.49999999999999822 ) ;
#38603 =( NAMED_UNIT ( * ) SI_UNIT ( $, .STERADIAN. ) SOLID_ANGLE_UNIT ( ) );
#38604 = VERTEX_POINT ( 'NONE', #36245 ) ;
#38605 = ORIENTED_EDGE ( 'NONE', *, *, #13785, .T. ) ;
#38606 = STYLED_ITEM ( 'NONE', ( #30585 ), #6454 ) ;
#38607 = DIRECTION ( 'NONE',  ( -0.000000000000000000, 1.000000000000000000, -0.000000000000000000 ) ) ;
#38608 = ORIENTED_EDGE ( 'NONE', *, *, #69051, .F. ) ;
#38609 = SURFACE_STYLE_FILL_AREA ( #27965 ) ;
#38610 = LINE ( 'NONE', #60009, #68185 ) ;
#38611 = CARTESIAN_POINT ( 'NONE',  ( 2.607480562268909008, 149.7929263765338135, -8.025000000000122924 ) ) ;
#38612 = CARTESIAN_POINT ( 'NONE',  ( -91.64499999999999602, 4.716976649647091513, -6.492361379858946790 ) ) ;
#38613 = ORIENTED_EDGE ( 'NONE', *, *, #29451, .F. ) ;
#38614 = EDGE_CURVE ( 'NONE', #37329, #47990, #66760, .T. ) ;
#38615 = VECTOR ( 'NONE', #54416, 1000.000000000000000 ) ;
#38616 = FACE_OUTER_BOUND ( 'NONE', #32423, .T. ) ;
#38617 = CYLINDRICAL_SURFACE ( 'NONE', #1861, 9.524999999999991473 ) ;
#38618 = DIRECTION ( 'NONE',  ( 0.000000000000000000, 0.000000000000000000, 1.000000000000000000 ) ) ;
#38619 = VERTEX_POINT ( 'NONE', #9838 ) ;
#38620 = CARTESIAN_POINT ( 'NONE',  ( 74.50000000000000000, -2.135340797662720349E-14, -9.500000000000000000 ) ) ;
#38621 = DIRECTION ( 'NONE',  ( 7.080503983578803083E-17, 1.000000000000000000, 0.000000000000000000 ) ) ;
#38622 = ORIENTED_EDGE ( 'NONE', *, *, #26958, .F. ) ;
#38623 = CARTESIAN_POINT ( 'NONE',  ( 3.000000000000030198, 38.70020753820971748, 89.00000000000000000 ) ) ;
#38624 = ORIENTED_EDGE ( 'NONE', *, *, #1447, .T. ) ;
#38625 = FILL_AREA_STYLE ('',( #16472 ) ) ;
#38626 = CARTESIAN_POINT ( 'NONE',  ( 179.4098300562505415, 0.000000000000000000, 5.000000000000000000 ) ) ;
#38627 = PLANE ( 'NONE',  #35522 ) ;
#38629 = COLOUR_RGB ( '', 0.40784314, 0.44705882, 0.49803922) ;
#38628 = AXIS2_PLACEMENT_3D ( 'NONE', #32308, #33693, #34719 ) ;
#38630 = CARTESIAN_POINT ( 'NONE',  ( -183.0570736234661808, 0.000000000000000000, 9.524999999999991473 ) ) ;
#38631 = LINE ( 'NONE', #18164, #17327 ) ;
#38632 = CIRCLE ( 'NONE', #64456, 5.000000000000004441 ) ;
#38633 = DIRECTION ( 'NONE',  ( 0.000000000000000000, 1.000000000000000000, 0.000000000000000000 ) ) ;
#38634 = CARTESIAN_POINT ( 'NONE',  ( -7.398101581744998434, 153.3646217335120809, -3.965660541892891189 ) ) ;
#38635 = EDGE_LOOP ( 'NONE', ( #3051, #12741, #8219, #36895 ) ) ;
#38636 = CARTESIAN_POINT ( 'NONE',  ( -161.6929263765337907, 10.01517768586948698, -1.839758294383808966E-15 ) ) ;
#38637 = CARTESIAN_POINT ( 'NONE',  ( 18.25000000000000711, 33.99999999999999289, -3.750000000000000000 ) ) ;
#38638 = EDGE_CURVE ( 'NONE', #25839, #66384, #52750, .T. ) ;
#38639 = SURFACE_SIDE_STYLE ('',( #17167 ) ) ;
#38640 = ORIENTED_EDGE ( 'NONE', *, *, #6655, .T. ) ;
#38641 = CYLINDRICAL_SURFACE ( 'NONE', #24864, 0.5000000000000004441 ) ;
#38642 = VECTOR ( 'NONE', #6775, 1000.000000000000000 ) ;
#38643 = CARTESIAN_POINT ( 'NONE',  ( -157.1049999999999898, -6.826472737025115478, 4.959722759717900331 ) ) ;
#38644 = ADVANCED_FACE ( 'NONE', ( #59360 ), #902, .T. ) ;
#38645 = CARTESIAN_POINT ( 'NONE',  ( -195.0000000000000000, 0.000000000000000000, 0.000000000000000000 ) ) ;
#38646 = CARTESIAN_POINT ( 'NONE',  ( 69.74999999999998579, 37.00000000000000000, 3.000000000000000000 ) ) ;
#38647 = CARTESIAN_POINT ( 'NONE',  ( -178.7949999999999875, 2.607480562269068880, -8.024999999999993250 ) ) ;
#38648 = VECTOR ( 'NONE', #62529, 1000.000000000000000 ) ;
#38649 = CARTESIAN_POINT ( 'NONE',  ( -158.2450000000000045, -4.716976649647093289, -6.492361379858945902 ) ) ;
#38650 = EDGE_LOOP ( 'NONE', ( #25410, #53887, #45551, #68276 ) ) ;
#38651 = VECTOR ( 'NONE', #15422, 1000.000000000000000 ) ;
#38652 = EDGE_CURVE ( 'NONE', #23317, #44704, #28573, .T. ) ;
#38653 = SURFACE_STYLE_FILL_AREA ( #21732 ) ;
#38654 = SURFACE_STYLE_FILL_AREA ( #6565 ) ;
#38655 = DIRECTION ( 'NONE',  ( 0.000000000000000000, 0.000000000000000000, -1.000000000000000000 ) ) ;
#38656 = VECTOR ( 'NONE', #6965, 1000.000000000000000 ) ;
#38657 = CARTESIAN_POINT ( 'NONE',  ( -69.20499999999998408, -2.607480562269071545, -8.024999999999991473 ) ) ;
#38658 = DIRECTION ( 'NONE',  ( 0.000000000000000000, 1.000000000000000000, 0.000000000000000000 ) ) ;
#38659 = CIRCLE ( 'NONE', #23993, 0.2500000000000002220 ) ;
#38660 = VECTOR ( 'NONE', #47866, 1000.000000000000000 ) ;
#38661 = CARTESIAN_POINT ( 'NONE',  ( -84.74499999999999034, 4.716976649647094177, 6.492361379858945902 ) ) ;
#38662 = CARTESIAN_POINT ( 'NONE',  ( -5.598654528085806881, 140.8549999999999898, -7.705886871421374629 ) ) ;
#38663 =( NAMED_UNIT ( * ) PLANE_ANGLE_UNIT ( ) SI_UNIT ( $, .RADIAN. ) );
#38664 = ADVANCED_FACE ( 'NONE', ( #2593 ), #48534, .T. ) ;
#38665 = AXIS2_PLACEMENT_3D ( 'NONE', #44063, #59479, #41719 ) ;
#38666 = CARTESIAN_POINT ( 'NONE',  ( 54.49999999999999289, 2.470600640510329340E-15, -6.500000000000000000 ) ) ;
#38667 = PRESENTATION_LAYER_ASSIGNMENT (  '', '', ( #11703 ) ) ;
#38668 = AXIS2_PLACEMENT_3D ( 'NONE', #18133, #61024, #33607 ) ;
#38669 = VERTEX_POINT ( 'NONE', #48885 ) ;
#38670 = EDGE_CURVE ( 'NONE', #40163, #1577, #29000, .T. ) ;
#38671 = SURFACE_SIDE_STYLE ('',( #9918 ) ) ;
#38672 = DIRECTION ( 'NONE',  ( 0.000000000000000000, 0.000000000000000000, 1.000000000000000000 ) ) ;
#38673 = DIRECTION ( 'NONE',  ( 0.000000000000000000, -0.000000000000000000, 1.000000000000000000 ) ) ;
#38674 = EDGE_LOOP ( 'NONE', ( #60525, #58752, #921 ) ) ;
#38676 = EDGE_LOOP ( 'NONE', ( #25051, #31742, #48931, #39397 ) ) ;
#38675 = MECHANICAL_DESIGN_GEOMETRIC_PRESENTATION_REPRESENTATION (  '', ( #50988 ), #10525 ) ;
#38677 =( GEOMETRIC_REPRESENTATION_CONTEXT ( 3 ) GLOBAL_UNCERTAINTY_ASSIGNED_CONTEXT ( ( #5205 ) ) GLOBAL_UNIT_ASSIGNED_CONTEXT ( ( #10100, #53010, #19231 ) ) REPRESENTATION_CONTEXT ( 'NONE', 'WORKASPACE' ) );
#38678 = SURFACE_SIDE_STYLE ('',( #59730 ) ) ;
#38679 = AXIS2_PLACEMENT_3D ( 'NONE', #8143, #67936, #34513 ) ;
#38680 = SURFACE_STYLE_FILL_AREA ( #17215 ) ;
#38681 = SURFACE_SIDE_STYLE ('',( #53441 ) ) ;
#38682 = EDGE_LOOP ( 'NONE', ( #50371, #20506, #36965, #53932 ) ) ;
#38683 = CARTESIAN_POINT ( 'NONE',  ( -113.6049999999999898, 6.826472737025113702, -4.959722759717902107 ) ) ;
#38684 = VERTEX_POINT ( 'NONE', #21764 ) ;
#38685 = FILL_AREA_STYLE ('',( #28043 ) ) ;
#38686 = CYLINDRICAL_SURFACE ( 'NONE', #26515, 0.5000000000000004441 ) ;
#38687 = AXIS2_PLACEMENT_3D ( 'NONE', #27095, #58440, #31702 ) ;
#38688 = ORIENTED_EDGE ( 'NONE', *, *, #49426, .F. ) ;
#38689 = SURFACE_STYLE_FILL_AREA ( #22463 ) ;
#38690 = CARTESIAN_POINT ( 'NONE',  ( -6.418790567836330396, -2.472216779103305395, 2.882328613363590808 ) ) ;
#38691 = ORIENTED_EDGE ( 'NONE', *, *, #59631, .F. ) ;
#38692 = CARTESIAN_POINT ( 'NONE',  ( 57.74999999999998579, 30.74999999999999289, -3.750000000000000000 ) ) ;
#38693 = CARTESIAN_POINT ( 'NONE',  ( -8.102448949553181734, 155.4950000000000045, 5.886773742842747126 ) ) ;
#38694 = DIRECTION ( 'NONE',  ( 0.000000000000000000, 0.000000000000000000, -1.000000000000000000 ) ) ;
#38695 = ORIENTED_EDGE ( 'NONE', *, *, #26703, .F. ) ;
#38696 = AXIS2_PLACEMENT_3D ( 'NONE', #44932, #8653, #18837 ) ;
#38697 = EDGE_CURVE ( 'NONE', #68077, #65971, #470, .T. ) ;
#38698 = ORIENTED_EDGE ( 'NONE', *, *, #15369, .T. ) ;
#38699 = DIRECTION ( 'NONE',  ( -0.000000000000000000, -0.000000000000000000, -1.000000000000000000 ) ) ;
#38700 = CARTESIAN_POINT ( 'NONE',  ( -7.794228634059947147, -2.500000000000000000, -4.500000000000000000 ) ) ;
#38701 = AXIS2_PLACEMENT_3D ( 'NONE', #9919, #67974, #41254 ) ;
#38702 = VERTEX_POINT ( 'NONE', #66670 ) ;
#38703 = CARTESIAN_POINT ( 'NONE',  ( 6.826472737025119919, 130.8929263765338362, 4.959722759717908325 ) ) ;
#38704 = CARTESIAN_POINT ( 'NONE',  ( 57.00000000000000000, 1.000000000000000000, 79.00402776293826435 ) ) ;
#38705 = DIRECTION ( 'NONE',  ( 0.000000000000000000, 0.000000000000000000, -1.000000000000000000 ) ) ;
#38706 = CIRCLE ( 'NONE', #19573, 1.000000000000000888 ) ;
#38707 = CARTESIAN_POINT ( 'NONE',  ( 1.800649583398763021, -9.000000000000007105, 0.1402270904467407264 ) ) ;
#38708 = DIRECTION ( 'NONE',  ( 0.000000000000000000, 1.000000000000000000, -0.000000000000000000 ) ) ;
#38709 = ORIENTED_EDGE ( 'NONE', *, *, #27092, .F. ) ;
#38710 = ORIENTED_EDGE ( 'NONE', *, *, #34024, .F. ) ;
#38711 = CARTESIAN_POINT ( 'NONE',  ( -48.44292637653380496, -1.166476076187852838E-15, -9.524999999999991473 ) ) ;
#38712 = CARTESIAN_POINT ( 'NONE',  ( 0.000000000000000000, 0.000000000000000000, 24.00000000000000000 ) ) ;
#38713 = CIRCLE ( 'NONE', #42090, 0.4999999999999994449 ) ;
#38714 = CARTESIAN_POINT ( 'NONE',  ( -138.5049999999999955, -6.826472737025115478, -4.959722759717899443 ) ) ;
#38715 = DIRECTION ( 'NONE',  ( 0.000000000000000000, 0.000000000000000000, 1.000000000000000000 ) ) ;
#38716 = ORIENTED_EDGE ( 'NONE', *, *, #56725, .T. ) ;
#38717 = STYLED_ITEM ( 'NONE', ( #9734 ), #26884 ) ;
#38718 = MECHANICAL_DESIGN_GEOMETRIC_PRESENTATION_REPRESENTATION (  '', ( #20536 ), #24058 ) ;
#38719 = ADVANCED_FACE ( 'NONE', ( #59732 ), #6266, .T. ) ;
#38720 = CARTESIAN_POINT ( 'NONE',  ( -157.3429263765337964, -9.058813317711329915, 2.943386871421371787 ) ) ;
#38721 = CARTESIAN_POINT ( 'NONE',  ( -45.00000000000000000, 9.290263934145977842, -6.640705990143890070 ) ) ;
#38722 = ORIENTED_EDGE ( 'NONE', *, *, #28972, .F. ) ;
#38723 = ORIENTED_EDGE ( 'NONE', *, *, #45391, .F. ) ;
#38724 = CARTESIAN_POINT ( 'NONE',  ( -44.99742101275325012, 9.654581538856286116, 3.431521703149617242 ) ) ;
#38725 = SURFACE_SIDE_STYLE ('',( #17263 ) ) ;
#38726 = EDGE_CURVE ( 'NONE', #46628, #69646, #3280, .T. ) ;
#38728 = CARTESIAN_POINT ( 'NONE',  ( -58.40499999999997982, -2.607480562269069768, 8.024999999999991473 ) ) ;
#38727 = AXIS2_PLACEMENT_3D ( 'NONE', #34193, #39494, #53150 ) ;
#38729 = ORIENTED_EDGE ( 'NONE', *, *, #10104, .F. ) ;
#38730 = FACE_OUTER_BOUND ( 'NONE', #37440, .T. ) ;
#38731 = SURFACE_STYLE_USAGE ( .BOTH. , #49949 ) ;
#38732 = EDGE_CURVE ( 'NONE', #59828, #21622, #51886, .T. ) ;
#38733 =( GEOMETRIC_REPRESENTATION_CONTEXT ( 3 ) GLOBAL_UNCERTAINTY_ASSIGNED_CONTEXT ( ( #59258 ) ) GLOBAL_UNIT_ASSIGNED_CONTEXT ( ( #23074, #28300, #1550 ) ) REPRESENTATION_CONTEXT ( 'NONE', 'WORKASPACE' ) );
#38734 = AXIS2_PLACEMENT_3D ( 'NONE', #13189, #34647, #56105 ) ;
#38735 = CARTESIAN_POINT ( 'NONE',  ( -28.74999999999999645, -13.99999999999999822, 11.89999999999999858 ) ) ;
#38736 = DIRECTION ( 'NONE',  ( 0.8660254037844387076, -0.000000000000000000, 0.5000000000000001110 ) ) ;
#38737 = ORIENTED_EDGE ( 'NONE', *, *, #25650, .F. ) ;
#38738 = ADVANCED_FACE ( 'NONE', ( #4338 ), #24768, .T. ) ;
#38739 = CARTESIAN_POINT ( 'NONE',  ( -129.4429263765338192, -1.166476076187852838E-15, -9.524999999999991473 ) ) ;
#38740 = FACE_OUTER_BOUND ( 'NONE', #34165, .T. ) ;
#38741 = DIRECTION ( 'NONE',  ( 0.000000000000000000, 0.000000000000000000, 1.000000000000000000 ) ) ;
#38742 = ADVANCED_FACE ( 'NONE', ( #4005 ), #46989, .F. ) ;
#38743 = CARTESIAN_POINT ( 'NONE',  ( -109.4949999999999619, 6.826472737025113702, -4.959722759717902107 ) ) ;
#38744 = CARTESIAN_POINT ( 'NONE',  ( -9.058813317711338797, 155.3449999999999704, 2.943386871421373563 ) ) ;
#38745 = CARTESIAN_POINT ( 'NONE',  ( -75.29500000000000171, -2.607480562269069768, 8.024999999999991473 ) ) ;
#38746 = DIRECTION ( 'NONE',  ( 0.000000000000000000, 0.000000000000000000, -1.000000000000000000 ) ) ;
#38747 = CARTESIAN_POINT ( 'NONE',  ( -2.607480562269157254, 141.0929263765338533, -8.024999999999939959 ) ) ;
#38748 = STYLED_ITEM ( 'NONE', ( #51509 ), #37546 ) ;
#38749 = FACE_BOUND ( 'NONE', #8576, .T. ) ;
#38750 = DIRECTION ( 'NONE',  ( -1.000000000000000000, 0.000000000000000000, 0.000000000000000000 ) ) ;
#38751 = ORIENTED_EDGE ( 'NONE', *, *, #34532, .T. ) ;
#38752 = CARTESIAN_POINT ( 'NONE',  ( -122.5429263765337993, 9.058813317711329915, 2.943386871421369566 ) ) ;
#38753 = AXIS2_PLACEMENT_3D ( 'NONE', #3430, #25964, #68914 ) ;
#38754 = SURFACE_SIDE_STYLE ('',( #38050 ) ) ;
#38755 = CARTESIAN_POINT ( 'NONE',  ( -147.8949999999999818, 6.826472737025116366, 4.959722759717898555 ) ) ;
#38756 = CARTESIAN_POINT ( 'NONE',  ( 0.000000000000000000, 87.30187232391182306, 0.000000000000000000 ) ) ;
#38757 = ORIENTED_EDGE ( 'NONE', *, *, #63470, .T. ) ;
#38758 = ORIENTED_EDGE ( 'NONE', *, *, #58856, .T. ) ;
#38759 = EDGE_CURVE ( 'NONE', #28382, #51968, #25819, .T. ) ;
#38760 = CARTESIAN_POINT ( 'NONE',  ( 10.39230484541327115, -4.119968255444916849E-15, 7.500000000000000000 ) ) ;
#38761 = DIRECTION ( 'NONE',  ( -1.000000000000000000, 0.000000000000000000, -0.000000000000000000 ) ) ;
#38762 = CARTESIAN_POINT ( 'NONE',  ( -22.25000000000000711, 33.74999999999999289, 3.750000000000000000 ) ) ;
#38763 = FILL_AREA_STYLE ('',( #43696 ) ) ;
#38764 =( LENGTH_UNIT ( ) NAMED_UNIT ( * ) SI_UNIT ( .MILLI., .METRE. ) );
#38765 = ORIENTED_EDGE ( 'NONE', *, *, #48092, .F. ) ;
#38766 = CARTESIAN_POINT ( 'NONE',  ( -143.0049999999999955, 6.826472737025115478, 4.959722759717899443 ) ) ;
#38767 = ORIENTED_EDGE ( 'NONE', *, *, #11006, .T. ) ;
#38768 = TOROIDAL_SURFACE ( 'NONE', #56709, 1.499999999999998668, 1.000000000000000000 ) ;
#38769 = ORIENTED_EDGE ( 'NONE', *, *, #43175, .F. ) ;
#38770 = CARTESIAN_POINT ( 'NONE',  ( 0.000000000000000000, 154.9999999999999716, -23.00000000000000000 ) ) ;
#38771 = ORIENTED_EDGE ( 'NONE', *, *, #18298, .T. ) ;
#38772 = TOROIDAL_SURFACE ( 'NONE', #8419, 0.5000000000000000000, 0.2500000000000000000 ) ;
#38773 = AXIS2_PLACEMENT_3D ( 'NONE', #14969, #19160, #8292 ) ;
#38774 = AXIS2_PLACEMENT_3D ( 'NONE', #28588, #27272, #1814 ) ;
#38775 = CARTESIAN_POINT ( 'NONE',  ( -57.11974195712093660, -8.499999999999992895, 0.06931351858119258469 ) ) ;
#38776 = FILL_AREA_STYLE ('',( #45093 ) ) ;
#38777 = CARTESIAN_POINT ( 'NONE',  ( -5.598654528085806881, 133.7450000000000045, -7.705886871421374629 ) ) ;
#38778 = SURFACE_STYLE_FILL_AREA ( #33121 ) ;
#38779 = ORIENTED_EDGE ( 'NONE', *, *, #5292, .F. ) ;
#38780 = CARTESIAN_POINT ( 'NONE',  ( -195.0000000000000000, 0.000000000000000000, 9.524999999999991473 ) ) ;
#38781 = CARTESIAN_POINT ( 'NONE',  ( -9.058813317711337021, 126.1549999999999869, -2.943386871421374895 ) ) ;
#38782 = CARTESIAN_POINT ( 'NONE',  ( -51.35499999999998266, -4.716976649647093289, -6.492361379858945902 ) ) ;
#38783 = VERTEX_POINT ( 'NONE', #13530 ) ;
#38784 = CARTESIAN_POINT ( 'NONE',  ( 3.094860106618435136, 158.4049999999999727, -9.525000000000000355 ) ) ;
#38785 = CARTESIAN_POINT ( 'NONE',  ( 3.673940397442060361E-16, 2.000000000000000444, -3.000000000000000444 ) ) ;
#38786 = VECTOR ( 'NONE', #56848, 1000.000000000000227 ) ;
#38787 = PLANE ( 'NONE',  #26072 ) ;
#38788 = STYLED_ITEM ( 'NONE', ( #39618 ), #38664 ) ;
#38789 = DIRECTION ( 'NONE',  ( -1.000000000000000000, 0.000000000000000000, 0.000000000000000000 ) ) ;
#38790 = VERTEX_POINT ( 'NONE', #57134 ) ;
#38791 = AXIS2_PLACEMENT_3D ( 'NONE', #7165, #60953, #28594 ) ;
#38792 = FILL_AREA_STYLE_COLOUR ( '', #7071 ) ;
#38793 = ORIENTED_EDGE ( 'NONE', *, *, #43590, .T. ) ;
#38794 = CYLINDRICAL_SURFACE ( 'NONE', #41268, 0.2500000000000002220 ) ;
#38795 = DIRECTION ( 'NONE',  ( 9.376883653928687363E-17, -1.000000000000000000, 0.000000000000000000 ) ) ;
#38796 = CARTESIAN_POINT ( 'NONE',  ( -167.1550000000000011, 7.632228543268600340, 2.479861379858949277 ) ) ;
#38797 = ORIENTED_EDGE ( 'NONE', *, *, #59817, .T. ) ;
#38798 = LINE ( 'NONE', #47988, #56444 ) ;
#38799 = AXIS2_PLACEMENT_3D ( 'NONE', #17721, #39192, #45169 ) ;
#38800 = DIRECTION ( 'NONE',  ( 0.6842105263157866046, 0.7292845505553195995, 0.000000000000000000 ) ) ;
#38801 = EDGE_CURVE ( 'NONE', #32321, #6265, #63450, .T. ) ;
#38802 =( NAMED_UNIT ( * ) SI_UNIT ( $, .STERADIAN. ) SOLID_ANGLE_UNIT ( ) );
#38803 = PRESENTATION_STYLE_ASSIGNMENT (( #55634 ) ) ;
#38804 = CARTESIAN_POINT ( 'NONE',  ( -77.84292637653379643, 9.058813317711329915, -2.943386871421373119 ) ) ;
#38805 = ORIENTED_EDGE ( 'NONE', *, *, #39333, .T. ) ;
#38806 = CARTESIAN_POINT ( 'NONE',  ( -44.99154893936432842, 9.591540374752314690, -3.000000000000000444 ) ) ;
#38808 = ADVANCED_FACE ( 'NONE', ( #30382, #41348 ), #14586, .F. ) ;
#38807 = CARTESIAN_POINT ( 'NONE',  ( -8.750000000000001776, 25.24999999999998934, 4.000000000000000000 ) ) ;
#38809 = CARTESIAN_POINT ( 'NONE',  ( -84.95499999999998408, -7.632228543268599452, 2.479861379858951054 ) ) ;
#38810 = ORIENTED_EDGE ( 'NONE', *, *, #26292, .T. ) ;
#38811 =( LENGTH_UNIT ( ) NAMED_UNIT ( * ) SI_UNIT ( .MILLI., .METRE. ) );
#38812 = PRESENTATION_STYLE_ASSIGNMENT (( #22597 ) ) ;
#38813 = FILL_AREA_STYLE ('',( #39154 ) ) ;
#38814 = CARTESIAN_POINT ( 'NONE',  ( -52.55707362346618083, -1.166476076187852838E-15, -9.524999999999991473 ) ) ;
#38815 = COLOUR_RGB ( '', 0.09019608, 0.27058824, 0.51372549) ;
#38816 = AXIS2_PLACEMENT_3D ( 'NONE', #46421, #25943, #3776 ) ;
#38817 = DIRECTION ( 'NONE',  ( 0.000000000000000000, 0.000000000000000000, 1.000000000000000000 ) ) ;
#38818 = VERTEX_POINT ( 'NONE', #58190 ) ;
#38819 = CARTESIAN_POINT ( 'NONE',  ( -75.50000000000000000, 64.49137674618943095, -9.500000000000001776 ) ) ;
#38821 = SURFACE_STYLE_USAGE ( .BOTH. , #54925 ) ;
#38820 = PRESENTATION_STYLE_ASSIGNMENT (( #6406 ) ) ;
#38822 = ADVANCED_FACE ( 'NONE', ( #11379 ), #32843, .T. ) ;
#38823 = AXIS2_PLACEMENT_3D ( 'NONE', #42821, #54691, #27600 ) ;
#38824 = CARTESIAN_POINT ( 'NONE',  ( -5.598654528085808657, 128.6449999999999818, 7.705886871421373741 ) ) ;
#38825 = CARTESIAN_POINT ( 'NONE',  ( -118.7950000000000017, 2.607480562269068880, -8.024999999999993250 ) ) ;
#38826 = COLOUR_RGB ( '', 0.09019608, 0.27058824, 0.51372549) ;
#38827 = VECTOR ( 'NONE', #64637, 1000.000000000000000 ) ;
#38828 = CARTESIAN_POINT ( 'NONE',  ( -78.44292637653380496, -1.166476076187852838E-15, -9.524999999999991473 ) ) ;
#38830 = CARTESIAN_POINT ( 'NONE',  ( -16.62366585040244971, 11.02492648493062610, -4.740184257027916459 ) ) ;
#38829 = CARTESIAN_POINT ( 'NONE',  ( 0.000000000000000000, 8.270287287112621792E-15, 12.50000000000000000 ) ) ;
#38831 = CARTESIAN_POINT ( 'NONE',  ( -154.6429263765338078, -5.598654528085801552, 7.705886871421367523 ) ) ;
#38832 = CARTESIAN_POINT ( 'NONE',  ( -179.8449999999999989, -7.632228543268599452, 2.479861379858951054 ) ) ;
#38833 = AXIS2_PLACEMENT_3D ( 'NONE', #64771, #10277, #32068 ) ;
#38834 = DIRECTION ( 'NONE',  ( -8.673617379884015751E-17, 0.000000000000000000, -1.000000000000000000 ) ) ;
#38835 = STYLED_ITEM ( 'NONE', ( #46582 ), #57826 ) ;
#38836 = FACE_OUTER_BOUND ( 'NONE', #49295, .T. ) ;
#38837 = VERTEX_POINT ( 'NONE', #32148 ) ;
#38838 = FACE_OUTER_BOUND ( 'NONE', #8915, .T. ) ;
#38839 = ORIENTED_EDGE ( 'NONE', *, *, #46016, .F. ) ;
#38840 = CARTESIAN_POINT ( 'NONE',  ( -67.19292637653379074, -10.01517768586948698, 6.132527647946031529E-16 ) ) ;
#38841 = EDGE_CURVE ( 'NONE', #51117, #20590, #61185, .T. ) ;
#38842 = VECTOR ( 'NONE', #33119, 1000.000000000000000 ) ;
#38843 = DIRECTION ( 'NONE',  ( 0.000000000000000000, 0.000000000000000000, 1.000000000000000000 ) ) ;
#38844 = SHAPE_REPRESENTATION ( '11. Nut M10', ( #42840 ), #37166 ) ;
#38845 = CARTESIAN_POINT ( 'NONE',  ( -4.041451884327381450, -7.000000000000002665, 7.500000000000000000 ) ) ;
#38846 = DIRECTION ( 'NONE',  ( -0.000000000000000000, -1.000000000000000000, -0.000000000000000000 ) ) ;
#38847 = DIRECTION ( 'NONE',  ( 0.000000000000000000, 1.000000000000000000, 0.000000000000000000 ) ) ;
#38848 = CARTESIAN_POINT ( 'NONE',  ( -74.99999999999998579, 50.00000000000000000, -11.50000000000001066 ) ) ;
#38849 = ORIENTED_EDGE ( 'NONE', *, *, #43649, .T. ) ;
#38850 = CARTESIAN_POINT ( 'NONE',  ( -171.8049999999999784, -8.437984349512086979, 5.166775262442717831E-16 ) ) ;
#38851 = B_SPLINE_CURVE_WITH_KNOTS ( 'NONE', 3,
 ( #21494, #36696, #43005, #36336, #58113, #57763, #32377, #63017 ),
 .UNSPECIFIED., .F., .F.,
 ( 4, 2, 2, 4 ),
 ( 2.544316211733585141E-07, 0.002094919859796804708, 0.003142252573884620707, 0.004189585287972436706 ),
 .UNSPECIFIED. ) ;
#38852 = ORIENTED_EDGE ( 'NONE', *, *, #26825, .T. ) ;
#38853 = DIRECTION ( 'NONE',  ( 1.000000000000000000, 0.000000000000000000, 0.000000000000000000 ) ) ;
#38854 = FILL_AREA_STYLE ('',( #54633 ) ) ;
#38855 = DIRECTION ( 'NONE',  ( 0.000000000000000000, 0.000000000000000000, -1.000000000000000000 ) ) ;
#38856 = PRESENTATION_STYLE_ASSIGNMENT (( #1808 ) ) ;
#38857 = CARTESIAN_POINT ( 'NONE',  ( -6.826472737025120807, 152.1070736234661354, 4.959722759717906548 ) ) ;
#38858 = EDGE_LOOP ( 'NONE', ( #12942, #48978, #61120, #44331 ) ) ;
#38859 = SURFACE_STYLE_FILL_AREA ( #17395 ) ;
#38860 = CARTESIAN_POINT ( 'NONE',  ( -88.25499999999998124, -4.716976649647092401, 6.492361379858946790 ) ) ;
#38861 =( NAMED_UNIT ( * ) SI_UNIT ( $, .STERADIAN. ) SOLID_ANGLE_UNIT ( ) );
#38862 =( NAMED_UNIT ( * ) SI_UNIT ( $, .STERADIAN. ) SOLID_ANGLE_UNIT ( ) );
#38863 = MECHANICAL_DESIGN_GEOMETRIC_PRESENTATION_REPRESENTATION (  '', ( #16423 ), #61307 ) ;
#38864 = SURFACE_STYLE_FILL_AREA ( #60277 ) ;
#38865 = DIRECTION ( 'NONE',  ( 1.000000000000000000, 0.000000000000000000, 0.000000000000000000 ) ) ;
#38866 = CARTESIAN_POINT ( 'NONE',  ( -23.71231517720798010, 112.9999999999999858, 9.500000000000000000 ) ) ;
#38867 = ADVANCED_FACE ( 'NONE', ( #21954 ), #69088, .F. ) ;
#38868 =( GEOMETRIC_REPRESENTATION_CONTEXT ( 3 ) GLOBAL_UNCERTAINTY_ASSIGNED_CONTEXT ( ( #37723 ) ) GLOBAL_UNIT_ASSIGNED_CONTEXT ( ( #14252, #24434, #67723 ) ) REPRESENTATION_CONTEXT ( 'NONE', 'WORKASPACE' ) );
#38869 = ORIENTED_EDGE ( 'NONE', *, *, #32386, .F. ) ;
#38870 = MECHANICAL_DESIGN_GEOMETRIC_PRESENTATION_REPRESENTATION (  '', ( #29833 ), #602 ) ;
#38871 = CARTESIAN_POINT ( 'NONE',  ( -140.3070736234661808, -10.01517768586948698, 6.132527647946031529E-16 ) ) ;
#38872 = FILL_AREA_STYLE_COLOUR ( '', #2483 ) ;
#38873 = CARTESIAN_POINT ( 'NONE',  ( -64.49499999999997613, 6.826472737025113702, -4.959722759717902107 ) ) ;
#38874 = VERTEX_POINT ( 'NONE', #16690 ) ;
#38875 = PLANE ( 'NONE',  #21558 ) ;
#38876 = LINE ( 'NONE', #66966, #48101 ) ;
#38877 = CARTESIAN_POINT ( 'NONE',  ( -45.82429090095276791, 9.081512406228320344, -6.320717432316791395 ) ) ;
#38878 = EDGE_LOOP ( 'NONE', ( #65016, #3204, #35602, #13401, #52586, #69315 ) ) ;
#38879 = SURFACE_STYLE_USAGE ( .BOTH. , #49402 ) ;
#38880 = ORIENTED_EDGE ( 'NONE', *, *, #37783, .T. ) ;
#38881 = COLOUR_RGB ( '', 0.08235294, 0.09019608, 0.10196078) ;
#38883 = EDGE_CURVE ( 'NONE', #60509, #54981, #63469, .T. ) ;
#38882 = CARTESIAN_POINT ( 'NONE',  ( -75.00000000000000000, 7.768687147774684831, 7.000000000000004441 ) ) ;
#38884 = CARTESIAN_POINT ( 'NONE',  ( -112.8550000000000040, 4.716976649647094177, 6.492361379858945902 ) ) ;
#38885 = VERTEX_POINT ( 'NONE', #52926 ) ;
#38886 = DIRECTION ( 'NONE',  ( 0.000000000000000000, 0.000000000000000000, -1.000000000000000000 ) ) ;
#38887 = DIRECTION ( 'NONE',  ( -1.000000000000000000, 0.000000000000000000, 0.000000000000000000 ) ) ;
#38888 = DIRECTION ( 'NONE',  ( -0.000000000000000000, -0.000000000000000000, 1.000000000000000000 ) ) ;
#38889 = CARTESIAN_POINT ( 'NONE',  ( 30.25000000000001066, 16.24999999999997513, -3.750000000000000000 ) ) ;
#38890 = STYLED_ITEM ( 'NONE', ( #18357 ), #1791 ) ;
#38891 = FILL_AREA_STYLE ('',( #27905 ) ) ;
#38892 = CARTESIAN_POINT ( 'NONE',  ( -153.0570736234661808, 0.000000000000000000, 9.524999999999991473 ) ) ;
#38893 = ADVANCED_FACE ( 'NONE', ( #53602 ), #5062, .F. ) ;
#38894 = CARTESIAN_POINT ( 'NONE',  ( 3.094860106618435136, 133.2949999999999875, -9.525000000000000355 ) ) ;
#38895 = AXIS2_PLACEMENT_3D ( 'NONE', #39711, #61130, #55855 ) ;
#38896 = CARTESIAN_POINT ( 'NONE',  ( -86.75707362346616947, -5.598654528085801552, 7.705886871421367523 ) ) ;
#38897 = ADVANCED_FACE ( 'NONE', ( #69438 ), #5736, .T. ) ;
#38898 = CIRCLE ( 'NONE', #54563, 8.000000000000000000 ) ;
#38899 = CARTESIAN_POINT ( 'NONE',  ( -54.25530022753511616, -9.366146071587957422, -2.498496607514901768 ) ) ;
#38900 = ORIENTED_EDGE ( 'NONE', *, *, #21690, .T. ) ;
#38901 = FILL_AREA_STYLE ('',( #18780 ) ) ;
#38902 = DIRECTION ( 'NONE',  ( 0.000000000000000000, 0.000000000000000000, 1.000000000000000000 ) ) ;
#38903 = ADVANCED_FACE ( 'NONE', ( #45163 ), #39889, .T. ) ;
#38904 = CARTESIAN_POINT ( 'NONE',  ( -131.3050000000000068, 8.437984349512085203, -1.550032578732815448E-15 ) ) ;
#38905 = DIRECTION ( 'NONE',  ( 1.000000000000000000, -0.000000000000000000, 0.000000000000000000 ) ) ;
#38906 = CARTESIAN_POINT ( 'NONE',  ( 15.48999599679679662, 117.9999999999999716, 9.500000000000000000 ) ) ;
#38907 = CARTESIAN_POINT ( 'NONE',  ( -145.7950000000000443, 2.607480562269068880, -8.024999999999993250 ) ) ;
#38908 = CARTESIAN_POINT ( 'NONE',  ( -130.1949999999999932, 8.437984349512086979, -1.550032578732815448E-15 ) ) ;
#38909 = EDGE_LOOP ( 'NONE', ( #62356, #39012, #785, #33283 ) ) ;
#38910 = DIRECTION ( 'NONE',  ( 0.000000000000000000, 0.000000000000000000, 1.000000000000000000 ) ) ;
#38911 = CARTESIAN_POINT ( 'NONE',  ( 45.00320036294424852, 10.00106678764806567, -3.045234739864692397 ) ) ;
#38912 = SURFACE_SIDE_STYLE ('',( #65599 ) ) ;
#38913 = PLANE ( 'NONE',  #64230 ) ;
#38914 = UNCERTAINTY_MEASURE_WITH_UNIT (LENGTH_MEASURE( 1.000000000000000082E-05 ), #19441, 'distance_accuracy_value', 'NONE');
#38915 = CARTESIAN_POINT ( 'NONE',  ( -183.5929263765338249, -3.094860106618431139, -9.524999999999991473 ) ) ;
#38916 =( LENGTH_UNIT ( ) NAMED_UNIT ( * ) SI_UNIT ( .MILLI., .METRE. ) );
#38917 = CARTESIAN_POINT ( 'NONE',  ( -55.34499999999997755, 7.632228543268599452, -2.479861379858951942 ) ) ;
#38918 = CARTESIAN_POINT ( 'NONE',  ( -103.1070736234661638, 8.102448949553172852, -5.886773742842744461 ) ) ;
#38919 = FILL_AREA_STYLE_COLOUR ( '', #52292 ) ;
#38920 = AXIS2_PLACEMENT_3D ( 'NONE', #34240, #12768, #2521 ) ;
#38921 = CIRCLE ( 'NONE', #29889, 0.2500000000000002220 ) ;
#38922 = CIRCLE ( 'NONE', #20915, 1.000000000000000888 ) ;
#38923 = CARTESIAN_POINT ( 'NONE',  ( -75.50707362346616947, 8.102448949553176405, 5.886773742842740909 ) ) ;
#38924 = PRODUCT_DEFINITION_CONTEXT ( 'detailed design', #16811, 'design' ) ;
#38925 = CARTESIAN_POINT ( 'NONE',  ( -98.54292637653381348, 9.058813317711329915, 2.943386871421369566 ) ) ;
#38926 = APPLICATION_PROTOCOL_DEFINITION ( 'draft international standard', 'automotive_design', 1998, #16811 ) ;
#38927 = CARTESIAN_POINT ( 'NONE',  ( -53.22985755524383222, -10.31531486637975803, 2.417283891829344888 ) ) ;
#38928 = DIRECTION ( 'NONE',  ( -0.000000000000000000, -0.000000000000000000, -1.000000000000000000 ) ) ;
#38929 = SURFACE_SIDE_STYLE ('',( #44893 ) ) ;
#38930 = DIRECTION ( 'NONE',  ( -1.000000000000000000, 0.000000000000000000, 0.000000000000000000 ) ) ;
#38931 = SURFACE_SIDE_STYLE ('',( #48791 ) ) ;
#38932 = AXIS2_PLACEMENT_3D ( 'NONE', #55853, #7652, #57956 ) ;
#38933 = DIRECTION ( 'NONE',  ( 0.000000000000000000, 0.000000000000000000, 1.000000000000000000 ) ) ;
#38934 = VERTEX_POINT ( 'NONE', #65541 ) ;
#38935 = SURFACE_STYLE_FILL_AREA ( #13180 ) ;
#38936 = DIRECTION ( 'NONE',  ( 0.000000000000000000, 0.000000000000000000, 1.000000000000000000 ) ) ;
#38937 = ORIENTED_EDGE ( 'NONE', *, *, #8917, .T. ) ;
#38938 = DIRECTION ( 'NONE',  ( 0.000000000000000000, -1.000000000000000000, 0.000000000000000000 ) ) ;
#38940 = CARTESIAN_POINT ( 'NONE',  ( 8.437984349512095861, 126.3070736234661666, 1.550032578732817026E-15 ) ) ;
#38939 = AXIS2_PLACEMENT_3D ( 'NONE', #6799, #39548, #49734 ) ;
#38941 = SURFACE_SIDE_STYLE ('',( #12494 ) ) ;
#38942 = CARTESIAN_POINT ( 'NONE',  ( 74.65811388299935913, 19.88603796099976506, -6.065461639931112536 ) ) ;
#38943 = DIRECTION ( 'NONE',  ( -0.000000000000000000, -0.000000000000000000, -1.000000000000000000 ) ) ;
#38944 = VERTEX_POINT ( 'NONE', #12753 ) ;
#38945 = CARTESIAN_POINT ( 'NONE',  ( 53.24999999999999289, 27.99999999999998579, -3.750000000000000000 ) ) ;
#38946 =( LENGTH_UNIT ( ) NAMED_UNIT ( * ) SI_UNIT ( .MILLI., .METRE. ) );
#38947 = ORIENTED_EDGE ( 'NONE', *, *, #4351, .T. ) ;
#38948 = CARTESIAN_POINT ( 'NONE',  ( 34.99999999999999289, 99.99999999999998579, 7.000000000000000000 ) ) ;
#38949 = CARTESIAN_POINT ( 'NONE',  ( -94.10707362346614957, 8.102448949553172852, -5.886773742842744461 ) ) ;
#38950 = EDGE_CURVE ( 'NONE', #29016, #8709, #17476, .T. ) ;
#38951 = CARTESIAN_POINT ( 'NONE',  ( -95.09499999999999886, -2.607480562269071545, -8.024999999999991473 ) ) ;
#38952 = ORIENTED_EDGE ( 'NONE', *, *, #21926, .F. ) ;
#38953 = ADVANCED_FACE ( 'NONE', ( #39530 ), #49721, .T. ) ;
#38954 = DIRECTION ( 'NONE',  ( 0.000000000000000000, 0.4705882352941173075, 0.8823529411764708952 ) ) ;
#38955 = EDGE_CURVE ( 'NONE', #31454, #55156, #7313, .T. ) ;
#38956 = FACE_OUTER_BOUND ( 'NONE', #14185, .T. ) ;
#38957 = SURFACE_STYLE_USAGE ( .BOTH. , #17488 ) ;
#38958 = UNCERTAINTY_MEASURE_WITH_UNIT (LENGTH_MEASURE( 1.000000000000000082E-05 ), #32581, 'distance_accuracy_value', 'NONE');
#38959 = ORIENTED_EDGE ( 'NONE', *, *, #12983, .F. ) ;
#38960 = CARTESIAN_POINT ( 'NONE',  ( -4.716976649647098618, 160.1429263765338362, 6.492361379858953008 ) ) ;
#38961 =( NAMED_UNIT ( * ) SI_UNIT ( $, .STERADIAN. ) SOLID_ANGLE_UNIT ( ) );
#38962 = ADVANCED_FACE ( 'NONE', ( #1459 ), #2505, .F. ) ;
#38963 = VECTOR ( 'NONE', #2629, 1000.000000000000000 ) ;
#38964 =( LENGTH_UNIT ( ) NAMED_UNIT ( * ) SI_UNIT ( .MILLI., .METRE. ) );
#38965 = ADVANCED_FACE ( 'NONE', ( #57061 ), #67624, .F. ) ;
#38966 = VERTEX_POINT ( 'NONE', #30299 ) ;
#38967 = VECTOR ( 'NONE', #35798, 1000.000000000000000 ) ;
#38968 = SURFACE_SIDE_STYLE ('',( #43898 ) ) ;
#38969 = EDGE_CURVE ( 'NONE', #8380, #31530, #41271, .T. ) ;
#38970 = ORIENTED_EDGE ( 'NONE', *, *, #39501, .F. ) ;
#38971 = CARTESIAN_POINT ( 'NONE',  ( -137.3929263765337794, 8.102448949553176405, 5.886773742842740909 ) ) ;
#38972 = MECHANICAL_DESIGN_GEOMETRIC_PRESENTATION_REPRESENTATION (  '', ( #63629 ), #62512 ) ;
#38973 = PRESENTATION_STYLE_ASSIGNMENT (( #65656 ) ) ;
#38974 =( NAMED_UNIT ( * ) SI_UNIT ( $, .STERADIAN. ) SOLID_ANGLE_UNIT ( ) );
#38975 = CARTESIAN_POINT ( 'NONE',  ( -180.2070736234661865, 3.094860106618433360, 9.524999999999991473 ) ) ;
#38976 = ADVANCED_FACE ( 'NONE', ( #46566 ), #66942, .T. ) ;
#38977 = DIRECTION ( 'NONE',  ( 0.000000000000000000, 0.000000000000000000, 1.000000000000000000 ) ) ;
#38978 = FILL_AREA_STYLE ('',( #27653 ) ) ;
#38979 = CARTESIAN_POINT ( 'NONE',  ( -1.136396319700226032, 9.000000000000010658, 0.06877762208650195497 ) ) ;
#38980 = EDGE_CURVE ( 'NONE', #29123, #54714, #51161, .T. ) ;
#38981 = CARTESIAN_POINT ( 'NONE',  ( -115.6429263765338078, -5.598654528085801552, 7.705886871421367523 ) ) ;
#38982 = VERTEX_POINT ( 'NONE', #67990 ) ;
#38983 = CARTESIAN_POINT ( 'NONE',  ( 34.99999999999992895, 109.9999999999999858, 10.00000000000000000 ) ) ;
#38984 = CARTESIAN_POINT ( 'NONE',  ( 0.000000000000000000, 24.74999999999998579, 4.000000000000000000 ) ) ;
#38985 = CARTESIAN_POINT ( 'NONE',  ( 23.50000000000001776, 15.00000000000000000, -29.68999999999999417 ) ) ;
#38986 = CARTESIAN_POINT ( 'NONE',  ( 68.99999999999998579, 1.000000000000008438, -3.000000000000000000 ) ) ;
#38988 = VERTEX_POINT ( 'NONE', #24682 ) ;
#38987 = CIRCLE ( 'NONE', #43472, 8.025000000000000355 ) ;
#38989 = CARTESIAN_POINT ( 'NONE',  ( -161.9050000000000011, 2.607480562269068880, -8.024999999999993250 ) ) ;
#38990 =( LENGTH_UNIT ( ) NAMED_UNIT ( * ) SI_UNIT ( .MILLI., .METRE. ) );
#38991 = CARTESIAN_POINT ( 'NONE',  ( -183.5761998908936619, -4.982236208952005363, -7.440177628705773927 ) ) ;
#38992 = CARTESIAN_POINT ( 'NONE',  ( -169.4949999999999761, 6.826472737025113702, -4.959722759717902107 ) ) ;
#38993 = CARTESIAN_POINT ( 'NONE',  ( -154.4949999999999477, 6.826472737025113702, -4.959722759717902107 ) ) ;
#38994 = EDGE_LOOP ( 'NONE', ( #35380, #68939 ) ) ;
#38995 = CARTESIAN_POINT ( 'NONE',  ( 8.000000000000024869, 0.000000000000000000, 32.00402776293825724 ) ) ;
#38996 = DIRECTION ( 'NONE',  ( 1.000000000000000000, 0.000000000000000000, -0.000000000000000000 ) ) ;
#38997 = CARTESIAN_POINT ( 'NONE',  ( -73.25499999999998124, -4.716976649647092401, 6.492361379858946790 ) ) ;
#38998 = CARTESIAN_POINT ( 'NONE',  ( -35.59516224449775024, -11.38366882999885554, 1.750067940178240411 ) ) ;
#39000 = VECTOR ( 'NONE', #16022, 1000.000000000000000 ) ;
#38999 = DIRECTION ( 'NONE',  ( 0.000000000000000000, 1.000000000000000000, 1.734723475976805615E-16 ) ) ;
#39001 = CARTESIAN_POINT ( 'NONE',  ( -71.69499999999997897, -8.437984349512086979, 5.166775262442717831E-16 ) ) ;
#39002 = CARTESIAN_POINT ( 'NONE',  ( -3.094860106618434248, 147.9049999999999727, 9.525000000000000355 ) ) ;
#39003 = CARTESIAN_POINT ( 'NONE',  ( -12.74999999999999822, -3.000000000000000000, 7.000000000000001776 ) ) ;
#39004 = CARTESIAN_POINT ( 'NONE',  ( 22.99999999999999289, 5.000000000000000000, -37.00402776293825013 ) ) ;
#39005 = UNCERTAINTY_MEASURE_WITH_UNIT (LENGTH_MEASURE( 1.000000000000000082E-05 ), #29073, 'distance_accuracy_value', 'NONE');
#39006 = B_SPLINE_CURVE_WITH_KNOTS ( 'NONE', 3,
 ( #68884, #31205, #57263, #37248, #52700, #68186, #19964, #58307, #20684, #14719, #10131, #57624 ),
 .UNSPECIFIED., .F., .F.,
 ( 4, 2, 2, 2, 2, 4 ),
 ( 0.000000000000000000, 0.0001178293706450991933, 0.0002356587412901983865, 0.0004713174825804007304, 0.0009426349651608007018, 0.001885269930321605523 ),
 .UNSPECIFIED. ) ;
#39007 = EDGE_CURVE ( 'NONE', #59162, #23616, #51803, .T. ) ;
#39008 = CARTESIAN_POINT ( 'NONE',  ( -195.0000000000000000, 0.000000000000000000, 9.524999999999991473 ) ) ;
#39009 = ORIENTED_EDGE ( 'NONE', *, *, #34880, .F. ) ;
#39010 = VECTOR ( 'NONE', #57722, 1000.000000000000114 ) ;
#39011 = DIRECTION ( 'NONE',  ( -0.000000000000000000, -0.000000000000000000, -1.000000000000000000 ) ) ;
#39012 = ORIENTED_EDGE ( 'NONE', *, *, #55012, .T. ) ;
#39013 = ORIENTED_EDGE ( 'NONE', *, *, #4094, .T. ) ;
#39014 = CARTESIAN_POINT ( 'NONE',  ( -4.716976649647098618, 136.1429263765338362, 6.492361379858953008 ) ) ;
#39015 = DIRECTION ( 'NONE',  ( 1.000000000000000000, 0.000000000000000000, 0.000000000000000000 ) ) ;
#39016 = CARTESIAN_POINT ( 'NONE',  ( 3.109477999331723641, 1.987149502472171703, 9.000000000000001776 ) ) ;
#39017 = CARTESIAN_POINT ( 'NONE',  ( -41.84210526315788314, 107.2928455055531600, 4.000000000000000000 ) ) ;
#39018 = EDGE_LOOP ( 'NONE', ( #30199, #63798, #64608, #47703 ) ) ;
#39019 = CARTESIAN_POINT ( 'NONE',  ( -114.9549999999999841, -7.632228543268599452, 2.479861379858951054 ) ) ;
#39020 = ORIENTED_EDGE ( 'NONE', *, *, #26451, .F. ) ;
#39021 = SURFACE_STYLE_FILL_AREA ( #32653 ) ;
#39022 =( GEOMETRIC_REPRESENTATION_CONTEXT ( 3 ) GLOBAL_UNCERTAINTY_ASSIGNED_CONTEXT ( ( #36275 ) ) GLOBAL_UNIT_ASSIGNED_CONTEXT ( ( #14419, #35892, #13379 ) ) REPRESENTATION_CONTEXT ( 'NONE', 'WORKASPACE' ) );
#39023 = EDGE_CURVE ( 'NONE', #63887, #9536, #34276, .T. ) ;
#39024 = ORIENTED_EDGE ( 'NONE', *, *, #25712, .F. ) ;
#39025 = CARTESIAN_POINT ( 'NONE',  ( -56.54292637653379927, 9.058813317711329915, 2.943386871421369566 ) ) ;
#39026 = CARTESIAN_POINT ( 'NONE',  ( 44.00000000000000000, 21.99999999999998579, 3.750000000000000000 ) ) ;
#39027 = ORIENTED_EDGE ( 'NONE', *, *, #27918, .T. ) ;
#39028 = FILL_AREA_STYLE_COLOUR ( '', #41147 ) ;
#39029 = FILL_AREA_STYLE_COLOUR ( '', #46284 ) ;
#39030 = PLANE ( 'NONE',  #1380 ) ;
#39031 = ORIENTED_EDGE ( 'NONE', *, *, #60241, .F. ) ;
#39032 = EDGE_CURVE ( 'NONE', #7249, #38874, #40923, .T. ) ;
#39033 = ORIENTED_EDGE ( 'NONE', *, *, #15385, .F. ) ;
#39034 = CARTESIAN_POINT ( 'NONE',  ( -8.091123032493692691, 110.4999999999999858, -5.044978548556969145 ) ) ;
#39035 = FILL_AREA_STYLE ('',( #17570 ) ) ;
#39036 = CARTESIAN_POINT ( 'NONE',  ( -152.1570736234661751, -9.058813317711329915, -2.943386871421370898 ) ) ;
#39037 = CARTESIAN_POINT ( 'NONE',  ( 0.000000000000000000, 42.00000000000000000, 74.38749456993816978 ) ) ;
#39038 = ORIENTED_EDGE ( 'NONE', *, *, #15018, .F. ) ;
#39039 = CARTESIAN_POINT ( 'NONE',  ( -4.716976649647097730, 135.2429263765338305, -6.492361379858953896 ) ) ;
#39040 = FACE_OUTER_BOUND ( 'NONE', #47790, .T. ) ;
#39041 = DIRECTION ( 'NONE',  ( -0.000000000000000000, -1.000000000000000000, -0.000000000000000000 ) ) ;
#39042 = CARTESIAN_POINT ( 'NONE',  ( -105.1429263765338078, 5.598654528085800663, -7.705886871421367523 ) ) ;
#39043 = LINE ( 'NONE', #33384, #45616 ) ;
#39044 = ORIENTED_EDGE ( 'NONE', *, *, #37876, .T. ) ;
#39045 = CARTESIAN_POINT ( 'NONE',  ( -11.24540022918535698, 52.49282396394303873, 2.000000000000000000 ) ) ;
#39046 = EDGE_CURVE ( 'NONE', #38153, #36170, #45524, .T. ) ;
#39047 = ORIENTED_EDGE ( 'NONE', *, *, #42157, .T. ) ;
#39048 = CARTESIAN_POINT ( 'NONE',  ( -49.04292637653379217, -9.058813317711329915, -2.943386871421370898 ) ) ;
#39049 = SURFACE_SIDE_STYLE ('',( #29110 ) ) ;
#39050 =( NAMED_UNIT ( * ) PLANE_ANGLE_UNIT ( ) SI_UNIT ( $, .RADIAN. ) );
#39051 = FILL_AREA_STYLE ('',( #11236 ) ) ;
#39052 = CARTESIAN_POINT ( 'NONE',  ( -130.4050000000000011, -2.607480562269069768, 8.024999999999991473 ) ) ;
#39053 = FILL_AREA_STYLE_COLOUR ( '', #45503 ) ;
#39054 = CYLINDRICAL_SURFACE ( 'NONE', #1248, 1.000000000000000888 ) ;
#39055 = ORIENTED_EDGE ( 'NONE', *, *, #57111, .T. ) ;
#39056 = DIRECTION ( 'NONE',  ( 1.000000000000000000, 0.000000000000000000, 0.000000000000000000 ) ) ;
#39057 = EDGE_CURVE ( 'NONE', #20853, #4364, #46205, .T. ) ;
#39058 = CARTESIAN_POINT ( 'NONE',  ( -106.7070736234671244, -3.094860106634161667, -9.524999999988564170 ) ) ;
#39059 = FILL_AREA_STYLE_COLOUR ( '', #34811 ) ;
#39060 = EDGE_LOOP ( 'NONE', ( #65301, #57669, #41517, #32265 ) ) ;
#39061 = AXIS2_PLACEMENT_3D ( 'NONE', #21341, #66334, #11834 ) ;
#39062 = ORIENTED_EDGE ( 'NONE', *, *, #62983, .F. ) ;
#39063 = CARTESIAN_POINT ( 'NONE',  ( -45.21668476452690300, 8.382617247417337936, 3.141345821310664643 ) ) ;
#39064 =( NAMED_UNIT ( * ) PLANE_ANGLE_UNIT ( ) SI_UNIT ( $, .RADIAN. ) );
#39065 = CARTESIAN_POINT ( 'NONE',  ( -58.25499999999997414, -4.716976649647092401, 6.492361379858946790 ) ) ;
#39066 = VERTEX_POINT ( 'NONE', #46914 ) ;
#39067 = DIRECTION ( 'NONE',  ( 0.000000000000000000, 0.000000000000000000, 1.000000000000000000 ) ) ;
#39068 = FACE_OUTER_BOUND ( 'NONE', #12216, .T. ) ;
#39070 = AXIS2_PLACEMENT_3D ( 'NONE', #54485, #11234, #53790 ) ;
#39069 = DIRECTION ( 'NONE',  ( -0.000000000000000000, -0.000000000000000000, -1.000000000000000000 ) ) ;
#39071 = CARTESIAN_POINT ( 'NONE',  ( 3.409623619629272184, 7.000000000000006217, 0.7804846576204730324 ) ) ;
#39072 = CARTESIAN_POINT ( 'NONE',  ( -183.4449999999999932, 0.000000000000000000, 8.024999999999991473 ) ) ;
#39073 = CARTESIAN_POINT ( 'NONE',  ( -52.24999999999999289, 4.336808689942018722E-16, 0.000000000000000000 ) ) ;
#39074 = ORIENTED_EDGE ( 'NONE', *, *, #57553, .T. ) ;
#39075 = FILL_AREA_STYLE_COLOUR ( '', #33815 ) ;
#39076 = CARTESIAN_POINT ( 'NONE',  ( -26.79538245034556709, -7.499999999999997335, 0.000000000000000000 ) ) ;
#39077 = DIRECTION ( 'NONE',  ( -0.000000000000000000, -0.000000000000000000, 1.000000000000000000 ) ) ;
#39078 = MECHANICAL_DESIGN_GEOMETRIC_PRESENTATION_REPRESENTATION (  '', ( #21059 ), #54726 ) ;
#39079 = VECTOR ( 'NONE', #28057, 1000.000000000000000 ) ;
#39080 = CARTESIAN_POINT ( 'NONE',  ( -96.89499999999998181, 6.826472737025115478, 4.959722759717899443 ) ) ;
#39081 = CARTESIAN_POINT ( 'NONE',  ( 10.01517768586949231, 156.6949999999999932, 1.839758294383810543E-15 ) ) ;
#39082 = CARTESIAN_POINT ( 'NONE',  ( -77.69499999999999318, -8.437984349512085203, 5.166775262442717831E-16 ) ) ;
#39083 = CARTESIAN_POINT ( 'NONE',  ( 0.000000000000000000, 112.0570736234661666, -8.025000000000000355 ) ) ;
#39084 = CARTESIAN_POINT ( 'NONE',  ( -7.632228543268607446, 141.5429263765338135, -2.479861379858953718 ) ) ;
#39085 = CARTESIAN_POINT ( 'NONE',  ( 71.50000000000000000, 35.92875272052971525, -7.000000000000000000 ) ) ;
#39086 = CARTESIAN_POINT ( 'NONE',  ( 3.000000000000030198, 43.00000000000000000, 90.00000000000000000 ) ) ;
#39087 = UNCERTAINTY_MEASURE_WITH_UNIT (LENGTH_MEASURE( 1.000000000000000082E-05 ), #68008, 'distance_accuracy_value', 'NONE');
#39088 = EDGE_CURVE ( 'NONE', #42646, #44927, #60134, .T. ) ;
#39089 = DIRECTION ( 'NONE',  ( -0.000000000000000000, -0.000000000000000000, -1.000000000000000000 ) ) ;
#39090 = DIRECTION ( 'NONE',  ( -0.000000000000000000, -0.000000000000000000, -1.000000000000000000 ) ) ;
#39091 = VERTEX_POINT ( 'NONE', #41609 ) ;
#39092 = CARTESIAN_POINT ( 'NONE',  ( -126.8929263765338220, -8.102448949553172852, -5.886773742842741797 ) ) ;
#39093 =( LENGTH_UNIT ( ) NAMED_UNIT ( * ) SI_UNIT ( .MILLI., .METRE. ) );
#39094 = CARTESIAN_POINT ( 'NONE',  ( -139.6449999999999818, 4.716976649647091513, -6.492361379858946790 ) ) ;
#39095 = FILL_AREA_STYLE_COLOUR ( '', #49370 ) ;
#39096 = SURFACE_STYLE_USAGE ( .BOTH. , #56261 ) ;
#39097 = SURFACE_STYLE_USAGE ( .BOTH. , #18306 ) ;
#39098 = ORIENTED_EDGE ( 'NONE', *, *, #18808, .T. ) ;
#39099 = ORIENTED_EDGE ( 'NONE', *, *, #28292, .T. ) ;
#39100 = CARTESIAN_POINT ( 'NONE',  ( -22.50000000000000711, 37.00000000000000000, 3.750000000000000000 ) ) ;
#39101 = VECTOR ( 'NONE', #19741, 1000.000000000000000 ) ;
#39102 = SURFACE_STYLE_USAGE ( .BOTH. , #55586 ) ;
#39103 = CARTESIAN_POINT ( 'NONE',  ( -132.0570736234661808, 0.000000000000000000, 9.524999999999991473 ) ) ;
#39104 = STYLED_ITEM ( 'NONE', ( #17412 ), #50731 ) ;
#39105 = CARTESIAN_POINT ( 'NONE',  ( -50.45707362346615810, -9.058813317711329915, 2.943386871421371787 ) ) ;
#39106 = AXIS2_PLACEMENT_3D ( 'NONE', #2980, #24468, #58236 ) ;
#39107 = ORIENTED_EDGE ( 'NONE', *, *, #10012, .F. ) ;
#39108 = CARTESIAN_POINT ( 'NONE',  ( -139.8550000000000182, 4.716976649647094177, 6.492361379858945902 ) ) ;
#39110 = EDGE_CURVE ( 'NONE', #69641, #47699, #52168, .T. ) ;
#39109 = ORIENTED_EDGE ( 'NONE', *, *, #32023, .T. ) ;
#39111 = EDGE_CURVE ( 'NONE', #6562, #20313, #37746, .T. ) ;
#39112 = ORIENTED_EDGE ( 'NONE', *, *, #59363, .F. ) ;
#39113 = CARTESIAN_POINT ( 'NONE',  ( -4.000000000000000000, 4.336808689942018722E-16, 24.00000000000000000 ) ) ;
#39114 = ORIENTED_EDGE ( 'NONE', *, *, #22888, .T. ) ;
#39115 = PRODUCT_DEFINITION_SHAPE ( 'NONE', 'NONE',  #69708 ) ;
#39116 = CARTESIAN_POINT ( 'NONE',  ( -1.585182400056157181, 2.380245935246553035, -9.000000000000005329 ) ) ;
#39117 =( LENGTH_UNIT ( ) NAMED_UNIT ( * ) SI_UNIT ( .MILLI., .METRE. ) );
#39118 = CARTESIAN_POINT ( 'NONE',  ( -9.058813317711337021, 131.0449999999999875, -2.943386871421374895 ) ) ;
#39119 = PRESENTATION_STYLE_ASSIGNMENT (( #33791 ) ) ;
#39120 = VERTEX_POINT ( 'NONE', #51443 ) ;
#39122 = ADVANCED_FACE ( 'NONE', ( #57775 ), #35625, .T. ) ;
#39121 = CARTESIAN_POINT ( 'NONE',  ( 3.094860106618435136, 128.4049999999999727, -9.525000000000000355 ) ) ;
#39123 = CARTESIAN_POINT ( 'NONE',  ( -59.15499999999998693, 7.632228543268600340, 2.479861379858949277 ) ) ;
#39124 = CARTESIAN_POINT ( 'NONE',  ( 41.01786561352940907, 107.7208547478738012, -3.150777047984585799 ) ) ;
#39125 = VERTEX_POINT ( 'NONE', #64065 ) ;
#39126 = CARTESIAN_POINT ( 'NONE',  ( -10.01517768586949231, 156.3049999999999500, -6.132527647946036459E-16 ) ) ;
#39127 = DIRECTION ( 'NONE',  ( -0.000000000000000000, 1.000000000000000000, -0.000000000000000000 ) ) ;
#39128 = UNCERTAINTY_MEASURE_WITH_UNIT (LENGTH_MEASURE( 1.000000000000000082E-05 ), #54976, 'distance_accuracy_value', 'NONE');
#39129 = AXIS2_PLACEMENT_3D ( 'NONE', #15296, #52225, #30719 ) ;
#39130 = CARTESIAN_POINT ( 'NONE',  ( -88.94292637653380496, 0.000000000000000000, 9.524999999999991473 ) ) ;
#39131 = EDGE_CURVE ( 'NONE', #2564, #58449, #23388, .T. ) ;
#39132 = CARTESIAN_POINT ( 'NONE',  ( 4.750000000000000000, 5.817072295949927426E-16, 0.7500000000000000000 ) ) ;
#39133 = ORIENTED_EDGE ( 'NONE', *, *, #15739, .T. ) ;
#39134 = DIRECTION ( 'NONE',  ( -0.000000000000000000, -0.000000000000000000, 1.000000000000000000 ) ) ;
#39135 = EDGE_CURVE ( 'NONE', #60144, #10312, #65760, .T. ) ;
#39136 = VERTEX_POINT ( 'NONE', #16611 ) ;
#39137 = DIRECTION ( 'NONE',  ( -2.312964634635740689E-15, 1.000000000000000000, 0.000000000000000000 ) ) ;
#39138 = PRESENTATION_STYLE_ASSIGNMENT (( #60883 ) ) ;
#39139 = CARTESIAN_POINT ( 'NONE',  ( -173.6049999999999898, 6.826472737025113702, -4.959722759717902107 ) ) ;
#39140 = ORIENTED_EDGE ( 'NONE', *, *, #69644, .F. ) ;
#39141 = CARTESIAN_POINT ( 'NONE',  ( 61.99999999999998579, 33.74999999999999289, 3.750000000000000000 ) ) ;
#39142 = UNCERTAINTY_MEASURE_WITH_UNIT (LENGTH_MEASURE( 1.000000000000000082E-05 ), #22990, 'distance_accuracy_value', 'NONE');
#39143 = FILL_AREA_STYLE_COLOUR ( '', #41888 ) ;
#39144 = ADVANCED_FACE ( 'NONE', ( #15919 ), #38073, .F. ) ;
#39145 = DIRECTION ( 'NONE',  ( -1.000000000000000000, 0.000000000000000000, 0.000000000000000000 ) ) ;
#39146 = LINE ( 'NONE', #60535, #20882 ) ;
#39147 = ORIENTED_EDGE ( 'NONE', *, *, #67762, .F. ) ;
#39148 = ORIENTED_EDGE ( 'NONE', *, *, #62968, .T. ) ;
#39149 = CARTESIAN_POINT ( 'NONE',  ( -45.00000000000000000, 9.708372675170616972, -3.611004237778681958 ) ) ;
#39150 = CARTESIAN_POINT ( 'NONE',  ( -5.196152422706636465, 1.107695154586737063, 9.000000000000001776 ) ) ;
#39151 = CARTESIAN_POINT ( 'NONE',  ( -84.05499999999999261, -9.827790563157499189E-16, -8.024999999999991473 ) ) ;
#39152 = ORIENTED_EDGE ( 'NONE', *, *, #24941, .T. ) ;
#39153 =( BOUNDED_CURVE ( )  B_SPLINE_CURVE ( 2, ( #2700, #24193, #45699, #46393, #9077, #19249, #67452, #36175, #25570, #40753, #62517 ),
 .UNSPECIFIED., .F., .F. ) 
 B_SPLINE_CURVE_WITH_KNOTS ( ( 3, 2, 2, 2, 2, 3 ),
 ( 0.02173913043478211890, 0.02391304347826033252, 0.02608695652173854268, 0.02826086956521675284, 0.03043478260869496993, 0.03260869565217317662 ),
 .UNSPECIFIED. ) 
 CURVE ( )  GEOMETRIC_REPRESENTATION_ITEM ( )  RATIONAL_B_SPLINE_CURVE ( ( 1.000000000000010880, 0.9510565162951424290, 1.000000000000000000, 0.9510565162951535312, 1.000000000000000000, 0.9510565162951535312, 1.000000000000000000, 0.9510565162951535312, 1.000000000000000000, 0.9510565162951700735, 0.9999999999999834577 ) ) 
 REPRESENTATION_ITEM ( '' )  );
#39154 = FILL_AREA_STYLE_COLOUR ( '', #13964 ) ;
#39155 = CARTESIAN_POINT ( 'NONE',  ( -75.00000000000000000, 8.537325437491082525, -6.129378421684882561 ) ) ;
#39156 = ORIENTED_EDGE ( 'NONE', *, *, #52042, .T. ) ;
#39157 = CARTESIAN_POINT ( 'NONE',  ( 20.71231517720798010, 149.9999999999999716, -10.00000000000000000 ) ) ;
#39158 = CONICAL_SURFACE ( 'NONE', #57090, 8.025000000000000355, 0.7853981633974491672 ) ;
#39159 = PLANE ( 'NONE',  #15643 ) ;
#39160 = CIRCLE ( 'NONE', #23347, 5.500000000000005329 ) ;
#39161 = CARTESIAN_POINT ( 'NONE',  ( -9.058813317711338797, 125.3449999999999847, 2.943386871421373563 ) ) ;
#39162 = CARTESIAN_POINT ( 'NONE',  ( -109.3449999999999847, 7.632228543268599452, -2.479861379858951942 ) ) ;
#39163 = LINE ( 'NONE', #34533, #61760 ) ;
#39164 = STYLED_ITEM ( 'NONE', ( #35893 ), #655 ) ;
#39165 = EDGE_CURVE ( 'NONE', #42774, #52109, #36592, .T. ) ;
#39166 = LINE ( 'NONE', #38829, #13253 ) ;
#39167 = CARTESIAN_POINT ( 'NONE',  ( -157.3429263765337964, -9.058813317711329915, 2.943386871421371787 ) ) ;
#39168 = CARTESIAN_POINT ( 'NONE',  ( -164.2450000000000045, -4.716976649647093289, -6.492361379858945902 ) ) ;
#39169 = AXIS2_PLACEMENT_3D ( 'NONE', #21118, #38031, #44008 ) ;
#39170 = SPHERICAL_SURFACE ( 'NONE', #27582, 0.2500000000000000000 ) ;
#39171 = CARTESIAN_POINT ( 'NONE',  ( -41.74159630588923875, -12.05724898635192233, 3.212438452487503149 ) ) ;
#39172 = ORIENTED_EDGE ( 'NONE', *, *, #50296, .F. ) ;
#39173 = DIRECTION ( 'NONE',  ( 1.000000000000000000, 0.000000000000000000, 0.000000000000000000 ) ) ;
#39174 = ORIENTED_EDGE ( 'NONE', *, *, #52752, .F. ) ;
#39175 = CARTESIAN_POINT ( 'NONE',  ( -64.19292637653380496, -10.01517768586948698, 6.132527647946031529E-16 ) ) ;
#39176 = DIRECTION ( 'NONE',  ( 0.000000000000000000, 0.000000000000000000, -1.000000000000000000 ) ) ;
#39177 = DIRECTION ( 'NONE',  ( -0.000000000000000000, -0.000000000000000000, -1.000000000000000000 ) ) ;
#39178 = EDGE_CURVE ( 'NONE', #17013, #11331, #32389, .T. ) ;
#39179 = FACE_OUTER_BOUND ( 'NONE', #1476, .T. ) ;
#39180 = CARTESIAN_POINT ( 'NONE',  ( -83.49999999999998579, 4.336808689942018722E-16, -0.000000000000000000 ) ) ;
#39181 = ADVANCED_FACE ( 'NONE', ( #69364 ), #7370, .T. ) ;
#39182 = DIRECTION ( 'NONE',  ( -0.000000000000000000, -0.000000000000000000, -1.000000000000000000 ) ) ;
#39183 = AXIS2_PLACEMENT_3D ( 'NONE', #36197, #30876, #63919 ) ;
#39184 = ORIENTED_EDGE ( 'NONE', *, *, #26275, .T. ) ;
#39185 = CARTESIAN_POINT ( 'NONE',  ( -168.9549999999999841, -7.632228543268599452, 2.479861379858951054 ) ) ;
#39186 = EDGE_CURVE ( 'NONE', #35021, #9250, #337, .T. ) ;
#39187 = EDGE_CURVE ( 'NONE', #54390, #42335, #10618, .T. ) ;
#39188 = ORIENTED_EDGE ( 'NONE', *, *, #34871, .T. ) ;
#39189 = LINE ( 'NONE', #22279, #38198 ) ;
#39190 = CARTESIAN_POINT ( 'NONE',  ( 179.4361977533490347, 0.9999999999999991118, 103.7004518695263044 ) ) ;
#39191 = VECTOR ( 'NONE', #8876, 1000.000000000000000 ) ;
#39192 = DIRECTION ( 'NONE',  ( 1.000000000000000000, -4.336808689941999001E-16, 0.000000000000000000 ) ) ;
#39193 = CARTESIAN_POINT ( 'NONE',  ( 6.826472737025119919, 156.0070736234661695, 4.959722759717908325 ) ) ;
#39194 = AXIS2_PLACEMENT_3D ( 'NONE', #22060, #43564, #49158 ) ;
#39195 = EDGE_LOOP ( 'NONE', ( #19868, #68245, #19363, #67610 ) ) ;
#39196 = CARTESIAN_POINT ( 'NONE',  ( -84.95499999999998408, -7.632228543268599452, 2.479861379858951054 ) ) ;
#39197 = CARTESIAN_POINT ( 'NONE',  ( 3.094860106618435136, 125.4050000000000011, -9.525000000000000355 ) ) ;
#39198 = UNCERTAINTY_MEASURE_WITH_UNIT (LENGTH_MEASURE( 1.000000000000000082E-05 ), #5256, 'distance_accuracy_value', 'NONE');
#39199 = STYLED_ITEM ( 'NONE', ( #9581 ), #51228 ) ;
#39200 = STYLED_ITEM ( 'NONE', ( #788 ), #66391 ) ;
#39201 = CARTESIAN_POINT ( 'NONE',  ( 13.25000000000000355, 27.99999999999998934, -4.000000000000000000 ) ) ;
#39202 = ADVANCED_FACE ( 'NONE', ( #21154 ), #2051, .F. ) ;
#39203 = DIRECTION ( 'NONE',  ( 1.000000000000000000, -1.084202172485504434E-16, -0.000000000000000000 ) ) ;
#39204 = VERTEX_POINT ( 'NONE', #69021 ) ;
#39205 = CIRCLE ( 'NONE', #48202, 0.5000000000000004441 ) ;
#39206 = DIRECTION ( 'NONE',  ( 0.000000000000000000, 0.000000000000000000, 1.000000000000000000 ) ) ;
#39207 = DIRECTION ( 'NONE',  ( -0.000000000000000000, -1.000000000000000000, 0.000000000000000000 ) ) ;
#39208 = CARTESIAN_POINT ( 'NONE',  ( -58.34499999999997755, 7.632228543268599452, -2.479861379858951942 ) ) ;
#39209 = ORIENTED_EDGE ( 'NONE', *, *, #17180, .F. ) ;
#39210 = FACE_OUTER_BOUND ( 'NONE', #8716, .T. ) ;
#39211 = CARTESIAN_POINT ( 'NONE',  ( -138.8070736234661524, 10.01517768586948698, -1.839758294383808966E-15 ) ) ;
#39212 = ORIENTED_EDGE ( 'NONE', *, *, #42803, .T. ) ;
#39213 = CARTESIAN_POINT ( 'NONE',  ( -52.19864025407932928, -11.16676068567596047, 1.871793189971100668 ) ) ;
#39214 = CARTESIAN_POINT ( 'NONE',  ( -56.69499999999998607, -8.437984349512086979, 5.166775262442717831E-16 ) ) ;
#39215 = FILL_AREA_STYLE ('',( #17745 ) ) ;
#39216 = ORIENTED_EDGE ( 'NONE', *, *, #55269, .F. ) ;
#39217 = AXIS2_PLACEMENT_3D ( 'NONE', #14031, #19646, #68538 ) ;
#39218 = CARTESIAN_POINT ( 'NONE',  ( -4.041451884327381450, 7.000000000000006217, 7.500000000000000000 ) ) ;
#39219 = CARTESIAN_POINT ( 'NONE',  ( -109.7049999999999699, 2.607480562269073321, 8.024999999999991473 ) ) ;
#39220 = ORIENTED_EDGE ( 'NONE', *, *, #49042, .T. ) ;
#39221 = ADVANCED_FACE ( 'NONE', ( #49639 ), #45090, .T. ) ;
#39222 = CARTESIAN_POINT ( 'NONE',  ( 20.12916642283592950, 109.9999999999999858, -10.05319148936170137 ) ) ;
#39223 = LINE ( 'NONE', #5417, #54358 ) ;
#39224 = DIRECTION ( 'NONE',  ( -0.000000000000000000, -0.000000000000000000, -1.000000000000000000 ) ) ;
#39225 = LINE ( 'NONE', #54998, #24084 ) ;
#39226 = CARTESIAN_POINT ( 'NONE',  ( -40.49999999999998579, 107.7459666924148394, 10.00000000000000000 ) ) ;
#39227 = CARTESIAN_POINT ( 'NONE',  ( -151.7070736234662149, -3.094860106618431139, -9.524999999999991473 ) ) ;
#39228 = EDGE_CURVE ( 'NONE', #46742, #34097, #68083, .T. ) ;
#39229 = DIRECTION ( 'NONE',  ( 1.000000000000000000, -0.000000000000000000, -1.300977106640434891E-16 ) ) ;
#39230 = CARTESIAN_POINT ( 'NONE',  ( -9.058813317711337021, 128.0449999999999875, -2.943386871421374895 ) ) ;
#39231 = CARTESIAN_POINT ( 'NONE',  ( -81.95707362346617231, 9.058813317711329915, -2.943386871421373119 ) ) ;
#39232 = MECHANICAL_DESIGN_GEOMETRIC_PRESENTATION_REPRESENTATION (  '', ( #7753 ), #68424 ) ;
#39233 = DIRECTION ( 'NONE',  ( 1.073081856240828566E-16, -1.000000000000000000, 0.000000000000000000 ) ) ;
#39234 = ORIENTED_EDGE ( 'NONE', *, *, #4593, .F. ) ;
#39235 = DIRECTION ( 'NONE',  ( -1.000000000000000000, 0.000000000000000000, 1.300977106640434891E-16 ) ) ;
#39236 = CARTESIAN_POINT ( 'NONE',  ( -71.75000000000000000, -0.9999999999999995559, 20.00000000000000000 ) ) ;
#39237 = COLOUR_RGB ( '', 0.72549020, 0.75294118, 0.79215686) ;
#39238 = CARTESIAN_POINT ( 'NONE',  ( -130.4050000000000011, -2.607480562269069768, 8.024999999999991473 ) ) ;
#39239 = CARTESIAN_POINT ( 'NONE',  ( -164.6929263765338476, 10.01517768586948698, -1.839758294383808966E-15 ) ) ;
#39240 = CARTESIAN_POINT ( 'NONE',  ( -55.49292637653380211, -8.102448949553174629, 5.886773742842742685 ) ) ;
#39241 = CARTESIAN_POINT ( 'NONE',  ( -133.0449999999999875, 7.632228543268600340, 2.479861379858949277 ) ) ;
#39242 = COLOUR_RGB ( '', 0.66274510, 0.83137255, 0.94901961) ;
#39243 = AXIS2_PLACEMENT_3D ( 'NONE', #42575, #63978, #53448 ) ;
#39244 = CARTESIAN_POINT ( 'NONE',  ( -124.1949999999999932, 8.437984349512086979, -1.550032578732815448E-15 ) ) ;
#39245 = VERTEX_POINT ( 'NONE', #28492 ) ;
#39246 = VECTOR ( 'NONE', #68800, 1000.000000000000000 ) ;
#39247 =( BOUNDED_CURVE ( )  B_SPLINE_CURVE ( 2, ( #56715, #46189, #50391, #8865, #66928, #50740, #61968, #18392, #61282, #8536, #24669 ),
 .UNSPECIFIED., .F., .F. ) 
 B_SPLINE_CURVE_WITH_KNOTS ( ( 3, 2, 2, 2, 2, 3 ),
 ( 0.3529411764705882582, 0.3588235294117647078, 0.3647058823529411575, 0.3705882352941177182, 0.3764705882352941679, 0.3823529411764706176 ),
 .UNSPECIFIED. ) 
 CURVE ( )  GEOMETRIC_REPRESENTATION_ITEM ( )  RATIONAL_B_SPLINE_CURVE ( ( 1.000000000000000000, 0.9510565162951535312, 1.000000000000000000, 0.9510565162951535312, 1.000000000000000000, 0.9510565162951535312, 1.000000000000000000, 0.9510565162951535312, 1.000000000000000000, 0.9510565162951530871, 1.000000000000000444 ) ) 
 REPRESENTATION_ITEM ( '' )  );
#39248 = CARTESIAN_POINT ( 'NONE',  ( 31.00000000000002132, 14.00000000000000000, 80.00402776293826435 ) ) ;
#39249 = LINE ( 'NONE', #65948, #63093 ) ;
#39250 = CARTESIAN_POINT ( 'NONE',  ( -177.4429263765338192, -1.166476076187852838E-15, -9.524999999999991473 ) ) ;
#39251 = CARTESIAN_POINT ( 'NONE',  ( -62.39499999999998181, -6.826472737025115478, -4.959722759717899443 ) ) ;
#39252 = SURFACE_STYLE_FILL_AREA ( #8859 ) ;
#39253 =( NAMED_UNIT ( * ) SI_UNIT ( $, .STERADIAN. ) SOLID_ANGLE_UNIT ( ) );
#39254 = DIRECTION ( 'NONE',  ( -1.000000000000000000, 0.000000000000000000, 0.000000000000000000 ) ) ;
#39255 = EDGE_CURVE ( 'NONE', #22411, #25215, #47900, .T. ) ;
#39256 = AXIS2_PLACEMENT_3D ( 'NONE', #21560, #26800, #48333 ) ;
#39257 = CARTESIAN_POINT ( 'NONE',  ( -57.11974195712093660, -8.499999999999992895, 0.06931351858119066955 ) ) ;
#39258 = FILL_AREA_STYLE ('',( #1532 ) ) ;
#39259 = CARTESIAN_POINT ( 'NONE',  ( -100.1929263765337907, -10.01517768586948698, 6.132527647946031529E-16 ) ) ;
#39260 = APPLICATION_PROTOCOL_DEFINITION ( 'draft international standard', 'automotive_design', 1998, #40642 ) ;
#39261 = FACE_OUTER_BOUND ( 'NONE', #3215, .T. ) ;
#39262 = CARTESIAN_POINT ( 'NONE',  ( -162.5070736234661695, 8.102448949553176405, 5.886773742842740909 ) ) ;
#39263 = ADVANCED_FACE ( 'NONE', ( #65811 ), #59835, .F. ) ;
#39264 = CARTESIAN_POINT ( 'NONE',  ( 8.000000000000000000, 0.000000000000000000, -72.00402776293825013 ) ) ;
#39265 = CARTESIAN_POINT ( 'NONE',  ( -78.65707362346617515, 9.058813317711329915, 2.943386871421369566 ) ) ;
#39266 = COLOUR_RGB ( '', 0.40784314, 0.44705882, 0.49803922) ;
#39267 = DIRECTION ( 'NONE',  ( 0.000000000000000000, 0.000000000000000000, 1.000000000000000000 ) ) ;
#39268 = ADVANCED_FACE ( 'NONE', ( #12315 ), #56826, .F. ) ;
#39269 = EDGE_LOOP ( 'NONE', ( #30694, #62016, #62758 ) ) ;
#39270 =( LENGTH_UNIT ( ) NAMED_UNIT ( * ) SI_UNIT ( .MILLI., .METRE. ) );
#39271 = CARTESIAN_POINT ( 'NONE',  ( -55.34553025815903027, -8.494271767728079681, -2.227830982676734628 ) ) ;
#39272 = ORIENTED_EDGE ( 'NONE', *, *, #19865, .T. ) ;
#39273 = CARTESIAN_POINT ( 'NONE',  ( 1.000000000000000000, 42.00000000000000000, 0.000000000000000000 ) ) ;
#39274 = CARTESIAN_POINT ( 'NONE',  ( 6.826472737025121695, 123.6070736234661496, -4.959722759717905660 ) ) ;
#39275 = CYLINDRICAL_SURFACE ( 'NONE', #65258, 0.2500000000000002220 ) ;
#39276 = DIRECTION ( 'NONE',  ( -0.000000000000000000, -0.000000000000000000, -1.000000000000000000 ) ) ;
#39278 = ORIENTED_EDGE ( 'NONE', *, *, #62341, .F. ) ;
#39277 = AXIS2_PLACEMENT_3D ( 'NONE', #62389, #57102, #8924 ) ;
#39279 = EDGE_CURVE ( 'NONE', #32568, #16179, #18322, .T. ) ;
#39280 = LINE ( 'NONE', #45261, #25971 ) ;
#39281 = ORIENTED_EDGE ( 'NONE', *, *, #51391, .F. ) ;
#39282 = B_SPLINE_CURVE_WITH_KNOTS ( 'NONE', 3,
 ( #60621, #6822, #21988, #90, #48399, #16388, #6142, #59943 ),
 .UNSPECIFIED., .F., .F.,
 ( 4, 2, 2, 4 ),
 ( -6.733023926842405106E-06, 0.0008427316310560229676, 0.001267463958547459645, 0.001692196286038896540 ),
 .UNSPECIFIED. ) ;
#39283 = CARTESIAN_POINT ( 'NONE',  ( -119.7570736234661695, -5.598654528085801552, 7.705886871421367523 ) ) ;
#39284 = VECTOR ( 'NONE', #2195, 1000.000000000000000 ) ;
#39285 = VECTOR ( 'NONE', #21251, 1000.000000000000000 ) ;
#39286 = DIRECTION ( 'NONE',  ( -1.000000000000000000, -0.000000000000000000, -0.000000000000000000 ) ) ;
#39287 = CARTESIAN_POINT ( 'NONE',  ( -92.99500000000000455, -6.826472737025115478, 4.959722759717900331 ) ) ;
#39289 = EDGE_LOOP ( 'NONE', ( #24320, #56726, #53309, #55145, #16105 ) ) ;
#39288 = VECTOR ( 'NONE', #2123, 1000.000000000000114 ) ;
#39290 =( GEOMETRIC_REPRESENTATION_CONTEXT ( 3 ) GLOBAL_UNCERTAINTY_ASSIGNED_CONTEXT ( ( #50860 ) ) GLOBAL_UNIT_ASSIGNED_CONTEXT ( ( #27904, #22672, #1137 ) ) REPRESENTATION_CONTEXT ( 'NONE', 'WORKASPACE' ) );
#39291 = CARTESIAN_POINT ( 'NONE',  ( -7.632228543268607446, 123.5429263765338135, -2.479861379858953718 ) ) ;
#39292 = CARTESIAN_POINT ( 'NONE',  ( 45.00000000000000000, 9.916356254361542000, 6.999999999944074069 ) ) ;
#39293 = VERTEX_POINT ( 'NONE', #1005 ) ;
#39294 = CARTESIAN_POINT ( 'NONE',  ( 0.000000000000000000, 161.9429263765338192, -8.025000000000000355 ) ) ;
#39295 = FILL_AREA_STYLE_COLOUR ( '', #29115 ) ;
#39296 = VERTEX_POINT ( 'NONE', #39804 ) ;
#39297 = FACE_OUTER_BOUND ( 'NONE', #21500, .T. ) ;
#39298 = B_SPLINE_CURVE_WITH_KNOTS ( 'NONE', 3,
 ( #44936, #19541, #12878, #8317, #7270, #29760, #35395, #14274 ),
 .UNSPECIFIED., .F., .F.,
 ( 4, 2, 2, 4 ),
 ( 0.01183260977662614621, 0.01392219916432753737, 0.01496699385817823122, 0.01601178855202892506 ),
 .UNSPECIFIED. ) ;
#39299 = EDGE_LOOP ( 'NONE', ( #43288, #26859 ) ) ;
#39300 = FILL_AREA_STYLE ('',( #44250 ) ) ;
#39301 = DIRECTION ( 'NONE',  ( 0.000000000000000000, 0.000000000000000000, 1.000000000000000000 ) ) ;
#39302 = DIRECTION ( 'NONE',  ( 0.000000000000000000, 0.000000000000000000, 1.000000000000000000 ) ) ;
#39304 =( GEOMETRIC_REPRESENTATION_CONTEXT ( 3 ) GLOBAL_UNCERTAINTY_ASSIGNED_CONTEXT ( ( #43322 ) ) GLOBAL_UNIT_ASSIGNED_CONTEXT ( ( #26400, #4952, #15537 ) ) REPRESENTATION_CONTEXT ( 'NONE', 'WORKASPACE' ) );
#39303 = CARTESIAN_POINT ( 'NONE',  ( -30.38025804287907405, -8.500000000000000000, 7.999999999999986677 ) ) ;
#39305 = DIRECTION ( 'NONE',  ( -1.000000000000000000, 0.000000000000000000, 0.000000000000000000 ) ) ;
#39306 = FACE_OUTER_BOUND ( 'NONE', #47364, .T. ) ;
#39307 =( NAMED_UNIT ( * ) SI_UNIT ( $, .STERADIAN. ) SOLID_ANGLE_UNIT ( ) );
#39308 = CARTESIAN_POINT ( 'NONE',  ( -113.0070736234661695, -8.102448949553172852, -5.886773742842741797 ) ) ;
#39309 = CARTESIAN_POINT ( 'NONE',  ( -0.3558155366086579452, 2.493171897977409568, 7.000000000000000000 ) ) ;
#39310 = CARTESIAN_POINT ( 'NONE',  ( 45.50000000000000000, 9.639620389971920389, 6.500000000000000000 ) ) ;
#39311 = ORIENTED_EDGE ( 'NONE', *, *, #13427, .F. ) ;
#39312 = DIRECTION ( 'NONE',  ( 0.000000000000000000, 0.000000000000000000, -1.000000000000000000 ) ) ;
#39313 = DIRECTION ( 'NONE',  ( 1.000000000000000000, 0.000000000000000000, -0.000000000000000000 ) ) ;
#39314 = DIRECTION ( 'NONE',  ( 0.000000000000000000, 0.000000000000000000, -1.000000000000000000 ) ) ;
#39315 = CARTESIAN_POINT ( 'NONE',  ( 21.25000000000001066, 24.74999999999998224, 3.750000000000000000 ) ) ;
#39316 = EDGE_LOOP ( 'NONE', ( #67038, #61264 ) ) ;
#39317 = CARTESIAN_POINT ( 'NONE',  ( -164.0049999999999955, 6.826472737025116366, 4.959722759717898555 ) ) ;
#39318 = LINE ( 'NONE', #43915, #45398 ) ;
#39319 = FILL_AREA_STYLE ('',( #6556 ) ) ;
#39320 = CARTESIAN_POINT ( 'NONE',  ( -165.1449999999999818, -4.716976649647092401, 6.492361379858946790 ) ) ;
#39321 = CARTESIAN_POINT ( 'NONE',  ( -153.8949999999999818, 6.826472737025115478, 4.959722759717899443 ) ) ;
#39322 = CIRCLE ( 'NONE', #48323, 0.2500000000000002220 ) ;
#39323 = STYLED_ITEM ( 'NONE', ( #20940 ), #58971 ) ;
#39324 = ORIENTED_EDGE ( 'NONE', *, *, #23206, .F. ) ;
#39325 =( NAMED_UNIT ( * ) SI_UNIT ( $, .STERADIAN. ) SOLID_ANGLE_UNIT ( ) );
#39326 = STYLED_ITEM ( 'NONE', ( #8521 ), #44302 ) ;
#39327 = SURFACE_STYLE_FILL_AREA ( #43584 ) ;
#39328 = CARTESIAN_POINT ( 'NONE',  ( -74.45499999999999829, 7.632228543268599452, -2.479861379858951942 ) ) ;
#39329 = CARTESIAN_POINT ( 'NONE',  ( 57.00000000000000000, 16.00000000000000000, 72.50402776293826435 ) ) ;
#39330 = CARTESIAN_POINT ( 'NONE',  ( -74.99499999999999034, -6.826472737025113702, 4.959722759717902107 ) ) ;
#39331 = CARTESIAN_POINT ( 'NONE',  ( -5.598654528085806881, 146.8549999999999898, -7.705886871421374629 ) ) ;
#39332 = FILL_AREA_STYLE_COLOUR ( '', #6165 ) ;
#39333 = EDGE_CURVE ( 'NONE', #56654, #39825, #6248, .T. ) ;
#39334 = CIRCLE ( 'NONE', #14604, 0.5000000000000004441 ) ;
#39335 = AXIS2_PLACEMENT_3D ( 'NONE', #64760, #65080, #59822 ) ;
#39336 = PLANE ( 'NONE',  #16666 ) ;
#39337 = AXIS2_PLACEMENT_3D ( 'NONE', #996, #18314, #66128 ) ;
#39338 = CARTESIAN_POINT ( 'NONE',  ( 60.00000000000000000, 1.797044900979284448E-15, -10.49999999999999822 ) ) ;
#39339 = FILL_AREA_STYLE ('',( #49880 ) ) ;
#39340 = VECTOR ( 'NONE', #13428, 1000.000000000000000 ) ;
#39341 =( NAMED_UNIT ( * ) SI_UNIT ( $, .STERADIAN. ) SOLID_ANGLE_UNIT ( ) );
#39342 = LINE ( 'NONE', #24164, #38144 ) ;
#39343 = AXIS2_PLACEMENT_3D ( 'NONE', #62419, #19498, #25131 ) ;
#39344 = EDGE_CURVE ( 'NONE', #57903, #35167, #54880, .T. ) ;
#39345 = CARTESIAN_POINT ( 'NONE',  ( 20.71231517720798010, 149.9999999999999716, -10.00000000000000000 ) ) ;
#39346 = EDGE_CURVE ( 'NONE', #1416, #16364, #61219, .T. ) ;
#39347 = ADVANCED_FACE ( 'NONE', ( #44743, #13030, #54204, #27457 ), #35878, .F. ) ;
#39348 = DIRECTION ( 'NONE',  ( -1.000000000000000000, 0.000000000000000000, 0.000000000000000000 ) ) ;
#39349 = ORIENTED_EDGE ( 'NONE', *, *, #18581, .T. ) ;
#39350 = ORIENTED_EDGE ( 'NONE', *, *, #11527, .F. ) ;
#39351 = SURFACE_STYLE_USAGE ( .BOTH. , #38678 ) ;
#39352 = EDGE_CURVE ( 'NONE', #59935, #22202, #9161, .T. ) ;
#39353 = CARTESIAN_POINT ( 'NONE',  ( -132.9570736234661865, 9.058813317711329915, -2.943386871421373119 ) ) ;
#39354 = EDGE_CURVE ( 'NONE', #61898, #2846, #61277, .T. ) ;
#39355 = FILL_AREA_STYLE_COLOUR ( '', #22636 ) ;
#39356 = FACE_OUTER_BOUND ( 'NONE', #2125, .T. ) ;
#39357 = VECTOR ( 'NONE', #69248, 1000.000000000000000 ) ;
#39358 = CARTESIAN_POINT ( 'NONE',  ( 45.65811388300841855, 10.21937129433612057, -6.500000000000000000 ) ) ;
#39359 = VERTEX_POINT ( 'NONE', #7745 ) ;
#39360 = CARTESIAN_POINT ( 'NONE',  ( -107.3049999999999642, 8.437984349512086979, -1.550032578732815448E-15 ) ) ;
#39361 = ORIENTED_EDGE ( 'NONE', *, *, #44823, .F. ) ;
#39362 = DIRECTION ( 'NONE',  ( 0.000000000000000000, 0.000000000000000000, -1.000000000000000000 ) ) ;
#39363 = ORIENTED_EDGE ( 'NONE', *, *, #6923, .T. ) ;
#39364 = CARTESIAN_POINT ( 'NONE',  ( 23.50000000000001776, 15.00000000000000000, 29.68999999999999417 ) ) ;
#39365 = DIRECTION ( 'NONE',  ( 0.000000000000000000, 0.000000000000000000, 1.000000000000000000 ) ) ;
#39366 = ORIENTED_EDGE ( 'NONE', *, *, #19689, .T. ) ;
#39368 = DIRECTION ( 'NONE',  ( 0.000000000000000000, 1.000000000000000000, 0.000000000000000000 ) ) ;
#39367 = COLOUR_RGB ( '', 0.08235294, 0.09019608, 0.10196078) ;
#39369 = ORIENTED_EDGE ( 'NONE', *, *, #57027, .T. ) ;
#39370 = ORIENTED_EDGE ( 'NONE', *, *, #24599, .T. ) ;
#39371 = CARTESIAN_POINT ( 'NONE',  ( -74.10731665482167330, 9.343685333619710320, -6.169793031889357238 ) ) ;
#39372 = CARTESIAN_POINT ( 'NONE',  ( -152.9070736234666015, -3.094860106612244977, 9.525000000004485656 ) ) ;
#39373 = STYLED_ITEM ( 'NONE', ( #65435 ), #44762 ) ;
#39374 = PRESENTATION_STYLE_ASSIGNMENT (( #1659 ) ) ;
#39375 = EDGE_LOOP ( 'NONE', ( #52949, #14002, #20091, #47357, #26524, #14104, #13746, #32429, #42502, #26389, #46572, #36881, #8700, #28753, #58974, #30483, #47427, #64896, #5920, #63632, #19269, #30157, #47433, #989, #51096, #43388, #51368, #69595, #288, #18029, #21802, #12671, #60455, #68421, #9143, #29299, #48053, #34491, #14080, #15924, #7546, #22458, #52451, #56107, #1951, #32676 ) ) ;
#39376 = CARTESIAN_POINT ( 'NONE',  ( -4.716976649647097730, 132.2429263765338021, -6.492361379858953896 ) ) ;
#39377 = SPHERICAL_SURFACE ( 'NONE', #46974, 0.2500000000000000000 ) ;
#39378 = LINE ( 'NONE', #6292, #47937 ) ;
#39379 = DIRECTION ( 'NONE',  ( -1.239088197126290817E-16, 0.000000000000000000, -1.000000000000000000 ) ) ;
#39380 = CARTESIAN_POINT ( 'NONE',  ( 60.00000000000000000, 112.4999999999999858, -9.500000000000000000 ) ) ;
#39381 = VERTEX_POINT ( 'NONE', #8469 ) ;
#39382 = MECHANICAL_DESIGN_GEOMETRIC_PRESENTATION_REPRESENTATION (  '', ( #24722 ), #42772 ) ;
#39383 = CYLINDRICAL_SURFACE ( 'NONE', #43124, 0.9999999999999992228 ) ;
#39384 = VERTEX_POINT ( 'NONE', #56643 ) ;
#39385 = DIRECTION ( 'NONE',  ( -1.000000000000000000, 0.000000000000000000, 0.000000000000000000 ) ) ;
#39386 = CIRCLE ( 'NONE', #13483, 5.000000000000004441 ) ;
#39387 = CARTESIAN_POINT ( 'NONE',  ( -6.826472737025120807, 140.1070736234661638, 4.959722759717906548 ) ) ;
#39388 = CARTESIAN_POINT ( 'NONE',  ( -71.99999999999998579, 119.9999999999997868, -9.500000000000000000 ) ) ;
#39389 = CARTESIAN_POINT ( 'NONE',  ( -128.9050000000000011, 2.607480562269068880, -8.024999999999993250 ) ) ;
#39390 =( NAMED_UNIT ( * ) SI_UNIT ( $, .STERADIAN. ) SOLID_ANGLE_UNIT ( ) );
#39391 = CIRCLE ( 'NONE', #50607, 9.999999999999998224 ) ;
#39392 = ORIENTED_EDGE ( 'NONE', *, *, #12640, .T. ) ;
#39393 = CARTESIAN_POINT ( 'NONE',  ( -66.49999999999998579, 50.00000000000000000, -12.00000000000000000 ) ) ;
#39394 = CIRCLE ( 'NONE', #21373, 0.5000000000000004441 ) ;
#39395 = CARTESIAN_POINT ( 'NONE',  ( 0.000000000000000000, 9.000000000000007105, 0.000000000000000000 ) ) ;
#39396 = CARTESIAN_POINT ( 'NONE',  ( -2.754976799258605169, -2.005084411322475724, 7.000000000000000000 ) ) ;
#39397 = ORIENTED_EDGE ( 'NONE', *, *, #67923, .T. ) ;
#39398 = PRESENTATION_LAYER_ASSIGNMENT (  '', '', ( #30349 ) ) ;
#39399 = VERTEX_POINT ( 'NONE', #52079 ) ;
#39400 = CARTESIAN_POINT ( 'NONE',  ( -45.89905495956738690, 9.405628579031734660, 2.999999999999999556 ) ) ;
#39401 = CARTESIAN_POINT ( 'NONE',  ( -109.4929263765337737, -8.102448949553174629, 5.886773742842742685 ) ) ;
#39402 = CARTESIAN_POINT ( 'NONE',  ( -49.55499999999998550, 0.000000000000000000, 8.024999999999991473 ) ) ;
#39403 = ORIENTED_EDGE ( 'NONE', *, *, #18435, .T. ) ;
#39404 = DIRECTION ( 'NONE',  ( 0.000000000000000000, 1.000000000000000000, 0.000000000000000000 ) ) ;
#39405 = LINE ( 'NONE', #55547, #31516 ) ;
#39406 = LINE ( 'NONE', #12625, #56527 ) ;
#39407 = DIRECTION ( 'NONE',  ( -1.000000000000000000, 0.000000000000000000, 0.000000000000000000 ) ) ;
#39408 = AXIS2_PLACEMENT_3D ( 'NONE', #11251, #54504, #32699 ) ;
#39409 = COLOUR_RGB ( '', 0.66274510, 0.83137255, 0.94901961) ;
#39410 = CARTESIAN_POINT ( 'NONE',  ( 6.123233995736766282E-16, 1.999999999999998668, -5.000000000000000000 ) ) ;
#39411 = DIRECTION ( 'NONE',  ( 1.000000000000000000, -0.000000000000000000, -0.000000000000000000 ) ) ;
#39412 = ORIENTED_EDGE ( 'NONE', *, *, #59964, .F. ) ;
#39413 = AXIS2_PLACEMENT_3D ( 'NONE', #22020, #48787, #487 ) ;
#39414 = DIRECTION ( 'NONE',  ( 1.000000000000000000, 0.000000000000000000, 0.000000000000000000 ) ) ;
#39415 = LINE ( 'NONE', #61178, #67219 ) ;
#39416 = CARTESIAN_POINT ( 'NONE',  ( 6.826472737025119919, 117.0070736234661410, 4.959722759717908325 ) ) ;
#39417 = CARTESIAN_POINT ( 'NONE',  ( 6.402811457828279984, 154.5000000000000284, -7.065455983348243763 ) ) ;
#39419 = DIRECTION ( 'NONE',  ( 0.000000000000000000, 1.000000000000000000, 0.000000000000000000 ) ) ;
#39418 = VECTOR ( 'NONE', #69496, 1000.000000000000000 ) ;
#39420 = FACE_BOUND ( 'NONE', #52847, .T. ) ;
#39421 = CARTESIAN_POINT ( 'NONE',  ( -101.2449999999999903, -4.716976649647093289, -6.492361379858945902 ) ) ;
#39422 = CARTESIAN_POINT ( 'NONE',  ( 0.000000000000000000, 119.5549999999999926, -9.525000000000000355 ) ) ;
#39423 = CARTESIAN_POINT ( 'NONE',  ( -76.79499999999998749, 2.607480562269068880, -8.024999999999993250 ) ) ;
#39424 =( NAMED_UNIT ( * ) PLANE_ANGLE_UNIT ( ) SI_UNIT ( $, .RADIAN. ) );
#39425 = EDGE_CURVE ( 'NONE', #33800, #51729, #3107, .T. ) ;
#39426 = DIRECTION ( 'NONE',  ( 0.3361263392814427542, 0.000000000000000000, 0.9418169057949938860 ) ) ;
#39427 = COLOUR_RGB ( '', 0.66274510, 0.83137255, 0.94901961) ;
#39428 = DIRECTION ( 'NONE',  ( 1.000000000000000000, 0.000000000000000000, -1.300977106640435137E-16 ) ) ;
#39429 = EDGE_CURVE ( 'NONE', #69624, #65961, #56983, .T. ) ;
#39430 = DIRECTION ( 'NONE',  ( -1.000000000000000000, 0.000000000000000000, 0.000000000000000000 ) ) ;
#39431 = CARTESIAN_POINT ( 'NONE',  ( 41.84210526315788314, 107.2928455055531600, -4.000000000000000000 ) ) ;
#39433 = ORIENTED_EDGE ( 'NONE', *, *, #60913, .T. ) ;
#39432 = AXIS2_PLACEMENT_3D ( 'NONE', #4258, #41980, #3928 ) ;
#39434 = CARTESIAN_POINT ( 'NONE',  ( -126.1429263765337936, 5.598654528085800663, -7.705886871421367523 ) ) ;
#39435 = MECHANICAL_DESIGN_GEOMETRIC_PRESENTATION_REPRESENTATION (  '', ( #1104 ), #17088 ) ;
#39436 = CARTESIAN_POINT ( 'NONE',  ( -137.9950000000000045, -6.826472737025115478, 4.959722759717900331 ) ) ;
#39437 = AXIS2_PLACEMENT_3D ( 'NONE', #26827, #21584, #42060 ) ;
#39438 = EDGE_CURVE ( 'NONE', #18810, #26382, #46476, .T. ) ;
#39439 = PRESENTATION_STYLE_ASSIGNMENT (( #39096 ) ) ;
#39440 = CARTESIAN_POINT ( 'NONE',  ( -173.8429263765338249, 9.058813317711329915, -2.943386871421373119 ) ) ;
#39441 = ORIENTED_EDGE ( 'NONE', *, *, #42612, .T. ) ;
#39442 = EDGE_LOOP ( 'NONE', ( #40219, #31918, #8377, #60002 ) ) ;
#39443 = VECTOR ( 'NONE', #11109, 1000.000000000000000 ) ;
#39444 = FACE_OUTER_BOUND ( 'NONE', #51778, .T. ) ;
#39445 = EDGE_CURVE ( 'NONE', #61513, #64160, #19338, .T. ) ;
#39446 = FACE_OUTER_BOUND ( 'NONE', #54375, .T. ) ;
#39447 = DIRECTION ( 'NONE',  ( 0.000000000000000000, 0.000000000000000000, 1.000000000000000000 ) ) ;
#39448 = VECTOR ( 'NONE', #50746, 1000.000000000000000 ) ;
#39449 = DIRECTION ( 'NONE',  ( 0.000000000000000000, 0.000000000000000000, 1.000000000000000000 ) ) ;
#39450 =( LENGTH_UNIT ( ) NAMED_UNIT ( * ) SI_UNIT ( .MILLI., .METRE. ) );
#39451 = ORIENTED_EDGE ( 'NONE', *, *, #23217, .F. ) ;
#39452 = CARTESIAN_POINT ( 'NONE',  ( -140.4549999999999841, 7.632228543268599452, -2.479861379858951942 ) ) ;
#39453 = ORIENTED_EDGE ( 'NONE', *, *, #64658, .F. ) ;
#39454 = ORIENTED_EDGE ( 'NONE', *, *, #69490, .T. ) ;
#39455 = CARTESIAN_POINT ( 'NONE',  ( 13.25000000000000355, 27.74999999999998934, -4.000000000000000000 ) ) ;
#39456 = EDGE_LOOP ( 'NONE', ( #16568, #63340, #10933 ) ) ;
#39457 = AXIS2_PLACEMENT_3D ( 'NONE', #34419, #55530, #51298 ) ;
#39458 = SURFACE_SIDE_STYLE ('',( #40147 ) ) ;
#39459 = FACE_OUTER_BOUND ( 'NONE', #48388, .T. ) ;
#39460 = CARTESIAN_POINT ( 'NONE',  ( 3.094860106618435136, 130.2949999999999591, -9.525000000000000355 ) ) ;
#39461 = FILL_AREA_STYLE_COLOUR ( '', #67677 ) ;
#39462 = CIRCLE ( 'NONE', #55119, 8.000000000000007105 ) ;
#39463 = ORIENTED_EDGE ( 'NONE', *, *, #9253, .T. ) ;
#39464 = CARTESIAN_POINT ( 'NONE',  ( 45.50000000000000000, 10.69371294336137801, 6.000000000000000888 ) ) ;
#39465 = CARTESIAN_POINT ( 'NONE',  ( 8.102448949553181734, 143.1049999999999613, -5.886773742842746238 ) ) ;
#39466 = CARTESIAN_POINT ( 'NONE',  ( -55.10499999999998266, -6.826472737025113702, 4.959722759717902107 ) ) ;
#39467 = EDGE_LOOP ( 'NONE', ( #64464, #67133 ) ) ;
#39468 = CARTESIAN_POINT ( 'NONE',  ( 8.102448949553183510, 155.1049999999999898, -5.886773742842746238 ) ) ;
#39469 = DIRECTION ( 'NONE',  ( 1.000000000000000000, -0.000000000000000000, 0.000000000000000000 ) ) ;
#39470 = DIRECTION ( 'NONE',  ( -1.000000000000000000, 0.000000000000000000, 0.000000000000000000 ) ) ;
#39471 =( NAMED_UNIT ( * ) SI_UNIT ( $, .STERADIAN. ) SOLID_ANGLE_UNIT ( ) );
#39472 = CARTESIAN_POINT ( 'NONE',  ( 0.000000000000000000, 27.74999999999998934, 3.750000000000000000 ) ) ;
#39473 = EDGE_LOOP ( 'NONE', ( #19871, #64093, #48741, #46188 ) ) ;
#39474 = SURFACE_STYLE_USAGE ( .BOTH. , #22931 ) ;
#39475 = VERTEX_POINT ( 'NONE', #51023 ) ;
#39476 = DIRECTION ( 'NONE',  ( 0.000000000000000000, 1.000000000000000000, 0.000000000000000000 ) ) ;
#39477 = CARTESIAN_POINT ( 'NONE',  ( -121.8570736234661780, -5.598654528085803328, -7.705886871421366635 ) ) ;
#39478 =( NAMED_UNIT ( * ) PLANE_ANGLE_UNIT ( ) SI_UNIT ( $, .RADIAN. ) );
#39480 = CARTESIAN_POINT ( 'NONE',  ( -157.8549999999999898, 4.716976649647094177, 6.492361379858945902 ) ) ;
#39479 = CIRCLE ( 'NONE', #9127, 9.000000000000007105 ) ;
#39481 = ORIENTED_EDGE ( 'NONE', *, *, #24081, .F. ) ;
#39482 = EDGE_CURVE ( 'NONE', #7454, #13649, #24602, .T. ) ;
#39483 = AXIS2_PLACEMENT_3D ( 'NONE', #643, #60815, #22169 ) ;
#39484 = LINE ( 'NONE', #49677, #41778 ) ;
#39485 = FACE_OUTER_BOUND ( 'NONE', #46129, .T. ) ;
#39486 = ORIENTED_EDGE ( 'NONE', *, *, #55440, .F. ) ;
#39487 = ORIENTED_EDGE ( 'NONE', *, *, #64346, .F. ) ;
#39488 = DIRECTION ( 'NONE',  ( 0.000000000000000000, 1.000000000000000000, 0.000000000000000000 ) ) ;
#39489 = CARTESIAN_POINT ( 'NONE',  ( -45.91547277936962246, 9.430195807687212550, -3.611004237778682402 ) ) ;
#39490 = CARTESIAN_POINT ( 'NONE',  ( -74.00499999999996703, 6.826472737025116366, 4.959722759717898555 ) ) ;
#39491 = ORIENTED_EDGE ( 'NONE', *, *, #13182, .F. ) ;
#39492 = COLOUR_RGB ( '', 0.40784314, 0.44705882, 0.49803922) ;
#39493 = CARTESIAN_POINT ( 'NONE',  ( 74.50000000000000000, 19.30628705663858113, -6.999999999999999112 ) ) ;
#39494 = DIRECTION ( 'NONE',  ( 1.000000000000000000, -0.000000000000000000, 0.000000000000000000 ) ) ;
#39495 = CIRCLE ( 'NONE', #15889, 0.2500000000000002220 ) ;
#39496 = ORIENTED_EDGE ( 'NONE', *, *, #11238, .F. ) ;
#39497 = CARTESIAN_POINT ( 'NONE',  ( -65.49999999999998579, 50.00000000000000000, 10.00000000000000000 ) ) ;
#39498 = CIRCLE ( 'NONE', #18079, 0.2500000000000002220 ) ;
#39500 = SPHERICAL_SURFACE ( 'NONE', #41566, 0.2500000000000000000 ) ;
#39499 = CARTESIAN_POINT ( 'NONE',  ( -53.75707362346618368, -5.598654528085801552, 7.705886871421367523 ) ) ;
#39501 = EDGE_CURVE ( 'NONE', #27268, #10308, #62438, .T. ) ;
#39502 = EDGE_CURVE ( 'NONE', #12316, #29106, #59072, .T. ) ;
#39503 = CARTESIAN_POINT ( 'NONE',  ( -3.094860106618434248, 134.7949999999999875, 9.525000000000000355 ) ) ;
#39504 = CARTESIAN_POINT ( 'NONE',  ( -110.3949999999999818, -6.826472737025115478, -4.959722759717899443 ) ) ;
#39505 = AXIS2_PLACEMENT_3D ( 'NONE', #58300, #57254, #30158 ) ;
#39506 = DIRECTION ( 'NONE',  ( -1.300977106640434891E-16, 0.000000000000000000, -1.000000000000000000 ) ) ;
#39507 = CIRCLE ( 'NONE', #47406, 7.500000000000000000 ) ;
#39508 = LINE ( 'NONE', #8524, #63826 ) ;
#39509 = EDGE_CURVE ( 'NONE', #65525, #47886, #54406, .T. ) ;
#39510 = CARTESIAN_POINT ( 'NONE',  ( -157.4929263765337737, -8.102448949553172852, 5.886773742842742685 ) ) ;
#39511 = CARTESIAN_POINT ( 'NONE',  ( -168.8949999999999818, 6.826472737025116366, 4.959722759717898555 ) ) ;
#39512 = EDGE_CURVE ( 'NONE', #30840, #46101, #52324, .T. ) ;
#39513 =( NAMED_UNIT ( * ) SI_UNIT ( $, .STERADIAN. ) SOLID_ANGLE_UNIT ( ) );
#39514 = EDGE_LOOP ( 'NONE', ( #27567, #25909, #34090 ) ) ;
#39515 = ORIENTED_EDGE ( 'NONE', *, *, #62891, .T. ) ;
#39516 = CIRCLE ( 'NONE', #2298, 6.999999999999997335 ) ;
#39517 = CARTESIAN_POINT ( 'NONE',  ( -69.89292637653380780, -8.102448949553172852, -5.886773742842741797 ) ) ;
#39518 = LINE ( 'NONE', #33186, #66833 ) ;
#39519 = AXIS2_PLACEMENT_3D ( 'NONE', #59213, #31105, #42768 ) ;
#39520 = MECHANICAL_DESIGN_GEOMETRIC_PRESENTATION_REPRESENTATION (  '', ( #28159 ), #63037 ) ;
#39521 = EDGE_CURVE ( 'NONE', #21141, #23645, #21779, .T. ) ;
#39522 = DIRECTION ( 'NONE',  ( 1.000000000000000000, 0.000000000000000000, 0.000000000000000000 ) ) ;
#39523 = CARTESIAN_POINT ( 'NONE',  ( -141.5929263765343649, -3.094860106627439933, -9.524999999993450928 ) ) ;
#39524 =( LENGTH_UNIT ( ) NAMED_UNIT ( * ) SI_UNIT ( .MILLI., .METRE. ) );
#39526 =( GEOMETRIC_REPRESENTATION_CONTEXT ( 3 ) GLOBAL_UNCERTAINTY_ASSIGNED_CONTEXT ( ( #17992 ) ) GLOBAL_UNIT_ASSIGNED_CONTEXT ( ( #45566, #49170, #11858 ) ) REPRESENTATION_CONTEXT ( 'NONE', 'WORKASPACE' ) );
#39525 = SURFACE_STYLE_USAGE ( .BOTH. , #50399 ) ;
#39527 = ORIENTED_EDGE ( 'NONE', *, *, #8296, .T. ) ;
#39528 = CARTESIAN_POINT ( 'NONE',  ( -170.6050000000000182, 6.826472737025113702, -4.959722759717902107 ) ) ;
#39529 = ORIENTED_EDGE ( 'NONE', *, *, #22813, .F. ) ;
#39530 = FACE_OUTER_BOUND ( 'NONE', #36797, .T. ) ;
#39531 = STYLED_ITEM ( 'NONE', ( #2302 ), #22165 ) ;
#39532 = CARTESIAN_POINT ( 'NONE',  ( -13.23915246117191025, 52.65078610323165265, 2.000000000000000000 ) ) ;
#39533 = CARTESIAN_POINT ( 'NONE',  ( -15.00000000000000000, 8.000000000000000000, 3.500000000000003997 ) ) ;
#39534 = VECTOR ( 'NONE', #54292, 1000.000000000000000 ) ;
#39535 = DIRECTION ( 'NONE',  ( 0.000000000000000000, 0.000000000000000000, 1.000000000000000000 ) ) ;
#39536 = CARTESIAN_POINT ( 'NONE',  ( -2.607480562269075097, 155.4070736234661467, 8.025000000000000355 ) ) ;
#39537 = COLOUR_RGB ( '', 0.31764706, 0.68627451, 0.89019608) ;
#39538 = ORIENTED_EDGE ( 'NONE', *, *, #33123, .T. ) ;
#39539 = DIRECTION ( 'NONE',  ( 0.2413793103448194644, -0.9704308468600220117, 0.000000000000000000 ) ) ;
#39540 = CARTESIAN_POINT ( 'NONE',  ( 75.00000000000000000, -2.215169945516535778E-14, -6.999999999999999112 ) ) ;
#39541 = CARTESIAN_POINT ( 'NONE',  ( -81.65499999999998693, -7.632228543268600340, -2.479861379858950166 ) ) ;
#39542 = DIRECTION ( 'NONE',  ( -1.000000000000000000, 0.000000000000000000, 0.000000000000000000 ) ) ;
#39543 = CARTESIAN_POINT ( 'NONE',  ( -3.094860106618432471, 131.7049999999999557, -9.525000000000000355 ) ) ;
#39544 = CIRCLE ( 'NONE', #36124, 1.000000000000000888 ) ;
#39545 = FACE_OUTER_BOUND ( 'NONE', #57587, .T. ) ;
#39546 = AXIS2_PLACEMENT_3D ( 'NONE', #48488, #187, #5173 ) ;
#39547 = CARTESIAN_POINT ( 'NONE',  ( -72.05707362346616662, 0.000000000000000000, 9.524999999999991473 ) ) ;
#39548 = DIRECTION ( 'NONE',  ( -0.000000000000000000, -1.000000000000000000, -0.000000000000000000 ) ) ;
#39549 = SURFACE_STYLE_USAGE ( .BOTH. , #1822 ) ;
#39550 = AXIS2_PLACEMENT_3D ( 'NONE', #68709, #31049, #36388 ) ;
#39551 = ORIENTED_EDGE ( 'NONE', *, *, #19634, .F. ) ;
#39552 = CARTESIAN_POINT ( 'NONE',  ( -139.7070736234666981, -3.094860106627305374, -9.524999999993545075 ) ) ;
#39553 = DIRECTION ( 'NONE',  ( 0.000000000000000000, 0.000000000000000000, 1.000000000000000000 ) ) ;
#39554 = CARTESIAN_POINT ( 'NONE',  ( -51.29499999999997328, -2.607480562269069768, 8.024999999999991473 ) ) ;
#39555 = ORIENTED_EDGE ( 'NONE', *, *, #62572, .T. ) ;
#39556 =( BOUNDED_SURFACE ( )  B_SPLINE_SURFACE ( 3, 2, ( 
 ( #14178, #30312, #26767 ),
 ( #31722, #42678, #30406 ),
 ( #54565, #37051, #21166 ),
 ( #65108, #44067, #32767 ),
 ( #21517, #43035, #11658 ),
 ( #16962, #6373, #58815 ),
 ( #59485, #10630, #4991 ),
 ( #15932, #59849, #27115 ) ),
 .UNSPECIFIED., .F., .F., .F. ) 
 B_SPLINE_SURFACE_WITH_KNOTS ( ( 4, 2, 2, 4 ),
 ( 3, 3 ),
 ( 0.0005765750791842532991, 0.001029553238931489936, 0.001482531398678726357, 0.002388487718173199631 ),
 ( 0.000000000000000000, 1.000000000000000000 ),
 .UNSPECIFIED. ) 
 GEOMETRIC_REPRESENTATION_ITEM ( )  RATIONAL_B_SPLINE_SURFACE ( (
 ( 1.000000000000000000, 0.8885233166386380388, 1.000000000000000000),
 ( 1.000000000000000000, 0.8885760224879380997, 1.000000000000000000),
 ( 1.000000000000000000, 0.8838232350071987264, 1.000000000000000000),
 ( 1.000000000000000000, 0.8662144792540084071, 1.000000000000000000),
 ( 1.000000000000000000, 0.8532605865698873471, 1.000000000000000000),
 ( 1.000000000000000000, 0.8046051514203296229, 1.000000000000000000),
 ( 1.000000000000000000, 0.7601637718248414055, 1.000000000000000000),
 ( 1.000000000000000000, 0.7071067811865441310, 1.000000000000000000) ) ) 
 REPRESENTATION_ITEM ( '' )  SURFACE ( )  );
#39557 = CARTESIAN_POINT ( 'NONE',  ( 57.00000000000000000, 16.00000000000000000, -55.00402776293825724 ) ) ;
#39558 = EDGE_CURVE ( 'NONE', #17220, #36075, #39983, .T. ) ;
#39559 = AXIS2_PLACEMENT_3D ( 'NONE', #15513, #15856, #48223 ) ;
#39560 =( NAMED_UNIT ( * ) PLANE_ANGLE_UNIT ( ) SI_UNIT ( $, .RADIAN. ) );
#39561 = CARTESIAN_POINT ( 'NONE',  ( -138.5070736234661695, 8.102448949553176405, 5.886773742842740909 ) ) ;
#39562 = CARTESIAN_POINT ( 'NONE',  ( -44.99999999999998579, 119.9999999999999716, -7.000000000000000000 ) ) ;
#39563 = EDGE_LOOP ( 'NONE', ( #41439, #12070, #34721, #1974 ) ) ;
#39564 = CARTESIAN_POINT ( 'NONE',  ( -50.50422316360081965, -10.70702235289599002, 3.851429980451545276 ) ) ;
#39565 = CARTESIAN_POINT ( 'NONE',  ( -56.39499999999997470, -6.826472737025113702, -4.959722759717900331 ) ) ;
#39566 = SURFACE_SIDE_STYLE ('',( #28944 ) ) ;
#39567 = ORIENTED_EDGE ( 'NONE', *, *, #65434, .T. ) ;
#39568 = CIRCLE ( 'NONE', #9221, 0.2500000000000002220 ) ;
#39569 = CARTESIAN_POINT ( 'NONE',  ( -74.17570909904742393, 9.081512406228229750, 6.320717432316669715 ) ) ;
#39570 = CARTESIAN_POINT ( 'NONE',  ( -118.5549999999999926, 0.000000000000000000, 8.024999999999991473 ) ) ;
#39571 = VERTEX_POINT ( 'NONE', #5567 ) ;
#39572 = CARTESIAN_POINT ( 'NONE',  ( -2.607480562269116842, 119.4070736234661609, 8.024999999999970157 ) ) ;
#39573 = DIRECTION ( 'NONE',  ( -1.000000000000000000, -0.000000000000000000, -0.000000000000000000 ) ) ;
#39574 = CARTESIAN_POINT ( 'NONE',  ( -150.6570736234661751, 9.058813317711329915, 2.943386871421369566 ) ) ;
#39575 =( GEOMETRIC_REPRESENTATION_CONTEXT ( 3 ) GLOBAL_UNCERTAINTY_ASSIGNED_CONTEXT ( ( #53742 ) ) GLOBAL_UNIT_ASSIGNED_CONTEXT ( ( #37382, #58787, #5294 ) ) REPRESENTATION_CONTEXT ( 'NONE', 'WORKASPACE' ) );
#39576 = DIRECTION ( 'NONE',  ( -1.000000000000000000, 0.000000000000000000, 0.000000000000000000 ) ) ;
#39577 = CARTESIAN_POINT ( 'NONE',  ( -3.094860106618432471, 145.5949999999999704, -9.525000000000000355 ) ) ;
#39578 = CARTESIAN_POINT ( 'NONE',  ( -82.10707362346616378, 8.102448949553171076, -5.886773742842744461 ) ) ;
#39579 = EDGE_CURVE ( 'NONE', #34321, #40436, #40443, .T. ) ;
#39580 = AXIS2_PLACEMENT_3D ( 'NONE', #63092, #10930, #46969 ) ;
#39581 = FACE_OUTER_BOUND ( 'NONE', #32063, .T. ) ;
#39582 = ORIENTED_EDGE ( 'NONE', *, *, #47146, .T. ) ;
#39584 = CARTESIAN_POINT ( 'NONE',  ( -177.0570736234661808, 0.000000000000000000, 9.524999999999991473 ) ) ;
#39583 = PRESENTATION_LAYER_ASSIGNMENT (  '', '', ( #51914 ) ) ;
#39585 = LINE ( 'NONE', #56060, #66066 ) ;
#39586 = DIRECTION ( 'NONE',  ( 0.000000000000000000, 0.000000000000000000, -1.000000000000000000 ) ) ;
#39587 = EDGE_CURVE ( 'NONE', #12513, #64724, #9648, .T. ) ;
#39588 = CARTESIAN_POINT ( 'NONE',  ( -130.7049999999999841, 2.607480562269073321, 8.024999999999991473 ) ) ;
#39589 = DIRECTION ( 'NONE',  ( 0.000000000000000000, 0.000000000000000000, -1.000000000000000000 ) ) ;
#39590 = EDGE_CURVE ( 'NONE', #22472, #61072, #24270, .T. ) ;
#39591 = AXIS2_PLACEMENT_3D ( 'NONE', #5142, #3729, #36857 ) ;
#39592 = CARTESIAN_POINT ( 'NONE',  ( -134.6950000000000216, -8.437984349512085203, 5.166775262442717831E-16 ) ) ;
#39593 = CARTESIAN_POINT ( 'NONE',  ( -125.8449999999999847, -7.632228543268599452, 2.479861379858951054 ) ) ;
#39594 = CIRCLE ( 'NONE', #45220, 0.5000000000000004441 ) ;
#39595 = CARTESIAN_POINT ( 'NONE',  ( 8.000000000000000000, 5.000000000000000000, 72.00402776293825013 ) ) ;
#39596 = EDGE_LOOP ( 'NONE', ( #63876, #39403, #35042, #59118 ) ) ;
#39597 = CIRCLE ( 'NONE', #67684, 1.999999999999998224 ) ;
#39598 = FACE_OUTER_BOUND ( 'NONE', #35082, .T. ) ;
#39599 =( NAMED_UNIT ( * ) SI_UNIT ( $, .STERADIAN. ) SOLID_ANGLE_UNIT ( ) );
#39600 = EDGE_CURVE ( 'NONE', #2089, #43714, #30933, .T. ) ;
#39601 = CARTESIAN_POINT ( 'NONE',  ( -121.7929263765346235, -3.094860106605321182, 9.525000000009514523 ) ) ;
#39602 = CARTESIAN_POINT ( 'NONE',  ( -48.80499999999998550, -8.437984349512085203, 5.166775262442717831E-16 ) ) ;
#39603 = FILL_AREA_STYLE_COLOUR ( '', #58513 ) ;
#39604 = CARTESIAN_POINT ( 'NONE',  ( -48.74499999999998323, 4.716976649647094177, 6.492361379858945902 ) ) ;
#39605 = ADVANCED_FACE ( 'NONE', ( #32316 ), #8577, .T. ) ;
#39606 = STYLED_ITEM ( 'NONE', ( #38812 ), #28807 ) ;
#39607 = CARTESIAN_POINT ( 'NONE',  ( 44.99999999999977973, 146.9999999999999716, 7.500000000000000000 ) ) ;
#39608 =( GEOMETRIC_REPRESENTATION_CONTEXT ( 3 ) GLOBAL_UNCERTAINTY_ASSIGNED_CONTEXT ( ( #67259 ) ) GLOBAL_UNIT_ASSIGNED_CONTEXT ( ( #62298, #3502, #34185 ) ) REPRESENTATION_CONTEXT ( 'NONE', 'WORKASPACE' ) );
#39609 = DIRECTION ( 'NONE',  ( 0.000000000000000000, 0.000000000000000000, 1.000000000000000000 ) ) ;
#39610 = CARTESIAN_POINT ( 'NONE',  ( -95.09292637653381064, 3.094860106618433360, 9.524999999999991473 ) ) ;
#39611 = DIRECTION ( 'NONE',  ( -1.000000000000000000, 0.000000000000000000, 0.000000000000000000 ) ) ;
#39612 = DIRECTION ( 'NONE',  ( 0.000000000000000000, 0.000000000000000000, -1.000000000000000000 ) ) ;
#39613 = MECHANICAL_DESIGN_GEOMETRIC_PRESENTATION_REPRESENTATION (  '', ( #17118 ), #20501 ) ;
#39614 = CARTESIAN_POINT ( 'NONE',  ( 44.50000000000000000, 99.99999999999992895, 3.500000000000000000 ) ) ;
#39615 =( GEOMETRIC_REPRESENTATION_CONTEXT ( 3 ) GLOBAL_UNCERTAINTY_ASSIGNED_CONTEXT ( ( #37838 ) ) GLOBAL_UNIT_ASSIGNED_CONTEXT ( ( #65126, #12019, #13394 ) ) REPRESENTATION_CONTEXT ( 'NONE', 'WORKASPACE' ) );
#39616 = ORIENTED_EDGE ( 'NONE', *, *, #8105, .T. ) ;
#39617 = FILL_AREA_STYLE_COLOUR ( '', #39761 ) ;
#39618 = PRESENTATION_STYLE_ASSIGNMENT (( #11199 ) ) ;
#39619 = ORIENTED_EDGE ( 'NONE', *, *, #52906, .T. ) ;
#39620 =( GEOMETRIC_REPRESENTATION_CONTEXT ( 3 ) GLOBAL_UNCERTAINTY_ASSIGNED_CONTEXT ( ( #39005 ) ) GLOBAL_UNIT_ASSIGNED_CONTEXT ( ( #29073, #55125, #28380 ) ) REPRESENTATION_CONTEXT ( 'NONE', 'WORKASPACE' ) );
#39621 = EDGE_CURVE ( 'NONE', #12723, #63323, #18663, .T. ) ;
#39622 = CARTESIAN_POINT ( 'NONE',  ( -9.827790563157511022E-16, 125.5570736234661524, 8.025000000000000355 ) ) ;
#39623 = DIRECTION ( 'NONE',  ( -1.000000000000000000, 0.000000000000000000, 0.000000000000000000 ) ) ;
#39624 = DIRECTION ( 'NONE',  ( 0.000000000000000000, 0.000000000000000000, 1.000000000000000000 ) ) ;
#39625 = ORIENTED_EDGE ( 'NONE', *, *, #1122, .T. ) ;
#39626 = CARTESIAN_POINT ( 'NONE',  ( 0.000000000000000000, 36.74999999999999289, -3.750000000000000000 ) ) ;
#39627 = LINE ( 'NONE', #67367, #32211 ) ;
#39628 = MECHANICAL_DESIGN_GEOMETRIC_PRESENTATION_REPRESENTATION (  '', ( #51963 ), #23881 ) ;
#39629 = FILL_AREA_STYLE_COLOUR ( '', #47486 ) ;
#39630 = CARTESIAN_POINT ( 'NONE',  ( -81.14499999999998181, -4.716976649647092401, 6.492361379858946790 ) ) ;
#39631 = ORIENTED_EDGE ( 'NONE', *, *, #45497, .T. ) ;
#39632 = CARTESIAN_POINT ( 'NONE',  ( -19.89974874213239886, 114.9999999999999574, -10.49999999999999645 ) ) ;
#39633 = CARTESIAN_POINT ( 'NONE',  ( 8.750000000000001776, 24.99999999999998579, 3.750000000000000000 ) ) ;
#39634 = PLANE ( 'NONE',  #3671 ) ;
#39635 = ORIENTED_EDGE ( 'NONE', *, *, #52775, .F. ) ;
#39636 =( NAMED_UNIT ( * ) PLANE_ANGLE_UNIT ( ) SI_UNIT ( $, .RADIAN. ) );
#39637 = DIRECTION ( 'NONE',  ( -1.000000000000000000, 0.000000000000000000, 0.000000000000000000 ) ) ;
#39638 = COLOUR_RGB ( '', 0.40784314, 0.44705882, 0.49803922) ;
#39639 = DIRECTION ( 'NONE',  ( -0.7713892158398705234, 0.000000000000000000, -0.6363636363636357984 ) ) ;
#39640 = ORIENTED_EDGE ( 'NONE', *, *, #28226, .F. ) ;
#39641 = VECTOR ( 'NONE', #40337, 1000.000000000000000 ) ;
#39642 = EDGE_CURVE ( 'NONE', #14417, #42069, #63646, .T. ) ;
#39643 = ORIENTED_EDGE ( 'NONE', *, *, #12286, .F. ) ;
#39644 = DIRECTION ( 'NONE',  ( -0.000000000000000000, -1.000000000000000000, -0.000000000000000000 ) ) ;
#39645 = CARTESIAN_POINT ( 'NONE',  ( 66.74999999999998579, 36.75000000000000000, -3.750000000000000000 ) ) ;
#39646 = CARTESIAN_POINT ( 'NONE',  ( -175.8570736234661638, -5.598654528085803328, -7.705886871421366635 ) ) ;
#39647 = CARTESIAN_POINT ( 'NONE',  ( -75.50000000000000000, -6.499999999999992006, 21.00000000000000000 ) ) ;
#39648 = DIRECTION ( 'NONE',  ( 1.000000000000000000, 0.000000000000000000, 0.000000000000000000 ) ) ;
#39649 =( BOUNDED_CURVE ( )  B_SPLINE_CURVE ( 2, ( #19224, #35778, #56171, #24497, #8701, #51604, #1952, #29445, #3364, #61441, #18208 ),
 .UNSPECIFIED., .F., .F. ) 
 B_SPLINE_CURVE_WITH_KNOTS ( ( 3, 2, 2, 2, 2, 3 ),
 ( 0.8804347826086956763, 0.8826086956521739246, 0.8847826086956521729, 0.8869565217391304213, 0.8891304347826086696, 0.8913043478260869179 ),
 .UNSPECIFIED. ) 
 CURVE ( )  GEOMETRIC_REPRESENTATION_ITEM ( )  RATIONAL_B_SPLINE_CURVE ( ( 1.000000000000000000, 0.9510565162951535312, 1.000000000000000000, 0.9510565162951535312, 1.000000000000000000, 0.9510565162951535312, 1.000000000000000000, 0.9510565162951535312, 1.000000000000000000, 0.9510565162951535312, 1.000000000000000000 ) ) 
 REPRESENTATION_ITEM ( '' )  );
#39650 = CARTESIAN_POINT ( 'NONE',  ( -108.9570736234661723, 9.058813317711329915, -2.943386871421373119 ) ) ;
#39651 = EDGE_CURVE ( 'NONE', #69192, #56560, #51250, .T. ) ;
#39652 = LINE ( 'NONE', #17831, #2067 ) ;
#39653 = ORIENTED_EDGE ( 'NONE', *, *, #53158, .F. ) ;
#39654 = STYLED_ITEM ( 'NONE', ( #30960 ), #24930 ) ;
#39655 = CARTESIAN_POINT ( 'NONE',  ( -65.49999999999997158, -2.024042244987997205E-14, -12.00000000000000000 ) ) ;
#39656 = DIRECTION ( 'NONE',  ( 0.000000000000000000, 1.000000000000000000, -0.000000000000000000 ) ) ;
#39657 = ORIENTED_EDGE ( 'NONE', *, *, #50296, .T. ) ;
#39658 = EDGE_CURVE ( 'NONE', #11473, #68610, #64709, .T. ) ;
#39659 = CARTESIAN_POINT ( 'NONE',  ( -155.6049999999999329, 6.826472737025113702, -4.959722759717902107 ) ) ;
#39660 = CARTESIAN_POINT ( 'NONE',  ( -184.0000000000000000, 0.000000000000000000, 0.000000000000000000 ) ) ;
#39661 = LINE ( 'NONE', #66356, #42643 ) ;
#39662 = CARTESIAN_POINT ( 'NONE',  ( -160.6449999999999818, 4.716976649647091513, -6.492361379858946790 ) ) ;
#39663 = STYLED_ITEM ( 'NONE', ( #4203 ), #47383 ) ;
#39664 = AXIS2_PLACEMENT_3D ( 'NONE', #29802, #68483, #9047 ) ;
#39665 = CARTESIAN_POINT ( 'NONE',  ( -154.6450000000000102, 4.716976649647091513, -6.492361379858946790 ) ) ;
#39666 = ORIENTED_EDGE ( 'NONE', *, *, #67923, .F. ) ;
#39667 = CARTESIAN_POINT ( 'NONE',  ( -84.49999999999997158, 50.00000000000000000, 10.50000000000000000 ) ) ;
#39668 = AXIS2_PLACEMENT_3D ( 'NONE', #64944, #34253, #48475 ) ;
#39669 = CARTESIAN_POINT ( 'NONE',  ( 44.45130529142682008, 9.817101763808558701, 3.473322258837134413 ) ) ;
#39670 = PRESENTATION_STYLE_ASSIGNMENT (( #12903 ) ) ;
#39671 = CARTESIAN_POINT ( 'NONE',  ( -71.90499999999995850, 2.607480562269068880, -8.024999999999993250 ) ) ;
#39672 = CARTESIAN_POINT ( 'NONE',  ( -70.55707362346616662, -1.166476076187852838E-15, -9.524999999999991473 ) ) ;
#39673 = AXIS2_PLACEMENT_3D ( 'NONE', #1117, #54977, #16710 ) ;
#39674 = CARTESIAN_POINT ( 'NONE',  ( 21.75000000000001066, 21.74999999999998224, -3.750000000000000000 ) ) ;
#39675 = ADVANCED_FACE ( 'NONE', ( #15829 ), #16437, .T. ) ;
#39676 = CARTESIAN_POINT ( 'NONE',  ( -68.99499999999999034, -6.826472737025113702, 4.959722759717902107 ) ) ;
#39677 = CARTESIAN_POINT ( 'NONE',  ( 3.094860106618431583, 142.2050000000000125, 9.525000000000000355 ) ) ;
#39678 = DIRECTION ( 'NONE',  ( 1.000000000000000000, 0.000000000000000000, 0.000000000000000000 ) ) ;
#39679 = CIRCLE ( 'NONE', #32933, 16.00000000000000711 ) ;
#39680 = CARTESIAN_POINT ( 'NONE',  ( 4.564701690884894525, 154.3402519334510998, 8.185492600732468205 ) ) ;
#39681 = UNCERTAINTY_MEASURE_WITH_UNIT (LENGTH_MEASURE( 1.000000000000000082E-05 ), #28709, 'distance_accuracy_value', 'NONE');
#39682 = B_SPLINE_CURVE_WITH_KNOTS ( 'NONE', 3,
 ( #46426, #35133, #13673, #36577, #14733, #9809, #14030, #25599 ),
 .UNSPECIFIED., .F., .F.,
 ( 4, 2, 2, 4 ),
 ( 2.544313220892349347E-07, 0.002693395767724533155, 0.004039966435925755432, 0.005386537104126977275 ),
 .UNSPECIFIED. ) ;
#39683 = COLOUR_RGB ( '', 0.72549020, 0.75294118, 0.79215686) ;
#39684 = FILL_AREA_STYLE ('',( #60741 ) ) ;
#39685 = CARTESIAN_POINT ( 'NONE',  ( 0.2500000000000000000, 36.99999999999999289, 3.000000000000000000 ) ) ;
#39686 = DIRECTION ( 'NONE',  ( 0.000000000000000000, -1.000000000000000000, 0.000000000000000000 ) ) ;
#39687 = CARTESIAN_POINT ( 'NONE',  ( 57.00000000000000000, 14.00000000000000000, 80.00402776293826435 ) ) ;
#39688 = AXIS2_PLACEMENT_3D ( 'NONE', #66270, #18096, #60634 ) ;
#39689 = CARTESIAN_POINT ( 'NONE',  ( -119.0929263765346064, 3.094860106632213004, 9.524999999989976374 ) ) ;
#39690 = DIRECTION ( 'NONE',  ( 0.000000000000000000, -2.430666987508117145E-16, 1.000000000000000000 ) ) ;
#39691 = ORIENTED_EDGE ( 'NONE', *, *, #18289, .F. ) ;
#39692 = ORIENTED_EDGE ( 'NONE', *, *, #52660, .T. ) ;
#39693 = EDGE_CURVE ( 'NONE', #19860, #21246, #21416, .T. ) ;
#39694 = CARTESIAN_POINT ( 'NONE',  ( -155.9929263765338021, 8.102448949553172852, -5.886773742842744461 ) ) ;
#39695 = VECTOR ( 'NONE', #27057, 1000.000000000000000 ) ;
#39696 = FILL_AREA_STYLE ('',( #50234 ) ) ;
#39697 = LINE ( 'NONE', #39358, #56574 ) ;
#39698 = FACE_OUTER_BOUND ( 'NONE', #36299, .T. ) ;
#39699 = VERTEX_POINT ( 'NONE', #27709 ) ;
#39700 = CARTESIAN_POINT ( 'NONE',  ( -98.30499999999997840, 8.437984349512086979, -1.550032578732815448E-15 ) ) ;
#39701 = VERTEX_POINT ( 'NONE', #6604 ) ;
#39702 = DIRECTION ( 'NONE',  ( -0.000000000000000000, -1.000000000000000000, -0.000000000000000000 ) ) ;
#39703 = DIRECTION ( 'NONE',  ( 1.000000000000000000, 0.000000000000000000, 0.000000000000000000 ) ) ;
#39704 = ORIENTED_EDGE ( 'NONE', *, *, #12694, .F. ) ;
#39705 = CARTESIAN_POINT ( 'NONE',  ( 8.102448949553183510, 113.1049999999999898, -5.886773742842746238 ) ) ;
#39706 = CARTESIAN_POINT ( 'NONE',  ( 10.00000000000001954, 42.00000000000000000, -28.38386403503541899 ) ) ;
#39707 = ORIENTED_EDGE ( 'NONE', *, *, #20080, .T. ) ;
#39708 = STYLED_ITEM ( 'NONE', ( #9723 ), #48029 ) ;
#39710 = AXIS2_PLACEMENT_3D ( 'NONE', #62953, #57340, #52446 ) ;
#39709 = MECHANICAL_DESIGN_GEOMETRIC_PRESENTATION_REPRESENTATION (  '', ( #11557 ), #50889 ) ;
#39711 = CARTESIAN_POINT ( 'NONE',  ( -34.99999999999999289, 99.99999999999998579, 3.500000000000000000 ) ) ;
#39712 =( LENGTH_UNIT ( ) NAMED_UNIT ( * ) SI_UNIT ( .MILLI., .METRE. ) );
#39713 = CARTESIAN_POINT ( 'NONE',  ( -124.3449999999999847, 7.632228543268599452, -2.479861379858951942 ) ) ;
#39714 = ORIENTED_EDGE ( 'NONE', *, *, #36212, .T. ) ;
#39715 = ORIENTED_EDGE ( 'NONE', *, *, #34163, .F. ) ;
#39716 = APPLICATION_CONTEXT ( 'automotive_design' ) ;
#39717 = CARTESIAN_POINT ( 'NONE',  ( 24.70577775730027881, 26.00000000000004619, -27.50000000000000711 ) ) ;
#39718 = CARTESIAN_POINT ( 'NONE',  ( 0.000000000000000000, 2.299999999999999822, 0.000000000000000000 ) ) ;
#39719 = EDGE_LOOP ( 'NONE', ( #61572, #65719, #11693, #17751, #35711, #4615, #34559, #18359 ) ) ;
#39720 = CARTESIAN_POINT ( 'NONE',  ( 2.607480562269071989, 142.5929263765337680, 8.025000000000002132 ) ) ;
#39721 = DIRECTION ( 'NONE',  ( -1.000000000000000000, 0.000000000000000000, 0.000000000000000000 ) ) ;
#39722 = CARTESIAN_POINT ( 'NONE',  ( 52.75000000000000000, 25.24999999999998579, -3.750000000000000000 ) ) ;
#39723 = CARTESIAN_POINT ( 'NONE',  ( 2.000000000000015543, 26.00000000000000355, 23.99999999999999645 ) ) ;
#39724 = CARTESIAN_POINT ( 'NONE',  ( -15.00000000000000000, 8.000000000000000000, 4.000000000000000000 ) ) ;
#39725 = CIRCLE ( 'NONE', #30693, 10.49999999999999822 ) ;
#39726 = ORIENTED_EDGE ( 'NONE', *, *, #22009, .T. ) ;
#39727 = EDGE_CURVE ( 'NONE', #65467, #48456, #16867, .T. ) ;
#39728 = LINE ( 'NONE', #33714, #8243 ) ;
#39729 = VERTEX_POINT ( 'NONE', #60423 ) ;
#39730 =( LENGTH_UNIT ( ) NAMED_UNIT ( * ) SI_UNIT ( .MILLI., .METRE. ) );
#39731 = SURFACE_STYLE_USAGE ( .BOTH. , #8396 ) ;
#39732 = DIRECTION ( 'NONE',  ( 0.000000000000000000, -1.000000000000000000, 0.000000000000000000 ) ) ;
#39733 = CARTESIAN_POINT ( 'NONE',  ( -158.3070736234661808, -10.01517768586948698, 6.132527647946031529E-16 ) ) ;
#39734 = CARTESIAN_POINT ( 'NONE',  ( -138.2049999999999272, -2.607480562269071545, -8.024999999999991473 ) ) ;
#39735 = AXIS2_PLACEMENT_3D ( 'NONE', #14010, #2341, #56563 ) ;
#39736 = SURFACE_STYLE_USAGE ( .BOTH. , #33390 ) ;
#39737 = LINE ( 'NONE', #7003, #30511 ) ;
#39738 = ORIENTED_EDGE ( 'NONE', *, *, #52310, .F. ) ;
#39739 = CONICAL_SURFACE ( 'NONE', #27325, 8.524999999999977263, 0.7853981633974552734 ) ;
#39740 = CARTESIAN_POINT ( 'NONE',  ( 10.99999999999999645, 11.99999999999999289, -4.000000000000000000 ) ) ;
#39741 = CARTESIAN_POINT ( 'NONE',  ( -107.6070736234661638, -8.102448949553174629, 5.886773742842742685 ) ) ;
#39742 = CARTESIAN_POINT ( 'NONE',  ( -1.233556390955556914, -2.406758536254373748, 6.999999999999999112 ) ) ;
#39743 = ORIENTED_EDGE ( 'NONE', *, *, #60204, .F. ) ;
#39744 = ORIENTED_EDGE ( 'NONE', *, *, #41484, .T. ) ;
#39745 = SURFACE_STYLE_FILL_AREA ( #24216 ) ;
#39746 = VECTOR ( 'NONE', #53869, 1000.000000000000000 ) ;
#39747 = CARTESIAN_POINT ( 'NONE',  ( 41.49999999999998579, 106.9282032302754999, 3.500000000000000000 ) ) ;
#39748 = CARTESIAN_POINT ( 'NONE',  ( -51.80707362346617373, 10.01517768586948698, -1.839758294383808966E-15 ) ) ;
#39749 = CIRCLE ( 'NONE', #36408, 0.5000000000000004441 ) ;
#39750 = CARTESIAN_POINT ( 'NONE',  ( -47.90499999999997272, 2.607480562269068880, -8.024999999999993250 ) ) ;
#39751 = ORIENTED_EDGE ( 'NONE', *, *, #6200, .F. ) ;
#39752 = SURFACE_SIDE_STYLE ('',( #45728 ) ) ;
#39753 = EDGE_CURVE ( 'NONE', #34416, #48755, #1651, .T. ) ;
#39754 = FILL_AREA_STYLE_COLOUR ( '', #33787 ) ;
#39755 = DIRECTION ( 'NONE',  ( -1.000000000000000000, -0.000000000000000000, -0.000000000000000000 ) ) ;
#39756 = EDGE_CURVE ( 'NONE', #34321, #3748, #56872, .T. ) ;
#39757 = LINE ( 'NONE', #22866, #36572 ) ;
#39758 = ORIENTED_EDGE ( 'NONE', *, *, #24101, .F. ) ;
#39759 = VECTOR ( 'NONE', #11159, 1000.000000000000000 ) ;
#39760 = FACE_OUTER_BOUND ( 'NONE', #39596, .T. ) ;
#39761 = COLOUR_RGB ( '', 0.40784314, 0.44705882, 0.49803922) ;
#39762 = EDGE_CURVE ( 'NONE', #4242, #51146, #53870, .T. ) ;
#39763 = CARTESIAN_POINT ( 'NONE',  ( -144.6570736234662036, 9.058813317711329915, 2.943386871421369566 ) ) ;
#39764 = LINE ( 'NONE', #8761, #50 ) ;
#39765 = CARTESIAN_POINT ( 'NONE',  ( -103.7049999999999983, 2.607480562269073321, 8.024999999999991473 ) ) ;
#39766 = CARTESIAN_POINT ( 'NONE',  ( -29.91370621994125756, -7.761720733523188365, -0.7755720678490063413 ) ) ;
#39767 = DIRECTION ( 'NONE',  ( 0.000000000000000000, 0.000000000000000000, 1.000000000000000000 ) ) ;
#39768 = CARTESIAN_POINT ( 'NONE',  ( 45.50000000000000000, -1.469576158976824618E-14, 6.999999999999999112 ) ) ;
#39769 = ADVANCED_FACE ( 'NONE', ( #598 ), #22464, .T. ) ;
#39770 = AXIS2_PLACEMENT_3D ( 'NONE', #61195, #18953, #45749 ) ;
#39771 = CARTESIAN_POINT ( 'NONE',  ( -97.04499999999998749, 7.632228543268600340, 2.479861379858949277 ) ) ;
#39772 = CARTESIAN_POINT ( 'NONE',  ( 0.000000000000000000, 122.5549999999999784, -9.525000000000000355 ) ) ;
#39773 = CARTESIAN_POINT ( 'NONE',  ( -73.49499999999999034, 6.826472737025113702, -4.959722759717902107 ) ) ;
#39774 = SURFACE_STYLE_USAGE ( .BOTH. , #23899 ) ;
#39775 =( GEOMETRIC_REPRESENTATION_CONTEXT ( 3 ) GLOBAL_UNCERTAINTY_ASSIGNED_CONTEXT ( ( #48088 ) ) GLOBAL_UNIT_ASSIGNED_CONTEXT ( ( #1634, #23154, #27353 ) ) REPRESENTATION_CONTEXT ( 'NONE', 'WORKASPACE' ) );
#39776 = MECHANICAL_DESIGN_GEOMETRIC_PRESENTATION_REPRESENTATION (  '', ( #13875 ), #59969 ) ;
#39777 = CARTESIAN_POINT ( 'NONE',  ( 57.00000000000000000, 0.000000000000000000, 65.00402776293825013 ) ) ;
#39778 = UNCERTAINTY_MEASURE_WITH_UNIT (LENGTH_MEASURE( 1.000000000000000082E-05 ), #12068, 'distance_accuracy_value', 'NONE');
#39779 = DIRECTION ( 'NONE',  ( -0.000000000000000000, -0.000000000000000000, 1.000000000000000000 ) ) ;
#39780 = CARTESIAN_POINT ( 'NONE',  ( 1.000000000000000000, 43.00000000000000000, -79.00402776293826435 ) ) ;
#39781 = ORIENTED_EDGE ( 'NONE', *, *, #3307, .F. ) ;
#39782 = CARTESIAN_POINT ( 'NONE',  ( -110.2429263765338021, 5.598654528085804216, 7.705886871421366635 ) ) ;
#39783 = DIRECTION ( 'NONE',  ( 1.000000000000000000, 0.000000000000000000, 0.000000000000000000 ) ) ;
#39784 = CARTESIAN_POINT ( 'NONE',  ( -138.4449999999999932, 0.000000000000000000, 8.024999999999991473 ) ) ;
#39785 = SURFACE_STYLE_USAGE ( .BOTH. , #1359 ) ;
#39786 = CIRCLE ( 'NONE', #49857, 9.000000000000000000 ) ;
#39787 = CARTESIAN_POINT ( 'NONE',  ( -6.062177826491071286, 3.500000000000000888, 0.000000000000000000 ) ) ;
#39788 =( NAMED_UNIT ( * ) PLANE_ANGLE_UNIT ( ) SI_UNIT ( $, .RADIAN. ) );
#39789 = ORIENTED_EDGE ( 'NONE', *, *, #27475, .T. ) ;
#39790 = EDGE_LOOP ( 'NONE', ( #15065, #45620, #31211, #9059 ) ) ;
#39791 = STYLED_ITEM ( 'NONE', ( #23779 ), #36818 ) ;
#39792 = PRESENTATION_STYLE_ASSIGNMENT (( #23566 ) ) ;
#39793 = TOROIDAL_SURFACE ( 'NONE', #38696, 1.000000000000000000, 0.5000000000000000000 ) ;
#39794 = CARTESIAN_POINT ( 'NONE',  ( 0.000000000000000000, 87.30187232391182306, 0.000000000000000000 ) ) ;
#39795 = DIRECTION ( 'NONE',  ( -1.000000000000000000, -0.000000000000000000, -0.000000000000000000 ) ) ;
#39796 = FACE_OUTER_BOUND ( 'NONE', #50835, .T. ) ;
#39798 = AXIS2_PLACEMENT_3D ( 'NONE', #59756, #11221, #32669 ) ;
#39797 = PLANE ( 'NONE',  #25122 ) ;
#39799 = ORIENTED_EDGE ( 'NONE', *, *, #49935, .T. ) ;
#39800 = CARTESIAN_POINT ( 'NONE',  ( -129.8050000000000068, -8.437984349512086979, 5.166775262442717831E-16 ) ) ;
#39801 = VERTEX_POINT ( 'NONE', #33700 ) ;
#39802 = ORIENTED_EDGE ( 'NONE', *, *, #36813, .F. ) ;
#39803 = DIRECTION ( 'NONE',  ( 0.000000000000000000, 0.000000000000000000, -1.000000000000000000 ) ) ;
#39804 = CARTESIAN_POINT ( 'NONE',  ( 48.25000000000000000, 21.99999999999998579, 3.750000000000000000 ) ) ;
#39805 = ORIENTED_EDGE ( 'NONE', *, *, #65686, .F. ) ;
#39806 = DIRECTION ( 'NONE',  ( -1.000000000000000000, 0.000000000000000000, 0.000000000000000000 ) ) ;
#39807 = SURFACE_SIDE_STYLE ('',( #50333 ) ) ;
#39808 = CARTESIAN_POINT ( 'NONE',  ( -1.166476076187854022E-15, 137.9449999999999932, 9.525000000000000355 ) ) ;
#39809 = DIRECTION ( 'NONE',  ( 0.000000000000000000, 0.000000000000000000, 1.000000000000000000 ) ) ;
#39810 =( GEOMETRIC_REPRESENTATION_CONTEXT ( 3 ) GLOBAL_UNCERTAINTY_ASSIGNED_CONTEXT ( ( #46927 ) ) GLOBAL_UNIT_ASSIGNED_CONTEXT ( ( #53646, #59250, #4393 ) ) REPRESENTATION_CONTEXT ( 'NONE', 'WORKASPACE' ) );
#39811 = ORIENTED_EDGE ( 'NONE', *, *, #53170, .F. ) ;
#39812 = VECTOR ( 'NONE', #56389, 1000.000000000000000 ) ;
#39813 = DIRECTION ( 'NONE',  ( 0.000000000000000000, 0.000000000000000000, 1.000000000000000000 ) ) ;
#39814 = CARTESIAN_POINT ( 'NONE',  ( 9.058813317711337021, 136.6550000000000011, 2.943386871421375783 ) ) ;
#39815 = CARTESIAN_POINT ( 'NONE',  ( -51.50499999999999545, -6.826472737025113702, -4.959722759717900331 ) ) ;
#39816 = CARTESIAN_POINT ( 'NONE',  ( -25.00000000000000355, 36.75000000000000000, 3.000000000000000000 ) ) ;
#39817 = ORIENTED_EDGE ( 'NONE', *, *, #47574, .F. ) ;
#39818 = CARTESIAN_POINT ( 'NONE',  ( 3.094860106618435136, 155.4050000000000011, -9.525000000000000355 ) ) ;
#39819 = LINE ( 'NONE', #23942, #37932 ) ;
#39820 = UNCERTAINTY_MEASURE_WITH_UNIT (LENGTH_MEASURE( 1.000000000000000082E-05 ), #34408, 'distance_accuracy_value', 'NONE');
#39821 = LINE ( 'NONE', #23597, #31035 ) ;
#39822 = AXIS2_PLACEMENT_3D ( 'NONE', #54737, #11146, #23430 ) ;
#39823 = SURFACE_STYLE_FILL_AREA ( #55618 ) ;
#39824 = CARTESIAN_POINT ( 'NONE',  ( -15.48999599679679662, 118.4999999999999716, 10.00000000000000000 ) ) ;
#39825 = VERTEX_POINT ( 'NONE', #11906 ) ;
#39826 = EDGE_CURVE ( 'NONE', #23699, #47153, #55714, .T. ) ;
#39827 = DIRECTION ( 'NONE',  ( 0.000000000000000000, 0.000000000000000000, 1.000000000000000000 ) ) ;
#39828 = ORIENTED_EDGE ( 'NONE', *, *, #43453, .T. ) ;
#39829 = CARTESIAN_POINT ( 'NONE',  ( 9.000000000000003553, 25.24999999999998934, -3.750000000000000000 ) ) ;
#39830 = STYLED_ITEM ( 'NONE', ( #62843 ), #61849 ) ;
#39831 = SURFACE_STYLE_FILL_AREA ( #50351 ) ;
#39832 = CARTESIAN_POINT ( 'NONE',  ( -49.16900266361303551, -11.26963036414519337, 3.521240599371135094 ) ) ;
#39833 = CARTESIAN_POINT ( 'NONE',  ( -162.6550000000000011, -7.632228543268600340, -2.479861379858950166 ) ) ;
#39834 = ORIENTED_EDGE ( 'NONE', *, *, #16406, .F. ) ;
#39835 = UNCERTAINTY_MEASURE_WITH_UNIT (LENGTH_MEASURE( 1.000000000000000082E-05 ), #69086, 'distance_accuracy_value', 'NONE');
#39836 = EDGE_CURVE ( 'NONE', #42429, #57245, #61445, .T. ) ;
#39837 = EDGE_CURVE ( 'NONE', #26382, #31359, #54794, .T. ) ;
#39838 =( LENGTH_UNIT ( ) NAMED_UNIT ( * ) SI_UNIT ( .MILLI., .METRE. ) );
#39839 = DIRECTION ( 'NONE',  ( -1.000000000000000000, 0.000000000000000000, 0.000000000000000000 ) ) ;
#39840 = FILL_AREA_STYLE ('',( #27211 ) ) ;
#39841 =( NAMED_UNIT ( * ) SI_UNIT ( $, .STERADIAN. ) SOLID_ANGLE_UNIT ( ) );
#39842 = EDGE_LOOP ( 'NONE', ( #21064, #59050, #53840, #35993 ) ) ;
#39843 = EDGE_CURVE ( 'NONE', #29123, #4364, #55144, .T. ) ;
#39844 = ORIENTED_EDGE ( 'NONE', *, *, #65536, .F. ) ;
#39845 = B_SPLINE_CURVE_WITH_KNOTS ( 'NONE', 3,
 ( #63784, #58177, #51868, #36420, #3618, #62407, #41684, #31075 ),
 .UNSPECIFIED., .F., .F.,
 ( 4, 2, 2, 4 ),
 ( 2.544313220889483728E-07, 0.002693395767724532722, 0.004039966435925754565, 0.005386537104126976408 ),
 .UNSPECIFIED. ) ;
#39846 = FACE_OUTER_BOUND ( 'NONE', #38650, .T. ) ;
#39847 = CARTESIAN_POINT ( 'NONE',  ( -76.85499999999998977, 4.716976649647094177, 6.492361379858945902 ) ) ;
#39849 = EDGE_LOOP ( 'NONE', ( #32650, #1222, #1558, #6685 ) ) ;
#39848 = TOROIDAL_SURFACE ( 'NONE', #64507, 8.499999999999998224, 0.5000000000000000000 ) ;
#39850 = ADVANCED_FACE ( 'NONE', ( #50245 ), #37841, .F. ) ;
#39851 = EDGE_CURVE ( 'NONE', #39384, #35304, #25380, .T. ) ;
#39852 = CIRCLE ( 'NONE', #55570, 14.49999999999999822 ) ;
#39853 = DIRECTION ( 'NONE',  ( 0.000000000000000000, 0.000000000000000000, 1.000000000000000000 ) ) ;
#39854 = AXIS2_PLACEMENT_3D ( 'NONE', #57864, #30750, #51890 ) ;
#39855 = ADVANCED_FACE ( 'NONE', ( #59745 ), #11554, .T. ) ;
#39856 = FACE_OUTER_BOUND ( 'NONE', #27733, .T. ) ;
#39857 = AXIS2_PLACEMENT_3D ( 'NONE', #33757, #33084, #16587 ) ;
#39858 = ORIENTED_EDGE ( 'NONE', *, *, #39693, .F. ) ;
#39859 = CARTESIAN_POINT ( 'NONE',  ( 12.34222745343792127, 115.4999999999999574, -10.18181818181818166 ) ) ;
#39861 = FACE_OUTER_BOUND ( 'NONE', #26224, .T. ) ;
#39860 = CARTESIAN_POINT ( 'NONE',  ( -53.60707362346617089, -8.102448949553174629, 5.886773742842742685 ) ) ;
#39862 = CONICAL_SURFACE ( 'NONE', #57806, 11.99999999999999645, 0.7853981633974552734 ) ;
#39863 = CARTESIAN_POINT ( 'NONE',  ( 9.058813317711337021, 141.5449999999999875, 2.943386871421375783 ) ) ;
#39864 = CARTESIAN_POINT ( 'NONE',  ( -104.0949999999999989, -2.607480562269071545, -8.024999999999991473 ) ) ;
#39865 = DIRECTION ( 'NONE',  ( 0.000000000000000000, 0.000000000000000000, 1.000000000000000000 ) ) ;
#39866 = AXIS2_PLACEMENT_3D ( 'NONE', #36669, #20073, #41235 ) ;
#39868 =( NAMED_UNIT ( * ) PLANE_ANGLE_UNIT ( ) SI_UNIT ( $, .RADIAN. ) );
#39867 = DIRECTION ( 'NONE',  ( 0.000000000000000000, 0.000000000000000000, 1.000000000000000000 ) ) ;
#39869 = AXIS2_PLACEMENT_3D ( 'NONE', #3043, #40773, #67468 ) ;
#39870 = CARTESIAN_POINT ( 'NONE',  ( -142.1929263765337623, -10.01517768586948698, 6.132527647946031529E-16 ) ) ;
#39871 =( NAMED_UNIT ( * ) SI_UNIT ( $, .STERADIAN. ) SOLID_ANGLE_UNIT ( ) );
#39872 = CARTESIAN_POINT ( 'NONE',  ( -170.5450000000000159, -7.632228543268600340, -2.479861379858950166 ) ) ;
#39873 = AXIS2_PLACEMENT_3D ( 'NONE', #54595, #33488, #1423 ) ;
#39874 = DIRECTION ( 'NONE',  ( 0.000000000000000000, 0.000000000000000000, 1.000000000000000000 ) ) ;
#39875 = AXIS2_PLACEMENT_3D ( 'NONE', #49724, #21229, #43104 ) ;
#39876 = AXIS2_PLACEMENT_3D ( 'NONE', #57145, #62762, #40661 ) ;
#39877 = ORIENTED_EDGE ( 'NONE', *, *, #46750, .T. ) ;
#39878 = CARTESIAN_POINT ( 'NONE',  ( -87.50000000000000000, -6.499999999999990230, 3.000000000000000000 ) ) ;
#39879 = ORIENTED_EDGE ( 'NONE', *, *, #29463, .T. ) ;
#39880 =( NAMED_UNIT ( * ) SI_UNIT ( $, .STERADIAN. ) SOLID_ANGLE_UNIT ( ) );
#39881 = EDGE_CURVE ( 'NONE', #61983, #30684, #50582, .T. ) ;
#39882 = PRESENTATION_STYLE_ASSIGNMENT (( #8186 ) ) ;
#39883 = SURFACE_SIDE_STYLE ('',( #66578 ) ) ;
#39884 = DIRECTION ( 'NONE',  ( 0.000000000000000000, 0.000000000000000000, 1.000000000000000000 ) ) ;
#39885 = EDGE_LOOP ( 'NONE', ( #9830, #8414, #7573, #48014 ) ) ;
#39886 = CARTESIAN_POINT ( 'NONE',  ( -162.0550000000000068, -9.827790563157499189E-16, -8.024999999999991473 ) ) ;
#39887 = ORIENTED_EDGE ( 'NONE', *, *, #6279, .F. ) ;
#39888 = CARTESIAN_POINT ( 'NONE',  ( -112.7929263765347088, -3.094860106603506189, 9.525000000010836132 ) ) ;
#39889 = SPHERICAL_SURFACE ( 'NONE', #24165, 0.5000000000000000000 ) ;
#39890 = CARTESIAN_POINT ( 'NONE',  ( -47.50000000000000000, 14.49137674618942562, 10.00000000000000000 ) ) ;
#39891 = CARTESIAN_POINT ( 'NONE',  ( 5.598654528085805993, 114.2449999999999903, 7.705886871421374629 ) ) ;
#39892 = CIRCLE ( 'NONE', #27485, 5.499999999999976907 ) ;
#39893 = VERTEX_POINT ( 'NONE', #50932 ) ;
#39894 = CARTESIAN_POINT ( 'NONE',  ( 3.000000000000030198, 43.00000000000000000, 90.00000000000000000 ) ) ;
#39895 = CARTESIAN_POINT ( 'NONE',  ( 5.598654528085809545, 113.2549999999999812, -7.705886871421373741 ) ) ;
#39896 = CARTESIAN_POINT ( 'NONE',  ( -82.70499999999998408, 2.607480562269072433, 8.024999999999991473 ) ) ;
#39897 = VECTOR ( 'NONE', #46721, 1000.000000000000000 ) ;
#39898 = CARTESIAN_POINT ( 'NONE',  ( 3.094860106618431583, 124.2049999999999841, 9.525000000000000355 ) ) ;
#39899 = UNCERTAINTY_MEASURE_WITH_UNIT (LENGTH_MEASURE( 1.000000000000000082E-05 ), #279, 'distance_accuracy_value', 'NONE');
#39900 = CARTESIAN_POINT ( 'NONE',  ( 6.826472737025121695, 132.6070736234661638, -4.959722759717905660 ) ) ;
#39901 = SURFACE_SIDE_STYLE ('',( #28592 ) ) ;
#39902 = CARTESIAN_POINT ( 'NONE',  ( 20.77895614775982125, 115.1380991538496801, 10.00000000000000000 ) ) ;
#39903 = EDGE_CURVE ( 'NONE', #55259, #24627, #32848, .T. ) ;
#39904 = SURFACE_STYLE_FILL_AREA ( #51733 ) ;
#39905 = DIRECTION ( 'NONE',  ( 1.000000000000000000, 0.000000000000000000, -0.000000000000000000 ) ) ;
#39906 = ORIENTED_EDGE ( 'NONE', *, *, #27155, .T. ) ;
#39907 = PRESENTATION_STYLE_ASSIGNMENT (( #56382 ) ) ;
#39908 = CARTESIAN_POINT ( 'NONE',  ( -55.64499999999997470, 4.716976649647091513, -6.492361379858946790 ) ) ;
#39909 = VERTEX_POINT ( 'NONE', #9066 ) ;
#39910 = DIRECTION ( 'NONE',  ( 0.9704308468600219006, 0.2413793103448194921, -0.000000000000000000 ) ) ;
#39911 = EDGE_CURVE ( 'NONE', #50171, #55963, #68099, .T. ) ;
#39912 = PRESENTATION_LAYER_ASSIGNMENT (  '', '', ( #23011 ) ) ;
#39913 = COLOUR_RGB ( '', 0.40784314, 0.44705882, 0.49803922) ;
#39914 = DIRECTION ( 'NONE',  ( -0.6163733505331072671, 0.000000000000000000, -0.7874540575504017648 ) ) ;
#39915 = CARTESIAN_POINT ( 'NONE',  ( -10.11618306975752368, 54.14354156754873060, -2.000000000000000000 ) ) ;
#39916 = ORIENTED_EDGE ( 'NONE', *, *, #7388, .F. ) ;
#39917 = DIRECTION ( 'NONE',  ( 0.000000000000000000, 0.000000000000000000, 1.000000000000000000 ) ) ;
#39918 = CARTESIAN_POINT ( 'NONE',  ( -51.14499999999999602, -4.716976649647092401, 6.492361379858946790 ) ) ;
#39919 =( LENGTH_UNIT ( ) NAMED_UNIT ( * ) SI_UNIT ( .MILLI., .METRE. ) );
#39920 = EDGE_LOOP ( 'NONE', ( #54199, #25719, #64063, #25145 ) ) ;
#39921 = AXIS2_PLACEMENT_3D ( 'NONE', #11257, #49601, #65423 ) ;
#39922 = CARTESIAN_POINT ( 'NONE',  ( -75.00000000000001421, 8.382277537376792154, 5.549490760430561664 ) ) ;
#39923 = CARTESIAN_POINT ( 'NONE',  ( -107.1549999999999869, 7.632228543268600340, 2.479861379858949277 ) ) ;
#39924 = EDGE_LOOP ( 'NONE', ( #23592, #3135, #2887 ) ) ;
#39925 = CARTESIAN_POINT ( 'NONE',  ( 31.00000000000002132, 42.47058823529412308, 74.11764705882352189 ) ) ;
#39926 = EDGE_CURVE ( 'NONE', #10308, #27268, #7466, .T. ) ;
#39927 = LINE ( 'NONE', #44856, #25231 ) ;
#39928 = CARTESIAN_POINT ( 'NONE',  ( -144.2070736234661865, 3.094860106618433360, 9.524999999999991473 ) ) ;
#39929 = SURFACE_STYLE_FILL_AREA ( #7868 ) ;
#39930 = CARTESIAN_POINT ( 'NONE',  ( 10.01517768586949408, 138.6949999999999932, 1.839758294383810543E-15 ) ) ;
#39931 = CARTESIAN_POINT ( 'NONE',  ( -86.15707362346617515, -9.058813317711329915, -2.943386871421370898 ) ) ;
#39932 = EDGE_CURVE ( 'NONE', #36632, #31059, #57233, .T. ) ;
#39933 = CYLINDRICAL_SURFACE ( 'NONE', #37093, 0.5000000000000004441 ) ;
#39934 = CARTESIAN_POINT ( 'NONE',  ( -28.74999999999999645, -8.499999999999996447, 15.00000000000000178 ) ) ;
#39935 = CARTESIAN_POINT ( 'NONE',  ( 10.00000000000002309, 43.00000000000000000, 74.38749456993816978 ) ) ;
#39937 = SURFACE_STYLE_USAGE ( .BOTH. , #60636 ) ;
#39936 = CARTESIAN_POINT ( 'NONE',  ( 2.607480562269030688, 119.7070736234661581, 8.025000000000034106 ) ) ;
#39938 = CARTESIAN_POINT ( 'NONE',  ( -119.4549999999999983, 7.632228543268599452, -2.479861379858951942 ) ) ;
#39939 = CARTESIAN_POINT ( 'NONE',  ( -159.1429263765338078, 5.598654528085800663, -7.705886871421367523 ) ) ;
#39940 = CARTESIAN_POINT ( 'NONE',  ( 9.058813317711337021, 114.5449999999999733, 2.943386871421375783 ) ) ;
#39941 = CARTESIAN_POINT ( 'NONE',  ( -131.6949999999999932, -8.437984349512085203, 5.166775262442717831E-16 ) ) ;
#39942 = AXIS2_PLACEMENT_3D ( 'NONE', #33806, #34164, #55620 ) ;
#39943 = CARTESIAN_POINT ( 'NONE',  ( -128.0949999999999989, -2.607480562269071545, -8.024999999999991473 ) ) ;
#39944 = LINE ( 'NONE', #27328, #21208 ) ;
#39945 = ORIENTED_EDGE ( 'NONE', *, *, #32139, .T. ) ;
#39946 = STYLED_ITEM ( 'NONE', ( #8880 ), #56478 ) ;
#39947 = CARTESIAN_POINT ( 'NONE',  ( -145.5570736234661808, -1.166476076187852838E-15, -9.524999999999991473 ) ) ;
#39948 = LINE ( 'NONE', #24746, #55953 ) ;
#39949 = FILL_AREA_STYLE ('',( #51171 ) ) ;
#39950 =( GEOMETRIC_REPRESENTATION_CONTEXT ( 3 ) GLOBAL_UNCERTAINTY_ASSIGNED_CONTEXT ( ( #63732 ) ) GLOBAL_UNIT_ASSIGNED_CONTEXT ( ( #15304, #42048, #2921 ) ) REPRESENTATION_CONTEXT ( 'NONE', 'WORKASPACE' ) );
#39951 = CARTESIAN_POINT ( 'NONE',  ( -182.5429263765337851, 9.058813317711329915, 2.943386871421369566 ) ) ;
#39952 =( BOUNDED_CURVE ( )  B_SPLINE_CURVE ( 2, ( #56972, #30213, #51706, #24954, #26332, #37651, #58352, #47157, #59048, #9840, #4528 ),
 .UNSPECIFIED., .F., .F. ) 
 B_SPLINE_CURVE_WITH_KNOTS ( ( 3, 2, 2, 2, 2, 3 ),
 ( 0.7058823529411767383, 0.7117647058823531880, 0.7176470588235296377, 0.7235294117647060874, 0.7294117647058825371, 0.7352941176470590978 ),
 .UNSPECIFIED. ) 
 CURVE ( )  GEOMETRIC_REPRESENTATION_ITEM ( )  RATIONAL_B_SPLINE_CURVE ( ( 0.9999999999999981126, 0.9510565162951554186, 1.000000000000000000, 0.9510565162951535312, 1.000000000000000000, 0.9510565162951535312, 1.000000000000000000, 0.9510565162951535312, 1.000000000000000000, 0.9510565162951516438, 1.000000000000001776 ) ) 
 REPRESENTATION_ITEM ( '' )  );
#39953 = CARTESIAN_POINT ( 'NONE',  ( -53.84499999999997755, -7.632228543268599452, 2.479861379858951054 ) ) ;
#39954 = DIRECTION ( 'NONE',  ( 0.000000000000000000, -1.000000000000000000, 0.000000000000000000 ) ) ;
#39955 = CARTESIAN_POINT ( 'NONE',  ( -21.02379604162863558, 109.9999999999999858, -9.500000000000000000 ) ) ;
#39956 = CARTESIAN_POINT ( 'NONE',  ( -91.79292637653381348, -3.094860106618429807, 9.524999999999991473 ) ) ;
#39957 = APPLICATION_PROTOCOL_DEFINITION ( 'draft international standard', 'automotive_design', 1998, #21288 ) ;
#39958 = CYLINDRICAL_SURFACE ( 'NONE', #59287, 0.9999999999999974465 ) ;
#39959 = MECHANICAL_DESIGN_GEOMETRIC_PRESENTATION_REPRESENTATION (  '', ( #43354 ), #7337 ) ;
#39960 = DIRECTION ( 'NONE',  ( 0.000000000000000000, 0.000000000000000000, 1.000000000000000000 ) ) ;
#39961 = EDGE_CURVE ( 'NONE', #20746, #39066, #34372, .T. ) ;
#39962 = AXIS2_PLACEMENT_3D ( 'NONE', #59687, #26627, #31924 ) ;
#39963 = CARTESIAN_POINT ( 'NONE',  ( -9.827790563157511022E-16, 151.4429263765338192, 8.025000000000000355 ) ) ;
#39964 = SURFACE_SIDE_STYLE ('',( #50485 ) ) ;
#39965 = CYLINDRICAL_SURFACE ( 'NONE', #47134, 9.524999999999991473 ) ;
#39966 = STYLED_ITEM ( 'NONE', ( #51424 ), #64125 ) ;
#39967 = ORIENTED_EDGE ( 'NONE', *, *, #17022, .F. ) ;
#39968 = SURFACE_STYLE_USAGE ( .BOTH. , #33949 ) ;
#39969 = LINE ( 'NONE', #61372, #60957 ) ;
#39971 = VERTEX_POINT ( 'NONE', #2688 ) ;
#39970 = AXIS2_PLACEMENT_3D ( 'NONE', #31532, #53685, #69518 ) ;
#39972 = CARTESIAN_POINT ( 'NONE',  ( -6.826472737025120807, 133.5070736234661410, -4.959722759717907437 ) ) ;
#39973 = AXIS2_PLACEMENT_3D ( 'NONE', #43910, #59008, #44264 ) ;
#39974 = CARTESIAN_POINT ( 'NONE',  ( -8.437984349512095861, 124.8070736234661382, -5.166775262442723748E-16 ) ) ;
#39975 = PRODUCT_RELATED_PRODUCT_CATEGORY ( 'part', '', ( #54094 ) ) ;
#39976 = EDGE_CURVE ( 'NONE', #69112, #31733, #55762, .T. ) ;
#39977 = PRESENTATION_STYLE_ASSIGNMENT (( #30061 ) ) ;
#39978 = LINE ( 'NONE', #51529, #41854 ) ;
#39979 = DIRECTION ( 'NONE',  ( -0.000000000000000000, 1.000000000000000000, -0.000000000000000000 ) ) ;
#39980 = ORIENTED_EDGE ( 'NONE', *, *, #49336, .T. ) ;
#39981 = CYLINDRICAL_SURFACE ( 'NONE', #32111, 0.2500000000000002220 ) ;
#39982 = EDGE_CURVE ( 'NONE', #16496, #35564, #5182, .T. ) ;
#39983 = CIRCLE ( 'NONE', #57937, 0.5000000000000004441 ) ;
#39984 = DIRECTION ( 'NONE',  ( -0.000000000000000000, -0.000000000000000000, -1.000000000000000000 ) ) ;
#39985 = EDGE_CURVE ( 'NONE', #9513, #9272, #3020, .T. ) ;
#39986 = DIRECTION ( 'NONE',  ( 0.000000000000000000, 0.000000000000000000, 1.000000000000000000 ) ) ;
#39987 = CARTESIAN_POINT ( 'NONE',  ( 6.516641522221524596, 43.00000000000000711, 28.13388297856903719 ) ) ;
#39988 = CARTESIAN_POINT ( 'NONE',  ( -80.99499999999999034, -6.826472737025115478, 4.959722759717900331 ) ) ;
#39989 = ORIENTED_EDGE ( 'NONE', *, *, #16163, .T. ) ;
#39990 = PRESENTATION_LAYER_ASSIGNMENT (  '', '', ( #17486 ) ) ;
#39991 = FILL_AREA_STYLE_COLOUR ( '', #54679 ) ;
#39992 = CARTESIAN_POINT ( 'NONE',  ( 22.00000000000002132, 50.00000000000000000, 65.00000000000000000 ) ) ;
#39993 = EDGE_CURVE ( 'NONE', #6265, #8139, #35087, .T. ) ;
#39994 = FACE_OUTER_BOUND ( 'NONE', #22974, .T. ) ;
#39995 = AXIS2_PLACEMENT_3D ( 'NONE', #49354, #34210, #28194 ) ;
#39996 = EDGE_LOOP ( 'NONE', ( #22191, #14795, #22249, #55936 ) ) ;
#39997 = CARTESIAN_POINT ( 'NONE',  ( -76.64292637653380780, -5.598654528085801552, 7.705886871421367523 ) ) ;
#39998 = EDGE_CURVE ( 'NONE', #17419, #26003, #30135, .T. ) ;
#39999 = FACE_OUTER_BOUND ( 'NONE', #16948, .T. ) ;
#40000 = ORIENTED_EDGE ( 'NONE', *, *, #47980, .T. ) ;
#40001 = DIRECTION ( 'NONE',  ( 0.000000000000000000, 0.000000000000000000, -1.000000000000000000 ) ) ;
#40002 = EDGE_LOOP ( 'NONE', ( #3911, #49080, #65647, #41184 ) ) ;
#40003 = CARTESIAN_POINT ( 'NONE',  ( -137.8429263765337964, 9.058813317711329915, -2.943386871421373119 ) ) ;
#40004 = EDGE_CURVE ( 'NONE', #34188, #18052, #52378, .T. ) ;
#40005 = SURFACE_STYLE_FILL_AREA ( #56482 ) ;
#40006 = PRESENTATION_STYLE_ASSIGNMENT (( #23106 ) ) ;
#40007 = FILL_AREA_STYLE_COLOUR ( '', #22100 ) ;
#40008 = CARTESIAN_POINT ( 'NONE',  ( -179.1570736234662036, -9.058813317711329915, -2.943386871421370898 ) ) ;
#40009 = CARTESIAN_POINT ( 'NONE',  ( -18.25000000000000711, 33.74999999999999289, 3.750000000000000000 ) ) ;
#40010 = CARTESIAN_POINT ( 'NONE',  ( 8.102448949553181734, 111.9949999999999761, -5.886773742842746238 ) ) ;
#40011 = CARTESIAN_POINT ( 'NONE',  ( -115.1070736234661638, 8.102448949553171076, -5.886773742842744461 ) ) ;
#40012 = STYLED_ITEM ( 'NONE', ( #4391 ), #8571 ) ;
#40013 = CARTESIAN_POINT ( 'NONE',  ( -183.0295608176848532, 7.162088766832200193, -6.277019169650422725 ) ) ;
#40014 = EDGE_CURVE ( 'NONE', #65503, #17013, #60235, .T. ) ;
#40015 = CARTESIAN_POINT ( 'NONE',  ( 57.00000000000000000, 14.00000000000000000, -80.00402776293826435 ) ) ;
#40016 = EDGE_LOOP ( 'NONE', ( #10326, #69138, #20424, #23258 ) ) ;
#40017 = CARTESIAN_POINT ( 'NONE',  ( 39.49999999999999289, 16.24999999999997513, -3.750000000000000000 ) ) ;
#40018 = CARTESIAN_POINT ( 'NONE',  ( 45.07697505292422591, 10.02565835097472480, -3.091949714863345910 ) ) ;
#40020 = SURFACE_STYLE_USAGE ( .BOTH. , #18533 ) ;
#40019 = COLOUR_RGB ( '', 0.09019608, 0.27058824, 0.51372549) ;
#40021 = VERTEX_POINT ( 'NONE', #14327 ) ;
#40022 = CARTESIAN_POINT ( 'NONE',  ( -163.1050000000000182, -6.826472737025115478, 4.959722759717900331 ) ) ;
#40023 = DIRECTION ( 'NONE',  ( 0.000000000000000000, 0.000000000000000000, 1.000000000000000000 ) ) ;
#40024 = CARTESIAN_POINT ( 'NONE',  ( -183.7236500287686738, -7.325335938885507048, -4.919193638985903227 ) ) ;
#40025 = CARTESIAN_POINT ( 'NONE',  ( -163.4949999999999761, 6.826472737025113702, -4.959722759717902107 ) ) ;
#40026 = MECHANICAL_DESIGN_GEOMETRIC_PRESENTATION_REPRESENTATION (  '', ( #69216 ), #600 ) ;
#40027 = COLOUR_RGB ( '', 0.08235294, 0.09019608, 0.10196078) ;
#40028 = AXIS2_PLACEMENT_3D ( 'NONE', #43290, #10872, #59373 ) ;
#40029 = CARTESIAN_POINT ( 'NONE',  ( -158.0949999999999989, -2.607480562269071545, -8.024999999999991473 ) ) ;
#40030 = ORIENTED_EDGE ( 'NONE', *, *, #13756, .T. ) ;
#40031 = CARTESIAN_POINT ( 'NONE',  ( -67.49292637653380211, -8.102448949553174629, 5.886773742842742685 ) ) ;
#40032 = CARTESIAN_POINT ( 'NONE',  ( -122.6929263765338050, 10.01517768586948698, -1.839758294383808966E-15 ) ) ;
#40033 = CARTESIAN_POINT ( 'NONE',  ( -70.70499999999996987, 2.607480562269073321, 8.024999999999991473 ) ) ;
#40034 = CARTESIAN_POINT ( 'NONE',  ( -33.89861118948982721, -9.947368421052628307, 2.722470280083841843 ) ) ;
#40035 = CARTESIAN_POINT ( 'NONE',  ( -69.59499999999998465, 2.607480562269072433, 8.024999999999991473 ) ) ;
#40036 = CARTESIAN_POINT ( 'NONE',  ( -10.01517768586949231, 147.3049999999999500, -6.132527647946036459E-16 ) ) ;
#40037 = LINE ( 'NONE', #29429, #18526 ) ;
#40038 = PRESENTATION_LAYER_ASSIGNMENT (  '', '', ( #55720 ) ) ;
#40039 = CARTESIAN_POINT ( 'NONE',  ( -156.0570736234661808, 0.000000000000000000, 9.524999999999991473 ) ) ;
#40040 = MECHANICAL_DESIGN_GEOMETRIC_PRESENTATION_REPRESENTATION (  '', ( #4029 ), #58001 ) ;
#40041 = DIRECTION ( 'NONE',  ( 0.000000000000000000, -0.000000000000000000, -1.000000000000000000 ) ) ;
#40042 = CARTESIAN_POINT ( 'NONE',  ( -19.98523465219084017, 114.9999999999999574, -10.47102667436386625 ) ) ;
#40043 = CARTESIAN_POINT ( 'NONE',  ( 60.00000000000000000, 1.797044900979284448E-15, 10.00000000000000000 ) ) ;
#40044 = PLANE ( 'NONE',  #38349 ) ;
#40045 = B_SPLINE_CURVE_WITH_KNOTS ( 'NONE', 3,
 ( #40018, #61409, #13226, #34683 ),
 .UNSPECIFIED., .F., .F.,
 ( 4, 4 ),
 ( -4.672407068503224980E-06, 0.0001893522667583410015 ),
 .UNSPECIFIED. ) ;
#40046 = CARTESIAN_POINT ( 'NONE',  ( 27.00000000000001776, 43.00000000000000000, -34.49999999999999289 ) ) ;
#40047 = FACE_OUTER_BOUND ( 'NONE', #43149, .T. ) ;
#40048 = VERTEX_POINT ( 'NONE', #35791 ) ;
#40049 = VERTEX_POINT ( 'NONE', #34400 ) ;
#40050 = CARTESIAN_POINT ( 'NONE',  ( -154.9429263765338192, 0.000000000000000000, 9.524999999999991473 ) ) ;
#40051 = CIRCLE ( 'NONE', #9721, 1.000000000000000888 ) ;
#40052 = EDGE_CURVE ( 'NONE', #23279, #35924, #22024, .T. ) ;
#40053 = FACE_OUTER_BOUND ( 'NONE', #6950, .T. ) ;
#40054 = CARTESIAN_POINT ( 'NONE',  ( 5.365183871890743639, -4.707228941936128841, 0.1074872947962652175 ) ) ;
#40055 = EDGE_CURVE ( 'NONE', #41886, #4261, #29902, .T. ) ;
#40056 = ORIENTED_EDGE ( 'NONE', *, *, #38267, .F. ) ;
#40057 = ORIENTED_EDGE ( 'NONE', *, *, #41772, .F. ) ;
#40058 = LINE ( 'NONE', #13268, #61222 ) ;
#40059 = PRESENTATION_STYLE_ASSIGNMENT (( #57230 ) ) ;
#40060 = EDGE_CURVE ( 'NONE', #57680, #65525, #57083, .T. ) ;
#40061 = ORIENTED_EDGE ( 'NONE', *, *, #4708, .F. ) ;
#40062 = DIRECTION ( 'NONE',  ( 1.000000000000000000, 0.000000000000000000, 0.000000000000000000 ) ) ;
#40063 = DIRECTION ( 'NONE',  ( 7.709882115452441682E-16, -1.000000000000000000, 0.000000000000000000 ) ) ;
#40064 = VECTOR ( 'NONE', #23175, 1000.000000000000000 ) ;
#40065 = EDGE_LOOP ( 'NONE', ( #24618, #27626, #32334, #545 ) ) ;
#40066 = PRESENTATION_LAYER_ASSIGNMENT (  '', '', ( #56902 ) ) ;
#40067 = CARTESIAN_POINT ( 'NONE',  ( -83.45707362346617231, -9.058813317711329915, 2.943386871421371787 ) ) ;
#40068 = DIRECTION ( 'NONE',  ( -0.8660254037844384856, -0.5000000000000004441, 0.000000000000000000 ) ) ;
#40069 = CARTESIAN_POINT ( 'NONE',  ( -112.6449999999999960, 4.716976649647091513, -6.492361379858946790 ) ) ;
#40070 = ORIENTED_EDGE ( 'NONE', *, *, #58912, .F. ) ;
#40071 =( BOUNDED_SURFACE ( )  B_SPLINE_SURFACE ( 3, 2, ( 
 ( #28626, #22680, #1849 ),
 ( #44183, #17431, #38899 ),
 ( #60302, #12106, #55006 ),
 ( #6834, #23032, #44529 ) ),
 .UNSPECIFIED., .F., .F., .F. ) 
 B_SPLINE_SURFACE_WITH_KNOTS ( ( 4, 4 ),
 ( 3, 3 ),
 ( 8.673617379884035472E-19, 0.002371732043478174713 ),
 ( 0.000000000000000000, 1.000000000000000000 ),
 .UNSPECIFIED. ) 
 GEOMETRIC_REPRESENTATION_ITEM ( )  RATIONAL_B_SPLINE_SURFACE ( (
 ( 1.000000000000000000, 0.9473232638932230776, 1.000000000000000000),
 ( 1.000000000000000000, 0.9785952379394217138, 1.000000000000000000),
 ( 1.000000000000000000, 1.000279878396956645, 1.000000000000000000),
 ( 1.000000000000000000, 1.000000000000000000, 1.000000000000000000) ) ) 
 REPRESENTATION_ITEM ( '' )  SURFACE ( )  );
#40072 = ORIENTED_EDGE ( 'NONE', *, *, #6942, .T. ) ;
#40073 = CARTESIAN_POINT ( 'NONE',  ( -0.2278693232858663154, 2.499999999999997780, 9.000000000000003553 ) ) ;
#40074 = CARTESIAN_POINT ( 'NONE',  ( -54.44292637653380496, -1.166476076187852838E-15, -9.524999999999991473 ) ) ;
#40075 = CARTESIAN_POINT ( 'NONE',  ( 24.70577775730027881, 26.17803040854050778, -27.50000000000000711 ) ) ;
#40076 = DIRECTION ( 'NONE',  ( 0.000000000000000000, 0.000000000000000000, 1.000000000000000000 ) ) ;
#40077 = ORIENTED_EDGE ( 'NONE', *, *, #55047, .F. ) ;
#40078 = CARTESIAN_POINT ( 'NONE',  ( -2.607480562269075097, 142.2929263765338135, 8.025000000000000355 ) ) ;
#40079 = LINE ( 'NONE', #56197, #22173 ) ;
#40080 = EDGE_CURVE ( 'NONE', #29086, #47020, #42827, .T. ) ;
#40081 = VECTOR ( 'NONE', #46302, 1000.000000000000000 ) ;
#40082 = VERTEX_POINT ( 'NONE', #69198 ) ;
#40083 = ORIENTED_EDGE ( 'NONE', *, *, #11882, .T. ) ;
#40084 = DIRECTION ( 'NONE',  ( 0.000000000000000000, 0.000000000000000000, 1.000000000000000000 ) ) ;
#40085 = CARTESIAN_POINT ( 'NONE',  ( -135.9549999999999841, -7.632228543268599452, 2.479861379858951054 ) ) ;
#40086 = PRESENTATION_STYLE_ASSIGNMENT (( #39736 ) ) ;
#40087 = DIRECTION ( 'NONE',  ( -0.7071067811865549002, 0.000000000000000000, -0.7071067811865402453 ) ) ;
#40088 = ORIENTED_EDGE ( 'NONE', *, *, #59734, .F. ) ;
#40089 =( LENGTH_UNIT ( ) NAMED_UNIT ( * ) SI_UNIT ( .MILLI., .METRE. ) );
#40090 = DIRECTION ( 'NONE',  ( 0.6842105263157866046, -0.7292845505553195995, 0.000000000000000000 ) ) ;
#40091 = DIRECTION ( 'NONE',  ( 1.000000000000000000, 0.000000000000000000, 0.000000000000000000 ) ) ;
#40092 = ORIENTED_EDGE ( 'NONE', *, *, #33291, .F. ) ;
#40093 = ORIENTED_EDGE ( 'NONE', *, *, #11903, .T. ) ;
#40094 = CARTESIAN_POINT ( 'NONE',  ( -24.21231517720798010, 112.9999999999999858, -10.00000000000000000 ) ) ;
#40095 = CARTESIAN_POINT ( 'NONE',  ( -30.87808905615140276, -8.491754569869277347, -1.062615821289257356 ) ) ;
#40096 = LINE ( 'NONE', #57630, #55888 ) ;
#40097 = CARTESIAN_POINT ( 'NONE',  ( 0.000000000000000000, -2.500000000000000000, 0.000000000000000000 ) ) ;
#40098 = ORIENTED_EDGE ( 'NONE', *, *, #31448, .F. ) ;
#40099 =( NAMED_UNIT ( * ) PLANE_ANGLE_UNIT ( ) SI_UNIT ( $, .RADIAN. ) );
#40100 = PRESENTATION_STYLE_ASSIGNMENT (( #60136 ) ) ;
#40101 = EDGE_CURVE ( 'NONE', #28347, #2934, #47075, .T. ) ;
#40102 = DIRECTION ( 'NONE',  ( 0.000000000000000000, 0.000000000000000000, 1.000000000000000000 ) ) ;
#40103 = CARTESIAN_POINT ( 'NONE',  ( -53.60707362346617089, -8.102448949553172852, 5.886773742842742685 ) ) ;
#40104 = CARTESIAN_POINT ( 'NONE',  ( -182.3950000000000102, -6.826472737025113702, -4.959722759717900331 ) ) ;
#40105 = EDGE_CURVE ( 'NONE', #40506, #3770, #25560, .T. ) ;
#40106 = DIRECTION ( 'NONE',  ( -0.000000000000000000, -0.000000000000000000, 1.000000000000000000 ) ) ;
#40107 = ORIENTED_EDGE ( 'NONE', *, *, #14463, .F. ) ;
#40108 = CARTESIAN_POINT ( 'NONE',  ( -161.0070736234661410, -8.102448949553174629, -5.886773742842741797 ) ) ;
#40109 = DIRECTION ( 'NONE',  ( 0.000000000000000000, -1.000000000000000000, 0.000000000000000000 ) ) ;
#40110 = CARTESIAN_POINT ( 'NONE',  ( -88.55707362346616662, -1.166476076187852838E-15, -9.524999999999991473 ) ) ;
#40111 = CARTESIAN_POINT ( 'NONE',  ( -103.4049999999999869, -2.607480562269069768, 8.024999999999991473 ) ) ;
#40112 = CARTESIAN_POINT ( 'NONE',  ( -57.11974195712093660, -8.499999999999992895, 0.06931351858119066955 ) ) ;
#40113 = FILL_AREA_STYLE_COLOUR ( '', #4453 ) ;
#40114 = FILL_AREA_STYLE ('',( #18635 ) ) ;
#40115 = CIRCLE ( 'NONE', #24342, 8.525000000000000355 ) ;
#40116 = CARTESIAN_POINT ( 'NONE',  ( -100.3449999999999847, 7.632228543268599452, -2.479861379858951942 ) ) ;
#40117 = CARTESIAN_POINT ( 'NONE',  ( 5.598654528085809545, 116.2549999999999812, -7.705886871421373741 ) ) ;
#40118 = CARTESIAN_POINT ( 'NONE',  ( -77.24499999999997613, -4.716976649647093289, -6.492361379858945902 ) ) ;
#40119 = CARTESIAN_POINT ( 'NONE',  ( 31.00000000000000711, -60.04052944165106709, -36.50000000000000000 ) ) ;
#40120 =( GEOMETRIC_REPRESENTATION_CONTEXT ( 3 ) GLOBAL_UNCERTAINTY_ASSIGNED_CONTEXT ( ( #64398 ) ) GLOBAL_UNIT_ASSIGNED_CONTEXT ( ( #15169, #67920, #51735 ) ) REPRESENTATION_CONTEXT ( 'NONE', 'WORKASPACE' ) );
#40121 = DIRECTION ( 'NONE',  ( 1.000000000000000000, -1.445602896647339656E-16, 0.000000000000000000 ) ) ;
#40122 = CYLINDRICAL_SURFACE ( 'NONE', #49479, 0.5000000000000004441 ) ;
#40123 = CARTESIAN_POINT ( 'NONE',  ( 71.62068965517239860, 36.41396814395972115, 7.500000000000000000 ) ) ;
#40124 = EDGE_LOOP ( 'NONE', ( #4386, #62142, #39216, #16454 ) ) ;
#40125 = CARTESIAN_POINT ( 'NONE',  ( -115.0429263765338135, -9.058813317711329915, -2.943386871421370898 ) ) ;
#40126 = CARTESIAN_POINT ( 'NONE',  ( -138.8949999999999534, 6.826472737025116366, 4.959722759717898555 ) ) ;
#40127 = FILL_AREA_STYLE ('',( #7727 ) ) ;
#40128 = AXIS2_PLACEMENT_3D ( 'NONE', #54891, #28510, #60198 ) ;
#40129 = DIRECTION ( 'NONE',  ( 0.000000000000000000, 0.000000000000000000, 1.000000000000000000 ) ) ;
#40130 = ADVANCED_FACE ( 'NONE', ( #19945 ), #41239, .F. ) ;
#40131 =( LENGTH_UNIT ( ) NAMED_UNIT ( * ) SI_UNIT ( .MILLI., .METRE. ) );
#40132 = ORIENTED_EDGE ( 'NONE', *, *, #1504, .F. ) ;
#40133 = ORIENTED_EDGE ( 'NONE', *, *, #49380, .F. ) ;
#40134 = CARTESIAN_POINT ( 'NONE',  ( -24.21231517720798010, 113.4999999999999858, -7.500000000000000000 ) ) ;
#40135 = CARTESIAN_POINT ( 'NONE',  ( -62.84292637653379643, 9.058813317711329915, -2.943386871421373119 ) ) ;
#40136 = DIRECTION ( 'NONE',  ( -0.000000000000000000, 1.000000000000000000, -0.000000000000000000 ) ) ;
#40137 = CARTESIAN_POINT ( 'NONE',  ( 18.25000000000000711, 31.24999999999999289, -4.000000000000000000 ) ) ;
#40138 = DIRECTION ( 'NONE',  ( 0.000000000000000000, 0.000000000000000000, -1.000000000000000000 ) ) ;
#40139 =( NAMED_UNIT ( * ) PLANE_ANGLE_UNIT ( ) SI_UNIT ( $, .RADIAN. ) );
#40140 = VERTEX_POINT ( 'NONE', #20658 ) ;
#40141 = CARTESIAN_POINT ( 'NONE',  ( -135.6550000000000011, -7.632228543268600340, -2.479861379858950166 ) ) ;
#40142 = ORIENTED_EDGE ( 'NONE', *, *, #47874, .F. ) ;
#40143 = ADVANCED_FACE ( 'NONE', ( #64243 ), #10793, .F. ) ;
#40144 = VERTEX_POINT ( 'NONE', #32241 ) ;
#40145 = CARTESIAN_POINT ( 'NONE',  ( -16.75000000000000000, -3.000000000000000000, 24.00000000000000000 ) ) ;
#40146 = ORIENTED_EDGE ( 'NONE', *, *, #55186, .F. ) ;
#40147 = SURFACE_STYLE_FILL_AREA ( #14688 ) ;
#40148 =( NAMED_UNIT ( * ) PLANE_ANGLE_UNIT ( ) SI_UNIT ( $, .RADIAN. ) );
#40149 = CARTESIAN_POINT ( 'NONE',  ( 9.058813317711337021, 135.5449999999999875, 2.943386871421375783 ) ) ;
#40150 = DIRECTION ( 'NONE',  ( -0.000000000000000000, -0.000000000000000000, 1.000000000000000000 ) ) ;
#40151 = ORIENTED_EDGE ( 'NONE', *, *, #26984, .T. ) ;
#40152 = CYLINDRICAL_SURFACE ( 'NONE', #43190, 0.5000000000000004441 ) ;
#40153 = CARTESIAN_POINT ( 'NONE',  ( 5.598654528085809545, 143.2549999999999955, -7.705886871421373741 ) ) ;
#40154 = CARTESIAN_POINT ( 'NONE',  ( -49.55499999999998550, 0.000000000000000000, 8.024999999999991473 ) ) ;
#40155 = DIRECTION ( 'NONE',  ( 0.000000000000000000, -0.000000000000000000, -1.000000000000000000 ) ) ;
#40156 = VERTEX_POINT ( 'NONE', #15738 ) ;
#40157 = CARTESIAN_POINT ( 'NONE',  ( 0.000000000000000000, 116.9429263765338192, -8.025000000000000355 ) ) ;
#40158 = FACE_OUTER_BOUND ( 'NONE', #68433, .T. ) ;
#40159 = PRESENTATION_STYLE_ASSIGNMENT (( #28861 ) ) ;
#40160 = EDGE_CURVE ( 'NONE', #34731, #24720, #56911, .T. ) ;
#40161 = PRESENTATION_STYLE_ASSIGNMENT (( #23946 ) ) ;
#40162 = FACE_OUTER_BOUND ( 'NONE', #18575, .T. ) ;
#40163 = VERTEX_POINT ( 'NONE', #23085 ) ;
#40164 = CARTESIAN_POINT ( 'NONE',  ( -0.2274700367024034831, -9.000000000000007105, -1.732394135371857768E-15 ) ) ;
#40165 = EDGE_LOOP ( 'NONE', ( #64800, #5000, #24636, #33063, #6273, #50270, #59830, #62594, #7742, #21150, #14818, #19287, #22816, #52869, #33529, #18009, #38002, #21417, #39527 ) ) ;
#40166 = DIRECTION ( 'NONE',  ( -0.000000000000000000, 1.000000000000000000, -0.000000000000000000 ) ) ;
#40167 = DIRECTION ( 'NONE',  ( 1.000000000000000000, 0.000000000000000000, 0.000000000000000000 ) ) ;
#40168 = CARTESIAN_POINT ( 'NONE',  ( -158.9050000000000011, 2.607480562269068880, -8.024999999999993250 ) ) ;
#40169 = ORIENTED_EDGE ( 'NONE', *, *, #1038, .T. ) ;
#40170 = CARTESIAN_POINT ( 'NONE',  ( 45.50000000000000000, -1.469576158976824618E-14, -9.500000000000000000 ) ) ;
#40171 = FACE_OUTER_BOUND ( 'NONE', #47321, .T. ) ;
#40172 = CARTESIAN_POINT ( 'NONE',  ( 9.250000000000003553, 27.74999999999998934, -4.000000000000000000 ) ) ;
#40173 = ORIENTED_EDGE ( 'NONE', *, *, #20275, .T. ) ;
#40174 = VERTEX_POINT ( 'NONE', #49472 ) ;
#40175 = CARTESIAN_POINT ( 'NONE',  ( 48.74999999999999289, 24.74999999999998579, 3.750000000000000000 ) ) ;
#40176 = CARTESIAN_POINT ( 'NONE',  ( 60.00000000000000000, 1.797044900979284448E-15, -6.500000000000000000 ) ) ;
#40177 = CARTESIAN_POINT ( 'NONE',  ( -72.50499999999998124, -6.826472737025115478, -4.959722759717899443 ) ) ;
#40178 = VERTEX_POINT ( 'NONE', #43544 ) ;
#40179 = FILL_AREA_STYLE ('',( #2460 ) ) ;
#40180 = CARTESIAN_POINT ( 'NONE',  ( -63.95707362346617231, 9.058813317711329915, -2.943386871421373119 ) ) ;
#40181 =( NAMED_UNIT ( * ) SI_UNIT ( $, .STERADIAN. ) SOLID_ANGLE_UNIT ( ) );
#40182 = CARTESIAN_POINT ( 'NONE',  ( -75.00000000000000000, 8.456227461324047567, -6.943431694471518867 ) ) ;
#40183 = ORIENTED_EDGE ( 'NONE', *, *, #23603, .F. ) ;
#40185 = SURFACE_STYLE_USAGE ( .BOTH. , #13778 ) ;
#40184 = DIRECTION ( 'NONE',  ( 1.156482317317873451E-16, -1.000000000000000000, 0.000000000000000000 ) ) ;
#40186 = CARTESIAN_POINT ( 'NONE',  ( 8.102448949553181734, 138.3950000000000102, 5.886773742842750679 ) ) ;
#40187 = CARTESIAN_POINT ( 'NONE',  ( -105.4449999999999790, 0.000000000000000000, 8.024999999999991473 ) ) ;
#40188 = DIRECTION ( 'NONE',  ( -0.7071067811865487940, 0.000000000000000000, 0.7071067811865463515 ) ) ;
#40189 = PLANE ( 'NONE',  #41583 ) ;
#40190 = LINE ( 'NONE', #56336, #62662 ) ;
#40191 = CARTESIAN_POINT ( 'NONE',  ( -145.9429263765337907, 0.000000000000000000, 9.524999999999991473 ) ) ;
#40192 = SURFACE_STYLE_USAGE ( .BOTH. , #56339 ) ;
#40193 = CARTESIAN_POINT ( 'NONE',  ( -162.8949999999999534, 6.826472737025116366, 4.959722759717898555 ) ) ;
#40194 = CIRCLE ( 'NONE', #9864, 0.5000000000000004441 ) ;
#40195 = VECTOR ( 'NONE', #24218, 1000.000000000000000 ) ;
#40196 = PRESENTATION_LAYER_ASSIGNMENT (  '', '', ( #4193 ) ) ;
#40197 = SURFACE_STYLE_USAGE ( .BOTH. , #8531 ) ;
#40198 = EDGE_CURVE ( 'NONE', #65770, #9058, #65900, .T. ) ;
#40199 = FACE_OUTER_BOUND ( 'NONE', #53436, .T. ) ;
#40200 = ORIENTED_EDGE ( 'NONE', *, *, #1377, .F. ) ;
#40201 = DIRECTION ( 'NONE',  ( -0.000000000000000000, 1.000000000000000000, -0.000000000000000000 ) ) ;
#40202 = VERTEX_POINT ( 'NONE', #59294 ) ;
#40204 = EDGE_CURVE ( 'NONE', #12261, #50231, #51292, .T. ) ;
#40203 = FILL_AREA_STYLE_COLOUR ( '', #3753 ) ;
#40205 = SURFACE_STYLE_FILL_AREA ( #29971 ) ;
#40206 = DIRECTION ( 'NONE',  ( 0.000000000000000000, -1.000000000000000000, 0.000000000000000000 ) ) ;
#40207 = DIRECTION ( 'NONE',  ( -1.445602896647337931E-16, 1.000000000000000000, 0.000000000000000000 ) ) ;
#40208 = CIRCLE ( 'NONE', #57015, 0.2500000000000002220 ) ;
#40209 = EDGE_CURVE ( 'NONE', #62740, #26681, #19850, .T. ) ;
#40210 = CYLINDRICAL_SURFACE ( 'NONE', #59990, 0.2500000000000002220 ) ;
#40211 = AXIS2_PLACEMENT_3D ( 'NONE', #41377, #53629, #63827 ) ;
#40212 = ORIENTED_EDGE ( 'NONE', *, *, #68979, .F. ) ;
#40213 = CARTESIAN_POINT ( 'NONE',  ( -158.7549999999999670, 4.716976649647091513, -6.492361379858946790 ) ) ;
#40214 = EDGE_CURVE ( 'NONE', #55377, #35021, #52427, .T. ) ;
#40215 = ORIENTED_EDGE ( 'NONE', *, *, #1693, .F. ) ;
#40216 = CARTESIAN_POINT ( 'NONE',  ( 0.000000000000000000, 114.4999999999999574, 0.000000000000000000 ) ) ;
#40217 = DIRECTION ( 'NONE',  ( 1.000000000000000000, 0.000000000000000000, 0.000000000000000000 ) ) ;
#40219 = ORIENTED_EDGE ( 'NONE', *, *, #25746, .T. ) ;
#40218 = ADVANCED_FACE ( 'NONE', ( #60347 ), #12154, .T. ) ;
#40220 = SURFACE_STYLE_FILL_AREA ( #13450 ) ;
#40221 = EDGE_CURVE ( 'NONE', #9855, #16376, #17137, .T. ) ;
#40222 = CARTESIAN_POINT ( 'NONE',  ( 0.000000000000000000, 109.4449999999999932, -9.525000000000000355 ) ) ;
#40223 = ORIENTED_EDGE ( 'NONE', *, *, #20702, .F. ) ;
#40225 = ADVANCED_FACE ( 'NONE', ( #28316 ), #26926, .T. ) ;
#40224 = CARTESIAN_POINT ( 'NONE',  ( -3.094860106618434248, 114.9049999999999727, 9.525000000000000355 ) ) ;
#40226 = CARTESIAN_POINT ( 'NONE',  ( -77.15499999999998693, 7.632228543268600340, 2.479861379858949277 ) ) ;
#40227 = DIRECTION ( 'NONE',  ( 0.000000000000000000, 1.000000000000000000, 0.000000000000000000 ) ) ;
#40228 = CARTESIAN_POINT ( 'NONE',  ( 5.598654528085805993, 136.3550000000000182, 7.705886871421374629 ) ) ;
#40229 = DIRECTION ( 'NONE',  ( 0.000000000000000000, 0.000000000000000000, -1.000000000000000000 ) ) ;
#40230 =( NAMED_UNIT ( * ) SI_UNIT ( $, .STERADIAN. ) SOLID_ANGLE_UNIT ( ) );
#40231 =( NAMED_UNIT ( * ) PLANE_ANGLE_UNIT ( ) SI_UNIT ( $, .RADIAN. ) );
#40232 = PRESENTATION_STYLE_ASSIGNMENT (( #29293 ) ) ;
#40233 = VERTEX_POINT ( 'NONE', #54715 ) ;
#40234 = SURFACE_SIDE_STYLE ('',( #18756 ) ) ;
#40235 = CARTESIAN_POINT ( 'NONE',  ( -51.44499999999999318, 0.000000000000000000, 8.024999999999991473 ) ) ;
#40236 = VERTEX_POINT ( 'NONE', #54376 ) ;
#40237 = LINE ( 'NONE', #34940, #60907 ) ;
#40238 = CARTESIAN_POINT ( 'NONE',  ( -184.0000000000000000, 0.000000000000000000, -8.524999999999977263 ) ) ;
#40239 = CARTESIAN_POINT ( 'NONE',  ( -45.00000000000000000, 7.951225523244941584, -6.457238017239539829 ) ) ;
#40240 = VECTOR ( 'NONE', #9207, 1000.000000000000000 ) ;
#40241 = ORIENTED_EDGE ( 'NONE', *, *, #65758, .F. ) ;
#40242 = CARTESIAN_POINT ( 'NONE',  ( -51.84221223720477667, -9.947368421052628307, 4.481646853389227303 ) ) ;
#40243 = CARTESIAN_POINT ( 'NONE',  ( -49.49499999999997613, 6.826472737025113702, -4.959722759717902107 ) ) ;
#40244 = VERTEX_POINT ( 'NONE', #27276 ) ;
#40245 = AXIS2_PLACEMENT_3D ( 'NONE', #29772, #45973, #56139 ) ;
#40246 = FILL_AREA_STYLE ('',( #8578 ) ) ;
#40247 = CARTESIAN_POINT ( 'NONE',  ( -103.1049999999999756, -6.826472737025115478, 4.959722759717900331 ) ) ;
#40248 = ORIENTED_EDGE ( 'NONE', *, *, #4675, .T. ) ;
#40249 = CARTESIAN_POINT ( 'NONE',  ( 9.250000000000003553, 25.24999999999998934, 4.000000000000000000 ) ) ;
#40250 = SURFACE_SIDE_STYLE ('',( #3236 ) ) ;
#40251 = PRESENTATION_LAYER_ASSIGNMENT (  '', '', ( #50332 ) ) ;
#40252 = CARTESIAN_POINT ( 'NONE',  ( -143.4570736234661865, -9.058813317711329915, 2.943386871421371787 ) ) ;
#40253 = FACE_OUTER_BOUND ( 'NONE', #6873, .T. ) ;
#40254 = CARTESIAN_POINT ( 'NONE',  ( -8.102448949553179958, 143.4949999999999477, 5.886773742842747126 ) ) ;
#40255 = CARTESIAN_POINT ( 'NONE',  ( -89.30707362346616662, -10.01517768586948698, 6.132527647946031529E-16 ) ) ;
#40256 = FACE_OUTER_BOUND ( 'NONE', #37605, .T. ) ;
#40257 = DIRECTION ( 'NONE',  ( -0.000000000000000000, -0.000000000000000000, 1.000000000000000000 ) ) ;
#40258 = LINE ( 'NONE', #33912, #22358 ) ;
#40260 = DIRECTION ( 'NONE',  ( 1.000000000000000000, 0.000000000000000000, 0.000000000000000000 ) ) ;
#40259 = LINE ( 'NONE', #55731, #62698 ) ;
#40261 = CARTESIAN_POINT ( 'NONE',  ( -122.1549999999999869, 7.632228543268600340, 2.479861379858949277 ) ) ;
#40262 = CARTESIAN_POINT ( 'NONE',  ( 24.68205682311551641, 25.64738524273002440, -27.48638708064855507 ) ) ;
#40263 = DIRECTION ( 'NONE',  ( -1.000000000000000000, 0.000000000000000000, 0.000000000000000000 ) ) ;
#40264 = CARTESIAN_POINT ( 'NONE',  ( -132.4449999999999932, 0.000000000000000000, 8.024999999999991473 ) ) ;
#40265 = CARTESIAN_POINT ( 'NONE',  ( -120.7449999999999903, 4.716976649647094177, 6.492361379858945902 ) ) ;
#40266 = DIRECTION ( 'NONE',  ( 0.000000000000000000, 0.000000000000000000, 1.000000000000000000 ) ) ;
#40267 = ORIENTED_EDGE ( 'NONE', *, *, #34163, .T. ) ;
#40268 = CARTESIAN_POINT ( 'NONE',  ( -15.98999599679679839, 146.9999999999999716, -9.500000000000000000 ) ) ;
#40269 =( LENGTH_UNIT ( ) NAMED_UNIT ( * ) SI_UNIT ( .MILLI., .METRE. ) );
#40270 = LINE ( 'NONE', #28981, #66454 ) ;
#40271 = COLOUR_RGB ( '', 0.72549020, 0.75294118, 0.79215686) ;
#40272 = CARTESIAN_POINT ( 'NONE',  ( -169.9429263765337907, 0.000000000000000000, 9.524999999999991473 ) ) ;
#40273 = SHAPE_REPRESENTATION_RELATIONSHIP ( 'NONE' , 'NONE' ,  #21315, #28762 ) ;
#40274 = FACE_OUTER_BOUND ( 'NONE', #9893, .T. ) ;
#40275 = ADVANCED_FACE ( 'NONE', ( #6521 ), #5475, .F. ) ;
#40276 = DIRECTION ( 'NONE',  ( -1.000000000000000000, 0.000000000000000000, 0.000000000000000000 ) ) ;
#40277 = EDGE_CURVE ( 'NONE', #22405, #46237, #50851, .T. ) ;
#40278 = AXIS2_PLACEMENT_3D ( 'NONE', #17644, #33784, #12314 ) ;
#40279 = FILL_AREA_STYLE_COLOUR ( '', #63817 ) ;
#40280 = DIRECTION ( 'NONE',  ( 0.000000000000000000, -1.000000000000000000, -0.000000000000000000 ) ) ;
#40281 = VERTEX_POINT ( 'NONE', #35010 ) ;
#40282 = CARTESIAN_POINT ( 'NONE',  ( -89.54292637653379927, 9.058813317711329915, 2.943386871421369566 ) ) ;
#40283 = SHAPE_DEFINITION_REPRESENTATION ( #14759, #38844 ) ;
#40284 = VECTOR ( 'NONE', #52002, 1000.000000000000000 ) ;
#40286 = EDGE_CURVE ( 'NONE', #50552, #54902, #37893, .T. ) ;
#40285 = FACE_OUTER_BOUND ( 'NONE', #4968, .T. ) ;
#40287 = CARTESIAN_POINT ( 'NONE',  ( 71.99999999999998579, 64.07124727947029896, 7.500000000000000000 ) ) ;
#40288 = FILL_AREA_STYLE ('',( #57488 ) ) ;
#40289 = CARTESIAN_POINT ( 'NONE',  ( -45.00000000000000000, 7.768687147774684831, 6.999999999999999112 ) ) ;
#40290 = CARTESIAN_POINT ( 'NONE',  ( -78.05707362346616662, 0.000000000000000000, 9.524999999999991473 ) ) ;
#40291 = ORIENTED_EDGE ( 'NONE', *, *, #57249, .F. ) ;
#40292 = LINE ( 'NONE', #57133, #11183 ) ;
#40293 = EDGE_CURVE ( 'NONE', #11591, #57943, #62523, .T. ) ;
#40294 = CARTESIAN_POINT ( 'NONE',  ( 60.00000000000000000, 1.797044900979284448E-15, -10.49999999999999822 ) ) ;
#40295 = ORIENTED_EDGE ( 'NONE', *, *, #1464, .T. ) ;
#40296 = CARTESIAN_POINT ( 'NONE',  ( -8.437984349512095861, 133.8070736234661524, -5.166775262442723748E-16 ) ) ;
#40297 = AXIS2_PLACEMENT_3D ( 'NONE', #4700, #63455, #4322 ) ;
#40298 = CARTESIAN_POINT ( 'NONE',  ( -2.607480562269075097, 134.4070736234661467, 8.025000000000000355 ) ) ;
#40299 = STYLED_ITEM ( 'NONE', ( #8723 ), #959 ) ;
#40301 = EDGE_CURVE ( 'NONE', #12604, #35982, #11973, .T. ) ;
#40300 = DIRECTION ( 'NONE',  ( 1.000000000000000000, 0.000000000000000000, 0.000000000000000000 ) ) ;
#40302 = DIRECTION ( 'NONE',  ( 1.000000000000000000, 0.000000000000000000, 0.000000000000000000 ) ) ;
#40303 = AXIS2_PLACEMENT_3D ( 'NONE', #60138, #23882, #40102 ) ;
#40304 = CARTESIAN_POINT ( 'NONE',  ( 12.34222745343792127, 149.9999999999999716, 10.18181818181818166 ) ) ;
#40305 = ORIENTED_EDGE ( 'NONE', *, *, #26825, .F. ) ;
#40306 = CARTESIAN_POINT ( 'NONE',  ( -93.44292637653380496, -1.166476076187852838E-15, -9.524999999999991473 ) ) ;
#40307 = DIRECTION ( 'NONE',  ( -0.000000000000000000, 0.000000000000000000, -1.000000000000000000 ) ) ;
#40308 = SURFACE_SIDE_STYLE ('',( #7929 ) ) ;
#40309 = SURFACE_SIDE_STYLE ('',( #13546 ) ) ;
#40310 = CARTESIAN_POINT ( 'NONE',  ( -84.44499999999999318, 0.000000000000000000, 8.024999999999991473 ) ) ;
#40311 = VERTEX_POINT ( 'NONE', #51537 ) ;
#40312 = CARTESIAN_POINT ( 'NONE',  ( -20.42000000000000881, -1.426810058990923835E-13, 12.50000000000000000 ) ) ;
#40313 = FACE_OUTER_BOUND ( 'NONE', #32314, .T. ) ;
#40314 = CARTESIAN_POINT ( 'NONE',  ( 27.99999999999999645, 0.000000000000000000, 24.00402776293821816 ) ) ;
#40315 = CIRCLE ( 'NONE', #32445, 0.2500000000000002220 ) ;
#40316 = UNCERTAINTY_MEASURE_WITH_UNIT (LENGTH_MEASURE( 1.000000000000000082E-05 ), #55326, 'distance_accuracy_value', 'NONE');
#40317 = VERTEX_POINT ( 'NONE', #3298 ) ;
#40318 =( NAMED_UNIT ( * ) PLANE_ANGLE_UNIT ( ) SI_UNIT ( $, .RADIAN. ) );
#40319 = SURFACE_SIDE_STYLE ('',( #8311 ) ) ;
#40320 = AXIS2_PLACEMENT_3D ( 'NONE', #31917, #37945, #5175 ) ;
#40321 = CYLINDRICAL_SURFACE ( 'NONE', #32490, 0.2500000000000002220 ) ;
#40322 = ORIENTED_EDGE ( 'NONE', *, *, #65978, .T. ) ;
#40323 = CARTESIAN_POINT ( 'NONE',  ( -195.0000000000000000, 0.000000000000000000, 0.000000000000000000 ) ) ;
#40324 = VERTEX_POINT ( 'NONE', #8639 ) ;
#40325 = COLOUR_RGB ( '', 0.08235294, 0.09019608, 0.10196078) ;
#40326 = SURFACE_STYLE_FILL_AREA ( #67055 ) ;
#40327 = VECTOR ( 'NONE', #13723, 1000.000000000000114 ) ;
#40328 = CARTESIAN_POINT ( 'NONE',  ( -165.2070736234661865, 3.094860106618433360, 9.524999999999991473 ) ) ;
#40329 =( NAMED_UNIT ( * ) PLANE_ANGLE_UNIT ( ) SI_UNIT ( $, .RADIAN. ) );
#40330 = LINE ( 'NONE', #40689, #42047 ) ;
#40331 = AXIS2_PLACEMENT_3D ( 'NONE', #1579, #49495, #1224 ) ;
#40332 = CARTESIAN_POINT ( 'NONE',  ( -113.7570736234661837, -5.598654528085801552, 7.705886871421367523 ) ) ;
#40333 = ADVANCED_FACE ( 'NONE', ( #13908 ), #2608, .T. ) ;
#40334 = CARTESIAN_POINT ( 'NONE',  ( 3.000000000000030198, 42.00000000000000000, 80.00402776293826435 ) ) ;
#40335 = ORIENTED_EDGE ( 'NONE', *, *, #28148, .F. ) ;
#40336 =( BOUNDED_CURVE ( )  B_SPLINE_CURVE ( 2, ( #4765, #22002, #47758, #59610, #43503, #5433, #110, #21279, #21639, #69153, #10752 ),
 .UNSPECIFIED., .F., .F. ) 
 B_SPLINE_CURVE_WITH_KNOTS ( ( 3, 2, 2, 2, 2, 3 ),
 ( 0.6956521739130434590, 0.6978260869565217073, 0.6999999999999999556, 0.7021739130434783149, 0.7043478260869565633, 0.7065217391304348116 ),
 .UNSPECIFIED. ) 
 CURVE ( )  GEOMETRIC_REPRESENTATION_ITEM ( )  RATIONAL_B_SPLINE_CURVE ( ( 1.000000000000000000, 0.9510565162951535312, 1.000000000000000000, 0.9510565162951535312, 1.000000000000000000, 0.9510565162951535312, 1.000000000000000000, 0.9510565162951535312, 1.000000000000000000, 0.9510565162951535312, 1.000000000000000000 ) ) 
 REPRESENTATION_ITEM ( '' )  );
#40337 = DIRECTION ( 'NONE',  ( -0.000000000000000000, 1.000000000000000000, -0.000000000000000000 ) ) ;
#40338 = PRESENTATION_LAYER_ASSIGNMENT (  '', '', ( #24582 ) ) ;
#40339 = CARTESIAN_POINT ( 'NONE',  ( 6.330869393641157750, 43.00000000000000000, -28.38386403503541899 ) ) ;
#40340 = DIRECTION ( 'NONE',  ( -1.000000000000000000, 0.000000000000000000, 0.000000000000000000 ) ) ;
#40341 = CARTESIAN_POINT ( 'NONE',  ( -149.9050000000000296, 2.607480562269068880, -8.024999999999993250 ) ) ;
#40342 = CARTESIAN_POINT ( 'NONE',  ( -75.00000000000001421, 7.967268226264176967, 6.999999999999999112 ) ) ;
#40343 = CARTESIAN_POINT ( 'NONE',  ( -7.294180917968233757, 111.2000015091183940, -4.983928513604040766 ) ) ;
#40344 = CARTESIAN_POINT ( 'NONE',  ( -161.0949999999999420, -2.607480562269071545, -8.024999999999991473 ) ) ;
#40345 = COLOUR_RGB ( '', 0.72549020, 0.75294118, 0.79215686) ;
#40346 = CARTESIAN_POINT ( 'NONE',  ( -146.2449999999999761, -4.716976649647093289, -6.492361379858945902 ) ) ;
#40347 = VERTEX_POINT ( 'NONE', #55777 ) ;
#40348 = AXIS2_PLACEMENT_3D ( 'NONE', #64476, #31753, #21917 ) ;
#40349 = DIRECTION ( 'NONE',  ( 0.000000000000000000, 0.000000000000000000, 1.000000000000000000 ) ) ;
#40350 = CARTESIAN_POINT ( 'NONE',  ( -64.55499999999999261, 0.000000000000000000, 8.024999999999991473 ) ) ;
#40351 = DIRECTION ( 'NONE',  ( -0.000000000000000000, -0.000000000000000000, -1.000000000000000000 ) ) ;
#40353 = CARTESIAN_POINT ( 'NONE',  ( -8.082903768654762899, 3.516382302766490365E-15, 7.500000000000000000 ) ) ;
#40352 = CIRCLE ( 'NONE', #4347, 17.50000000000000000 ) ;
#40354 = EDGE_CURVE ( 'NONE', #62518, #69284, #24787, .T. ) ;
#40355 = CARTESIAN_POINT ( 'NONE',  ( -76.04499999999998749, 7.632228543268600340, 2.479861379858949277 ) ) ;
#40356 = EDGE_CURVE ( 'NONE', #21253, #33323, #69223, .T. ) ;
#40357 = CARTESIAN_POINT ( 'NONE',  ( 5.598654528085809545, 149.2549999999999955, -7.705886871421373741 ) ) ;
#40358 = SURFACE_SIDE_STYLE ('',( #12910 ) ) ;
#40359 = CARTESIAN_POINT ( 'NONE',  ( -34.99999999999999289, 99.99999999999998579, -4.000000000000000000 ) ) ;
#40360 = UNCERTAINTY_MEASURE_WITH_UNIT (LENGTH_MEASURE( 1.000000000000000082E-05 ), #37, 'distance_accuracy_value', 'NONE');
#40361 = DIRECTION ( 'NONE',  ( 1.000000000000000000, 1.224646799147353207E-16, 0.000000000000000000 ) ) ;
#40362 = CARTESIAN_POINT ( 'NONE',  ( -20.48276553341834827, 114.7646630323463057, -10.30680354032555712 ) ) ;
#40363 = EDGE_CURVE ( 'NONE', #45776, #6348, #38987, .T. ) ;
#40364 = STYLED_ITEM ( 'NONE', ( #55992 ), #44200 ) ;
#40365 = CARTESIAN_POINT ( 'NONE',  ( -74.50000000000000000, 64.49137674618943095, 10.00000000000000000 ) ) ;
#40366 = EDGE_CURVE ( 'NONE', #5580, #52546, #39627, .T. ) ;
#40367 = CIRCLE ( 'NONE', #10041, 1.000000000000000888 ) ;
#40368 = DIRECTION ( 'NONE',  ( -0.000000000000000000, -1.000000000000000000, 0.000000000000000000 ) ) ;
#40369 = CARTESIAN_POINT ( 'NONE',  ( -119.8429263765338106, 9.058813317711329915, -2.943386871421373119 ) ) ;
#40370 = EDGE_CURVE ( 'NONE', #16530, #45721, #8620, .T. ) ;
#40371 = SURFACE_SIDE_STYLE ('',( #22803 ) ) ;
#40372 = ORIENTED_EDGE ( 'NONE', *, *, #58166, .T. ) ;
#40373 = CIRCLE ( 'NONE', #52731, 1.000000000000000000 ) ;
#40374 = ORIENTED_EDGE ( 'NONE', *, *, #4149, .T. ) ;
#40375 = AXIS2_PLACEMENT_3D ( 'NONE', #64837, #65178, #53930 ) ;
#40377 = TOROIDAL_SURFACE ( 'NONE', #37044, 0.5000000000000000000, 0.2500000000000000000 ) ;
#40376 = CARTESIAN_POINT ( 'NONE',  ( -88.94292637653380496, 0.000000000000000000, 9.524999999999991473 ) ) ;
#40378 = CIRCLE ( 'NONE', #964, 1.000000000000000888 ) ;
#40379 = ADVANCED_FACE ( 'NONE', ( #29012, #66684 ), #13196, .F. ) ;
#40380 =( NAMED_UNIT ( * ) SI_UNIT ( $, .STERADIAN. ) SOLID_ANGLE_UNIT ( ) );
#40381 =( GEOMETRIC_REPRESENTATION_CONTEXT ( 3 ) GLOBAL_UNCERTAINTY_ASSIGNED_CONTEXT ( ( #4601 ) ) GLOBAL_UNIT_ASSIGNED_CONTEXT ( ( #7400, #11972, #6681 ) ) REPRESENTATION_CONTEXT ( 'NONE', 'WORKASPACE' ) );
#40382 = CARTESIAN_POINT ( 'NONE',  ( 0.000000000000000000, 0.000000000000000000, 0.000000000000000000 ) ) ;
#40383 = ORIENTED_EDGE ( 'NONE', *, *, #50744, .T. ) ;
#40384 = VERTEX_POINT ( 'NONE', #8982 ) ;
#40385 = FILL_AREA_STYLE_COLOUR ( '', #38826 ) ;
#40386 = DIRECTION ( 'NONE',  ( 1.000000000000000000, 0.000000000000000000, 0.000000000000000000 ) ) ;
#40387 = EDGE_LOOP ( 'NONE', ( #49198, #51051, #59218, #69639 ) ) ;
#40388 = DIRECTION ( 'NONE',  ( 0.000000000000000000, 1.000000000000000000, -0.000000000000000000 ) ) ;
#40389 = ORIENTED_EDGE ( 'NONE', *, *, #11675, .T. ) ;
#40390 = MECHANICAL_DESIGN_GEOMETRIC_PRESENTATION_REPRESENTATION (  '', ( #4396 ), #43785 ) ;
#40391 = CARTESIAN_POINT ( 'NONE',  ( -83.00707362346615525, -8.102448949553174629, -5.886773742842741797 ) ) ;
#40392 = PLANE ( 'NONE',  #36221 ) ;
#40393 = CARTESIAN_POINT ( 'NONE',  ( -109.9449999999999932, -9.827790563157499189E-16, -8.024999999999991473 ) ) ;
#40394 = ORIENTED_EDGE ( 'NONE', *, *, #64645, .F. ) ;
#40395 = CIRCLE ( 'NONE', #46035, 0.5000000000000004441 ) ;
#40396 = CARTESIAN_POINT ( 'NONE',  ( -13.23915246117191025, 52.65078610323165265, 2.000000000000000000 ) ) ;
#40397 = SURFACE_STYLE_FILL_AREA ( #19248 ) ;
#40398 = CARTESIAN_POINT ( 'NONE',  ( -11.69787818154473413, -11.39543851400849839, -3.768533683846105209 ) ) ;
#40399 = DIRECTION ( 'NONE',  ( -1.000000000000000000, -1.224646799147353454E-16, 0.000000000000000000 ) ) ;
#40400 = ORIENTED_EDGE ( 'NONE', *, *, #39587, .F. ) ;
#40401 = CARTESIAN_POINT ( 'NONE',  ( -4.716976649647098618, 148.1429263765338078, 6.492361379858953008 ) ) ;
#40402 = CARTESIAN_POINT ( 'NONE',  ( -54.39629169766776329, -9.126466545921049445, -3.681448577167658609 ) ) ;
#40403 = AXIS2_PLACEMENT_3D ( 'NONE', #42812, #20962, #16055 ) ;
#40404 = CARTESIAN_POINT ( 'NONE',  ( -71.50000000000000000, 35.92875272052971525, -10.00000000000000000 ) ) ;
#40405 = DIRECTION ( 'NONE',  ( 1.000000000000000000, 0.000000000000000000, -1.300977106640434891E-16 ) ) ;
#40406 = ORIENTED_EDGE ( 'NONE', *, *, #40707, .F. ) ;
#40407 = EDGE_LOOP ( 'NONE', ( #24274, #28916, #66087, #30851 ) ) ;
#40408 = CARTESIAN_POINT ( 'NONE',  ( 0.000000000000000000, 0.000000000000000000, 0.000000000000000000 ) ) ;
#40409 = DIRECTION ( 'NONE',  ( -1.000000000000000000, 0.000000000000000000, 0.000000000000000000 ) ) ;
#40410 = CARTESIAN_POINT ( 'NONE',  ( 2.000000000000022649, 50.00000000000000000, 60.00000000000000711 ) ) ;
#40411 = FACE_OUTER_BOUND ( 'NONE', #26257, .T. ) ;
#40412 = CARTESIAN_POINT ( 'NONE',  ( -132.3549999999999898, -4.716976649647093289, -6.492361379858945902 ) ) ;
#40413 =( NAMED_UNIT ( * ) SI_UNIT ( $, .STERADIAN. ) SOLID_ANGLE_UNIT ( ) );
#40414 = AXIS2_PLACEMENT_3D ( 'NONE', #6533, #61055, #12871 ) ;
#40415 = EDGE_LOOP ( 'NONE', ( #36830, #4520, #54710, #43954 ) ) ;
#40416 = CYLINDRICAL_SURFACE ( 'NONE', #36672, 8.025000000000000355 ) ;
#40417 = EDGE_CURVE ( 'NONE', #49817, #11185, #49000, .T. ) ;
#40418 = AXIS2_PLACEMENT_3D ( 'NONE', #23296, #65866, #56332 ) ;
#40419 =( NAMED_UNIT ( * ) PLANE_ANGLE_UNIT ( ) SI_UNIT ( $, .RADIAN. ) );
#40420 = SURFACE_STYLE_FILL_AREA ( #24212 ) ;
#40421 = DIRECTION ( 'NONE',  ( -1.000000000000000000, 0.000000000000000000, 0.000000000000000000 ) ) ;
#40422 = EDGE_LOOP ( 'NONE', ( #33512, #45946, #20825, #5723 ) ) ;
#40423 = ORIENTED_EDGE ( 'NONE', *, *, #19996, .F. ) ;
#40424 = DIRECTION ( 'NONE',  ( -0.000000000000000000, -0.000000000000000000, 1.000000000000000000 ) ) ;
#40425 = CIRCLE ( 'NONE', #28015, 13.00000000000000533 ) ;
#40426 = DIRECTION ( 'NONE',  ( -1.000000000000000000, -0.000000000000000000, -0.000000000000000000 ) ) ;
#40427 = CARTESIAN_POINT ( 'NONE',  ( 40.99999999999997868, 9.999999999999980460, -3.000000000000000444 ) ) ;
#40428 = CARTESIAN_POINT ( 'NONE',  ( -48.80499999999998550, -8.437984349512085203, 5.166775262442717831E-16 ) ) ;
#40429 = ORIENTED_EDGE ( 'NONE', *, *, #50753, .F. ) ;
#40430 = CARTESIAN_POINT ( 'NONE',  ( -177.8049999999999784, -8.437984349512085203, 5.166775262442717831E-16 ) ) ;
#40431 = SURFACE_STYLE_FILL_AREA ( #2006 ) ;
#40432 = CARTESIAN_POINT ( 'NONE',  ( -60.50707362346616236, 8.102448949553176405, 5.886773742842740909 ) ) ;
#40433 = AXIS2_PLACEMENT_3D ( 'NONE', #62778, #14617, #36082 ) ;
#40434 = DIRECTION ( 'NONE',  ( 8.659560562354932858E-17, 0.7071067811865474617, -0.7071067811865474617 ) ) ;
#40435 = CARTESIAN_POINT ( 'NONE',  ( -177.5070736234661695, 8.102448949553176405, 5.886773742842740909 ) ) ;
#40436 = VERTEX_POINT ( 'NONE', #20210 ) ;
#40437 = CARTESIAN_POINT ( 'NONE',  ( -74.54819447403424704, 36.40925622619634794, -10.00000000000000355 ) ) ;
#40438 = EDGE_CURVE ( 'NONE', #37912, #23750, #36776, .T. ) ;
#40439 = CARTESIAN_POINT ( 'NONE',  ( 18.00000000000000711, 30.99999999999999289, 4.000000000000000000 ) ) ;
#40440 = VECTOR ( 'NONE', #7186, 1000.000000000000000 ) ;
#40441 = DIRECTION ( 'NONE',  ( 1.000000000000000000, -0.000000000000000000, -0.000000000000000000 ) ) ;
#40442 = CARTESIAN_POINT ( 'NONE',  ( -99.05499999999999261, -9.827790563157499189E-16, -8.024999999999991473 ) ) ;
#40443 = B_SPLINE_CURVE_WITH_KNOTS ( 'NONE', 3,
 ( #9515, #69607, #26345, #10187, #52763, #43293 ),
 .UNSPECIFIED., .F., .F.,
 ( 4, 2, 4 ),
 ( 0.004189585287972436706, 0.006269578072783809838, 0.008349570857595182971 ),
 .UNSPECIFIED. ) ;
#40444 = CARTESIAN_POINT ( 'NONE',  ( -7.794228634059953364, 4.500000000000004441, 0.000000000000000000 ) ) ;
#40445 = DIRECTION ( 'NONE',  ( 1.000000000000000000, -0.000000000000000000, -1.300977106640434891E-16 ) ) ;
#40446 = EDGE_CURVE ( 'NONE', #65737, #40140, #34465, .T. ) ;
#40447 = CARTESIAN_POINT ( 'NONE',  ( -103.4949999999999761, 6.826472737025113702, -4.959722759717902107 ) ) ;
#40448 = EDGE_CURVE ( 'NONE', #34565, #15660, #53597, .T. ) ;
#40449 = CARTESIAN_POINT ( 'NONE',  ( 10.01517768586949231, 118.8049999999999926, 1.839758294383810543E-15 ) ) ;
#40450 = CARTESIAN_POINT ( 'NONE',  ( -68.24499999999999034, -4.716976649647093289, -6.492361379858945902 ) ) ;
#40451 = COLOUR_RGB ( '', 0.08235294, 0.09019608, 0.10196078) ;
#40452 = SURFACE_SIDE_STYLE ('',( #30544 ) ) ;
#40453 = UNCERTAINTY_MEASURE_WITH_UNIT (LENGTH_MEASURE( 1.000000000000000082E-05 ), #22319, 'distance_accuracy_value', 'NONE');
#40454 = AXIS2_PLACEMENT_3D ( 'NONE', #56251, #40813, #67875 ) ;
#40455 = FACE_OUTER_BOUND ( 'NONE', #48272, .T. ) ;
#40456 = CARTESIAN_POINT ( 'NONE',  ( 28.00000000000000000, 43.00000000000000000, -79.00402776293826435 ) ) ;
#40457 = ORIENTED_EDGE ( 'NONE', *, *, #9253, .F. ) ;
#40458 = EDGE_CURVE ( 'NONE', #20280, #49901, #60321, .T. ) ;
#40459 = CARTESIAN_POINT ( 'NONE',  ( -111.2929263765337851, 3.094860106618428031, -9.524999999999993250 ) ) ;
#40460 = CARTESIAN_POINT ( 'NONE',  ( -141.8950000000000102, 6.826472737025116366, 4.959722759717898555 ) ) ;
#40461 = FACE_OUTER_BOUND ( 'NONE', #32294, .T. ) ;
#40462 = VECTOR ( 'NONE', #36752, 1000.000000000000000 ) ;
#40463 = EDGE_CURVE ( 'NONE', #28627, #2770, #32084, .T. ) ;
#40464 = CARTESIAN_POINT ( 'NONE',  ( 16.75000000000000711, 27.74999999999998224, -3.750000000000000000 ) ) ;
#40465 = CARTESIAN_POINT ( 'NONE',  ( 185.0000000000000000, 0.000000000000000000, 0.000000000000000000 ) ) ;
#40466 = CARTESIAN_POINT ( 'NONE',  ( 39.74999999999999289, 18.99999999999997868, -3.750000000000000000 ) ) ;
#40467 = ORIENTED_EDGE ( 'NONE', *, *, #33410, .T. ) ;
#40468 = ORIENTED_EDGE ( 'NONE', *, *, #44051, .T. ) ;
#40469 = AXIS2_PLACEMENT_3D ( 'NONE', #49240, #22498, #43995 ) ;
#40470 = DIRECTION ( 'NONE',  ( -3.469446951953611033E-15, 0.000000000000000000, -1.000000000000000000 ) ) ;
#40471 =( BOUNDED_CURVE ( )  B_SPLINE_CURVE ( 2, ( #31615, #53093, #31249, #52419, #63291, #25302, #4884, #42565, #69597, #59047, #26328 ),
 .UNSPECIFIED., .F., .F. ) 
 B_SPLINE_CURVE_WITH_KNOTS ( ( 3, 2, 2, 2, 2, 3 ),
 ( 0.05434782608695529205, 0.05652173913043350567, 0.05869565217391171930, 0.06086956521738993292, 0.06304347826086814655, 0.06521739130434635323 ),
 .UNSPECIFIED. ) 
 CURVE ( )  GEOMETRIC_REPRESENTATION_ITEM ( )  RATIONAL_B_SPLINE_CURVE ( ( 1.000000000000027534, 0.9510565162951257756, 1.000000000000000000, 0.9510565162951535312, 1.000000000000000000, 0.9510565162951535312, 1.000000000000000000, 0.9510565162951535312, 1.000000000000000000, 0.9510565162951866158, 0.9999999999999669154 ) ) 
 REPRESENTATION_ITEM ( '' )  );
#40472 = MECHANICAL_DESIGN_GEOMETRIC_PRESENTATION_REPRESENTATION (  '', ( #16925 ), #45007 ) ;
#40473 = CARTESIAN_POINT ( 'NONE',  ( -74.99999999999998579, 118.4999999999999716, 7.500000000000000000 ) ) ;
#40474 = FILL_AREA_STYLE_COLOUR ( '', #30341 ) ;
#40475 = DIRECTION ( 'NONE',  ( 0.000000000000000000, 0.000000000000000000, 1.000000000000000000 ) ) ;
#40476 = CARTESIAN_POINT ( 'NONE',  ( 43.75000000000000000, 19.24999999999998224, 3.750000000000000000 ) ) ;
#40477 = ORIENTED_EDGE ( 'NONE', *, *, #43855, .T. ) ;
#40478 = CARTESIAN_POINT ( 'NONE',  ( -129.9549999999999841, -7.632228543268599452, 2.479861379858951054 ) ) ;
#40479 = ORIENTED_EDGE ( 'NONE', *, *, #45933, .T. ) ;
#40480 = CARTESIAN_POINT ( 'NONE',  ( -15.98999599679679839, 118.4999999999999716, -7.500000000000000000 ) ) ;
#40481 = CARTESIAN_POINT ( 'NONE',  ( -124.2570736234661837, 5.598654528085800663, -7.705886871421367523 ) ) ;
#40482 = EDGE_CURVE ( 'NONE', #28531, #56560, #34518, .T. ) ;
#40483 = EDGE_LOOP ( 'NONE', ( #67826, #48632, #14074 ) ) ;
#40484 = DIRECTION ( 'NONE',  ( 0.000000000000000000, -0.000000000000000000, 1.000000000000000000 ) ) ;
#40485 = CARTESIAN_POINT ( 'NONE',  ( -83.24292637653380211, 5.598654528085804216, 7.705886871421366635 ) ) ;
#40486 = ORIENTED_EDGE ( 'NONE', *, *, #12634, .T. ) ;
#40487 = AXIS2_PLACEMENT_3D ( 'NONE', #68225, #47864, #41866 ) ;
#40488 = MECHANICAL_DESIGN_GEOMETRIC_PRESENTATION_REPRESENTATION (  '', ( #47238 ), #32607 ) ;
#40489 =( NAMED_UNIT ( * ) SI_UNIT ( $, .STERADIAN. ) SOLID_ANGLE_UNIT ( ) );
#40490 = ADVANCED_FACE ( 'NONE', ( #5670 ), #63693, .F. ) ;
#40491 = MECHANICAL_DESIGN_GEOMETRIC_PRESENTATION_REPRESENTATION (  '', ( #5595 ), #58392 ) ;
#40492 = CARTESIAN_POINT ( 'NONE',  ( 0.000000000000000000, 139.4449999999999932, -9.525000000000000355 ) ) ;
#40493 = SURFACE_STYLE_USAGE ( .BOTH. , #18983 ) ;
#40494 = ORIENTED_EDGE ( 'NONE', *, *, #68046, .F. ) ;
#40495 = CARTESIAN_POINT ( 'NONE',  ( -5.598654528085806881, 143.8549999999999898, -7.705886871421374629 ) ) ;
#40496 = SURFACE_SIDE_STYLE ('',( #40849 ) ) ;
#40497 = STYLED_ITEM ( 'NONE', ( #3532 ), #32962 ) ;
#40498 = EDGE_LOOP ( 'NONE', ( #31036, #54116, #37225, #48894 ) ) ;
#40499 = CARTESIAN_POINT ( 'NONE',  ( -4.716976649647098618, 115.1429263765338078, 6.492361379858953008 ) ) ;
#40500 = SURFACE_SIDE_STYLE ('',( #30588 ) ) ;
#40501 = UNCERTAINTY_MEASURE_WITH_UNIT (LENGTH_MEASURE( 1.000000000000000082E-05 ), #1882, 'distance_accuracy_value', 'NONE');
#40502 = AXIS2_PLACEMENT_3D ( 'NONE', #16762, #49453, #1880 ) ;
#40503 = FILL_AREA_STYLE ('',( #8126 ) ) ;
#40504 = FACE_OUTER_BOUND ( 'NONE', #22943, .T. ) ;
#40505 = DIRECTION ( 'NONE',  ( -1.000000000000000000, 0.000000000000000000, 0.000000000000000000 ) ) ;
#40506 = VERTEX_POINT ( 'NONE', #351 ) ;
#40507 = LINE ( 'NONE', #24988, #47607 ) ;
#40508 = EDGE_LOOP ( 'NONE', ( #4936, #12889, #41986, #48457 ) ) ;
#40509 = CARTESIAN_POINT ( 'NONE',  ( 18.25000000000000711, 33.74999999999999289, -3.750000000000000000 ) ) ;
#40510 = CARTESIAN_POINT ( 'NONE',  ( -32.15258571259099085, -8.506466480591909018, -2.217585092922450318 ) ) ;
#40511 = DIRECTION ( 'NONE',  ( -1.000000000000000000, -0.000000000000000000, 0.000000000000000000 ) ) ;
#40512 = CARTESIAN_POINT ( 'NONE',  ( -167.0049999999999670, 6.826472737025116366, 4.959722759717898555 ) ) ;
#40513 = ORIENTED_EDGE ( 'NONE', *, *, #66901, .T. ) ;
#40514 = UNCERTAINTY_MEASURE_WITH_UNIT (LENGTH_MEASURE( 1.000000000000000082E-05 ), #54079, 'distance_accuracy_value', 'NONE');
#40515 = STYLED_ITEM ( 'NONE', ( #28023 ), #16655 ) ;
#40516 = COLOUR_RGB ( '', 0.09019608, 0.27058824, 0.51372549) ;
#40517 = PRESENTATION_STYLE_ASSIGNMENT (( #45799 ) ) ;
#40518 = CARTESIAN_POINT ( 'NONE',  ( -56.14388227616464633, -8.500000000000000000, 7.349426879366860454 ) ) ;
#40519 = CARTESIAN_POINT ( 'NONE',  ( 68.00000000000000000, 2.776762340297168394E-15, 12.00000000000000000 ) ) ;
#40520 = ORIENTED_EDGE ( 'NONE', *, *, #29440, .F. ) ;
#40521 = ORIENTED_EDGE ( 'NONE', *, *, #9307, .F. ) ;
#40522 = DIRECTION ( 'NONE',  ( 0.000000000000000000, 0.000000000000000000, 1.000000000000000000 ) ) ;
#40523 = DIRECTION ( 'NONE',  ( -0.000000000000000000, -0.000000000000000000, -1.000000000000000000 ) ) ;
#40524 = CARTESIAN_POINT ( 'NONE',  ( -42.80240508717511005, -12.17312045095308903, 3.179269702374134976 ) ) ;
#40525 = CARTESIAN_POINT ( 'NONE',  ( -76.40499999999995850, -2.607480562269069768, 8.024999999999991473 ) ) ;
#40526 = ORIENTED_EDGE ( 'NONE', *, *, #39658, .T. ) ;
#40527 = PRESENTATION_STYLE_ASSIGNMENT (( #18002 ) ) ;
#40528 = EDGE_CURVE ( 'NONE', #12300, #57001, #32771, .T. ) ;
#40529 =( GEOMETRIC_REPRESENTATION_CONTEXT ( 3 ) GLOBAL_UNCERTAINTY_ASSIGNED_CONTEXT ( ( #35513 ) ) GLOBAL_UNIT_ASSIGNED_CONTEXT ( ( #8407, #68527, #67840 ) ) REPRESENTATION_CONTEXT ( 'NONE', 'WORKASPACE' ) );
#40530 =( NAMED_UNIT ( * ) SI_UNIT ( $, .STERADIAN. ) SOLID_ANGLE_UNIT ( ) );
#40531 = DIRECTION ( 'NONE',  ( 0.000000000000000000, 0.000000000000000000, -1.000000000000000000 ) ) ;
#40532 = CIRCLE ( 'NONE', #9027, 16.00000000000000000 ) ;
#40533 = EDGE_CURVE ( 'NONE', #56835, #22411, #6394, .T. ) ;
#40534 = CARTESIAN_POINT ( 'NONE',  ( -75.00000000000000000, 9.372809501821780742, -6.584099566153144067 ) ) ;
#40535 = ORIENTED_EDGE ( 'NONE', *, *, #68560, .F. ) ;
#40537 = CARTESIAN_POINT ( 'NONE',  ( 48.00000000000000000, 99.99999999999992895, -7.000000000000000000 ) ) ;
#40536 = DIRECTION ( 'NONE',  ( -1.000000000000000000, 0.000000000000000000, 0.000000000000000000 ) ) ;
#40538 = EDGE_CURVE ( 'NONE', #32404, #61539, #50242, .T. ) ;
#40539 = CARTESIAN_POINT ( 'NONE',  ( -3.094860106618432471, 139.5949999999999420, -9.525000000000000355 ) ) ;
#40540 = CARTESIAN_POINT ( 'NONE',  ( -99.74499999999999034, 4.716976649647094177, 6.492361379858945902 ) ) ;
#40541 = SURFACE_SIDE_STYLE ('',( #45819 ) ) ;
#40542 =( GEOMETRIC_REPRESENTATION_CONTEXT ( 3 ) GLOBAL_UNCERTAINTY_ASSIGNED_CONTEXT ( ( #66530 ) ) GLOBAL_UNIT_ASSIGNED_CONTEXT ( ( #56585, #40099, #34437 ) ) REPRESENTATION_CONTEXT ( 'NONE', 'WORKASPACE' ) );
#40543 = COLOUR_RGB ( '', 0.40784314, 0.44705882, 0.49803922) ;
#40544 = UNCERTAINTY_MEASURE_WITH_UNIT (LENGTH_MEASURE( 1.000000000000000082E-05 ), #55353, 'distance_accuracy_value', 'NONE');
#40545 = AXIS2_PLACEMENT_3D ( 'NONE', #6090, #48705, #60926 ) ;
#40547 = LINE ( 'NONE', #2838, #7789 ) ;
#40546 = FILL_AREA_STYLE ('',( #7801 ) ) ;
#40548 = CARTESIAN_POINT ( 'NONE',  ( -139.7929263765337851, -3.094860106618429807, 9.524999999999991473 ) ) ;
#40549 = CARTESIAN_POINT ( 'NONE',  ( -166.1949999999999932, 8.437984349512085203, -1.550032578732815448E-15 ) ) ;
#40550 = AXIS2_PLACEMENT_3D ( 'NONE', #32141, #25813, #58526 ) ;
#40551 = EDGE_CURVE ( 'NONE', #31165, #54295, #2066, .T. ) ;
#40552 = AXIS2_PLACEMENT_3D ( 'NONE', #290, #21461, #26391 ) ;
#40553 = DIRECTION ( 'NONE',  ( 0.000000000000000000, 1.000000000000000000, 0.000000000000000000 ) ) ;
#40554 = ORIENTED_EDGE ( 'NONE', *, *, #48431, .F. ) ;
#40555 = CARTESIAN_POINT ( 'NONE',  ( -72.00000000000000000, 14.49137674618942562, -9.500000000000000000 ) ) ;
#40556 = ORIENTED_EDGE ( 'NONE', *, *, #27948, .F. ) ;
#40557 = CIRCLE ( 'NONE', #51791, 8.000000000000000000 ) ;
#40558 = DIRECTION ( 'NONE',  ( 1.000000000000000000, 0.000000000000000000, 0.000000000000000000 ) ) ;
#40559 = CARTESIAN_POINT ( 'NONE',  ( 0.000000000000000000, 131.5549999999999784, -9.525000000000000355 ) ) ;
#40560 =( NAMED_UNIT ( * ) PLANE_ANGLE_UNIT ( ) SI_UNIT ( $, .RADIAN. ) );
#40561 = CARTESIAN_POINT ( 'NONE',  ( 7.632228543268608334, 119.3429263765338249, -2.479861379858951942 ) ) ;
#40562 = DIRECTION ( 'NONE',  ( 1.000000000000000000, 1.027984282060330356E-15, 0.000000000000000000 ) ) ;
#40563 = FACE_OUTER_BOUND ( 'NONE', #44910, .T. ) ;
#40564 = ORIENTED_EDGE ( 'NONE', *, *, #45922, .F. ) ;
#40565 = CARTESIAN_POINT ( 'NONE',  ( -160.5550000000000068, 0.000000000000000000, 8.024999999999991473 ) ) ;
#40566 = ORIENTED_EDGE ( 'NONE', *, *, #24233, .F. ) ;
#40567 = CARTESIAN_POINT ( 'NONE',  ( 1.709458476932651091E-14, 14.00000000000000533, 35.50000000000000000 ) ) ;
#40568 = ORIENTED_EDGE ( 'NONE', *, *, #12746, .F. ) ;
#40569 = TOROIDAL_SURFACE ( 'NONE', #24806, 4.000000000000000000, 1.000000000000000000 ) ;
#40570 = FILL_AREA_STYLE_COLOUR ( '', #38284 ) ;
#40571 = CARTESIAN_POINT ( 'NONE',  ( 5.598654528085809545, 112.1449999999999818, -7.705886871421373741 ) ) ;
#40572 = ORIENTED_EDGE ( 'NONE', *, *, #44127, .F. ) ;
#40573 = COLOUR_RGB ( '', 0.31764706, 0.68627451, 0.89019608) ;
#40574 = FILL_AREA_STYLE ('',( #51118 ) ) ;
#40575 = CARTESIAN_POINT ( 'NONE',  ( 9.058813317711337021, 115.6549999999999869, 2.943386871421375783 ) ) ;
#40576 = AXIS2_PLACEMENT_3D ( 'NONE', #31937, #26638, #9817 ) ;
#40577 = CARTESIAN_POINT ( 'NONE',  ( -74.90500000000000114, 2.607480562269069324, -8.024999999999993250 ) ) ;
#40578 =( LENGTH_UNIT ( ) NAMED_UNIT ( * ) SI_UNIT ( .MILLI., .METRE. ) );
#40579 = ORIENTED_EDGE ( 'NONE', *, *, #63648, .T. ) ;
#40580 = CARTESIAN_POINT ( 'NONE',  ( 8.102448949553181734, 136.5049999999999386, 5.886773742842750679 ) ) ;
#40581 = UNCERTAINTY_MEASURE_WITH_UNIT (LENGTH_MEASURE( 1.000000000000000082E-05 ), #20096, 'distance_accuracy_value', 'NONE');
#40582 = AXIS2_PLACEMENT_3D ( 'NONE', #47497, #36600, #10512 ) ;
#40583 = CARTESIAN_POINT ( 'NONE',  ( -114.4429263765338050, -1.166476076187852838E-15, -9.524999999999991473 ) ) ;
#40584 = VECTOR ( 'NONE', #44398, 1000.000000000000000 ) ;
#40585 = FACE_OUTER_BOUND ( 'NONE', #10186, .T. ) ;
#40586 = ORIENTED_EDGE ( 'NONE', *, *, #14288, .F. ) ;
#40587 = FACE_OUTER_BOUND ( 'NONE', #14263, .T. ) ;
#40588 = DIRECTION ( 'NONE',  ( 1.000000000000000000, 0.000000000000000000, 0.000000000000000000 ) ) ;
#40589 = CARTESIAN_POINT ( 'NONE',  ( -56.84499999999997755, -7.632228543268599452, 2.479861379858951054 ) ) ;
#40591 = EDGE_LOOP ( 'NONE', ( #8293, #20767, #48568, #38542 ) ) ;
#40590 =( GEOMETRIC_REPRESENTATION_CONTEXT ( 3 ) GLOBAL_UNCERTAINTY_ASSIGNED_CONTEXT ( ( #22927 ) ) GLOBAL_UNIT_ASSIGNED_CONTEXT ( ( #39450, #19593, #62500 ) ) REPRESENTATION_CONTEXT ( 'NONE', 'WORKASPACE' ) );
#40592 = CARTESIAN_POINT ( 'NONE',  ( 4.250000000000001776, 21.74999999999998579, -4.000000000000000000 ) ) ;
#40593 = MECHANICAL_DESIGN_GEOMETRIC_PRESENTATION_REPRESENTATION (  '', ( #58539 ), #51776 ) ;
#40594 = CARTESIAN_POINT ( 'NONE',  ( 60.00000000000000000, 1.797044900979284448E-15, -11.50000000000001066 ) ) ;
#40595 = SURFACE_STYLE_USAGE ( .BOTH. , #3953 ) ;
#40596 = VERTEX_POINT ( 'NONE', #34157 ) ;
#40597 = CARTESIAN_POINT ( 'NONE',  ( -57.74499999999999034, 4.716976649647094177, 6.492361379858945902 ) ) ;
#40598 = EDGE_LOOP ( 'NONE', ( #35174, #29368, #37231, #46209 ) ) ;
#40599 = CARTESIAN_POINT ( 'NONE',  ( 71.99999999999998579, 119.9999999999997868, -7.000000000000000000 ) ) ;
#40600 = CARTESIAN_POINT ( 'NONE',  ( -101.3050000000000068, 8.437984349512085203, -1.550032578732815448E-15 ) ) ;
#40601 = ORIENTED_EDGE ( 'NONE', *, *, #3863, .T. ) ;
#40602 = CARTESIAN_POINT ( 'NONE',  ( 15.48999599679679662, 147.4999999999999716, 9.500000000000000000 ) ) ;
#40603 = EDGE_CURVE ( 'NONE', #2689, #28083, #5279, .T. ) ;
#40604 = DIRECTION ( 'NONE',  ( 0.000000000000000000, 0.000000000000000000, -1.000000000000000000 ) ) ;
#40605 = CARTESIAN_POINT ( 'NONE',  ( -137.7570736234661695, -5.598654528085801552, 7.705886871421367523 ) ) ;
#40606 = CARTESIAN_POINT ( 'NONE',  ( -59.45707362346616520, -9.058813317711329915, 2.943386871421371787 ) ) ;
#40607 = VECTOR ( 'NONE', #45916, 1000.000000000000000 ) ;
#40608 = CARTESIAN_POINT ( 'NONE',  ( -5.598654528085808657, 143.6449999999999818, 7.705886871421373741 ) ) ;
#40609 = CARTESIAN_POINT ( 'NONE',  ( -78.05707362346616662, 0.000000000000000000, 9.524999999999991473 ) ) ;
#40610 = SPHERICAL_SURFACE ( 'NONE', #13426, 1.000000000000000000 ) ;
#40611 = DIRECTION ( 'NONE',  ( 0.000000000000000000, 1.000000000000000000, 0.000000000000000000 ) ) ;
#40612 = CARTESIAN_POINT ( 'NONE',  ( -16.77315986280488147, -11.05089483305399867, 4.677852893037058202 ) ) ;
#40614 = CARTESIAN_POINT ( 'NONE',  ( -100.0429263765338135, -9.058813317711329915, -2.943386871421370898 ) ) ;
#40613 = DIRECTION ( 'NONE',  ( 0.000000000000000000, 0.000000000000000000, 1.000000000000000000 ) ) ;
#40615 = CARTESIAN_POINT ( 'NONE',  ( -120.3549999999999898, -4.716976649647093289, -6.492361379858945902 ) ) ;
#40616 = EDGE_CURVE ( 'NONE', #37694, #58312, #39819, .T. ) ;
#40617 = CARTESIAN_POINT ( 'NONE',  ( -3.094860106618432471, 109.5949999999999847, -9.525000000000000355 ) ) ;
#40618 = CARTESIAN_POINT ( 'NONE',  ( -140.3950000000000102, -6.826472737025115478, -4.959722759717899443 ) ) ;
#40619 = EDGE_CURVE ( 'NONE', #28517, #41509, #7079, .T. ) ;
#40620 = CARTESIAN_POINT ( 'NONE',  ( -123.4449999999999932, 0.000000000000000000, 8.024999999999991473 ) ) ;
#40621 = AXIS2_PLACEMENT_3D ( 'NONE', #318, #64051, #11975 ) ;
#40622 = EDGE_CURVE ( 'NONE', #35271, #47282, #43517, .T. ) ;
#40623 = CARTESIAN_POINT ( 'NONE',  ( 18.25000000000000711, 33.74999999999999289, 4.000000000000000000 ) ) ;
#40624 = ORIENTED_EDGE ( 'NONE', *, *, #1855, .T. ) ;
#40625 = DIRECTION ( 'NONE',  ( -1.000000000000000000, 0.000000000000000000, 0.000000000000000000 ) ) ;
#40626 = CARTESIAN_POINT ( 'NONE',  ( 60.00000000000000000, -2.024042244987997205E-14, -7.000000000000000000 ) ) ;
#40627 = VECTOR ( 'NONE', #9768, 1000.000000000000000 ) ;
#40628 = EDGE_CURVE ( 'NONE', #30410, #19536, #45753, .T. ) ;
#40629 = CARTESIAN_POINT ( 'NONE',  ( -175.4929263765337737, -8.102448949553172852, 5.886773742842742685 ) ) ;
#40630 = CARTESIAN_POINT ( 'NONE',  ( 30.99999999999998579, 5.000000000000000000, 72.00402776293822171 ) ) ;
#40631 = STYLED_ITEM ( 'NONE', ( #59689 ), #11533 ) ;
#40632 = EDGE_CURVE ( 'NONE', #5105, #41266, #54690, .T. ) ;
#40633 = B_SPLINE_CURVE_WITH_KNOTS ( 'NONE', 3,
 ( #7945, #25166, #8312, #2623, #66696, #29390 ),
 .UNSPECIFIED., .F., .F.,
 ( 4, 2, 4 ),
 ( 0.004189585287972440175, 0.006269578072783814175, 0.008349570857595188175 ),
 .UNSPECIFIED. ) ;
#40634 = DIRECTION ( 'NONE',  ( 1.000000000000000000, 0.000000000000000000, 0.000000000000000000 ) ) ;
#40635 = LINE ( 'NONE', #29711, #30498 ) ;
#40636 = EDGE_LOOP ( 'NONE', ( #67140, #28477, #5680, #63708 ) ) ;
#40637 = VECTOR ( 'NONE', #20562, 1000.000000000000000 ) ;
#40638 = CARTESIAN_POINT ( 'NONE',  ( -89.69292637653380496, 10.01517768586948698, -1.839758294383808571E-15 ) ) ;
#40639 = CONTEXT_DEPENDENT_SHAPE_REPRESENTATION ( #20373, #7531 ) ;
#40640 = CARTESIAN_POINT ( 'NONE',  ( -72.00000000000000000, 35.92875272052971525, -9.500000000000000000 ) ) ;
#40641 = AXIS2_PLACEMENT_3D ( 'NONE', #22364, #49456, #63115 ) ;
#40642 = APPLICATION_CONTEXT ( 'automotive_design' ) ;
#40643 = CARTESIAN_POINT ( 'NONE',  ( -3.000000000000000000, -2.499999999999999556, 24.00000000000000000 ) ) ;
#40644 =( LENGTH_UNIT ( ) NAMED_UNIT ( * ) SI_UNIT ( .MILLI., .METRE. ) );
#40645 = PRESENTATION_STYLE_ASSIGNMENT (( #4000 ) ) ;
#40646 =( GEOMETRIC_REPRESENTATION_CONTEXT ( 3 ) GLOBAL_UNCERTAINTY_ASSIGNED_CONTEXT ( ( #55028 ) ) GLOBAL_UNIT_ASSIGNED_CONTEXT ( ( #32320, #27712, #44204 ) ) REPRESENTATION_CONTEXT ( 'NONE', 'WORKASPACE' ) );
#40647 = CARTESIAN_POINT ( 'NONE',  ( -22.50000000000000711, 33.99999999999999289, 3.750000000000000000 ) ) ;
#40648 = ORIENTED_EDGE ( 'NONE', *, *, #29136, .T. ) ;
#40649 = CIRCLE ( 'NONE', #128, 8.499999999999992895 ) ;
#40650 = CARTESIAN_POINT ( 'NONE',  ( -136.1929263765337907, -10.01517768586948698, 6.132527647946031529E-16 ) ) ;
#40651 =( LENGTH_UNIT ( ) NAMED_UNIT ( * ) SI_UNIT ( .MILLI., .METRE. ) );
#40652 = ORIENTED_EDGE ( 'NONE', *, *, #26584, .T. ) ;
#40653 = CARTESIAN_POINT ( 'NONE',  ( -63.74292637653379501, -5.598654528085803328, -7.705886871421366635 ) ) ;
#40654 = SURFACE_STYLE_USAGE ( .BOTH. , #31096 ) ;
#40655 = CARTESIAN_POINT ( 'NONE',  ( -9.827790563157511022E-16, 134.5570736234661808, 8.025000000000000355 ) ) ;
#40656 = CIRCLE ( 'NONE', #65335, 0.2500000000000002220 ) ;
#40657 = ORIENTED_EDGE ( 'NONE', *, *, #53659, .T. ) ;
#40658 = DIRECTION ( 'NONE',  ( -1.000000000000000000, 0.000000000000000000, 0.000000000000000000 ) ) ;
#40659 = CARTESIAN_POINT ( 'NONE',  ( 74.57962914963243861, 19.59826060529046288, -6.436893197989947524 ) ) ;
#40660 = AXIS2_PLACEMENT_3D ( 'NONE', #4651, #47275, #63053 ) ;
#40661 = DIRECTION ( 'NONE',  ( 0.000000000000000000, 0.000000000000000000, 1.000000000000000000 ) ) ;
#40662 = ORIENTED_EDGE ( 'NONE', *, *, #67824, .F. ) ;
#40663 = CARTESIAN_POINT ( 'NONE',  ( 23.50000000000001776, 15.00000000000000000, 27.18999999999999417 ) ) ;
#40664 = CARTESIAN_POINT ( 'NONE',  ( 179.4361977533490347, 0.000000000000000000, -103.7004518695263044 ) ) ;
#40665 = SURFACE_STYLE_USAGE ( .BOTH. , #55778 ) ;
#40666 = CIRCLE ( 'NONE', #58614, 18.00000000000000355 ) ;
#40667 =( LENGTH_UNIT ( ) NAMED_UNIT ( * ) SI_UNIT ( .MILLI., .METRE. ) );
#40668 = CARTESIAN_POINT ( 'NONE',  ( -84.74499999999999034, 4.716976649647094177, 6.492361379858945902 ) ) ;
#40669 = ORIENTED_EDGE ( 'NONE', *, *, #30038, .T. ) ;
#40670 = SHAPE_REPRESENTATION ( '1. Base', ( #42840 ), #53979 ) ;
#40671 = MECHANICAL_DESIGN_GEOMETRIC_PRESENTATION_REPRESENTATION (  '', ( #64190 ), #37283 ) ;
#40672 = AXIS2_PLACEMENT_3D ( 'NONE', #56081, #67687, #50138 ) ;
#40673 = CARTESIAN_POINT ( 'NONE',  ( 0.000000000000000000, 154.9999999999999716, 0.000000000000000000 ) ) ;
#40674 = ORIENTED_EDGE ( 'NONE', *, *, #56795, .T. ) ;
#40675 = CARTESIAN_POINT ( 'NONE',  ( -75.48275862068965125, 63.99167409976910648, -6.499999999999999112 ) ) ;
#40676 = CIRCLE ( 'NONE', #58622, 23.00000000000000355 ) ;
#40677 = DIRECTION ( 'NONE',  ( -1.000000000000000000, 0.000000000000000000, 0.000000000000000000 ) ) ;
#40678 = EDGE_LOOP ( 'NONE', ( #64281, #40564, #37516, #34516 ) ) ;
#40679 = AXIS2_PLACEMENT_3D ( 'NONE', #9762, #4431, #63554 ) ;
#40680 = LINE ( 'NONE', #51218, #44326 ) ;
#40682 = EDGE_LOOP ( 'NONE', ( #9159, #65026, #32349, #63396 ) ) ;
#40681 = EDGE_CURVE ( 'NONE', #51630, #33237, #25521, .T. ) ;
#40683 = FACE_BOUND ( 'NONE', #14877, .T. ) ;
#40684 =( NAMED_UNIT ( * ) SI_UNIT ( $, .STERADIAN. ) SOLID_ANGLE_UNIT ( ) );
#40685 = LINE ( 'NONE', #67744, #12008 ) ;
#40686 = CARTESIAN_POINT ( 'NONE',  ( -169.1070736234662206, 8.102448949553171076, -5.886773742842744461 ) ) ;
#40687 = AXIS2_PLACEMENT_3D ( 'NONE', #48558, #11565, #33035 ) ;
#40688 = DIRECTION ( 'NONE',  ( 0.000000000000000000, 1.000000000000000000, 0.000000000000000000 ) ) ;
#40689 = CARTESIAN_POINT ( 'NONE',  ( 22.25000000000000711, 33.99999999999999289, -4.000000000000000000 ) ) ;
#40690 = EDGE_CURVE ( 'NONE', #15308, #53146, #44654, .T. ) ;
#40691 = CARTESIAN_POINT ( 'NONE',  ( -118.2570736234661695, 5.598654528085800663, -7.705886871421367523 ) ) ;
#40692 = CARTESIAN_POINT ( 'NONE',  ( -70.75000000000000000, -4.000000000000000000, 20.00000000000000000 ) ) ;
#40693 = DIRECTION ( 'NONE',  ( 0.000000000000000000, -0.000000000000000000, -1.000000000000000000 ) ) ;
#40694 = EDGE_LOOP ( 'NONE', ( #52282, #64839, #14231, #50629 ) ) ;
#40695 = AXIS2_PLACEMENT_3D ( 'NONE', #49706, #22973, #39173 ) ;
#40696 = DIRECTION ( 'NONE',  ( 0.000000000000000000, 0.000000000000000000, 1.000000000000000000 ) ) ;
#40697 = EDGE_CURVE ( 'NONE', #7755, #33323, #28860, .T. ) ;
#40698 = CARTESIAN_POINT ( 'NONE',  ( -82.04292637653379927, -9.058813317711329915, -2.943386871421370898 ) ) ;
#40700 = CARTESIAN_POINT ( 'NONE',  ( -61.04292637653379927, -9.058813317711329915, -2.943386871421370898 ) ) ;
#40699 = FACE_OUTER_BOUND ( 'NONE', #45929, .T. ) ;
#40701 = DIRECTION ( 'NONE',  ( 1.000000000000000000, -0.000000000000000000, 0.000000000000000000 ) ) ;
#40702 = VECTOR ( 'NONE', #3049, 1000.000000000000000 ) ;
#40703 = CARTESIAN_POINT ( 'NONE',  ( -154.4050000000000011, -2.607480562269069768, 8.024999999999991473 ) ) ;
#40704 = FILL_AREA_STYLE ('',( #46339 ) ) ;
#40705 = CARTESIAN_POINT ( 'NONE',  ( -148.7929263765342398, -3.094860106610967776, 9.525000000005412915 ) ) ;
#40706 = CARTESIAN_POINT ( 'NONE',  ( -163.0449999999999875, 7.632228543268600340, 2.479861379858949277 ) ) ;
#40707 = EDGE_CURVE ( 'NONE', #30995, #16782, #35639, .T. ) ;
#40708 = CARTESIAN_POINT ( 'NONE',  ( -151.6450000000000102, 4.716976649647091513, -6.492361379858946790 ) ) ;
#40709 = ORIENTED_EDGE ( 'NONE', *, *, #2059, .T. ) ;
#40710 = LINE ( 'NONE', #56150, #2113 ) ;
#40711 = VECTOR ( 'NONE', #2168, 1000.000000000000000 ) ;
#40712 = FACE_OUTER_BOUND ( 'NONE', #29804, .T. ) ;
#40713 = ADVANCED_FACE ( 'NONE', ( #50342 ), #50012, .F. ) ;
#40714 = CARTESIAN_POINT ( 'NONE',  ( 71.99999999999998579, 64.07124727947029896, 9.500000000000000000 ) ) ;
#40715 = CARTESIAN_POINT ( 'NONE',  ( -67.40499999999997272, -2.607480562269069768, 8.024999999999991473 ) ) ;
#40716 =( NAMED_UNIT ( * ) SI_UNIT ( $, .STERADIAN. ) SOLID_ANGLE_UNIT ( ) );
#40717 = CIRCLE ( 'NONE', #53048, 9.000000000000000000 ) ;
#40718 = CARTESIAN_POINT ( 'NONE',  ( -168.1429263765338078, 5.598654528085800663, -7.705886871421367523 ) ) ;
#40719 = CARTESIAN_POINT ( 'NONE',  ( -63.74499999999998323, 4.716976649647094177, 6.492361379858945902 ) ) ;
#40720 = CARTESIAN_POINT ( 'NONE',  ( 9.058813317711338797, 154.9549999999999841, -2.943386871421372675 ) ) ;
#40721 = CARTESIAN_POINT ( 'NONE',  ( -143.7570736234661695, -5.598654528085801552, 7.705886871421367523 ) ) ;
#40722 = STYLED_ITEM ( 'NONE', ( #37984 ), #60689 ) ;
#40723 = DIRECTION ( 'NONE',  ( -0.000000000000000000, -1.000000000000000000, -0.000000000000000000 ) ) ;
#40724 = CARTESIAN_POINT ( 'NONE',  ( -159.9570736234661865, 9.058813317711329915, -2.943386871421373119 ) ) ;
#40725 = PRESENTATION_LAYER_ASSIGNMENT (  '', '', ( #5825 ) ) ;
#40726 = DIRECTION ( 'NONE',  ( 1.000000000000000000, -1.189524669241239115E-16, -0.000000000000000000 ) ) ;
#40727 = DIRECTION ( 'NONE',  ( 1.000000000000000000, 0.000000000000000000, 0.000000000000000000 ) ) ;
#40728 = CIRCLE ( 'NONE', #9286, 0.2500000000000002220 ) ;
#40729 = LINE ( 'NONE', #62829, #2275 ) ;
#40730 = SPHERICAL_SURFACE ( 'NONE', #53247, 0.2500000000000000000 ) ;
#40731 = CARTESIAN_POINT ( 'NONE',  ( -75.75000000000000000, -3.000000000000000000, 19.00000000000000000 ) ) ;
#40732 = EDGE_LOOP ( 'NONE', ( #14218, #41818, #62598, #35454 ) ) ;
#40733 = ORIENTED_EDGE ( 'NONE', *, *, #10027, .F. ) ;
#40734 = PRESENTATION_STYLE_ASSIGNMENT (( #8368 ) ) ;
#40735 = VECTOR ( 'NONE', #61137, 1000.000000000000000 ) ;
#40736 = DIRECTION ( 'NONE',  ( 0.000000000000000000, 1.000000000000000000, 0.000000000000000000 ) ) ;
#40737 = EDGE_CURVE ( 'NONE', #53177, #36309, #45105, .T. ) ;
#40738 = CARTESIAN_POINT ( 'NONE',  ( -45.00000000000000000, 9.520518382567219717, 6.450733387540871888 ) ) ;
#40739 = ORIENTED_EDGE ( 'NONE', *, *, #20580, .F. ) ;
#40740 = VERTEX_POINT ( 'NONE', #17659 ) ;
#40741 = CARTESIAN_POINT ( 'NONE',  ( -69.50000000000000000, 50.00000000000000000, -12.00000000000000000 ) ) ;
#40742 = AXIS2_PLACEMENT_3D ( 'NONE', #49023, #16650, #10657 ) ;
#40743 = ORIENTED_EDGE ( 'NONE', *, *, #36855, .F. ) ;
#40744 = SURFACE_STYLE_USAGE ( .BOTH. , #32656 ) ;
#40745 = CARTESIAN_POINT ( 'NONE',  ( -144.8929263765338078, -8.102448949553174629, -5.886773742842741797 ) ) ;
#40746 = EDGE_LOOP ( 'NONE', ( #141, #61323, #57969 ) ) ;
#40747 = AXIS2_PLACEMENT_3D ( 'NONE', #41134, #30879, #47830 ) ;
#40748 = DIRECTION ( 'NONE',  ( 0.000000000000000000, 0.000000000000000000, -1.000000000000000000 ) ) ;
#40749 = CARTESIAN_POINT ( 'NONE',  ( 21.02379604162864268, 110.4999999999999858, -10.00000000000000000 ) ) ;
#40750 = CARTESIAN_POINT ( 'NONE',  ( -109.7950000000000017, 2.607480562269068880, -8.024999999999993250 ) ) ;
#40751 = ORIENTED_EDGE ( 'NONE', *, *, #23194, .T. ) ;
#40752 = CARTESIAN_POINT ( 'NONE',  ( -163.5570736234661524, -1.166476076187852838E-15, -9.524999999999991473 ) ) ;
#40753 = CARTESIAN_POINT ( 'NONE',  ( -178.7070736234662718, -3.094860106619322426, -9.524999999999344880 ) ) ;
#40754 = VERTEX_POINT ( 'NONE', #54568 ) ;
#40755 = CARTESIAN_POINT ( 'NONE',  ( 7.632228543268607446, 149.0429263765338135, 2.479861379858954606 ) ) ;
#40756 = SURFACE_SIDE_STYLE ('',( #61811 ) ) ;
#40757 =( BOUNDED_CURVE ( )  B_SPLINE_CURVE ( 2, ( #49774, #7205, #27588, #60639, #23717, #39239, #28635, #1151, #6843, #2186, #793 ),
 .UNSPECIFIED., .F., .F. ) 
 B_SPLINE_CURVE_WITH_KNOTS ( ( 3, 2, 2, 2, 2, 3 ),
 ( 0.1413043478260836983, 0.1434782608695618911, 0.1456521739130400284, 0.1478260869565182212, 0.1499999999999963585, 0.1521739130434745513 ),
 .UNSPECIFIED. ) 
 CURVE ( )  GEOMETRIC_REPRESENTATION_ITEM ( )  RATIONAL_B_SPLINE_CURVE ( ( 1.000000000000073053, 0.9510565162950803675, 1.000000000000000000, 0.9510565162951535312, 1.000000000000000000, 0.9510565162951535312, 1.000000000000000000, 0.9510565162951535312, 1.000000000000000000, 0.9510565162952372420, 0.9999999999999162892 ) ) 
 REPRESENTATION_ITEM ( '' )  );
#40758 = CARTESIAN_POINT ( 'NONE',  ( 72.49999999999998579, 119.9999999999997868, 9.500000000000000000 ) ) ;
#40759 = AXIS2_PLACEMENT_3D ( 'NONE', #25675, #57713, #56671 ) ;
#40760 = EDGE_CURVE ( 'NONE', #60757, #21935, #64699, .T. ) ;
#40761 = DIRECTION ( 'NONE',  ( 0.000000000000000000, 1.000000000000000000, 0.000000000000000000 ) ) ;
#40762 = SURFACE_SIDE_STYLE ('',( #24528 ) ) ;
#40763 = EDGE_CURVE ( 'NONE', #20328, #330, #14285, .T. ) ;
#40764 = EDGE_LOOP ( 'NONE', ( #900, #43597, #40887, #46206 ) ) ;
#40765 = CARTESIAN_POINT ( 'NONE',  ( 3.999798566743339556, 49.09558629977726696, -2.000000000000000000 ) ) ;
#40766 = ORIENTED_EDGE ( 'NONE', *, *, #54300, .T. ) ;
#40767 = FACE_OUTER_BOUND ( 'NONE', #13405, .T. ) ;
#40768 = DIRECTION ( 'NONE',  ( 1.000000000000000000, 0.000000000000000000, 0.000000000000000000 ) ) ;
#40769 = CARTESIAN_POINT ( 'NONE',  ( -20.20529291564252361, 114.9650358309326634, 10.39743153126989128 ) ) ;
#40770 = DIRECTION ( 'NONE',  ( 1.000000000000000000, 0.000000000000000000, 0.000000000000000000 ) ) ;
#40771 = AXIS2_PLACEMENT_3D ( 'NONE', #57980, #53393, #69224 ) ;
#40772 = CARTESIAN_POINT ( 'NONE',  ( -123.9549999999999841, -7.632228543268599452, 2.479861379858951054 ) ) ;
#40773 = DIRECTION ( 'NONE',  ( 0.000000000000000000, 0.000000000000000000, 1.000000000000000000 ) ) ;
#40774 = CARTESIAN_POINT ( 'NONE',  ( 4.716976649647096842, 140.8570736234661638, 6.492361379858953896 ) ) ;
#40775 = EDGE_CURVE ( 'NONE', #51660, #41879, #18751, .T. ) ;
#40776 = VECTOR ( 'NONE', #67922, 1000.000000000000000 ) ;
#40777 = CYLINDRICAL_SURFACE ( 'NONE', #64336, 9.524999999999991473 ) ;
#40778 = CARTESIAN_POINT ( 'NONE',  ( -23.21231517720797655, 117.9999999999999716, -7.000000000000000000 ) ) ;
#40779 = ORIENTED_EDGE ( 'NONE', *, *, #41024, .F. ) ;
#40780 = ORIENTED_EDGE ( 'NONE', *, *, #51249, .F. ) ;
#40781 = CARTESIAN_POINT ( 'NONE',  ( -44.99154893936432842, 9.591540374752316467, 2.999999999999999556 ) ) ;
#40782 = CARTESIAN_POINT ( 'NONE',  ( 45.65811388300841855, 10.21937129433612235, 6.000000000000000888 ) ) ;
#40783 = CARTESIAN_POINT ( 'NONE',  ( 6.062177826491067734, -2.500000000000000000, 3.500000000000000000 ) ) ;
#40784 = CARTESIAN_POINT ( 'NONE',  ( -51.80499999999998550, -8.437984349512085203, 5.166775262442717831E-16 ) ) ;
#40785 = VERTEX_POINT ( 'NONE', #12329 ) ;
#40786 = CARTESIAN_POINT ( 'NONE',  ( -177.6550000000000011, -7.632228543268600340, -2.479861379858950166 ) ) ;
#40787 = CARTESIAN_POINT ( 'NONE',  ( -90.44292637653379074, -1.166476076187852838E-15, -9.524999999999991473 ) ) ;
#40788 = STYLED_ITEM ( 'NONE', ( #13728 ), #22800 ) ;
#40789 = CARTESIAN_POINT ( 'NONE',  ( -57.80707362346616662, 10.01517768586948698, -1.839758294383808571E-15 ) ) ;
#40790 = EDGE_CURVE ( 'NONE', #2682, #10224, #35197, .T. ) ;
#40791 = COLOUR_RGB ( '', 0.08235294, 0.09019608, 0.10196078) ;
#40792 = CARTESIAN_POINT ( 'NONE',  ( -178.4949999999999477, 6.826472737025113702, -4.959722759717902107 ) ) ;
#40793 = DIRECTION ( 'NONE',  ( -1.387778780781444413E-14, 0.000000000000000000, -1.000000000000000000 ) ) ;
#40794 = EDGE_LOOP ( 'NONE', ( #43123, #14800, #33650 ) ) ;
#40795 = AXIS2_PLACEMENT_3D ( 'NONE', #4999, #53877, #53547 ) ;
#40796 = CARTESIAN_POINT ( 'NONE',  ( -75.00000000000000000, 35.50862325381056905, -9.500000000000000000 ) ) ;
#40797 = FACE_OUTER_BOUND ( 'NONE', #6877, .T. ) ;
#40798 = ADVANCED_FACE ( 'NONE', ( #19350 ), #41285, .T. ) ;
#40799 = DIRECTION ( 'NONE',  ( -5.782411586589351722E-16, -1.000000000000000000, 0.000000000000000000 ) ) ;
#40800 = CARTESIAN_POINT ( 'NONE',  ( -92.90499999999997272, 2.607480562269068880, -8.024999999999993250 ) ) ;
#40801 = FILL_AREA_STYLE ('',( #68206 ) ) ;
#40802 = SURFACE_SIDE_STYLE ('',( #63269 ) ) ;
#40803 = VECTOR ( 'NONE', #63897, 1000.000000000000000 ) ;
#40804 = VECTOR ( 'NONE', #34777, 1000.000000000000000 ) ;
#40805 = CARTESIAN_POINT ( 'NONE',  ( -91.04499999999998749, 7.632228543268600340, 2.479861379858949277 ) ) ;
#40806 = CARTESIAN_POINT ( 'NONE',  ( -5.598654528085806881, 119.8549999999999898, -7.705886871421374629 ) ) ;
#40807 = CARTESIAN_POINT ( 'NONE',  ( -70.04499999999998749, 7.632228543268600340, 2.479861379858949277 ) ) ;
#40808 = AXIS2_PLACEMENT_3D ( 'NONE', #49100, #21998, #38203 ) ;
#40809 = CARTESIAN_POINT ( 'NONE',  ( 31.00000000000000000, 15.00000000000000000, -79.00402776293826435 ) ) ;
#40810 = CARTESIAN_POINT ( 'NONE',  ( -56.00707362346614815, -8.102448949553174629, -5.886773742842741797 ) ) ;
#40811 = PLANE ( 'NONE',  #46220 ) ;
#40812 = MECHANICAL_DESIGN_GEOMETRIC_PRESENTATION_REPRESENTATION (  '', ( #16106 ), #57656 ) ;
#40813 = DIRECTION ( 'NONE',  ( 0.000000000000000000, 0.000000000000000000, 1.000000000000000000 ) ) ;
#40814 = ORIENTED_EDGE ( 'NONE', *, *, #68246, .T. ) ;
#40815 = CARTESIAN_POINT ( 'NONE',  ( -115.4929263765338021, -8.102448949553172852, 5.886773742842742685 ) ) ;
#40816 = CARTESIAN_POINT ( 'NONE',  ( -127.7949999999999875, 2.607480562269068880, -8.024999999999993250 ) ) ;
#40817 = FACE_OUTER_BOUND ( 'NONE', #24634, .T. ) ;
#40818 = DIRECTION ( 'NONE',  ( -1.000000000000000000, 0.000000000000000000, 0.000000000000000000 ) ) ;
#40820 = DIRECTION ( 'NONE',  ( -1.000000000000000000, 0.000000000000000000, 0.000000000000000000 ) ) ;
#40819 = CARTESIAN_POINT ( 'NONE',  ( -75.75000000000000000, -3.000000000000000000, 7.000000000000001776 ) ) ;
#40821 = CARTESIAN_POINT ( 'NONE',  ( -75.50000000000000000, -6.499999999999992006, 3.000000000000000000 ) ) ;
#40822 = ORIENTED_EDGE ( 'NONE', *, *, #20171, .T. ) ;
#40824 = ORIENTED_EDGE ( 'NONE', *, *, #33839, .T. ) ;
#40823 = TOROIDAL_SURFACE ( 'NONE', #65543, 14.49999999999999822, 0.5000000000000000000 ) ;
#40825 = DIRECTION ( 'NONE',  ( -1.000000000000000000, 0.000000000000000000, 1.300977106640434891E-16 ) ) ;
#40826 = EDGE_CURVE ( 'NONE', #2827, #2682, #59197, .T. ) ;
#40827 = AXIS2_PLACEMENT_3D ( 'NONE', #39562, #48130, #2159 ) ;
#40828 = DIRECTION ( 'NONE',  ( -1.000000000000000000, 0.000000000000000000, 0.000000000000000000 ) ) ;
#40829 = DIRECTION ( 'NONE',  ( -1.000000000000000000, 0.000000000000000000, 0.000000000000000000 ) ) ;
#40830 = CARTESIAN_POINT ( 'NONE',  ( 92.41620014002536720, 0.000000000000000000, -29.00402776293825724 ) ) ;
#40831 = ORIENTED_EDGE ( 'NONE', *, *, #30114, .T. ) ;
#40832 = CARTESIAN_POINT ( 'NONE',  ( -133.4049999999999727, -2.607480562269069768, 8.024999999999991473 ) ) ;
#40833 = VERTEX_POINT ( 'NONE', #8808 ) ;
#40834 = CARTESIAN_POINT ( 'NONE',  ( -125.3070736234661808, -10.01517768586948698, 6.132527647946031529E-16 ) ) ;
#40835 = ORIENTED_EDGE ( 'NONE', *, *, #55908, .F. ) ;
#40836 = DIRECTION ( 'NONE',  ( 1.000000000000000000, 0.000000000000000000, 0.000000000000000000 ) ) ;
#40837 = CARTESIAN_POINT ( 'NONE',  ( -60.00000000000000000, -2.024042244987997205E-14, 11.50000000000003020 ) ) ;
#40838 = VERTEX_POINT ( 'NONE', #9172 ) ;
#40839 = COLOUR_RGB ( '', 0.72549020, 0.75294118, 0.79215686) ;
#40840 = SURFACE_STYLE_USAGE ( .BOTH. , #18981 ) ;
#40841 = CARTESIAN_POINT ( 'NONE',  ( -5.598654528085808657, 143.6449999999999818, 7.705886871421373741 ) ) ;
#40842 = DIRECTION ( 'NONE',  ( 0.000000000000000000, 1.000000000000000000, 0.000000000000000000 ) ) ;
#40843 = AXIS2_PLACEMENT_3D ( 'NONE', #24620, #21801, #16550 ) ;
#40844 = PRODUCT_RELATED_PRODUCT_CATEGORY ( 'part', '', ( #20359 ) ) ;
#40845 = ORIENTED_EDGE ( 'NONE', *, *, #3352, .T. ) ;
#40846 = EDGE_CURVE ( 'NONE', #60416, #36619, #46131, .T. ) ;
#40847 = CARTESIAN_POINT ( 'NONE',  ( -54.05707362346618083, 0.000000000000000000, 9.524999999999991473 ) ) ;
#40848 = CARTESIAN_POINT ( 'NONE',  ( -3.094860106618432471, 137.7049999999999841, -9.525000000000000355 ) ) ;
#40849 = SURFACE_STYLE_FILL_AREA ( #13374 ) ;
#40850 = EDGE_CURVE ( 'NONE', #25927, #2411, #29917, .T. ) ;
#40851 = AXIS2_PLACEMENT_3D ( 'NONE', #53440, #5222, #26667 ) ;
#40852 = ORIENTED_EDGE ( 'NONE', *, *, #3371, .T. ) ;
#40853 = CARTESIAN_POINT ( 'NONE',  ( 0.000000000000000000, 119.9429263765338050, -8.025000000000000355 ) ) ;
#40854 = FILL_AREA_STYLE ('',( #14098 ) ) ;
#40855 = ADVANCED_FACE ( 'NONE', ( #36274 ), #56292, .F. ) ;
#40856 = MECHANICAL_DESIGN_GEOMETRIC_PRESENTATION_REPRESENTATION (  '', ( #43086 ), #43132 ) ;
#40857 = LINE ( 'NONE', #3123, #67667 ) ;
#40858 = CARTESIAN_POINT ( 'NONE',  ( 69.74999999999998579, 36.75000000000000000, 3.000000000000000000 ) ) ;
#40859 = EDGE_CURVE ( 'NONE', #64235, #10212, #51400, .T. ) ;
#40860 = VERTEX_POINT ( 'NONE', #56656 ) ;
#40861 = DIRECTION ( 'NONE',  ( -0.7071067811865474617, 8.659560562354932858E-17, 0.7071067811865474617 ) ) ;
#40862 = ORIENTED_EDGE ( 'NONE', *, *, #8766, .T. ) ;
#40863 = FACE_OUTER_BOUND ( 'NONE', #37393, .T. ) ;
#40864 = CARTESIAN_POINT ( 'NONE',  ( 20.54889675933014814, 114.6603872790887095, 10.28544290717500509 ) ) ;
#40865 = LINE ( 'NONE', #55961, #25098 ) ;
#40866 = CARTESIAN_POINT ( 'NONE',  ( -154.2549999999999955, -4.716976649647092401, 6.492361379858946790 ) ) ;
#40867 = EDGE_LOOP ( 'NONE', ( #5882, #61783, #26753, #15400 ) ) ;
#40868 =( LENGTH_UNIT ( ) NAMED_UNIT ( * ) SI_UNIT ( .MILLI., .METRE. ) );
#40869 = AXIS2_PLACEMENT_3D ( 'NONE', #54069, #53056, #49172 ) ;
#40870 = MECHANICAL_DESIGN_GEOMETRIC_PRESENTATION_REPRESENTATION (  '', ( #28446 ), #58810 ) ;
#40871 = EDGE_CURVE ( 'NONE', #1278, #62287, #63735, .T. ) ;
#40872 = SURFACE_STYLE_FILL_AREA ( #55966 ) ;
#40873 = CARTESIAN_POINT ( 'NONE',  ( -8.437984349512095861, 151.8070736234661524, -5.166775262442723748E-16 ) ) ;
#40874 = CARTESIAN_POINT ( 'NONE',  ( 75.00000000000000000, 20.33294439366000006, 6.261747904192467296 ) ) ;
#40875 = PRESENTATION_STYLE_ASSIGNMENT (( #9885 ) ) ;
#40876 = VERTEX_POINT ( 'NONE', #25663 ) ;
#40877 = SURFACE_STYLE_USAGE ( .BOTH. , #45801 ) ;
#40879 = ADVANCED_FACE ( 'NONE', ( #40158 ), #45804, .T. ) ;
#40878 = ORIENTED_EDGE ( 'NONE', *, *, #13985, .F. ) ;
#40880 = DIRECTION ( 'NONE',  ( -0.000000000000000000, 0.000000000000000000, -1.000000000000000000 ) ) ;
#40881 = SURFACE_STYLE_FILL_AREA ( #20061 ) ;
#40882 = CARTESIAN_POINT ( 'NONE',  ( -78.95499999999998408, -7.632228543268599452, 2.479861379858951054 ) ) ;
#40883 = VERTEX_POINT ( 'NONE', #8124 ) ;
#40884 = AXIS2_PLACEMENT_3D ( 'NONE', #35870, #57316, #4530 ) ;
#40885 = CARTESIAN_POINT ( 'NONE',  ( -123.7429263765338021, -5.598654528085803328, -7.705886871421366635 ) ) ;
#40886 = CARTESIAN_POINT ( 'NONE',  ( 57.00000000000000000, 16.00000000000000000, -47.50402776293824303 ) ) ;
#40887 = ORIENTED_EDGE ( 'NONE', *, *, #66292, .F. ) ;
#40888 = CARTESIAN_POINT ( 'NONE',  ( 6.123233995736766282E-16, 2.299999999999999822, 5.000000000000000000 ) ) ;
#40889 = DIRECTION ( 'NONE',  ( 0.5792071321891958391, 0.5736185108958186118, 0.5792071321891946178 ) ) ;
#40890 = MECHANICAL_DESIGN_GEOMETRIC_PRESENTATION_REPRESENTATION (  '', ( #24028 ), #45423 ) ;
#40891 = CARTESIAN_POINT ( 'NONE',  ( 9.058813317711337021, 138.5449999999999875, 2.943386871421375783 ) ) ;
#40892 = CARTESIAN_POINT ( 'NONE',  ( -93.44499999999999318, 0.000000000000000000, 8.024999999999991473 ) ) ;
#40893 =( NAMED_UNIT ( * ) SI_UNIT ( $, .STERADIAN. ) SOLID_ANGLE_UNIT ( ) );
#40894 = CIRCLE ( 'NONE', #10540, 1.000000000000000888 ) ;
#40895 = LINE ( 'NONE', #57744, #48328 ) ;
#40896 = EDGE_CURVE ( 'NONE', #29039, #24476, #60363, .T. ) ;
#40897 = MECHANICAL_DESIGN_GEOMETRIC_PRESENTATION_REPRESENTATION (  '', ( #66676 ), #10543 ) ;
#40898 = CARTESIAN_POINT ( 'NONE',  ( -41.03386404901051776, 107.6974965691265140, -3.186685921634084817 ) ) ;
#40899 = VERTEX_POINT ( 'NONE', #36967 ) ;
#40900 = CARTESIAN_POINT ( 'NONE',  ( -148.0429263765338135, -9.058813317711329915, -2.943386871421370898 ) ) ;
#40901 = PRESENTATION_LAYER_ASSIGNMENT (  '', '', ( #20630 ) ) ;
#40902 = SURFACE_STYLE_FILL_AREA ( #8527 ) ;
#40903 = DIRECTION ( 'NONE',  ( -0.000000000000000000, -1.000000000000000000, -0.000000000000000000 ) ) ;
#40904 = CARTESIAN_POINT ( 'NONE',  ( -157.1950000000000216, 8.437984349512085203, -1.550032578732815448E-15 ) ) ;
#40905 = VECTOR ( 'NONE', #24881, 1000.000000000000000 ) ;
#40906 = AXIS2_PLACEMENT_3D ( 'NONE', #25895, #19221, #47058 ) ;
#40907 = PRESENTATION_STYLE_ASSIGNMENT (( #67606 ) ) ;
#40908 = CARTESIAN_POINT ( 'NONE',  ( 49.12162162162162105, 13.70805908423323238, -10.00000000000000000 ) ) ;
#40909 = VERTEX_POINT ( 'NONE', #11224 ) ;
#40910 = DIRECTION ( 'NONE',  ( 1.000000000000000000, 0.000000000000000000, 0.000000000000000000 ) ) ;
#40912 = VERTEX_POINT ( 'NONE', #48212 ) ;
#40911 = AXIS2_PLACEMENT_3D ( 'NONE', #27465, #48991, #59136 ) ;
#40913 = CARTESIAN_POINT ( 'NONE',  ( 0.000000000000000000, 9.000000000000007105, 0.000000000000000000 ) ) ;
#40914 = AXIS2_PLACEMENT_3D ( 'NONE', #41754, #67402, #14646 ) ;
#40915 = DIRECTION ( 'NONE',  ( 0.000000000000000000, 0.000000000000000000, -1.000000000000000000 ) ) ;
#40916 = CARTESIAN_POINT ( 'NONE',  ( -172.5570736234661808, -1.166476076187852838E-15, -9.524999999999991473 ) ) ;
#40917 = CARTESIAN_POINT ( 'NONE',  ( -181.5570736234661808, -1.166476076187852838E-15, -9.524999999999991473 ) ) ;
#40918 = VERTEX_POINT ( 'NONE', #16197 ) ;
#40919 = CARTESIAN_POINT ( 'NONE',  ( -156.2049999999999841, -2.607480562269071545, -8.024999999999991473 ) ) ;
#40920 =( GEOMETRIC_REPRESENTATION_CONTEXT ( 3 ) GLOBAL_UNCERTAINTY_ASSIGNED_CONTEXT ( ( #62909 ) ) GLOBAL_UNIT_ASSIGNED_CONTEXT ( ( #53041, #63242, #36560 ) ) REPRESENTATION_CONTEXT ( 'NONE', 'WORKASPACE' ) );
#40921 = EDGE_LOOP ( 'NONE', ( #5473, #36604, #41471, #6811 ) ) ;
#40922 = CARTESIAN_POINT ( 'NONE',  ( 60.00000000000000000, 1.797044900979284448E-15, 11.50000000000003730 ) ) ;
#40923 = LINE ( 'NONE', #13809, #15235 ) ;
#40924 = ORIENTED_EDGE ( 'NONE', *, *, #13251, .T. ) ;
#40925 = AXIS2_PLACEMENT_3D ( 'NONE', #50839, #7237, #3283 ) ;
#40926 = LINE ( 'NONE', #66944, #68578 ) ;
#40927 = DIRECTION ( 'NONE',  ( 0.000000000000000000, -1.000000000000000000, 0.000000000000000000 ) ) ;
#40928 = CARTESIAN_POINT ( 'NONE',  ( -9.058813317711337021, 110.0449999999999875, -2.943386871421374895 ) ) ;
#40929 = VERTEX_POINT ( 'NONE', #69620 ) ;
#40930 = EDGE_CURVE ( 'NONE', #48045, #42659, #63658, .T. ) ;
#40931 = CARTESIAN_POINT ( 'NONE',  ( 48.00000000000000000, 99.99999999999992895, 7.500000000000000000 ) ) ;
#40932 = CARTESIAN_POINT ( 'NONE',  ( 3.094860106618431583, 112.2049999999999841, 9.525000000000000355 ) ) ;
#40933 = CARTESIAN_POINT ( 'NONE',  ( -73.55499999999997840, 0.000000000000000000, 8.024999999999991473 ) ) ;
#40934 = ORIENTED_EDGE ( 'NONE', *, *, #47742, .F. ) ;
#40935 = CARTESIAN_POINT ( 'NONE',  ( -5.598654528085808657, 138.7549999999999955, 7.705886871421373741 ) ) ;
#40936 = FACE_OUTER_BOUND ( 'NONE', #34037, .T. ) ;
#40937 = ADVANCED_FACE ( 'NONE', ( #259 ), #64350, .T. ) ;
#40938 = CARTESIAN_POINT ( 'NONE',  ( 19.89974874213239886, 114.9999999999999574, 10.50000000000000000 ) ) ;
#40939 = MECHANICAL_DESIGN_GEOMETRIC_PRESENTATION_REPRESENTATION (  '', ( #1526 ), #42063 ) ;
#40940 =( NAMED_UNIT ( * ) SI_UNIT ( $, .STERADIAN. ) SOLID_ANGLE_UNIT ( ) );
#40941 = CARTESIAN_POINT ( 'NONE',  ( 4.000000000000002665, 43.00000000000000000, -79.00402776293826435 ) ) ;
#40942 = ORIENTED_EDGE ( 'NONE', *, *, #14891, .T. ) ;
#40944 = FILL_AREA_STYLE_COLOUR ( '', #40791 ) ;
#40943 = VECTOR ( 'NONE', #5859, 1000.000000000000000 ) ;
#40945 = CARTESIAN_POINT ( 'NONE',  ( -6.759171781091400710, -2.392512705203732715, -2.292771058063876488 ) ) ;
#40946 = CARTESIAN_POINT ( 'NONE',  ( -55.04499999999998039, 7.632228543268600340, 2.479861379858949277 ) ) ;
#40947 = ORIENTED_EDGE ( 'NONE', *, *, #69423, .F. ) ;
#40948 = CARTESIAN_POINT ( 'NONE',  ( 31.28473954617955854, 42.96841842781390142, 45.59272046071828299 ) ) ;
#40949 =( GEOMETRIC_REPRESENTATION_CONTEXT ( 3 ) GLOBAL_UNCERTAINTY_ASSIGNED_CONTEXT ( ( #1707 ) ) GLOBAL_UNIT_ASSIGNED_CONTEXT ( ( #61396, #2248, #56842 ) ) REPRESENTATION_CONTEXT ( 'NONE', 'WORKASPACE' ) );
#40950 = VECTOR ( 'NONE', #53289, 999.9999999999998863 ) ;
#40951 = CARTESIAN_POINT ( 'NONE',  ( 0.000000000000000000, -1.999999999999999556, 0.000000000000000000 ) ) ;
#40952 = CYLINDRICAL_SURFACE ( 'NONE', #31876, 0.2500000000000002220 ) ;
#40953 = CIRCLE ( 'NONE', #45431, 0.5000000000000000000 ) ;
#40954 = FILL_AREA_STYLE ('',( #51139 ) ) ;
#40955 = ORIENTED_EDGE ( 'NONE', *, *, #63932, .T. ) ;
#40956 = CARTESIAN_POINT ( 'NONE',  ( 0.000000000000000000, 2.299999999999999822, 0.000000000000000000 ) ) ;
#40957 = EDGE_LOOP ( 'NONE', ( #40383, #43909, #53713 ) ) ;
#40958 = EDGE_CURVE ( 'NONE', #67110, #31971, #64889, .T. ) ;
#40959 = AXIS2_PLACEMENT_3D ( 'NONE', #52327, #3722, #4420 ) ;
#40960 = DIRECTION ( 'NONE',  ( 1.000000000000000000, 0.000000000000000000, 0.000000000000000000 ) ) ;
#40961 = CARTESIAN_POINT ( 'NONE',  ( -100.7049999999999841, 2.607480562269073321, 8.024999999999991473 ) ) ;
#40962 = ORIENTED_EDGE ( 'NONE', *, *, #52921, .T. ) ;
#40963 = LINE ( 'NONE', #62017, #40711 ) ;
#40964 = PRESENTATION_STYLE_ASSIGNMENT (( #35311 ) ) ;
#40965 = CARTESIAN_POINT ( 'NONE',  ( -144.9570736234661865, 9.058813317711329915, -2.943386871421373119 ) ) ;
#40966 = CIRCLE ( 'NONE', #49932, 4.999999999999997335 ) ;
#40967 = FACE_OUTER_BOUND ( 'NONE', #30066, .T. ) ;
#40968 = CARTESIAN_POINT ( 'NONE',  ( 5.598654528085805993, 141.2449999999999761, 7.705886871421374629 ) ) ;
#40969 = CARTESIAN_POINT ( 'NONE',  ( -77.90707362346617515, -3.094860106618429807, 9.524999999999991473 ) ) ;
#40970 = AXIS2_PLACEMENT_3D ( 'NONE', #55383, #43832, #18455 ) ;
#40971 = DIRECTION ( 'NONE',  ( 1.000000000000000000, -0.000000000000000000, 0.000000000000000000 ) ) ;
#40972 = CARTESIAN_POINT ( 'NONE',  ( 43.75000000000000000, 19.24999999999998224, -4.000000000000000000 ) ) ;
#40974 = CARTESIAN_POINT ( 'NONE',  ( -100.1929263765337907, -10.01517768586948698, 6.132527647946031529E-16 ) ) ;
#40973 = CARTESIAN_POINT ( 'NONE',  ( 0.000000000000000000, -2.500000000000000000, 0.000000000000000000 ) ) ;
#40975 = AXIS2_PLACEMENT_3D ( 'NONE', #2823, #12719, #40531 ) ;
#40976 = CARTESIAN_POINT ( 'NONE',  ( -118.1049999999999898, -6.826472737025115478, 4.959722759717900331 ) ) ;
#40978 = ADVANCED_FACE ( 'NONE', ( #37673 ), #21794, .F. ) ;
#40977 = DIRECTION ( 'NONE',  ( 0.000000000000000000, 0.000000000000000000, 1.000000000000000000 ) ) ;
#40979 = CARTESIAN_POINT ( 'NONE',  ( -5.598654528085806881, 109.7449999999999761, -7.705886871421374629 ) ) ;
#40980 = CARTESIAN_POINT ( 'NONE',  ( -128.6950000000000216, -8.437984349512085203, 5.166775262442717831E-16 ) ) ;
#40981 = COLOUR_RGB ( '', 0.66274510, 0.83137255, 0.94901961) ;
#40982 = AXIS2_PLACEMENT_3D ( 'NONE', #64521, #37839, #433 ) ;
#40983 = CARTESIAN_POINT ( 'NONE',  ( -120.4449999999999932, 0.000000000000000000, 8.024999999999991473 ) ) ;
#40984 = DIRECTION ( 'NONE',  ( 0.7071067811865549002, 0.000000000000000000, 0.7071067811865401342 ) ) ;
#40985 = ADVANCED_FACE ( 'NONE', ( #10204 ), #18796, .T. ) ;
#40986 = EDGE_LOOP ( 'NONE', ( #11742, #30572, #44814, #48277 ) ) ;
#40987 =( LENGTH_UNIT ( ) NAMED_UNIT ( * ) SI_UNIT ( .MILLI., .METRE. ) );
#40988 = DIRECTION ( 'NONE',  ( 0.000000000000000000, 0.000000000000000000, -1.000000000000000000 ) ) ;
#40989 = CARTESIAN_POINT ( 'NONE',  ( -173.2429263765338305, 5.598654528085804216, 7.705886871421366635 ) ) ;
#40990 = CARTESIAN_POINT ( 'NONE',  ( -47.99499999999998323, -6.826472737025115478, 4.959722759717900331 ) ) ;
#40991 = VECTOR ( 'NONE', #3094, 1000.000000000000000 ) ;
#40992 = AXIS2_PLACEMENT_3D ( 'NONE', #64184, #59236, #58568 ) ;
#40993 = DIRECTION ( 'NONE',  ( -0.000000000000000000, 1.000000000000000000, 0.000000000000000000 ) ) ;
#40994 = CARTESIAN_POINT ( 'NONE',  ( -0.3545099074454303167, -7.000000000000004441, -2.440407800158045118E-14 ) ) ;
#40995 = ORIENTED_EDGE ( 'NONE', *, *, #34394, .T. ) ;
#40996 = CARTESIAN_POINT ( 'NONE',  ( -83.24292637653380211, 5.598654528085804216, 7.705886871421366635 ) ) ;
#40997 = SHAPE_DEFINITION_REPRESENTATION ( #63040, #21315 ) ;
#40998 = CIRCLE ( 'NONE', #63416, 5.000000000000000000 ) ;
#40999 = TOROIDAL_SURFACE ( 'NONE', #42130, 18.50000000000000355, 0.5000000000000000000 ) ;
#41000 = LINE ( 'NONE', #35697, #9044 ) ;
#41001 = DIRECTION ( 'NONE',  ( 0.000000000000000000, 1.000000000000000000, -0.000000000000000000 ) ) ;
#41002 = ORIENTED_EDGE ( 'NONE', *, *, #62254, .T. ) ;
#41003 = CARTESIAN_POINT ( 'NONE',  ( -136.3429263765337964, -9.058813317711329915, 2.943386871421371787 ) ) ;
#41004 = EDGE_CURVE ( 'NONE', #9275, #45578, #13947, .T. ) ;
#41005 = DIRECTION ( 'NONE',  ( 1.000000000000000000, 0.000000000000000000, 0.000000000000000000 ) ) ;
#41006 = ORIENTED_EDGE ( 'NONE', *, *, #60125, .T. ) ;
#41007 = CARTESIAN_POINT ( 'NONE',  ( 6.887213563469345878, -2.329718218673042962, 6.070996185493596542 ) ) ;
#41008 = DIRECTION ( 'NONE',  ( -0.000000000000000000, -0.000000000000000000, 1.000000000000000000 ) ) ;
#41009 = CARTESIAN_POINT ( 'NONE',  ( 7.632228543268607446, 135.1570736234661467, 2.479861379858954606 ) ) ;
#41010 = DIRECTION ( 'NONE',  ( -0.000000000000000000, -1.000000000000000000, 0.000000000000000000 ) ) ;
#41011 = VECTOR ( 'NONE', #16500, 1000.000000000000000 ) ;
#41012 = VERTEX_POINT ( 'NONE', #54127 ) ;
#41013 = DIRECTION ( 'NONE',  ( -0.000000000000000000, 1.000000000000000000, -0.000000000000000000 ) ) ;
#41014 = CARTESIAN_POINT ( 'NONE',  ( -106.4049999999999727, -2.607480562269069768, 8.024999999999991473 ) ) ;
#41015 = DIRECTION ( 'NONE',  ( -0.000000000000000000, -0.000000000000000000, -1.000000000000000000 ) ) ;
#41016 = ORIENTED_EDGE ( 'NONE', *, *, #38075, .T. ) ;
#41017 = STYLED_ITEM ( 'NONE', ( #34442 ), #63755 ) ;
#41018 = EDGE_CURVE ( 'NONE', #9552, #417, #31641, .T. ) ;
#41019 = CARTESIAN_POINT ( 'NONE',  ( 16.00000000000001776, 42.00000000000000000, 29.68999999999999417 ) ) ;
#41020 = CARTESIAN_POINT ( 'NONE',  ( 8.437984349512095861, 150.3070736234661524, 1.550032578732816828E-15 ) ) ;
#41021 = STYLED_ITEM ( 'NONE', ( #17389 ), #48750 ) ;
#41022 = AXIS2_PLACEMENT_3D ( 'NONE', #54643, #60274, #23002 ) ;
#41023 = AXIS2_PLACEMENT_3D ( 'NONE', #47072, #68499, #31883 ) ;
#41024 = EDGE_CURVE ( 'NONE', #39381, #59067, #4553, .T. ) ;
#41025 = CARTESIAN_POINT ( 'NONE',  ( -70.85707362346617799, -5.598654528085803328, -7.705886871421366635 ) ) ;
#41026 = CARTESIAN_POINT ( 'NONE',  ( -78.74499999999997613, 4.716976649647094177, 6.492361379858945902 ) ) ;
#41027 = EDGE_LOOP ( 'NONE', ( #33951, #23777, #52267 ) ) ;
#41028 =( LENGTH_UNIT ( ) NAMED_UNIT ( * ) SI_UNIT ( .MILLI., .METRE. ) );
#41029 = EDGE_CURVE ( 'NONE', #49208, #57733, #58055, .T. ) ;
#41030 =( NAMED_UNIT ( * ) SI_UNIT ( $, .STERADIAN. ) SOLID_ANGLE_UNIT ( ) );
#41031 = UNCERTAINTY_MEASURE_WITH_UNIT (LENGTH_MEASURE( 1.000000000000000082E-05 ), #4126, 'distance_accuracy_value', 'NONE');
#41032 = ORIENTED_EDGE ( 'NONE', *, *, #45624, .T. ) ;
#41033 = CIRCLE ( 'NONE', #5046, 0.2500000000000002220 ) ;
#41034 = EDGE_CURVE ( 'NONE', #38125, #7596, #52779, .T. ) ;
#41035 = CARTESIAN_POINT ( 'NONE',  ( -65.99999999999998579, 50.00000000000000000, -11.50000000000000000 ) ) ;
#41036 = DIRECTION ( 'NONE',  ( -1.000000000000000000, -0.000000000000000000, -0.000000000000000000 ) ) ;
#41037 = ORIENTED_EDGE ( 'NONE', *, *, #7612, .F. ) ;
#41038 = SURFACE_STYLE_FILL_AREA ( #2625 ) ;
#41039 = VECTOR ( 'NONE', #46932, 1000.000000000000000 ) ;
#41040 = ORIENTED_EDGE ( 'NONE', *, *, #46482, .T. ) ;
#41041 = CARTESIAN_POINT ( 'NONE',  ( -149.9929263765338021, 8.102448949553172852, -5.886773742842744461 ) ) ;
#41042 = CARTESIAN_POINT ( 'NONE',  ( -174.0570736234661808, 0.000000000000000000, 9.524999999999991473 ) ) ;
#41043 = CARTESIAN_POINT ( 'NONE',  ( 31.00000000000002132, 43.00000000000000000, 74.38749456993815556 ) ) ;
#41044 = CARTESIAN_POINT ( 'NONE',  ( 9.058813317711338797, 117.8449999999999847, -2.943386871421372675 ) ) ;
#41045 = CIRCLE ( 'NONE', #47804, 5.000000000000004441 ) ;
#41046 = CARTESIAN_POINT ( 'NONE',  ( -105.8070736234661808, 10.01517768586948698, -1.839758294383808571E-15 ) ) ;
#41047 = DIRECTION ( 'NONE',  ( 5.782411586589351722E-16, -1.000000000000000000, -0.000000000000000000 ) ) ;
#41048 = AXIS2_PLACEMENT_3D ( 'NONE', #57203, #47049, #36128 ) ;
#41049 = ORIENTED_EDGE ( 'NONE', *, *, #25816, .T. ) ;
#41050 = CYLINDRICAL_SURFACE ( 'NONE', #11864, 4.999999999999997335 ) ;
#41051 = LINE ( 'NONE', #24141, #69410 ) ;
#41052 = CARTESIAN_POINT ( 'NONE',  ( -152.0050000000000239, 6.826472737025116366, 4.959722759717898555 ) ) ;
#41053 = CARTESIAN_POINT ( 'NONE',  ( -75.00000000000000000, 9.680388875877742549, 6.198302543666472708 ) ) ;
#41054 = CARTESIAN_POINT ( 'NONE',  ( -7.682360912638867667, 111.2596883495873925, -4.277065875361336644 ) ) ;
#41055 = CARTESIAN_POINT ( 'NONE',  ( -155.2450000000000045, -4.716976649647093289, -6.492361379858945902 ) ) ;
#41056 = CARTESIAN_POINT ( 'NONE',  ( -149.2449999999999761, -4.716976649647093289, -6.492361379858945902 ) ) ;
#41057 = VERTEX_POINT ( 'NONE', #4908 ) ;
#41058 = CARTESIAN_POINT ( 'NONE',  ( 8.250000000000001776, 30.99999999999998579, 3.750000000000000000 ) ) ;
#41059 = COLOUR_RGB ( '', 0.31764706, 0.68627451, 0.89019608) ;
#41060 = CARTESIAN_POINT ( 'NONE',  ( -65.00000000000000000, -1.962809905030629631E-14, -11.50000000000000355 ) ) ;
#41061 = DIRECTION ( 'NONE',  ( 0.000000000000000000, -1.000000000000000000, 0.000000000000000000 ) ) ;
#41062 = UNCERTAINTY_MEASURE_WITH_UNIT (LENGTH_MEASURE( 1.000000000000000082E-05 ), #47561, 'distance_accuracy_value', 'NONE');
#41063 = CARTESIAN_POINT ( 'NONE',  ( -67.55499999999999261, 0.000000000000000000, 8.024999999999991473 ) ) ;
#41064 = DIRECTION ( 'NONE',  ( 0.000000000000000000, 0.000000000000000000, -1.000000000000000000 ) ) ;
#41065 = LINE ( 'NONE', #61764, #53971 ) ;
#41066 = AXIS2_PLACEMENT_3D ( 'NONE', #20973, #69166, #15706 ) ;
#41067 = CARTESIAN_POINT ( 'NONE',  ( -64.19499999999999318, 8.437984349512086979, -1.550032578732815448E-15 ) ) ;
#41068 = CARTESIAN_POINT ( 'NONE',  ( -5.598654528085808657, 159.7549999999999670, 7.705886871421373741 ) ) ;
#41069 = CARTESIAN_POINT ( 'NONE',  ( -74.99999999999998579, 50.00000000000000000, -6.999999999999988454 ) ) ;
#41070 = AXIS2_PLACEMENT_3D ( 'NONE', #46744, #19939, #50929 ) ;
#41071 =( GEOMETRIC_REPRESENTATION_CONTEXT ( 3 ) GLOBAL_UNCERTAINTY_ASSIGNED_CONTEXT ( ( #14987 ) ) GLOBAL_UNIT_ASSIGNED_CONTEXT ( ( #62540, #47831, #62880 ) ) REPRESENTATION_CONTEXT ( 'NONE', 'WORKASPACE' ) );
#41072 = CARTESIAN_POINT ( 'NONE',  ( -155.6070736234661922, -8.102448949553174629, 5.886773742842742685 ) ) ;
#41073 = UNCERTAINTY_MEASURE_WITH_UNIT (LENGTH_MEASURE( 1.000000000000000082E-05 ), #38916, 'distance_accuracy_value', 'NONE');
#41074 = CARTESIAN_POINT ( 'NONE',  ( 15.99999999999999645, 130.6078173946806942, 43.74999999999997868 ) ) ;
#41075 = DIRECTION ( 'NONE',  ( 0.000000000000000000, -0.000000000000000000, 1.000000000000000000 ) ) ;
#41076 = DIRECTION ( 'NONE',  ( -1.000000000000000000, 0.000000000000000000, 0.000000000000000000 ) ) ;
#41077 = PRESENTATION_LAYER_ASSIGNMENT (  '', '', ( #12917 ) ) ;
#41078 = VECTOR ( 'NONE', #7086, 1000.000000000000000 ) ;
#41079 = EDGE_CURVE ( 'NONE', #11506, #15151, #26359, .T. ) ;
#41080 = DIRECTION ( 'NONE',  ( 0.000000000000000000, 0.000000000000000000, -1.000000000000000000 ) ) ;
#41081 = VERTEX_POINT ( 'NONE', #37324 ) ;
#41082 = ORIENTED_EDGE ( 'NONE', *, *, #67253, .T. ) ;
#41083 = DIRECTION ( 'NONE',  ( 0.000000000000000000, 0.000000000000000000, 1.000000000000000000 ) ) ;
#41084 = UNCERTAINTY_MEASURE_WITH_UNIT (LENGTH_MEASURE( 1.000000000000000082E-05 ), #786, 'distance_accuracy_value', 'NONE');
#41086 = FACE_OUTER_BOUND ( 'NONE', #946, .T. ) ;
#41085 = AXIS2_PLACEMENT_3D ( 'NONE', #50676, #55604, #28496 ) ;
#41087 = EDGE_CURVE ( 'NONE', #3199, #57410, #58731, .T. ) ;
#41088 = EDGE_CURVE ( 'NONE', #33026, #65139, #23180, .T. ) ;
#41089 = STYLED_ITEM ( 'NONE', ( #60655 ), #32465 ) ;
#41090 = CARTESIAN_POINT ( 'NONE',  ( 31.00000000000000711, 15.00000000000000711, -36.50000000000000000 ) ) ;
#41091 = CARTESIAN_POINT ( 'NONE',  ( -45.00000000000000000, 7.967158085982124049, 7.000000000000001776 ) ) ;
#41092 = ADVANCED_FACE ( 'NONE', ( #55522 ), #17238, .T. ) ;
#41093 = FILL_AREA_STYLE_COLOUR ( '', #49894 ) ;
#41094 = ORIENTED_EDGE ( 'NONE', *, *, #26170, .F. ) ;
#41095 = VERTEX_POINT ( 'NONE', #23498 ) ;
#41096 =( NAMED_UNIT ( * ) PLANE_ANGLE_UNIT ( ) SI_UNIT ( $, .RADIAN. ) );
#41097 = CARTESIAN_POINT ( 'NONE',  ( 18.00000000000000711, 33.74999999999999289, 4.000000000000000000 ) ) ;
#41098 = EDGE_CURVE ( 'NONE', #68401, #37913, #42452, .T. ) ;
#41099 = EDGE_LOOP ( 'NONE', ( #36428, #43943, #17793, #69436 ) ) ;
#41100 = DIRECTION ( 'NONE',  ( 0.000000000000000000, 0.000000000000000000, -1.000000000000000000 ) ) ;
#41101 = DIRECTION ( 'NONE',  ( -0.000000000000000000, 3.469446951953611428E-15, 1.000000000000000000 ) ) ;
#41102 = ORIENTED_EDGE ( 'NONE', *, *, #60865, .T. ) ;
#41103 = EDGE_CURVE ( 'NONE', #34116, #42614, #10972, .T. ) ;
#41104 = EDGE_CURVE ( 'NONE', #44405, #69362, #50297, .T. ) ;
#41105 = DIRECTION ( 'NONE',  ( 0.000000000000000000, 1.000000000000000000, 0.000000000000000000 ) ) ;
#41106 = CARTESIAN_POINT ( 'NONE',  ( -106.4950000000000045, 6.826472737025113702, -4.959722759717902107 ) ) ;
#41107 = ORIENTED_EDGE ( 'NONE', *, *, #243, .F. ) ;
#41108 = FILL_AREA_STYLE_COLOUR ( '', #37826 ) ;
#41109 = CARTESIAN_POINT ( 'NONE',  ( -53.24292637653380211, 5.598654528085804216, 7.705886871421366635 ) ) ;
#41110 = EDGE_CURVE ( 'NONE', #17255, #65035, #68278, .T. ) ;
#41111 = CARTESIAN_POINT ( 'NONE',  ( 3.062509476195515228E-31, -2.500728763858896269E-15, -12.50000000000000000 ) ) ;
#41112 = ORIENTED_EDGE ( 'NONE', *, *, #12, .T. ) ;
#41113 = CARTESIAN_POINT ( 'NONE',  ( -6.826472737025120807, 141.3929263765338078, -4.959722759717907437 ) ) ;
#41114 = FACE_OUTER_BOUND ( 'NONE', #53634, .T. ) ;
#41115 = CARTESIAN_POINT ( 'NONE',  ( -12.74999999999999822, -4.000000000000000000, 18.00000000000000000 ) ) ;
#41116 = SURFACE_STYLE_USAGE ( .BOTH. , #46761 ) ;
#41117 = DIRECTION ( 'NONE',  ( 0.000000000000000000, 1.000000000000000000, 0.000000000000000000 ) ) ;
#41118 = ORIENTED_EDGE ( 'NONE', *, *, #48798, .T. ) ;
#41119 = FILL_AREA_STYLE ('',( #30156 ) ) ;
#41120 = VERTEX_POINT ( 'NONE', #12950 ) ;
#41121 = CARTESIAN_POINT ( 'NONE',  ( 4.041451884327376121, 7.000000000000007105, 1.082903768654759569 ) ) ;
#41122 = VECTOR ( 'NONE', #62764, 1000.000000000000000 ) ;
#41123 = DIRECTION ( 'NONE',  ( 0.000000000000000000, 0.000000000000000000, 1.000000000000000000 ) ) ;
#41124 = CARTESIAN_POINT ( 'NONE',  ( 6.000000000000017764, 43.00000000000000000, -35.50000000000000000 ) ) ;
#41125 = DIRECTION ( 'NONE',  ( -1.000000000000000000, -0.000000000000000000, -0.000000000000000000 ) ) ;
#41126 = CARTESIAN_POINT ( 'NONE',  ( -121.1050000000000040, -6.826472737025115478, 4.959722759717900331 ) ) ;
#41127 = FACE_OUTER_BOUND ( 'NONE', #65537, .T. ) ;
#41128 = CARTESIAN_POINT ( 'NONE',  ( 74.99999999999998579, 50.00000000000000000, 9.500000000000000000 ) ) ;
#41129 = LINE ( 'NONE', #62536, #54241 ) ;
#41130 = CARTESIAN_POINT ( 'NONE',  ( 61.74999999999998579, 31.24999999999999289, -3.750000000000000000 ) ) ;
#41131 = SURFACE_STYLE_FILL_AREA ( #46781 ) ;
#41132 = EDGE_LOOP ( 'NONE', ( #5603, #33696, #10496, #7188 ) ) ;
#41133 = ORIENTED_EDGE ( 'NONE', *, *, #59374, .T. ) ;
#41134 = CARTESIAN_POINT ( 'NONE',  ( 13.25000000000000355, 28.24999999999998934, -3.750000000000000000 ) ) ;
#41135 = SURFACE_STYLE_FILL_AREA ( #15436 ) ;
#41136 = DIRECTION ( 'NONE',  ( -1.000000000000000000, 0.000000000000000000, 0.000000000000000000 ) ) ;
#41137 = ORIENTED_EDGE ( 'NONE', *, *, #34461, .F. ) ;
#41138 = SURFACE_STYLE_USAGE ( .BOTH. , #39752 ) ;
#41139 = CARTESIAN_POINT ( 'NONE',  ( -176.0049999999999670, 6.826472737025116366, 4.959722759717898555 ) ) ;
#41140 = CARTESIAN_POINT ( 'NONE',  ( -91.34292637653381064, -9.058813317711329915, 2.943386871421371787 ) ) ;
#41141 = FACE_OUTER_BOUND ( 'NONE', #13923, .T. ) ;
#41142 = PRESENTATION_LAYER_ASSIGNMENT (  '', '', ( #33229 ) ) ;
#41143 = CARTESIAN_POINT ( 'NONE',  ( -58.40707362346616094, 3.094860106618428031, -9.524999999999993250 ) ) ;
#41144 = PRESENTATION_LAYER_ASSIGNMENT (  '', '', ( #38890 ) ) ;
#41145 = CARTESIAN_POINT ( 'NONE',  ( -179.8449999999999989, -7.632228543268599452, 2.479861379858951054 ) ) ;
#41146 = FACE_OUTER_BOUND ( 'NONE', #10959, .T. ) ;
#41147 = COLOUR_RGB ( '', 0.08235294, 0.09019608, 0.10196078) ;
#41148 = EDGE_LOOP ( 'NONE', ( #12584, #3187, #5743, #13844 ) ) ;
#41149 = EDGE_CURVE ( 'NONE', #48589, #61721, #60104, .T. ) ;
#41150 = LINE ( 'NONE', #24917, #16759 ) ;
#41151 = CARTESIAN_POINT ( 'NONE',  ( -195.0000000000000000, 0.000000000000000000, 9.524999999999991473 ) ) ;
#41152 = CARTESIAN_POINT ( 'NONE',  ( -96.95499999999998408, -7.632228543268599452, 2.479861379858951054 ) ) ;
#41153 = CARTESIAN_POINT ( 'NONE',  ( 8.752505052433008359, 154.4999999999998863, 3.782828924242557900 ) ) ;
#41154 = CARTESIAN_POINT ( 'NONE',  ( 15.98999599679679839, 146.9999999999999716, 9.500000000000000000 ) ) ;
#41155 = DIRECTION ( 'NONE',  ( 1.000000000000000000, 0.000000000000000000, 0.000000000000000000 ) ) ;
#41156 = CARTESIAN_POINT ( 'NONE',  ( -95.09499999999998465, -2.607480562269071545, -8.024999999999991473 ) ) ;
#41157 = CARTESIAN_POINT ( 'NONE',  ( -8.102448949553181734, 132.0049999999999386, -5.886773742842749790 ) ) ;
#41158 = CARTESIAN_POINT ( 'NONE',  ( -64.79500000000000171, 2.607480562269068880, -8.024999999999993250 ) ) ;
#41159 = DIRECTION ( 'NONE',  ( 1.000000000000000000, 0.000000000000000000, 0.000000000000000000 ) ) ;
#41160 = CARTESIAN_POINT ( 'NONE',  ( -55.55707362346618083, -1.166476076187852838E-15, -9.524999999999991473 ) ) ;
#41161 = DIRECTION ( 'NONE',  ( -0.7239014318314619389, -0.3935725838164222390, -0.5666280422467853128 ) ) ;
#41162 = UNCERTAINTY_MEASURE_WITH_UNIT (LENGTH_MEASURE( 1.000000000000000082E-05 ), #18197, 'distance_accuracy_value', 'NONE');
#41163 = DIRECTION ( 'NONE',  ( 0.000000000000000000, 0.000000000000000000, -1.000000000000000000 ) ) ;
#41164 = AXIS2_PLACEMENT_3D ( 'NONE', #9373, #4056, #68814 ) ;
#41165 = ORIENTED_EDGE ( 'NONE', *, *, #5658, .T. ) ;
#41166 = CARTESIAN_POINT ( 'NONE',  ( -116.5429263765338135, 9.058813317711329915, 2.943386871421369566 ) ) ;
#41167 = PRODUCT_DEFINITION_SHAPE ( 'NONE', 'NONE',  #48158 ) ;
#41168 = CARTESIAN_POINT ( 'NONE',  ( -128.9950000000000045, -6.826472737025115478, 4.959722759717900331 ) ) ;
#41169 =( NAMED_UNIT ( * ) SI_UNIT ( $, .STERADIAN. ) SOLID_ANGLE_UNIT ( ) );
#41170 = AXIS2_PLACEMENT_3D ( 'NONE', #15763, #47095, #41823 ) ;
#41171 = EDGE_CURVE ( 'NONE', #58314, #58151, #44711, .T. ) ;
#41173 = CARTESIAN_POINT ( 'NONE',  ( -12.72792206135785698, 115.4999999999999574, -10.50000000000000000 ) ) ;
#41172 = DIRECTION ( 'NONE',  ( 0.000000000000000000, 0.000000000000000000, -1.000000000000000000 ) ) ;
#41174 = COLOUR_RGB ( '', 0.72549020, 0.75294118, 0.79215686) ;
#41175 = DIRECTION ( 'NONE',  ( -1.000000000000000000, -1.084202172485503448E-16, 0.000000000000000000 ) ) ;
#41176 = VERTEX_POINT ( 'NONE', #45012 ) ;
#41177 = VERTEX_POINT ( 'NONE', #28773 ) ;
#41178 = CARTESIAN_POINT ( 'NONE',  ( 0.000000000000000000, 2.500000000000000000, 3.500000000000003553 ) ) ;
#41179 = UNCERTAINTY_MEASURE_WITH_UNIT (LENGTH_MEASURE( 1.000000000000000082E-05 ), #12292, 'distance_accuracy_value', 'NONE');
#41180 = ADVANCED_FACE ( 'NONE', ( #7346 ), #39377, .T. ) ;
#41181 = DIRECTION ( 'NONE',  ( 0.000000000000000000, 0.000000000000000000, -1.000000000000000000 ) ) ;
#41182 = DIRECTION ( 'NONE',  ( -0.000000000000000000, -0.000000000000000000, 1.000000000000000000 ) ) ;
#41183 = DIRECTION ( 'NONE',  ( 0.000000000000000000, -0.000000000000000000, -1.000000000000000000 ) ) ;
#41184 = ORIENTED_EDGE ( 'NONE', *, *, #27339, .F. ) ;
#41185 = CARTESIAN_POINT ( 'NONE',  ( -131.3050000000000068, 8.437984349512086979, -1.550032578732815448E-15 ) ) ;
#41186 = ORIENTED_EDGE ( 'NONE', *, *, #55202, .F. ) ;
#41187 = DIRECTION ( 'NONE',  ( 0.000000000000000000, 0.000000000000000000, -1.000000000000000000 ) ) ;
#41188 = VECTOR ( 'NONE', #34050, 1000.000000000000000 ) ;
#41189 = CARTESIAN_POINT ( 'NONE',  ( -118.5570736234661808, -1.166476076187852838E-15, -9.524999999999991473 ) ) ;
#41190 = VERTEX_POINT ( 'NONE', #54477 ) ;
#41191 = CARTESIAN_POINT ( 'NONE',  ( -172.4929263765338305, -8.102448949553174629, 5.886773742842742685 ) ) ;
#41192 = SURFACE_STYLE_FILL_AREA ( #57324 ) ;
#41193 = ORIENTED_EDGE ( 'NONE', *, *, #3621, .T. ) ;
#41194 = EDGE_CURVE ( 'NONE', #61072, #38783, #22134, .T. ) ;
#41195 = CARTESIAN_POINT ( 'NONE',  ( -195.0000000000000000, 0.000000000000000000, 9.524999999999991473 ) ) ;
#41196 = CARTESIAN_POINT ( 'NONE',  ( 3.094860106618435136, 139.2949999999999591, -9.525000000000000355 ) ) ;
#41197 = VERTEX_POINT ( 'NONE', #17575 ) ;
#41198 = CARTESIAN_POINT ( 'NONE',  ( -48.00000000000000000, 14.49137674618942562, -9.500000000000000000 ) ) ;
#41199 = CARTESIAN_POINT ( 'NONE',  ( -9.058813317711337021, 153.1549999999999727, -2.943386871421374895 ) ) ;
#41200 = CARTESIAN_POINT ( 'NONE',  ( -48.20499999999999829, -2.607480562269071545, -8.024999999999991473 ) ) ;
#41201 = EDGE_CURVE ( 'NONE', #20191, #43736, #14323, .T. ) ;
#41202 = VERTEX_POINT ( 'NONE', #927 ) ;
#41203 = CARTESIAN_POINT ( 'NONE',  ( 2.607480562269076430, 119.7929263765337993, -8.025000000000000355 ) ) ;
#41204 =( NAMED_UNIT ( * ) PLANE_ANGLE_UNIT ( ) SI_UNIT ( $, .RADIAN. ) );
#41205 = UNCERTAINTY_MEASURE_WITH_UNIT (LENGTH_MEASURE( 1.000000000000000082E-05 ), #36626, 'distance_accuracy_value', 'NONE');
#41206 = DIRECTION ( 'NONE',  ( 0.000000000000000000, 0.000000000000000000, 1.000000000000000000 ) ) ;
#41207 =( NAMED_UNIT ( * ) SI_UNIT ( $, .STERADIAN. ) SOLID_ANGLE_UNIT ( ) );
#41208 = DIRECTION ( 'NONE',  ( -1.000000000000000000, -7.709882115452468306E-16, 0.000000000000000000 ) ) ;
#41209 =( LENGTH_UNIT ( ) NAMED_UNIT ( * ) SI_UNIT ( .MILLI., .METRE. ) );
#41210 = EDGE_LOOP ( 'NONE', ( #18566, #44267, #43968, #4992 ) ) ;
#41211 = CARTESIAN_POINT ( 'NONE',  ( -7.766025168014158986, 0.5488498361408529203, 0.7660251680141585418 ) ) ;
#41212 = EDGE_LOOP ( 'NONE', ( #3279, #43937, #25476, #19801, #39433, #33385, #55767, #4267, #31823, #49748, #64541, #2857, #59424 ) ) ;
#41213 = CARTESIAN_POINT ( 'NONE',  ( -57.74292637653380211, -5.598654528085803328, -7.705886871421366635 ) ) ;
#41214 = CARTESIAN_POINT ( 'NONE',  ( 4.041451884327377897, 2.500000000000000000, 7.000000000000000888 ) ) ;
#41215 = CARTESIAN_POINT ( 'NONE',  ( -149.3049999999999500, 8.437984349512085203, -1.550032578732815448E-15 ) ) ;
#41216 = EDGE_LOOP ( 'NONE', ( #47902, #67195, #63203, #19600 ) ) ;
#41217 = FACE_OUTER_BOUND ( 'NONE', #4666, .T. ) ;
#41218 = UNCERTAINTY_MEASURE_WITH_UNIT (LENGTH_MEASURE( 1.000000000000000082E-05 ), #57272, 'distance_accuracy_value', 'NONE');
#41219 = DIRECTION ( 'NONE',  ( 8.659560562354941486E-17, -0.7071067811865469066, 0.7071067811865482389 ) ) ;
#41220 = CARTESIAN_POINT ( 'NONE',  ( -52.56905535911819527, -9.512283121613261727, 4.966208934664647856 ) ) ;
#41221 = DIRECTION ( 'NONE',  ( 1.000000000000000000, 0.000000000000000000, 0.000000000000000000 ) ) ;
#41222 = CYLINDRICAL_SURFACE ( 'NONE', #35387, 10.00000000000000533 ) ;
#41223 = ORIENTED_EDGE ( 'NONE', *, *, #52466, .F. ) ;
#41224 = ORIENTED_EDGE ( 'NONE', *, *, #15041, .F. ) ;
#41225 = VECTOR ( 'NONE', #49496, 1000.000000000000000 ) ;
#41226 = CARTESIAN_POINT ( 'NONE',  ( -62.75499999999998835, 4.716976649647091513, -6.492361379858946790 ) ) ;
#41227 = ORIENTED_EDGE ( 'NONE', *, *, #33197, .T. ) ;
#41228 = CARTESIAN_POINT ( 'NONE',  ( 22.00000000000002132, 50.00000000000000000, 55.00000000000000711 ) ) ;
#41229 = CARTESIAN_POINT ( 'NONE',  ( -90.35707362346617799, 5.598654528085804216, 7.705886871421366635 ) ) ;
#41230 = CARTESIAN_POINT ( 'NONE',  ( -162.0570736234661808, 0.000000000000000000, 9.524999999999991473 ) ) ;
#41231 = EDGE_LOOP ( 'NONE', ( #36717, #29093, #7376, #66240, #4906, #12203 ) ) ;
#41232 = ADVANCED_FACE ( 'NONE', ( #39040 ), #11921, .F. ) ;
#41233 = CARTESIAN_POINT ( 'NONE',  ( -75.00000000000000000, 9.291225313367323935, -6.640072787442762525 ) ) ;
#41234 = CARTESIAN_POINT ( 'NONE',  ( -74.50000000000000000, -2.220952357103124925E-14, -6.500000000000000000 ) ) ;
#41235 = DIRECTION ( 'NONE',  ( 0.000000000000000000, 0.000000000000000000, -1.000000000000000000 ) ) ;
#41236 = ADVANCED_FACE ( 'NONE', ( #34412 ), #44333, .T. ) ;
#41238 = CARTESIAN_POINT ( 'NONE',  ( 22.75000000000000711, 34.24999999999999289, -4.000000000000000000 ) ) ;
#41237 = LINE ( 'NONE', #14460, #40240 ) ;
#41239 = CONICAL_SURFACE ( 'NONE', #67018, 5.000000000000004441, 0.7853981633974579379 ) ;
#41240 = CARTESIAN_POINT ( 'NONE',  ( 8.102448949553183510, 144.9950000000000045, -5.886773742842746238 ) ) ;
#41241 = CARTESIAN_POINT ( 'NONE',  ( -96.44499999999999318, 0.000000000000000000, 8.024999999999991473 ) ) ;
#41242 = PRESENTATION_STYLE_ASSIGNMENT (( #52138 ) ) ;
#41243 = CARTESIAN_POINT ( 'NONE',  ( 39.74999999999999289, 16.24999999999997513, 4.000000000000000000 ) ) ;
#41244 = UNCERTAINTY_MEASURE_WITH_UNIT (LENGTH_MEASURE( 1.000000000000000082E-05 ), #12569, 'distance_accuracy_value', 'NONE');
#41245 = CARTESIAN_POINT ( 'NONE',  ( -6.826472737025120807, 144.3929263765338078, -4.959722759717907437 ) ) ;
#41246 = AXIS2_PLACEMENT_3D ( 'NONE', #22734, #11818, #54717 ) ;
#41247 = ORIENTED_EDGE ( 'NONE', *, *, #32392, .T. ) ;
#41248 = CARTESIAN_POINT ( 'NONE',  ( -142.4929263765338590, -8.102448949553172852, 5.886773742842742685 ) ) ;
#41249 =( LENGTH_UNIT ( ) NAMED_UNIT ( * ) SI_UNIT ( .MILLI., .METRE. ) );
#41250 = CARTESIAN_POINT ( 'NONE',  ( -160.7949999999999591, 2.607480562269068880, -8.024999999999993250 ) ) ;
#41251 = ADVANCED_FACE ( 'NONE', ( #55866 ), #25635, .F. ) ;
#41252 = ADVANCED_FACE ( 'NONE', ( #46396 ), #24196, .F. ) ;
#41253 = FILL_AREA_STYLE ('',( #57398 ) ) ;
#41254 = DIRECTION ( 'NONE',  ( 0.000000000000000000, 0.000000000000000000, -1.000000000000000000 ) ) ;
#41255 = FACE_OUTER_BOUND ( 'NONE', #65438, .T. ) ;
#41256 = VERTEX_POINT ( 'NONE', #24884 ) ;
#41257 = CARTESIAN_POINT ( 'NONE',  ( -8.437984349512095861, 129.6929263765338192, -5.166775262442723748E-16 ) ) ;
#41258 = ORIENTED_EDGE ( 'NONE', *, *, #2974, .T. ) ;
#41259 = DIRECTION ( 'NONE',  ( -1.000000000000000000, 1.156482317317866302E-16, 0.000000000000000000 ) ) ;
#41260 = UNCERTAINTY_MEASURE_WITH_UNIT (LENGTH_MEASURE( 1.000000000000000082E-05 ), #2355, 'distance_accuracy_value', 'NONE');
#41261 = EDGE_CURVE ( 'NONE', #25473, #50390, #40079, .T. ) ;
#41262 = FACE_OUTER_BOUND ( 'NONE', #50741, .T. ) ;
#41263 = CARTESIAN_POINT ( 'NONE',  ( -45.00000000000000000, 8.553059399042474809, 6.924772212933272719 ) ) ;
#41264 = CARTESIAN_POINT ( 'NONE',  ( 44.70264083260470755, 9.999999999999978684, 3.296021741783508041 ) ) ;
#41265 = EDGE_CURVE ( 'NONE', #24621, #7947, #9831, .T. ) ;
#41266 = VERTEX_POINT ( 'NONE', #19616 ) ;
#41267 = CARTESIAN_POINT ( 'NONE',  ( -158.0049999999999670, 6.826472737025115478, 4.959722759717899443 ) ) ;
#41268 = AXIS2_PLACEMENT_3D ( 'NONE', #5677, #39137, #59151 ) ;
#41269 = VERTEX_POINT ( 'NONE', #8391 ) ;
#41270 = FACE_OUTER_BOUND ( 'NONE', #22769, .T. ) ;
#41271 = LINE ( 'NONE', #14492, #23082 ) ;
#41272 = ORIENTED_EDGE ( 'NONE', *, *, #20766, .F. ) ;
#41274 = EDGE_CURVE ( 'NONE', #3117, #60568, #67455, .T. ) ;
#41273 = AXIS2_PLACEMENT_3D ( 'NONE', #35381, #56836, #67375 ) ;
#41275 = CARTESIAN_POINT ( 'NONE',  ( -8.102448949553181734, 110.4949999999999903, 5.886773742842747126 ) ) ;
#41276 = VERTEX_POINT ( 'NONE', #29100 ) ;
#41277 = DIRECTION ( 'NONE',  ( 0.000000000000000000, 0.000000000000000000, -1.000000000000000000 ) ) ;
#41278 = CARTESIAN_POINT ( 'NONE',  ( -3.094860106618432471, 122.7049999999999699, -9.525000000000000355 ) ) ;
#41279 = CARTESIAN_POINT ( 'NONE',  ( -76.25499999999999545, -4.716976649647092401, 6.492361379858946790 ) ) ;
#41280 = ADVANCED_FACE ( 'NONE', ( #41114 ), #67117, .F. ) ;
#41281 = FACE_OUTER_BOUND ( 'NONE', #32182, .T. ) ;
#41282 = ORIENTED_EDGE ( 'NONE', *, *, #44535, .T. ) ;
#41283 = CARTESIAN_POINT ( 'NONE',  ( 5.598654528085805993, 142.3549999999999898, 7.705886871421374629 ) ) ;
#41284 = UNCERTAINTY_MEASURE_WITH_UNIT (LENGTH_MEASURE( 1.000000000000000082E-05 ), #22159, 'distance_accuracy_value', 'NONE');
#41285 = TOROIDAL_SURFACE ( 'NONE', #19897, 27.49999999999999645, 0.5000000000000000000 ) ;
#41286 = FILL_AREA_STYLE ('',( #57434 ) ) ;
#41287 = SURFACE_STYLE_FILL_AREA ( #41998 ) ;
#41288 = ORIENTED_EDGE ( 'NONE', *, *, #5055, .T. ) ;
#41289 = CARTESIAN_POINT ( 'NONE',  ( -71.50000000000000000, 35.92875272052971525, -7.000000000000000000 ) ) ;
#41290 = DIRECTION ( 'NONE',  ( 0.000000000000000000, 1.000000000000000000, 0.000000000000000000 ) ) ;
#41291 = CARTESIAN_POINT ( 'NONE',  ( -181.4050000000000011, -2.607480562269069768, 8.024999999999991473 ) ) ;
#41292 = ORIENTED_EDGE ( 'NONE', *, *, #65617, .T. ) ;
#41293 = CARTESIAN_POINT ( 'NONE',  ( 8.487565887160195999, 111.4912942411369841, -0.9261705213944099180 ) ) ;
#41294 =( NAMED_UNIT ( * ) PLANE_ANGLE_UNIT ( ) SI_UNIT ( $, .RADIAN. ) );
#41295 = DIRECTION ( 'NONE',  ( 1.000000000000000000, 0.000000000000000000, 0.000000000000000000 ) ) ;
#41296 = FACE_OUTER_BOUND ( 'NONE', #67719, .T. ) ;
#41297 = EDGE_LOOP ( 'NONE', ( #26758, #48307, #38437, #31807 ) ) ;
#41298 = DIRECTION ( 'NONE',  ( -1.000000000000000000, -0.000000000000000000, -0.000000000000000000 ) ) ;
#41299 = VERTEX_POINT ( 'NONE', #6866 ) ;
#41300 = CARTESIAN_POINT ( 'NONE',  ( -100.5549999999999926, 0.000000000000000000, 8.024999999999991473 ) ) ;
#41301 = VERTEX_POINT ( 'NONE', #55759 ) ;
#41302 = DIRECTION ( 'NONE',  ( -0.000000000000000000, -0.000000000000000000, -1.000000000000000000 ) ) ;
#41303 = CARTESIAN_POINT ( 'NONE',  ( -141.8070736234661808, 10.01517768586948698, -1.839758294383808571E-15 ) ) ;
#41304 = CARTESIAN_POINT ( 'NONE',  ( 3.000000000000002665, 0.000000000000000000, 3.772833609257260986E-15 ) ) ;
#41305 = CARTESIAN_POINT ( 'NONE',  ( 9.058813317711337021, 150.5449999999999875, 2.943386871421375783 ) ) ;
#41306 = CARTESIAN_POINT ( 'NONE',  ( -78.80707362346618083, 10.01517768586948698, -1.839758294383808571E-15 ) ) ;
#41307 = EDGE_CURVE ( 'NONE', #66039, #35189, #8765, .T. ) ;
#41308 = DIRECTION ( 'NONE',  ( -1.000000000000000000, 0.000000000000000000, 0.000000000000000000 ) ) ;
#41309 = VERTEX_POINT ( 'NONE', #45235 ) ;
#41310 = LINE ( 'NONE', #30704, #34982 ) ;
#41311 = CARTESIAN_POINT ( 'NONE',  ( -15.33043442081600638, -10.90871211463571022, 5.000000000000000000 ) ) ;
#41312 = AXIS2_PLACEMENT_3D ( 'NONE', #28415, #54810, #7671 ) ;
#41313 = LINE ( 'NONE', #31755, #59436 ) ;
#41314 = AXIS2_PLACEMENT_3D ( 'NONE', #27050, #9891, #48587 ) ;
#41315 = CARTESIAN_POINT ( 'NONE',  ( -123.0549999999999926, -9.827790563157499189E-16, -8.024999999999991473 ) ) ;
#41316 = CIRCLE ( 'NONE', #55896, 0.2500000000000002220 ) ;
#41317 = PRESENTATION_STYLE_ASSIGNMENT (( #14213 ) ) ;
#41318 = CARTESIAN_POINT ( 'NONE',  ( 10.01517768586949231, 114.6949999999999932, 1.839758294383810543E-15 ) ) ;
#41319 = CARTESIAN_POINT ( 'NONE',  ( -124.3449999999999847, 7.632228543268599452, -2.479861379858951942 ) ) ;
#41320 = CARTESIAN_POINT ( 'NONE',  ( 18.25000000000000711, 33.74999999999999289, 3.750000000000000000 ) ) ;
#41321 = ORIENTED_EDGE ( 'NONE', *, *, #47634, .T. ) ;
#41322 =( NAMED_UNIT ( * ) SI_UNIT ( $, .STERADIAN. ) SOLID_ANGLE_UNIT ( ) );
#41323 = DIRECTION ( 'NONE',  ( 0.000000000000000000, 0.000000000000000000, 1.000000000000000000 ) ) ;
#41324 = ADVANCED_FACE ( 'NONE', ( #22359 ), #2209, .F. ) ;
#41325 = EDGE_LOOP ( 'NONE', ( #17907, #28381, #29724, #1963 ) ) ;
#41326 = CARTESIAN_POINT ( 'NONE',  ( -167.0070736234661695, -8.102448949553174629, -5.886773742842741797 ) ) ;
#41327 = CARTESIAN_POINT ( 'NONE',  ( -169.4929263765338305, -8.102448949553172852, 5.886773742842742685 ) ) ;
#41328 = CARTESIAN_POINT ( 'NONE',  ( 6.000000000000017764, 26.00000000000000355, 27.49999999999999645 ) ) ;
#41329 = CIRCLE ( 'NONE', #63733, 0.2500000000000002220 ) ;
#41330 = EDGE_CURVE ( 'NONE', #681, #26367, #32670, .T. ) ;
#41331 = AXIS2_PLACEMENT_3D ( 'NONE', #5582, #41900, #16544 ) ;
#41332 = ADVANCED_FACE ( 'NONE', ( #60328 ), #66298, .T. ) ;
#41333 = ADVANCED_FACE ( 'NONE', ( #13172 ), #65957, .F. ) ;
#41334 = CARTESIAN_POINT ( 'NONE',  ( -8.437984349512095861, 124.8070736234661382, -5.166775262442723748E-16 ) ) ;
#41335 = CARTESIAN_POINT ( 'NONE',  ( 21.25000000000001066, 24.99999999999998579, 3.750000000000000000 ) ) ;
#41336 = DIRECTION ( 'NONE',  ( -0.000000000000000000, -1.000000000000000000, -0.000000000000000000 ) ) ;
#41337 = VERTEX_POINT ( 'NONE', #17115 ) ;
#41338 = CARTESIAN_POINT ( 'NONE',  ( -90.29292637653378506, 3.094860106618428031, -9.524999999999993250 ) ) ;
#41339 = CONTEXT_DEPENDENT_SHAPE_REPRESENTATION ( #2326, #51373 ) ;
#41340 = CARTESIAN_POINT ( 'NONE',  ( -166.9429263765337907, 0.000000000000000000, 9.524999999999991473 ) ) ;
#41341 = CARTESIAN_POINT ( 'NONE',  ( -179.9929263765337737, 8.102448949553172852, -5.886773742842744461 ) ) ;
#41342 = CARTESIAN_POINT ( 'NONE',  ( -48.00000000000000000, 99.99999999999992895, -9.500000000000000000 ) ) ;
#41343 = DIRECTION ( 'NONE',  ( -0.000000000000000000, 1.000000000000000000, -0.000000000000000000 ) ) ;
#41344 = ADVANCED_FACE ( 'NONE', ( #39261 ), #39958, .T. ) ;
#41345 = CARTESIAN_POINT ( 'NONE',  ( -156.0570736234661808, 0.000000000000000000, 9.524999999999991473 ) ) ;
#41346 = ORIENTED_EDGE ( 'NONE', *, *, #42790, .F. ) ;
#41347 = CARTESIAN_POINT ( 'NONE',  ( -135.4429263765338192, -1.166476076187852838E-15, -9.524999999999991473 ) ) ;
#41348 = FACE_BOUND ( 'NONE', #26326, .T. ) ;
#41349 = EDGE_LOOP ( 'NONE', ( #30770, #61228, #63211, #36453 ) ) ;
#41350 = CARTESIAN_POINT ( 'NONE',  ( -111.2929263765347088, 3.094860106603101180, -9.525000000011131007 ) ) ;
#41351 = CARTESIAN_POINT ( 'NONE',  ( -7.632228543268608334, 136.9570736234661581, 2.479861379858952830 ) ) ;
#41352 = ORIENTED_EDGE ( 'NONE', *, *, #17278, .T. ) ;
#41353 = PRESENTATION_LAYER_ASSIGNMENT (  '', '', ( #1932 ) ) ;
#41354 = CARTESIAN_POINT ( 'NONE',  ( -101.3049999999999926, 8.437984349512086979, -1.550032578732815448E-15 ) ) ;
#41355 = CARTESIAN_POINT ( 'NONE',  ( 48.81081081081080697, 14.09971791521133255, 7.500000000000000000 ) ) ;
#41356 = TOROIDAL_SURFACE ( 'NONE', #69407, 29.50000000000000000, 0.5000000000000000000 ) ;
#41357 = ORIENTED_EDGE ( 'NONE', *, *, #59030, .T. ) ;
#41358 = PRESENTATION_LAYER_ASSIGNMENT (  '', '', ( #5359 ) ) ;
#41359 = SURFACE_STYLE_FILL_AREA ( #42767 ) ;
#41360 = FILL_AREA_STYLE ('',( #67725 ) ) ;
#41361 = ADVANCED_FACE ( 'NONE', ( #44207 ), #63154, .F. ) ;
#41362 = LINE ( 'NONE', #4354, #40950 ) ;
#41363 = ORIENTED_EDGE ( 'NONE', *, *, #69346, .F. ) ;
#41364 = PRESENTATION_LAYER_ASSIGNMENT (  '', '', ( #49233 ) ) ;
#41365 = DIRECTION ( 'NONE',  ( 0.000000000000000000, 0.000000000000000000, -1.000000000000000000 ) ) ;
#41366 = EDGE_CURVE ( 'NONE', #30380, #12003, #57889, .T. ) ;
#41367 = CARTESIAN_POINT ( 'NONE',  ( -68.84499999999998465, -7.632228543268599452, 2.479861379858951054 ) ) ;
#41368 = ORIENTED_EDGE ( 'NONE', *, *, #35986, .F. ) ;
#41369 = DIRECTION ( 'NONE',  ( -1.000000000000000000, 0.000000000000000000, 0.000000000000000000 ) ) ;
#41370 = PRESENTATION_STYLE_ASSIGNMENT (( #3665 ) ) ;
#41371 = DIRECTION ( 'NONE',  ( -0.000000000000000000, -0.000000000000000000, -1.000000000000000000 ) ) ;
#41372 = ORIENTED_EDGE ( 'NONE', *, *, #3127, .T. ) ;
#41373 = CARTESIAN_POINT ( 'NONE',  ( 71.99999999999998579, 64.07124727947029896, -7.500000000000000000 ) ) ;
#41374 = DIRECTION ( 'NONE',  ( 0.000000000000000000, 0.000000000000000000, 1.000000000000000000 ) ) ;
#41375 = AXIS2_PLACEMENT_3D ( 'NONE', #7227, #65261, #18124 ) ;
#41376 = CARTESIAN_POINT ( 'NONE',  ( -25.00000000000000355, 37.00000000000000000, 4.000000000000000000 ) ) ;
#41377 = CARTESIAN_POINT ( 'NONE',  ( -60.00000000000000000, -2.024042244987997205E-14, -6.500000000000000000 ) ) ;
#41378 = ORIENTED_EDGE ( 'NONE', *, *, #36046, .T. ) ;
#41379 = CARTESIAN_POINT ( 'NONE',  ( 0.000000000000000000, 0.000000000000000000, 0.000000000000000000 ) ) ;
#41380 = VERTEX_POINT ( 'NONE', #52619 ) ;
#41381 =( NAMED_UNIT ( * ) SI_UNIT ( $, .STERADIAN. ) SOLID_ANGLE_UNIT ( ) );
#41382 = CARTESIAN_POINT ( 'NONE',  ( 4.041451884327376121, 7.000000000000007105, 7.500000000000000000 ) ) ;
#41383 = CARTESIAN_POINT ( 'NONE',  ( -40.78947368421052744, 108.1536491499103647, 3.158024016299530334 ) ) ;
#41384 = CARTESIAN_POINT ( 'NONE',  ( -166.8570736234661922, -5.598654528085803328, -7.705886871421366635 ) ) ;
#41385 = CARTESIAN_POINT ( 'NONE',  ( 8.102448949553179958, 126.3949999999999818, 5.886773742842750679 ) ) ;
#41386 = CARTESIAN_POINT ( 'NONE',  ( -101.0070736234661695, -8.102448949553172852, -5.886773742842741797 ) ) ;
#41387 = CARTESIAN_POINT ( 'NONE',  ( -9.827790563157511022E-16, 112.4429263765338192, 8.025000000000000355 ) ) ;
#41388 = DIRECTION ( 'NONE',  ( -1.000000000000000000, -0.000000000000000000, -0.000000000000000000 ) ) ;
#41389 = EDGE_LOOP ( 'NONE', ( #9963, #48882, #56491, #37699 ) ) ;
#41390 = CARTESIAN_POINT ( 'NONE',  ( -195.0000000000000000, 0.000000000000000000, 0.000000000000000000 ) ) ;
#41391 = CARTESIAN_POINT ( 'NONE',  ( -105.5070736234661553, 8.102448949553176405, 5.886773742842740909 ) ) ;
#41393 = LINE ( 'NONE', #9372, #14465 ) ;
#41392 = CARTESIAN_POINT ( 'NONE',  ( -44.50000000000000000, 9.999999999999980460, -3.499999999999999112 ) ) ;
#41394 = CARTESIAN_POINT ( 'NONE',  ( 0.000000000000000000, 14.00000000000000000, -79.00402776293826435 ) ) ;
#41395 = CARTESIAN_POINT ( 'NONE',  ( -146.9049999999999727, 2.607480562269068880, -8.024999999999993250 ) ) ;
#41396 = DIRECTION ( 'NONE',  ( 0.000000000000000000, 0.000000000000000000, 1.000000000000000000 ) ) ;
#41397 = CARTESIAN_POINT ( 'NONE',  ( -5.805106041259629812, 111.0237597212471456, -6.890929992047162500 ) ) ;
#41398 = ADVANCED_BREP_SHAPE_REPRESENTATION ( '', ( #27198, #42840 ), #37272 ) ;
#41399 = ADVANCED_FACE ( 'NONE', ( #35390 ), #25504, .F. ) ;
#41400 = CARTESIAN_POINT ( 'NONE',  ( -150.4449999999999932, 0.000000000000000000, 8.024999999999991473 ) ) ;
#41401 = STYLED_ITEM ( 'NONE', ( #49638 ), #9839 ) ;
#41402 = CARTESIAN_POINT ( 'NONE',  ( -151.0449999999999875, 7.632228543268600340, 2.479861379858949277 ) ) ;
#41403 =( BOUNDED_CURVE ( )  B_SPLINE_CURVE ( 2, ( #46353, #45660, #19572, #54608, #5714, #48695, #398, #57560, #58865, #32127, #9389 ),
 .UNSPECIFIED., .F., .F. ) 
 B_SPLINE_CURVE_WITH_KNOTS ( ( 3, 2, 2, 2, 2, 3 ),
 ( 0.2065217391304298988, 0.2086956521739080916, 0.2108695652173863400, 0.2130434782608645328, 0.2152173913043427811, 0.2173913043478209739 ),
 .UNSPECIFIED. ) 
 CURVE ( )  GEOMETRIC_REPRESENTATION_ITEM ( )  RATIONAL_B_SPLINE_CURVE ( ( 1.000000000000109912, 0.9510565162950435081, 1.000000000000000000, 0.9510565162951535312, 1.000000000000000000, 0.9510565162951535312, 1.000000000000000000, 0.9510565162951535312, 1.000000000000000000, 0.9510565162952685503, 0.9999999999998849809 ) ) 
 REPRESENTATION_ITEM ( '' )  );
#41404 = ORIENTED_EDGE ( 'NONE', *, *, #59648, .F. ) ;
#41405 = FACE_OUTER_BOUND ( 'NONE', #27644, .T. ) ;
#41406 = DIRECTION ( 'NONE',  ( -1.000000000000000000, 0.000000000000000000, 0.000000000000000000 ) ) ;
#41407 = EDGE_CURVE ( 'NONE', #64348, #21270, #15025, .T. ) ;
#41408 = CARTESIAN_POINT ( 'NONE',  ( -61.25499999999998835, -4.716976649647092401, 6.492361379858946790 ) ) ;
#41409 = DIRECTION ( 'NONE',  ( 1.000000000000000000, -1.541976423090495436E-15, 0.000000000000000000 ) ) ;
#41410 = CARTESIAN_POINT ( 'NONE',  ( 29.00000000000002842, 42.58578643762690774, 89.58578643762690774 ) ) ;
#41411 = VECTOR ( 'NONE', #56759, 1000.000000000000000 ) ;
#41412 = STYLED_ITEM ( 'NONE', ( #26132 ), #66631 ) ;
#41413 = EDGE_CURVE ( 'NONE', #60416, #36711, #61503, .T. ) ;
#41414 = CARTESIAN_POINT ( 'NONE',  ( -60.29499999999998749, -2.607480562269069768, 8.024999999999991473 ) ) ;
#41415 = CARTESIAN_POINT ( 'NONE',  ( -5.598654528085806881, 155.8549999999999898, -7.705886871421374629 ) ) ;
#41416 = AXIS2_PLACEMENT_3D ( 'NONE', #35691, #57123, #8951 ) ;
#41417 = DIRECTION ( 'NONE',  ( 0.000000000000000000, 0.9984713486292863260, 0.05527174654752588234 ) ) ;
#41418 = AXIS2_PLACEMENT_3D ( 'NONE', #47448, #52687, #21700 ) ;
#41419 = CARTESIAN_POINT ( 'NONE',  ( 48.74999999999999289, 24.74999999999998579, -3.750000000000000000 ) ) ;
#41420 = CARTESIAN_POINT ( 'NONE',  ( -28.74999999999999645, -4.000000000000000000, 15.00000000000000178 ) ) ;
#41421 = DIRECTION ( 'NONE',  ( 0.000000000000000000, -0.000000000000000000, -1.000000000000000000 ) ) ;
#41422 = AXIS2_PLACEMENT_3D ( 'NONE', #61846, #19974, #62887 ) ;
#41423 = EDGE_CURVE ( 'NONE', #38572, #48124, #67381, .T. ) ;
#41424 = DIRECTION ( 'NONE',  ( -0.000000000000000000, -1.000000000000000000, -0.000000000000000000 ) ) ;
#41425 = FILL_AREA_STYLE_COLOUR ( '', #23864 ) ;
#41426 = ORIENTED_EDGE ( 'NONE', *, *, #7711, .T. ) ;
#41427 = ORIENTED_EDGE ( 'NONE', *, *, #51973, .F. ) ;
#41428 =( NAMED_UNIT ( * ) SI_UNIT ( $, .STERADIAN. ) SOLID_ANGLE_UNIT ( ) );
#41429 = AXIS2_PLACEMENT_3D ( 'NONE', #23288, #2465, #12363 ) ;
#41430 = CYLINDRICAL_SURFACE ( 'NONE', #55260, 16.00000000000000000 ) ;
#41431 = DIRECTION ( 'NONE',  ( 0.000000000000000000, 0.000000000000000000, 1.000000000000000000 ) ) ;
#41432 = ORIENTED_EDGE ( 'NONE', *, *, #3664, .F. ) ;
#41434 = ORIENTED_EDGE ( 'NONE', *, *, #68629, .F. ) ;
#41433 = AXIS2_PLACEMENT_3D ( 'NONE', #51063, #25937, #26288 ) ;
#41435 = SURFACE_STYLE_USAGE ( .BOTH. , #67802 ) ;
#41436 = ORIENTED_EDGE ( 'NONE', *, *, #57741, .F. ) ;
#41437 = CARTESIAN_POINT ( 'NONE',  ( -9.058813317711338797, 123.4549999999999841, 2.943386871421373563 ) ) ;
#41438 = CARTESIAN_POINT ( 'NONE',  ( -74.99999999999998579, 50.00000000000000000, 11.50000000000003730 ) ) ;
#41439 = ORIENTED_EDGE ( 'NONE', *, *, #2402, .T. ) ;
#41440 = AXIS2_PLACEMENT_3D ( 'NONE', #25277, #68202, #19980 ) ;
#41441 = COLOUR_RGB ( '', 0.72549020, 0.75294118, 0.79215686) ;
#41442 = DIRECTION ( 'NONE',  ( 0.000000000000000000, 0.000000000000000000, -1.000000000000000000 ) ) ;
#41443 = CARTESIAN_POINT ( 'NONE',  ( -105.8949999999999676, 6.826472737025116366, 4.959722759717898555 ) ) ;
#41444 = ORIENTED_EDGE ( 'NONE', *, *, #62409, .T. ) ;
#41445 = CARTESIAN_POINT ( 'NONE',  ( 0.000000000000000000, 14.00000000000000000, 79.00402776293826435 ) ) ;
#41446 = SURFACE_SIDE_STYLE ('',( #20301 ) ) ;
#41447 = DIRECTION ( 'NONE',  ( -1.000000000000000000, 0.000000000000000000, 0.000000000000000000 ) ) ;
#41448 = ORIENTED_EDGE ( 'NONE', *, *, #52042, .F. ) ;
#41449 = CARTESIAN_POINT ( 'NONE',  ( 0.000000000000000000, 155.9429263765338192, -8.025000000000000355 ) ) ;
#41450 = FACE_OUTER_BOUND ( 'NONE', #68572, .T. ) ;
#41451 = CIRCLE ( 'NONE', #60485, 0.5000000000000004441 ) ;
#41452 = PRESENTATION_LAYER_ASSIGNMENT (  '', '', ( #58161 ) ) ;
#41453 = DIRECTION ( 'NONE',  ( -1.000000000000000000, -1.074176415464006764E-16, 0.000000000000000000 ) ) ;
#41454 = CARTESIAN_POINT ( 'NONE',  ( 23.21231517720797655, 118.4999999999999716, 7.500000000000000000 ) ) ;
#41455 = ORIENTED_EDGE ( 'NONE', *, *, #44917, .T. ) ;
#41456 = DIRECTION ( 'NONE',  ( 0.000000000000000000, 1.000000000000000000, 0.000000000000000000 ) ) ;
#41457 = ORIENTED_EDGE ( 'NONE', *, *, #63605, .T. ) ;
#41458 = CARTESIAN_POINT ( 'NONE',  ( 20.99060317843563794, 114.7782486714346533, 10.00000000000000178 ) ) ;
#41459 = FILL_AREA_STYLE ('',( #46769 ) ) ;
#41460 = CARTESIAN_POINT ( 'NONE',  ( -18.25000000000000711, 33.99999999999999289, 3.750000000000000000 ) ) ;
#41461 = CARTESIAN_POINT ( 'NONE',  ( -125.1549999999999869, 7.632228543268600340, 2.479861379858949277 ) ) ;
#41462 = FILL_AREA_STYLE_COLOUR ( '', #63237 ) ;
#41463 = CARTESIAN_POINT ( 'NONE',  ( -74.97963758645435917, 36.02033812954885406, 9.659135740435630169 ) ) ;
#41464 =( NAMED_UNIT ( * ) SI_UNIT ( $, .STERADIAN. ) SOLID_ANGLE_UNIT ( ) );
#41465 = ORIENTED_EDGE ( 'NONE', *, *, #46983, .F. ) ;
#41466 = CIRCLE ( 'NONE', #34698, 0.2500000000000002220 ) ;
#41467 = VERTEX_POINT ( 'NONE', #19174 ) ;
#41468 = DIRECTION ( 'NONE',  ( 1.224646799147353454E-16, -1.000000000000000000, 0.000000000000000000 ) ) ;
#41469 = DIRECTION ( 'NONE',  ( 0.000000000000000000, 0.000000000000000000, -1.000000000000000000 ) ) ;
#41470 = CARTESIAN_POINT ( 'NONE',  ( 4.750000000000002665, 24.74999999999998579, -4.000000000000000000 ) ) ;
#41471 = ORIENTED_EDGE ( 'NONE', *, *, #57421, .F. ) ;
#41472 = CARTESIAN_POINT ( 'NONE',  ( -174.8050000000000068, -8.437984349512085203, 5.166775262442717831E-16 ) ) ;
#41473 = EDGE_CURVE ( 'NONE', #68888, #12986, #19534, .T. ) ;
#41474 = CARTESIAN_POINT ( 'NONE',  ( -50.00707362346616947, -8.102448949553172852, -5.886773742842741797 ) ) ;
#41475 = CARTESIAN_POINT ( 'NONE',  ( -175.9449999999999932, -9.827790563157499189E-16, -8.024999999999991473 ) ) ;
#41476 = DIRECTION ( 'NONE',  ( 0.000000000000000000, 0.000000000000000000, 1.000000000000000000 ) ) ;
#41477 = VERTEX_POINT ( 'NONE', #35731 ) ;
#41478 =( LENGTH_UNIT ( ) NAMED_UNIT ( * ) SI_UNIT ( .MILLI., .METRE. ) );
#41480 = SURFACE_SIDE_STYLE ('',( #56237 ) ) ;
#41479 = PRESENTATION_LAYER_ASSIGNMENT (  '', '', ( #7753 ) ) ;
#41481 = CARTESIAN_POINT ( 'NONE',  ( -10.66861100029810316, 11.73594037587654171, 2.518823584575576646 ) ) ;
#41482 = CARTESIAN_POINT ( 'NONE',  ( -95.00499999999998124, 6.826472737025116366, 4.959722759717898555 ) ) ;
#41483 = DIRECTION ( 'NONE',  ( 1.000000000000000000, -0.000000000000000000, -1.300977106640434891E-16 ) ) ;
#41484 = EDGE_CURVE ( 'NONE', #40244, #36166, #62664, .T. ) ;
#41485 = MECHANICAL_DESIGN_GEOMETRIC_PRESENTATION_REPRESENTATION (  '', ( #12207 ), #5468 ) ;
#41486 = ADVANCED_FACE ( 'NONE', ( #51916 ), #790, .F. ) ;
#41487 = CARTESIAN_POINT ( 'NONE',  ( -94.49499999999997613, 6.826472737025113702, -4.959722759717902107 ) ) ;
#41488 = CARTESIAN_POINT ( 'NONE',  ( -5.598654528085806881, 125.8549999999999898, -7.705886871421374629 ) ) ;
#41489 = CARTESIAN_POINT ( 'NONE',  ( -67.79499999999998749, 2.607480562269068880, -8.024999999999993250 ) ) ;
#41490 = EDGE_CURVE ( 'NONE', #26732, #9552, #43486, .T. ) ;
#41491 = CARTESIAN_POINT ( 'NONE',  ( -13.75000000000000533, 30.99999999999999289, 4.000000000000000000 ) ) ;
#41492 = VECTOR ( 'NONE', #44876, 1000.000000000000000 ) ;
#41493 = VECTOR ( 'NONE', #17147, 1000.000000000000000 ) ;
#41494 = CARTESIAN_POINT ( 'NONE',  ( -57.05707362346618083, 0.000000000000000000, 9.524999999999991473 ) ) ;
#41495 = EDGE_CURVE ( 'NONE', #40311, #34254, #64180, .T. ) ;
#41496 =( NAMED_UNIT ( * ) PLANE_ANGLE_UNIT ( ) SI_UNIT ( $, .RADIAN. ) );
#41497 = VECTOR ( 'NONE', #34382, 1000.000000000000000 ) ;
#41498 = PRESENTATION_LAYER_ASSIGNMENT (  '', '', ( #48239 ) ) ;
#41499 =( BOUNDED_CURVE ( )  B_SPLINE_CURVE ( 2, ( #53667, #20978, #5454, #47409, #48444, #135, #53348, #42473, #9752, #58604, #5815 ),
 .UNSPECIFIED., .F., .F. ) 
 B_SPLINE_CURVE_WITH_KNOTS ( ( 3, 2, 2, 2, 2, 3 ),
 ( 0.6739130434782450996, 0.6760869565217264565, 0.6782608695652079245, 0.6804347826086892814, 0.6826086956521707494, 0.6847826086956522174 ),
 .UNSPECIFIED. ) 
 CURVE ( )  GEOMETRIC_REPRESENTATION_ITEM ( )  RATIONAL_B_SPLINE_CURVE ( ( 1.000000000000354827, 0.9510565162947985929, 1.000000000000000000, 0.9510565162951535312, 1.000000000000000000, 0.9510565162951535312, 1.000000000000000000, 0.9510565162951535312, 1.000000000000000000, 0.9510565162951535312, 1.000000000000000000 ) ) 
 REPRESENTATION_ITEM ( '' )  );
#41500 = CARTESIAN_POINT ( 'NONE',  ( -87.50000000000000000, -6.499999999999990230, 21.00000000000000000 ) ) ;
#41501 = EDGE_LOOP ( 'NONE', ( #58896, #69228, #40423, #31174 ) ) ;
#41502 = EDGE_CURVE ( 'NONE', #61490, #12327, #50345, .T. ) ;
#41503 = CARTESIAN_POINT ( 'NONE',  ( -105.4429263765338050, -1.166476076187852838E-15, -9.524999999999991473 ) ) ;
#41504 = CARTESIAN_POINT ( 'NONE',  ( -131.8449999999999989, -7.632228543268599452, 2.479861379858951054 ) ) ;
#41505 = VECTOR ( 'NONE', #43684, 1000.000000000000000 ) ;
#41507 = CYLINDRICAL_SURFACE ( 'NONE', #62907, 4.999999999999990230 ) ;
#41506 = CARTESIAN_POINT ( 'NONE',  ( 44.99999999999977973, 147.4999999999999716, -9.500000000000000000 ) ) ;
#41508 =( LENGTH_UNIT ( ) NAMED_UNIT ( * ) SI_UNIT ( .MILLI., .METRE. ) );
#41509 = VERTEX_POINT ( 'NONE', #10396 ) ;
#41510 = MECHANICAL_DESIGN_GEOMETRIC_PRESENTATION_REPRESENTATION (  '', ( #53825 ), #46030 ) ;
#41511 = ORIENTED_EDGE ( 'NONE', *, *, #23598, .T. ) ;
#41512 = CARTESIAN_POINT ( 'NONE',  ( -45.75852489800470835, 8.825811131586496217, -6.400570753484253750 ) ) ;
#41513 = CARTESIAN_POINT ( 'NONE',  ( -135.4429263765338192, -1.166476076187852838E-15, -9.524999999999991473 ) ) ;
#41514 = AXIS2_PLACEMENT_3D ( 'NONE', #5703, #21557, #48684 ) ;
#41515 = FACE_OUTER_BOUND ( 'NONE', #42536, .T. ) ;
#41516 = CARTESIAN_POINT ( 'NONE',  ( -7.511572993685801073E-16, 2.500000000000000000, 7.000000000000000888 ) ) ;
#41517 = ORIENTED_EDGE ( 'NONE', *, *, #67171, .T. ) ;
#41518 = CARTESIAN_POINT ( 'NONE',  ( -118.5549999999999926, 0.000000000000000000, 8.024999999999991473 ) ) ;
#41519 = VERTEX_POINT ( 'NONE', #11056 ) ;
#41520 = CARTESIAN_POINT ( 'NONE',  ( -123.5070736234661837, 8.102448949553176405, 5.886773742842740909 ) ) ;
#41521 = EDGE_LOOP ( 'NONE', ( #34521, #20024, #65662, #35656 ) ) ;
#41522 = CARTESIAN_POINT ( 'NONE',  ( 2.000000000000008882, 26.00000000000000355, -24.00000000000000355 ) ) ;
#41523 = CARTESIAN_POINT ( 'NONE',  ( 60.00000000000000000, 1.797044900979284448E-15, -12.00000000000000000 ) ) ;
#41524 = VERTEX_POINT ( 'NONE', #37514 ) ;
#41525 = AXIS2_PLACEMENT_3D ( 'NONE', #19530, #30077, #39637 ) ;
#41527 = CARTESIAN_POINT ( 'NONE',  ( 22.00000000000000000, 43.00000000000000000, -90.00000000000000000 ) ) ;
#41526 = MECHANICAL_DESIGN_GEOMETRIC_PRESENTATION_REPRESENTATION (  '', ( #63982 ), #48266 ) ;
#41528 = CARTESIAN_POINT ( 'NONE',  ( -3.094860106618434248, 152.7949999999999591, 9.525000000000000355 ) ) ;
#41529 = VERTEX_POINT ( 'NONE', #48061 ) ;
#41530 = CARTESIAN_POINT ( 'NONE',  ( -1.166476076187854022E-15, 154.0550000000000068, 9.525000000000000355 ) ) ;
#41531 = CARTESIAN_POINT ( 'NONE',  ( 0.000000000000000000, 114.9999999999999574, 22.50000000000000000 ) ) ;
#41532 =( GEOMETRIC_REPRESENTATION_CONTEXT ( 3 ) GLOBAL_UNCERTAINTY_ASSIGNED_CONTEXT ( ( #16419 ) ) GLOBAL_UNIT_ASSIGNED_CONTEXT ( ( #7799, #7470, #1431 ) ) REPRESENTATION_CONTEXT ( 'NONE', 'WORKASPACE' ) );
#41533 = EDGE_LOOP ( 'NONE', ( #39412, #28166, #34339, #36949 ) ) ;
#41534 = CARTESIAN_POINT ( 'NONE',  ( 2.607480562269071989, 112.5929263765338249, 8.025000000000002132 ) ) ;
#41535 = CARTESIAN_POINT ( 'NONE',  ( -44.99999999999998579, 119.9999999999999716, 10.00000000000000000 ) ) ;
#41536 = CIRCLE ( 'NONE', #39277, 0.5000000000000004441 ) ;
#41537 = FILL_AREA_STYLE ('',( #36973 ) ) ;
#41538 = DIRECTION ( 'NONE',  ( -1.000000000000000000, 0.000000000000000000, -1.073081856240828689E-16 ) ) ;
#41539 = ORIENTED_EDGE ( 'NONE', *, *, #2953, .T. ) ;
#41540 = PRESENTATION_LAYER_ASSIGNMENT (  '', '', ( #10088 ) ) ;
#41541 = CARTESIAN_POINT ( 'NONE',  ( -93.44292637653380496, -1.166476076187852838E-15, -9.524999999999991473 ) ) ;
#41542 = EDGE_LOOP ( 'NONE', ( #18206, #48638 ) ) ;
#41543 = CARTESIAN_POINT ( 'NONE',  ( -62.24292637653379501, 5.598654528085804216, 7.705886871421366635 ) ) ;
#41544 = AXIS2_PLACEMENT_3D ( 'NONE', #68790, #19876, #42100 ) ;
#41545 = FACE_OUTER_BOUND ( 'NONE', #30105, .T. ) ;
#41546 = DIRECTION ( 'NONE',  ( -1.000000000000000000, 0.000000000000000000, 0.000000000000000000 ) ) ;
#41547 = CARTESIAN_POINT ( 'NONE',  ( -154.5550000000000068, 0.000000000000000000, 8.024999999999991473 ) ) ;
#41548 = ORIENTED_EDGE ( 'NONE', *, *, #43660, .T. ) ;
#41549 = AXIS2_PLACEMENT_3D ( 'NONE', #38512, #22274, #59905 ) ;
#41550 = DIRECTION ( 'NONE',  ( 0.000000000000000000, 0.000000000000000000, 1.000000000000000000 ) ) ;
#41551 = COLOUR_RGB ( '', 0.08235294, 0.09019608, 0.10196078) ;
#41552 = AXIS2_PLACEMENT_3D ( 'NONE', #6102, #18401, #54959 ) ;
#41553 = CARTESIAN_POINT ( 'NONE',  ( -4.682380833558966948, -5.889878495889163013, 0.4967607073414698760 ) ) ;
#41554 =( GEOMETRIC_REPRESENTATION_CONTEXT ( 3 ) GLOBAL_UNCERTAINTY_ASSIGNED_CONTEXT ( ( #9529 ) ) GLOBAL_UNIT_ASSIGNED_CONTEXT ( ( #15602, #31740, #9967 ) ) REPRESENTATION_CONTEXT ( 'NONE', 'WORKASPACE' ) );
#41555 = CARTESIAN_POINT ( 'NONE',  ( 0.000000000000000000, -4.000000000000000000, 18.00000000000000000 ) ) ;
#41556 = CARTESIAN_POINT ( 'NONE',  ( 74.54138597727602189, 19.45803563998439856, 6.486986334521347430 ) ) ;
#41557 = DIRECTION ( 'NONE',  ( -0.000000000000000000, -0.000000000000000000, -1.000000000000000000 ) ) ;
#41558 = ORIENTED_EDGE ( 'NONE', *, *, #10336, .T. ) ;
#41559 = STYLED_ITEM ( 'NONE', ( #6952 ), #51663 ) ;
#41560 = EDGE_LOOP ( 'NONE', ( #49660, #34138, #25717 ) ) ;
#41561 = DIRECTION ( 'NONE',  ( -1.000000000000000000, -0.000000000000000000, -0.000000000000000000 ) ) ;
#41562 = FACE_OUTER_BOUND ( 'NONE', #5575, .T. ) ;
#41563 = CARTESIAN_POINT ( 'NONE',  ( -61.70499999999997698, 2.607480562269073321, 8.024999999999991473 ) ) ;
#41564 = ORIENTED_EDGE ( 'NONE', *, *, #3460, .F. ) ;
#41565 = EDGE_CURVE ( 'NONE', #67546, #20470, #15670, .T. ) ;
#41566 = AXIS2_PLACEMENT_3D ( 'NONE', #22605, #65505, #33494 ) ;
#41567 = CARTESIAN_POINT ( 'NONE',  ( 3.999798566743339556, 8.867945265733707672, -12.50000000000000000 ) ) ;
#41568 = DIRECTION ( 'NONE',  ( 0.000000000000000000, 1.000000000000000000, 0.000000000000000000 ) ) ;
#41569 = AXIS2_PLACEMENT_3D ( 'NONE', #16331, #66918, #44798 ) ;
#41571 = EDGE_CURVE ( 'NONE', #54956, #3572, #37860, .T. ) ;
#41570 = ORIENTED_EDGE ( 'NONE', *, *, #6662, .F. ) ;
#41572 = CARTESIAN_POINT ( 'NONE',  ( -74.99999999999998579, 8.189963308881907267, -5.659193869481054406 ) ) ;
#41573 = SURFACE_STYLE_USAGE ( .BOTH. , #35936 ) ;
#41574 = MECHANICAL_DESIGN_GEOMETRIC_PRESENTATION_REPRESENTATION (  '', ( #7839 ), #29164 ) ;
#41575 = CARTESIAN_POINT ( 'NONE',  ( 45.00000000000000000, 10.69371294336139222, 4.000000000000000000 ) ) ;
#41576 = CARTESIAN_POINT ( 'NONE',  ( -5.598654528085806881, 151.7450000000000045, -7.705886871421374629 ) ) ;
#41577 = CARTESIAN_POINT ( 'NONE',  ( -99.14499999999998181, -4.716976649647092401, 6.492361379858946790 ) ) ;
#41578 = ADVANCED_FACE ( 'NONE', ( #32877 ), #58395, .F. ) ;
#41579 =( NAMED_UNIT ( * ) SI_UNIT ( $, .STERADIAN. ) SOLID_ANGLE_UNIT ( ) );
#41580 = CARTESIAN_POINT ( 'NONE',  ( -7.731910350068054619E-16, -6.500000000000000888, 21.00000000000000000 ) ) ;
#41581 = STYLED_ITEM ( 'NONE', ( #64719 ), #59192 ) ;
#41582 = DIRECTION ( 'NONE',  ( 1.000000000000000000, 0.000000000000000000, 0.000000000000000000 ) ) ;
#41584 = ORIENTED_EDGE ( 'NONE', *, *, #63999, .F. ) ;
#41583 = AXIS2_PLACEMENT_3D ( 'NONE', #1786, #44463, #33498 ) ;
#41585 = EDGE_CURVE ( 'NONE', #8511, #68594, #21984, .T. ) ;
#41586 = CARTESIAN_POINT ( 'NONE',  ( -137.0929263765338249, 3.094860106618433360, 9.524999999999991473 ) ) ;
#41587 = DIRECTION ( 'NONE',  ( -1.000000000000000000, -0.000000000000000000, -0.000000000000000000 ) ) ;
#41588 = CARTESIAN_POINT ( 'NONE',  ( -159.1449999999999818, -4.716976649647092401, 6.492361379858946790 ) ) ;
#41589 = FILL_AREA_STYLE ('',( #68656 ) ) ;
#41590 =( LENGTH_UNIT ( ) NAMED_UNIT ( * ) SI_UNIT ( .MILLI., .METRE. ) );
#41591 = MECHANICAL_DESIGN_GEOMETRIC_PRESENTATION_REPRESENTATION (  '', ( #10088 ), #46068 ) ;
#41592 = DIRECTION ( 'NONE',  ( 1.445602896647337931E-16, -1.000000000000000000, 0.000000000000000000 ) ) ;
#41593 = MECHANICAL_DESIGN_GEOMETRIC_PRESENTATION_REPRESENTATION (  '', ( #5591 ), #60626 ) ;
#41594 = SURFACE_STYLE_USAGE ( .BOTH. , #20818 ) ;
#41595 = VERTEX_POINT ( 'NONE', #26197 ) ;
#41596 = FILL_AREA_STYLE ('',( #5547 ) ) ;
#41597 = ORIENTED_EDGE ( 'NONE', *, *, #39753, .T. ) ;
#41598 = AXIS2_PLACEMENT_3D ( 'NONE', #3545, #25049, #14861 ) ;
#41599 = FACE_OUTER_BOUND ( 'NONE', #53225, .T. ) ;
#41600 =( GEOMETRIC_REPRESENTATION_CONTEXT ( 3 ) GLOBAL_UNCERTAINTY_ASSIGNED_CONTEXT ( ( #15935 ) ) GLOBAL_UNIT_ASSIGNED_CONTEXT ( ( #41590, #61601, #29622 ) ) REPRESENTATION_CONTEXT ( 'NONE', 'WORKASPACE' ) );
#41601 = LINE ( 'NONE', #15560, #22604 ) ;
#41602 = DIRECTION ( 'NONE',  ( -1.000000000000000000, -0.000000000000000000, -0.000000000000000000 ) ) ;
#41603 = CARTESIAN_POINT ( 'NONE',  ( 44.37560827694797183, 9.999999999999980460, 3.428805698905382560 ) ) ;
#41604 = AXIS2_PLACEMENT_3D ( 'NONE', #51512, #34991, #3273 ) ;
#41605 = ORIENTED_EDGE ( 'NONE', *, *, #9733, .T. ) ;
#41606 = CARTESIAN_POINT ( 'NONE',  ( -154.1049999999999898, -6.826472737025113702, 4.959722759717902107 ) ) ;
#41607 = ORIENTED_EDGE ( 'NONE', *, *, #41680, .F. ) ;
#41608 = CARTESIAN_POINT ( 'NONE',  ( -20.56323889998346388, 115.3189275942976337, -10.00000000000000000 ) ) ;
#41609 = CARTESIAN_POINT ( 'NONE',  ( 7.511572993685799101E-16, 2.500000000000000000, -6.999999999999997335 ) ) ;
#41610 = ORIENTED_EDGE ( 'NONE', *, *, #42237, .T. ) ;
#41611 = AXIS2_PLACEMENT_3D ( 'NONE', #64656, #38658, #60731 ) ;
#41612 = CARTESIAN_POINT ( 'NONE',  ( 35.99999999999999289, 5.000000000000000000, 24.00402776293825369 ) ) ;
#41613 = CARTESIAN_POINT ( 'NONE',  ( 108.3664351561509562, 0.000000000000000000, -18.43563588791579733 ) ) ;
#41614 = CARTESIAN_POINT ( 'NONE',  ( 8.102448949553181734, 120.3949999999999960, 5.886773742842750679 ) ) ;
#41615 = AXIS2_PLACEMENT_3D ( 'NONE', #38047, #11271, #20806 ) ;
#41616 = EDGE_CURVE ( 'NONE', #417, #60539, #22314, .T. ) ;
#41617 = MECHANICAL_DESIGN_GEOMETRIC_PRESENTATION_REPRESENTATION (  '', ( #15746 ), #31481 ) ;
#41618 = ORIENTED_EDGE ( 'NONE', *, *, #47378, .F. ) ;
#41619 = FACE_OUTER_BOUND ( 'NONE', #37039, .T. ) ;
#41620 = CARTESIAN_POINT ( 'NONE',  ( 0.000000000000000000, 119.5549999999999926, -9.525000000000000355 ) ) ;
#41621 = CARTESIAN_POINT ( 'NONE',  ( -75.95499999999998408, -7.632228543268599452, 2.479861379858951054 ) ) ;
#41622 = CARTESIAN_POINT ( 'NONE',  ( -44.50000000000000000, 9.999999999999980460, 3.000000000000000000 ) ) ;
#41623 = ORIENTED_EDGE ( 'NONE', *, *, #3213, .T. ) ;
#41624 = CARTESIAN_POINT ( 'NONE',  ( -8.102448949553181734, 141.6050000000000182, 5.886773742842747126 ) ) ;
#41625 = AXIS2_PLACEMENT_3D ( 'NONE', #51587, #13953, #18859 ) ;
#41626 = PLANE ( 'NONE',  #64444 ) ;
#41627 = CARTESIAN_POINT ( 'NONE',  ( -195.0000000000000000, 0.000000000000000000, 0.000000000000000000 ) ) ;
#41628 = CARTESIAN_POINT ( 'NONE',  ( 20.57648123434812959, 114.5706806360227290, 10.27659574044459667 ) ) ;
#41629 = SURFACE_SIDE_STYLE ('',( #29996 ) ) ;
#41630 = SURFACE_STYLE_USAGE ( .BOTH. , #51824 ) ;
#41631 = ORIENTED_EDGE ( 'NONE', *, *, #39032, .T. ) ;
#41632 = LINE ( 'NONE', #36723, #45744 ) ;
#41633 = CARTESIAN_POINT ( 'NONE',  ( -13.25000000000000355, 27.74999999999998934, -4.000000000000000000 ) ) ;
#41634 = CARTESIAN_POINT ( 'NONE',  ( 39.74999999999999289, 18.74999999999997868, -4.000000000000000000 ) ) ;
#41636 = CARTESIAN_POINT ( 'NONE',  ( -184.2549999999999955, -4.716976649647092401, 6.492361379858946790 ) ) ;
#41635 = AXIS2_PLACEMENT_3D ( 'NONE', #21353, #48489, #43229 ) ;
#41637 = ORIENTED_EDGE ( 'NONE', *, *, #11050, .F. ) ;
#41638 = CARTESIAN_POINT ( 'NONE',  ( 6.257356667978436704, 111.7229373514514634, -5.482883996731869658 ) ) ;
#41639 =( LENGTH_UNIT ( ) NAMED_UNIT ( * ) SI_UNIT ( .MILLI., .METRE. ) );
#41640 = ORIENTED_EDGE ( 'NONE', *, *, #63836, .T. ) ;
#41641 = FILL_AREA_STYLE ('',( #30688 ) ) ;
#41642 = DIRECTION ( 'NONE',  ( 1.000000000000000000, 0.000000000000000000, 0.000000000000000000 ) ) ;
#41643 = ORIENTED_EDGE ( 'NONE', *, *, #25959, .T. ) ;
#41644 = LINE ( 'NONE', #58835, #60841 ) ;
#41645 = EDGE_CURVE ( 'NONE', #32302, #13670, #17068, .T. ) ;
#41646 = PRESENTATION_STYLE_ASSIGNMENT (( #25090 ) ) ;
#41647 = CARTESIAN_POINT ( 'NONE',  ( -90.80499999999996419, -8.437984349512085203, 5.166775262442717831E-16 ) ) ;
#41648 = ORIENTED_EDGE ( 'NONE', *, *, #59648, .T. ) ;
#41649 = EDGE_CURVE ( 'NONE', #66803, #61112, #20174, .T. ) ;
#41650 = DIRECTION ( 'NONE',  ( 1.000000000000000000, 0.000000000000000000, -0.000000000000000000 ) ) ;
#41651 = COLOUR_RGB ( '', 0.40784314, 0.44705882, 0.49803922) ;
#41652 = FACE_OUTER_BOUND ( 'NONE', #39375, .T. ) ;
#41653 = PRESENTATION_LAYER_ASSIGNMENT (  '', '', ( #47238 ) ) ;
#41654 = CARTESIAN_POINT ( 'NONE',  ( -131.6070736234661922, -8.102448949553172852, 5.886773742842742685 ) ) ;
#41655 = MECHANICAL_DESIGN_GEOMETRIC_PRESENTATION_REPRESENTATION (  '', ( #1119 ), #29249 ) ;
#41656 =( NAMED_UNIT ( * ) PLANE_ANGLE_UNIT ( ) SI_UNIT ( $, .RADIAN. ) );
#41657 = CARTESIAN_POINT ( 'NONE',  ( -3.094860106618432471, 151.5949999999999704, -9.525000000000000355 ) ) ;
#41658 = CARTESIAN_POINT ( 'NONE',  ( -71.30707362346616662, -10.01517768586948698, 6.132527647946031529E-16 ) ) ;
#41659 = ADVANCED_FACE ( 'NONE', ( #58220 ), #21131, .T. ) ;
#41660 = STYLED_ITEM ( 'NONE', ( #58961 ), #33429 ) ;
#41661 = CARTESIAN_POINT ( 'NONE',  ( 0.000000000000000000, 140.9429263765338192, -8.025000000000000355 ) ) ;
#41662 = ORIENTED_EDGE ( 'NONE', *, *, #49659, .T. ) ;
#41663 = CARTESIAN_POINT ( 'NONE',  ( 57.00000000000000000, 16.00000000000000000, -60.00402776293825724 ) ) ;
#41664 = STYLED_ITEM ( 'NONE', ( #31424 ), #52385 ) ;
#41665 = CARTESIAN_POINT ( 'NONE',  ( 24.21231517720798010, 112.4999999999999858, -9.500000000000000000 ) ) ;
#41666 = CARTESIAN_POINT ( 'NONE',  ( -115.8549999999999898, 4.716976649647094177, 6.492361379858945902 ) ) ;
#41667 = DIRECTION ( 'NONE',  ( 0.000000000000000000, 0.000000000000000000, 1.000000000000000000 ) ) ;
#41668 = CARTESIAN_POINT ( 'NONE',  ( 9.058813317711337021, 117.5449999999999875, 2.943386871421375783 ) ) ;
#41669 = CARTESIAN_POINT ( 'NONE',  ( -125.8449999999999847, -7.632228543268599452, 2.479861379858951054 ) ) ;
#41670 = AXIS2_PLACEMENT_3D ( 'NONE', #37681, #39385, #24532 ) ;
#41671 = EDGE_CURVE ( 'NONE', #47273, #35967, #13437, .T. ) ;
#41672 = CIRCLE ( 'NONE', #42796, 5.000000000000004441 ) ;
#41673 = FILL_AREA_STYLE ('',( #15293 ) ) ;
#41674 =( GEOMETRIC_REPRESENTATION_CONTEXT ( 3 ) GLOBAL_UNCERTAINTY_ASSIGNED_CONTEXT ( ( #48188 ) ) GLOBAL_UNIT_ASSIGNED_CONTEXT ( ( #52735, #26316, #31952 ) ) REPRESENTATION_CONTEXT ( 'NONE', 'WORKASPACE' ) );
#41675 =( NAMED_UNIT ( * ) PLANE_ANGLE_UNIT ( ) SI_UNIT ( $, .RADIAN. ) );
#41676 = PRODUCT_DEFINITION_FORMATION_WITH_SPECIFIED_SOURCE ( 'ANY', '', #4050, .NOT_KNOWN. ) ;
#41677 = CARTESIAN_POINT ( 'NONE',  ( 13.25000000000000355, 27.74999999999998934, 3.750000000000000000 ) ) ;
#41678 = ORIENTED_EDGE ( 'NONE', *, *, #55579, .T. ) ;
#41679 = CARTESIAN_POINT ( 'NONE',  ( -167.6070736234661638, -8.102448949553174629, 5.886773742842742685 ) ) ;
#41680 = EDGE_CURVE ( 'NONE', #56481, #39384, #8944, .T. ) ;
#41681 = CARTESIAN_POINT ( 'NONE',  ( -175.7929263765337851, -3.094860106618429807, 9.524999999999991473 ) ) ;
#41682 = FILL_AREA_STYLE_COLOUR ( '', #43939 ) ;
#41683 = AXIS2_PLACEMENT_3D ( 'NONE', #58950, #20969, #32210 ) ;
#41684 = CARTESIAN_POINT ( 'NONE',  ( 8.021777294149474713, -4.105874159530734424, 3.896351557369779711E-17 ) ) ;
#41685 = CARTESIAN_POINT ( 'NONE',  ( -9.827790563157511022E-16, 125.5570736234661524, 8.025000000000000355 ) ) ;
#41686 = CARTESIAN_POINT ( 'NONE',  ( 0.000000000000000000, 0.000000000000000000, 0.000000000000000000 ) ) ;
#41687 = ORIENTED_EDGE ( 'NONE', *, *, #27603, .F. ) ;
#41688 = CARTESIAN_POINT ( 'NONE',  ( -90.14292637653380780, 5.598654528085800663, -7.705886871421367523 ) ) ;
#41689 = FACE_OUTER_BOUND ( 'NONE', #60969, .T. ) ;
#41690 = PRESENTATION_STYLE_ASSIGNMENT (( #4329 ) ) ;
#41691 = CARTESIAN_POINT ( 'NONE',  ( 7.632228543268608334, 152.3429263765338249, -2.479861379858951942 ) ) ;
#41692 = FILL_AREA_STYLE ('',( #46646 ) ) ;
#41693 = DIRECTION ( 'NONE',  ( 1.000000000000000000, 0.000000000000000000, 0.000000000000000000 ) ) ;
#41694 = VERTEX_POINT ( 'NONE', #1492 ) ;
#41695 = CARTESIAN_POINT ( 'NONE',  ( -4.750000000000002665, 24.74999999999998579, -4.000000000000000000 ) ) ;
#41696 = CARTESIAN_POINT ( 'NONE',  ( 25.75000000000001066, 0.000000000000000000, 4.000000000000000000 ) ) ;
#41697 = CIRCLE ( 'NONE', #9084, 1.000000000000001110 ) ;
#41698 = ORIENTED_EDGE ( 'NONE', *, *, #65521, .F. ) ;
#41699 = CARTESIAN_POINT ( 'NONE',  ( -103.1929263765338050, -10.01517768586948698, 6.132527647946031529E-16 ) ) ;
#41700 = CARTESIAN_POINT ( 'NONE',  ( -72.50000000000000000, 14.49137674618942562, 10.00000000000000000 ) ) ;
#41701 = CARTESIAN_POINT ( 'NONE',  ( 8.437984349512095861, 135.3070736234661240, 1.550032578732817026E-15 ) ) ;
#41702 = EDGE_CURVE ( 'NONE', #46073, #13670, #23020, .T. ) ;
#41703 = CIRCLE ( 'NONE', #15836, 11.99999999999999467 ) ;
#41704 = ORIENTED_EDGE ( 'NONE', *, *, #29628, .T. ) ;
#41705 = LINE ( 'NONE', #32154, #56318 ) ;
#41706 = CARTESIAN_POINT ( 'NONE',  ( -99.65499999999998693, -7.632228543268600340, -2.479861379858950166 ) ) ;
#41707 = FACE_OUTER_BOUND ( 'NONE', #10569, .T. ) ;
#41708 = ORIENTED_EDGE ( 'NONE', *, *, #49261, .T. ) ;
#41709 = PRESENTATION_STYLE_ASSIGNMENT (( #68413 ) ) ;
#41710 = CARTESIAN_POINT ( 'NONE',  ( 2.607480562269198554, 142.5929263765338533, 8.024999999999911537 ) ) ;
#41711 = SURFACE_SIDE_STYLE ('',( #4728 ) ) ;
#41712 = AXIS2_PLACEMENT_3D ( 'NONE', #530, #1223, #64950 ) ;
#41713 = ORIENTED_EDGE ( 'NONE', *, *, #41915, .F. ) ;
#41714 = CARTESIAN_POINT ( 'NONE',  ( -11.54296011127659050, 55.11956624581093678, 6.687176662279907369 ) ) ;
#41715 = CARTESIAN_POINT ( 'NONE',  ( -67.49499999999999034, 6.826472737025113702, -4.959722759717902107 ) ) ;
#41716 = ORIENTED_EDGE ( 'NONE', *, *, #52659, .T. ) ;
#41717 = AXIS2_PLACEMENT_3D ( 'NONE', #65262, #38928, #59632 ) ;
#41718 =( NAMED_UNIT ( * ) SI_UNIT ( $, .STERADIAN. ) SOLID_ANGLE_UNIT ( ) );
#41719 = DIRECTION ( 'NONE',  ( 0.000000000000000000, 0.000000000000000000, -1.000000000000000000 ) ) ;
#41720 = ADVANCED_FACE ( 'NONE', ( #44516 ), #65919, .F. ) ;
#41721 = DIRECTION ( 'NONE',  ( -0.000000000000000000, -0.000000000000000000, -1.000000000000000000 ) ) ;
#41722 = DIRECTION ( 'NONE',  ( -0.000000000000000000, -0.000000000000000000, 1.000000000000000000 ) ) ;
#41723 = UNCERTAINTY_MEASURE_WITH_UNIT (LENGTH_MEASURE( 1.000000000000000082E-05 ), #18517, 'distance_accuracy_value', 'NONE');
#41724 = VERTEX_POINT ( 'NONE', #68023 ) ;
#41725 = CARTESIAN_POINT ( 'NONE',  ( 17.15973193263811680, -3.000000000000000000, -12.50000000000000000 ) ) ;
#41726 = CARTESIAN_POINT ( 'NONE',  ( 22.00000000000000355, 60.69879356856722552, -69.02971849933236115 ) ) ;
#41727 = EDGE_CURVE ( 'NONE', #52777, #66680, #30251, .T. ) ;
#41728 = CARTESIAN_POINT ( 'NONE',  ( 0.000000000000000000, 149.9999999999999716, 0.000000000000000000 ) ) ;
#41729 = CARTESIAN_POINT ( 'NONE',  ( -195.0000000000000000, 0.000000000000000000, 9.524999999999991473 ) ) ;
#41730 = ORIENTED_EDGE ( 'NONE', *, *, #61435, .T. ) ;
#41731 = ADVANCED_FACE ( 'NONE', ( #35654 ), #45876, .T. ) ;
#41732 = CARTESIAN_POINT ( 'NONE',  ( 0.000000000000000000, 2.500000000000000000, 0.000000000000000000 ) ) ;
#41733 = ORIENTED_EDGE ( 'NONE', *, *, #3056, .F. ) ;
#41734 =( LENGTH_UNIT ( ) NAMED_UNIT ( * ) SI_UNIT ( .MILLI., .METRE. ) );
#41735 = CARTESIAN_POINT ( 'NONE',  ( -149.6929263765338192, 10.01517768586948698, -1.839758294383808966E-15 ) ) ;
#41736 = DIRECTION ( 'NONE',  ( -1.000000000000000000, 0.000000000000000000, 0.000000000000000000 ) ) ;
#41737 = CARTESIAN_POINT ( 'NONE',  ( -173.3070736234661808, -10.01517768586948698, 6.132527647946031529E-16 ) ) ;
#41738 = VECTOR ( 'NONE', #26416, 1000.000000000000000 ) ;
#41739 = CARTESIAN_POINT ( 'NONE',  ( -3.094860106618432471, 127.5949999999999847, -9.525000000000000355 ) ) ;
#41740 = CARTESIAN_POINT ( 'NONE',  ( -106.2570736234661695, 5.598654528085800663, -7.705886871421367523 ) ) ;
#41741 = AXIS2_PLACEMENT_3D ( 'NONE', #24276, #45773, #18670 ) ;
#41742 = CARTESIAN_POINT ( 'NONE',  ( 7.632228543268608334, 113.3429263765338106, -2.479861379858951942 ) ) ;
#41743 = EDGE_CURVE ( 'NONE', #61387, #29181, #10097, .T. ) ;
#41744 = STYLED_ITEM ( 'NONE', ( #48778 ), #12804 ) ;
#41745 = PLANE ( 'NONE',  #50455 ) ;
#41746 = ORIENTED_EDGE ( 'NONE', *, *, #42648, .F. ) ;
#41747 = DIRECTION ( 'NONE',  ( 0.000000000000000000, 1.000000000000000000, 0.000000000000000000 ) ) ;
#41748 = ADVANCED_FACE ( 'NONE', ( #24718 ), #14908, .T. ) ;
#41751 = AXIS2_PLACEMENT_3D ( 'NONE', #60156, #57296, #19666 ) ;
#41750 = CARTESIAN_POINT ( 'NONE',  ( -115.4070736234669994, 3.094860106604512495, -9.525000000010106049 ) ) ;
#41749 = CYLINDRICAL_SURFACE ( 'NONE', #68304, 9.524999999999991473 ) ;
#41752 = LINE ( 'NONE', #41394, #3997 ) ;
#41753 = CARTESIAN_POINT ( 'NONE',  ( -151.4049999999999443, -2.607480562269069768, 8.024999999999991473 ) ) ;
#41754 = CARTESIAN_POINT ( 'NONE',  ( -3.000000000000000000, -2.499999999999999556, 24.00000000000000000 ) ) ;
#41755 = VECTOR ( 'NONE', #54194, 1000.000000000000000 ) ;
#41756 = CARTESIAN_POINT ( 'NONE',  ( -154.3449999999999704, 7.632228543268599452, -2.479861379858951942 ) ) ;
#41757 = CARTESIAN_POINT ( 'NONE',  ( -144.7449999999999761, 4.716976649647094177, 6.492361379858945902 ) ) ;
#41758 = CIRCLE ( 'NONE', #67524, 0.5000000000000004441 ) ;
#41759 = ORIENTED_EDGE ( 'NONE', *, *, #30734, .T. ) ;
#41760 = AXIS2_PLACEMENT_3D ( 'NONE', #62422, #19145, #8621 ) ;
#41761 = CYLINDRICAL_SURFACE ( 'NONE', #21257, 5.000000000000004441 ) ;
#41762 = CARTESIAN_POINT ( 'NONE',  ( 10.00000000000002132, 50.00000000000000000, 60.00000000000000000 ) ) ;
#41763 = UNCERTAINTY_MEASURE_WITH_UNIT (LENGTH_MEASURE( 1.000000000000000082E-05 ), #18974, 'distance_accuracy_value', 'NONE');
#41764 = CARTESIAN_POINT ( 'NONE',  ( -68.45499999999998408, 7.632228543268599452, -2.479861379858951942 ) ) ;
#41765 = DIRECTION ( 'NONE',  ( -1.000000000000000000, 0.000000000000000000, 0.000000000000000000 ) ) ;
#41766 = CARTESIAN_POINT ( 'NONE',  ( -62.09499999999998465, -2.607480562269071545, -8.024999999999991473 ) ) ;
#41767 = CARTESIAN_POINT ( 'NONE',  ( 9.058813317711337021, 157.6550000000000011, 2.943386871421375783 ) ) ;
#41768 = FILL_AREA_STYLE_COLOUR ( '', #63863 ) ;
#41769 = DIRECTION ( 'NONE',  ( -1.000000000000000000, 0.000000000000000000, 0.000000000000000000 ) ) ;
#41770 = CIRCLE ( 'NONE', #1242, 3.000000000000000444 ) ;
#41771 = CARTESIAN_POINT ( 'NONE',  ( 8.000000000000030198, 5.000000000000000000, -32.00402776293825013 ) ) ;
#41772 = EDGE_CURVE ( 'NONE', #41202, #13131, #19051, .T. ) ;
#41773 = UNCERTAINTY_MEASURE_WITH_UNIT (LENGTH_MEASURE( 1.000000000000000082E-05 ), #63525, 'distance_accuracy_value', 'NONE');
#41774 =( NAMED_UNIT ( * ) PLANE_ANGLE_UNIT ( ) SI_UNIT ( $, .RADIAN. ) );
#41775 = CARTESIAN_POINT ( 'NONE',  ( -152.3929263765338078, 8.102448949553176405, 5.886773742842740909 ) ) ;
#41776 = CARTESIAN_POINT ( 'NONE',  ( 16.00000000000001776, 42.00000000000000000, -29.68999999999999417 ) ) ;
#41777 = CARTESIAN_POINT ( 'NONE',  ( -41.49999999999997868, 10.49999999999998046, 3.000000000000000000 ) ) ;
#41778 = VECTOR ( 'NONE', #60891, 1000.000000000000000 ) ;
#41779 = FILL_AREA_STYLE_COLOUR ( '', #19202 ) ;
#41780 = B_SPLINE_CURVE_WITH_KNOTS ( 'NONE', 3,
 ( #21254, #47740, #69137, #20943, #10732, #53633 ),
 .UNSPECIFIED., .F., .F.,
 ( 4, 2, 4 ),
 ( 0.005386537104126974673, 0.008060814333094815098, 0.01073509156206265379 ),
 .UNSPECIFIED. ) ;
#41781 = CARTESIAN_POINT ( 'NONE',  ( -74.75000000000000000, 4.336808689942017736E-16, 7.000000000000001776 ) ) ;
#41782 = DIRECTION ( 'NONE',  ( -0.000000000000000000, 0.000000000000000000, -1.000000000000000000 ) ) ;
#41783 = DIRECTION ( 'NONE',  ( -1.000000000000000000, 0.000000000000000000, 0.000000000000000000 ) ) ;
#41784 = ORIENTED_EDGE ( 'NONE', *, *, #39178, .T. ) ;
#41785 = ORIENTED_EDGE ( 'NONE', *, *, #6372, .F. ) ;
#41786 = STYLED_ITEM ( 'NONE', ( #51350 ), #60433 ) ;
#41787 = SPHERICAL_SURFACE ( 'NONE', #59636, 1.000000000000000000 ) ;
#41788 = STYLED_ITEM ( 'NONE', ( #19077 ), #45997 ) ;
#41789 = STYLED_ITEM ( 'NONE', ( #16418 ), #12899 ) ;
#41790 = CARTESIAN_POINT ( 'NONE',  ( -20.07572180596747913, 115.0406156812134952, 10.00000000000000000 ) ) ;
#41791 = DIRECTION ( 'NONE',  ( -0.000000000000000000, 0.000000000000000000, -1.000000000000000000 ) ) ;
#41792 = SURFACE_STYLE_FILL_AREA ( #25222 ) ;
#41793 = ORIENTED_EDGE ( 'NONE', *, *, #62267, .F. ) ;
#41794 = ORIENTED_EDGE ( 'NONE', *, *, #43256, .F. ) ;
#41795 = CARTESIAN_POINT ( 'NONE',  ( -12.74999999999999822, -3.000000000000000000, 7.000000000000001776 ) ) ;
#41796 = CYLINDRICAL_SURFACE ( 'NONE', #33117, 9.524999999999991473 ) ;
#41797 = DIRECTION ( 'NONE',  ( 0.3403530053317448401, -0.9351121967924955758, 0.09861547125863370789 ) ) ;
#41798 = EDGE_LOOP ( 'NONE', ( #61397, #28610, #27314, #63328 ) ) ;
#41799 = CARTESIAN_POINT ( 'NONE',  ( -5.598654528085808657, 120.7549999999999812, 7.705886871421373741 ) ) ;
#41800 = CARTESIAN_POINT ( 'NONE',  ( -84.89292637653377938, -8.102448949553174629, -5.886773742842741797 ) ) ;
#41801 =( LENGTH_UNIT ( ) NAMED_UNIT ( * ) SI_UNIT ( .MILLI., .METRE. ) );
#41802 = ADVANCED_FACE ( 'NONE', ( #30691 ), #19094, .T. ) ;
#41803 = PRESENTATION_LAYER_ASSIGNMENT (  '', '', ( #64201 ) ) ;
#41804 = CARTESIAN_POINT ( 'NONE',  ( 179.4361977533490347, 0.000000000000000000, -103.7004518695263044 ) ) ;
#41805 = CARTESIAN_POINT ( 'NONE',  ( -96.44499999999999318, 0.000000000000000000, 8.024999999999991473 ) ) ;
#41806 = ORIENTED_EDGE ( 'NONE', *, *, #26897, .T. ) ;
#41807 = COLOUR_RGB ( '', 0.72549020, 0.75294118, 0.79215686) ;
#41808 = SURFACE_SIDE_STYLE ('',( #14698 ) ) ;
#41809 =( LENGTH_UNIT ( ) NAMED_UNIT ( * ) SI_UNIT ( .MILLI., .METRE. ) );
#41810 = EDGE_CURVE ( 'NONE', #60935, #7949, #53868, .T. ) ;
#41811 =( LENGTH_UNIT ( ) NAMED_UNIT ( * ) SI_UNIT ( .MILLI., .METRE. ) );
#41812 = ORIENTED_EDGE ( 'NONE', *, *, #11779, .T. ) ;
#41813 = CARTESIAN_POINT ( 'NONE',  ( 4.716976649647099507, 152.6429263765338078, -6.492361379858953008 ) ) ;
#41814 = DIRECTION ( 'NONE',  ( -1.000000000000000000, 0.000000000000000000, 0.000000000000000000 ) ) ;
#41815 = DIRECTION ( 'NONE',  ( -1.000000000000000000, 0.000000000000000000, 0.000000000000000000 ) ) ;
#41816 = EDGE_CURVE ( 'NONE', #13211, #24116, #21268, .T. ) ;
#41817 = AXIS2_PLACEMENT_3D ( 'NONE', #31563, #21713, #36892 ) ;
#41818 = ORIENTED_EDGE ( 'NONE', *, *, #25841, .F. ) ;
#41819 = AXIS2_PLACEMENT_3D ( 'NONE', #60540, #39488, #49326 ) ;
#41820 = EDGE_LOOP ( 'NONE', ( #63591, #27720, #31547, #66215 ) ) ;
#41821 = CARTESIAN_POINT ( 'NONE',  ( 21.02379604162863913, 114.4999999999999574, 10.00000000000000000 ) ) ;
#41822 = CARTESIAN_POINT ( 'NONE',  ( 70.87837837837835764, 13.70805908423324482, -10.00000000000000000 ) ) ;
#41823 = DIRECTION ( 'NONE',  ( 0.000000000000000000, 0.000000000000000000, 1.000000000000000000 ) ) ;
#41824 = CARTESIAN_POINT ( 'NONE',  ( -119.6049999999999756, 6.826472737025113702, -4.959722759717902107 ) ) ;
#41825 =( BOUNDED_CURVE ( )  B_SPLINE_CURVE ( 3, ( #32366, #30723, #32723, #21481 ),
 .UNSPECIFIED., .F., .F. ) 
 B_SPLINE_CURVE_WITH_KNOTS ( ( 4, 4 ),
 ( 8.673617379884026597E-16, 1.570796326794896558 ),
 .UNSPECIFIED. ) 
 CURVE ( )  GEOMETRIC_REPRESENTATION_ITEM ( )  RATIONAL_B_SPLINE_CURVE ( ( 1.000000000000000000, 0.8047378541243652705, 0.8047378541243652705, 1.000000000000000000 ) ) 
 REPRESENTATION_ITEM ( '' )  );
#41826 = DIRECTION ( 'NONE',  ( 0.000000000000000000, 0.000000000000000000, 1.000000000000000000 ) ) ;
#41827 = DIRECTION ( 'NONE',  ( -0.000000000000000000, -0.000000000000000000, -1.000000000000000000 ) ) ;
#41828 = LINE ( 'NONE', #19965, #1282 ) ;
#41829 = CARTESIAN_POINT ( 'NONE',  ( -7.794228634059953364, 4.500000000000004441, 0.000000000000000000 ) ) ;
#41830 = CARTESIAN_POINT ( 'NONE',  ( 2.999999999999998668, 5.000000000000000000, 72.00402776293822171 ) ) ;
#41831 = ORIENTED_EDGE ( 'NONE', *, *, #8118, .F. ) ;
#41832 = AXIS2_PLACEMENT_3D ( 'NONE', #37146, #31459, #41369 ) ;
#41833 = ORIENTED_EDGE ( 'NONE', *, *, #34159, .T. ) ;
#41834 = CARTESIAN_POINT ( 'NONE',  ( 60.00000000000000000, -2.024042244987997205E-14, 7.000000000000000000 ) ) ;
#41835 = DIRECTION ( 'NONE',  ( -0.000000000000000000, 0.000000000000000000, -1.000000000000000000 ) ) ;
#41836 = ADVANCED_FACE ( 'NONE', ( #53560 ), #53227, .F. ) ;
#41837 = DIRECTION ( 'NONE',  ( -0.000000000000000000, -0.000000000000000000, -1.000000000000000000 ) ) ;
#41838 = ORIENTED_EDGE ( 'NONE', *, *, #67053, .T. ) ;
#41839 = CARTESIAN_POINT ( 'NONE',  ( -180.3549999999999898, -4.716976649647093289, -6.492361379858945902 ) ) ;
#41840 = DIRECTION ( 'NONE',  ( 0.000000000000000000, 0.000000000000000000, 1.000000000000000000 ) ) ;
#41841 = PRESENTATION_STYLE_ASSIGNMENT (( #30178 ) ) ;
#41842 = CARTESIAN_POINT ( 'NONE',  ( -182.0949999999999989, -2.607480562269071545, -8.024999999999991473 ) ) ;
#41843 = AXIS2_PLACEMENT_3D ( 'NONE', #60076, #11538, #54099 ) ;
#41844 = CARTESIAN_POINT ( 'NONE',  ( -174.5949999999999989, 2.607480562269072433, 8.024999999999991473 ) ) ;
#41845 = ORIENTED_EDGE ( 'NONE', *, *, #46834, .F. ) ;
#41846 = DIRECTION ( 'NONE',  ( -1.000000000000000000, 0.000000000000000000, 0.000000000000000000 ) ) ;
#41847 = AXIS2_PLACEMENT_3D ( 'NONE', #55572, #17622, #33087 ) ;
#41848 = CARTESIAN_POINT ( 'NONE',  ( -10.03355964668487843, 11.98590840856550344, -0.6655800929182279502 ) ) ;
#41849 = CARTESIAN_POINT ( 'NONE',  ( -89.60499999999997556, 6.826472737025113702, -4.959722759717902107 ) ) ;
#41850 = COLOUR_RGB ( '', 0.72549020, 0.75294118, 0.79215686) ;
#41851 = CARTESIAN_POINT ( 'NONE',  ( -91.94499999999997897, -9.827790563157499189E-16, -8.024999999999991473 ) ) ;
#41852 = CARTESIAN_POINT ( 'NONE',  ( -8.102448949553181734, 123.0049999999999955, -5.886773742842749790 ) ) ;
#41853 = CARTESIAN_POINT ( 'NONE',  ( -72.74499999999999034, 4.716976649647094177, 6.492361379858945902 ) ) ;
#41854 = VECTOR ( 'NONE', #39276, 1000.000000000000000 ) ;
#41855 = DIRECTION ( 'NONE',  ( -0.000000000000000000, 1.000000000000000000, -0.000000000000000000 ) ) ;
#41856 = CARTESIAN_POINT ( 'NONE',  ( -56.30707362346618794, -10.01517768586948698, 6.132527647946031529E-16 ) ) ;
#41857 = MECHANICAL_DESIGN_GEOMETRIC_PRESENTATION_REPRESENTATION (  '', ( #5840 ), #47496 ) ;
#41858 = ADVANCED_FACE ( 'NONE', ( #5689 ), #43415, .T. ) ;
#41859 = UNCERTAINTY_MEASURE_WITH_UNIT (LENGTH_MEASURE( 1.000000000000000082E-05 ), #13610, 'distance_accuracy_value', 'NONE');
#41860 = DIRECTION ( 'NONE',  ( 0.000000000000000000, -1.000000000000000000, 0.000000000000000000 ) ) ;
#41861 = ORIENTED_EDGE ( 'NONE', *, *, #43064, .T. ) ;
#41862 = CARTESIAN_POINT ( 'NONE',  ( -105.7429263765338021, -5.598654528085803328, -7.705886871421366635 ) ) ;
#41863 = CARTESIAN_POINT ( 'NONE',  ( -130.3449999999999989, 7.632228543268599452, -2.479861379858951942 ) ) ;
#41864 = SURFACE_SIDE_STYLE ('',( #19315 ) ) ;
#41865 = COLOUR_RGB ( '', 0.72549020, 0.75294118, 0.79215686) ;
#41866 = DIRECTION ( 'NONE',  ( 1.000000000000000000, 0.000000000000000000, 0.000000000000000000 ) ) ;
#41868 = DIRECTION ( 'NONE',  ( -0.000000000000000000, 1.000000000000000000, -0.000000000000000000 ) ) ;
#41867 = CARTESIAN_POINT ( 'NONE',  ( 7.632228543268607446, 135.1570736234661467, 2.479861379858954606 ) ) ;
#41869 = PRESENTATION_STYLE_ASSIGNMENT (( #68571 ) ) ;
#41870 = ORIENTED_EDGE ( 'NONE', *, *, #65995, .T. ) ;
#41871 = EDGE_LOOP ( 'NONE', ( #62329, #48855, #36254, #53562 ) ) ;
#41872 = DIRECTION ( 'NONE',  ( 1.000000000000000000, 0.000000000000000000, 0.000000000000000000 ) ) ;
#41873 = CARTESIAN_POINT ( 'NONE',  ( 7.632228543268607446, 131.0429263765338135, 2.479861379858954606 ) ) ;
#41874 = UNCERTAINTY_MEASURE_WITH_UNIT (LENGTH_MEASURE( 1.000000000000000082E-05 ), #22624, 'distance_accuracy_value', 'NONE');
#41875 = SURFACE_STYLE_USAGE ( .BOTH. , #47875 ) ;
#41876 = DIRECTION ( 'NONE',  ( -1.000000000000000000, 0.000000000000000000, 0.000000000000000000 ) ) ;
#41877 =( GEOMETRIC_REPRESENTATION_CONTEXT ( 3 ) GLOBAL_UNCERTAINTY_ASSIGNED_CONTEXT ( ( #21599 ) ) GLOBAL_UNIT_ASSIGNED_CONTEXT ( ( #8570, #49743, #2154 ) ) REPRESENTATION_CONTEXT ( 'NONE', 'WORKASPACE' ) );
#41878 = CARTESIAN_POINT ( 'NONE',  ( -10.39230484541326938, -1.107695154586735509, -1.661048719643172847E-15 ) ) ;
#41879 = VERTEX_POINT ( 'NONE', #10314 ) ;
#41880 = CARTESIAN_POINT ( 'NONE',  ( -121.2549999999999812, -4.716976649647092401, 6.492361379858946790 ) ) ;
#41881 = ORIENTED_EDGE ( 'NONE', *, *, #9488, .T. ) ;
#41882 = CARTESIAN_POINT ( 'NONE',  ( -137.6070736234661922, -8.102448949553174629, 5.886773742842742685 ) ) ;
#41883 = CARTESIAN_POINT ( 'NONE',  ( -126.2070736234661723, 3.094860106618433360, 9.524999999999991473 ) ) ;
#41884 = ORIENTED_EDGE ( 'NONE', *, *, #62341, .T. ) ;
#41885 = CARTESIAN_POINT ( 'NONE',  ( 3.673940397442060361E-16, 2.299999999999999822, 3.000000000000000444 ) ) ;
#41886 = VERTEX_POINT ( 'NONE', #63425 ) ;
#41887 = ADVANCED_FACE ( 'NONE', ( #15956 ), #56008, .T. ) ;
#41888 = COLOUR_RGB ( '', 0.09019608, 0.27058824, 0.51372549) ;
#41889 = AXIS2_PLACEMENT_3D ( 'NONE', #4797, #43188, #825 ) ;
#41890 = CARTESIAN_POINT ( 'NONE',  ( -10.01517768586949231, 146.1949999999999648, -6.132527647946036459E-16 ) ) ;
#41891 = DIRECTION ( 'NONE',  ( 1.000000000000000000, 0.000000000000000000, 0.000000000000000000 ) ) ;
#41892 = ORIENTED_EDGE ( 'NONE', *, *, #12469, .F. ) ;
#41893 = AXIS2_PLACEMENT_3D ( 'NONE', #39723, #35106, #39379 ) ;
#41894 = CARTESIAN_POINT ( 'NONE',  ( 0.000000000000000000, 114.4999999999999574, 0.000000000000000000 ) ) ;
#41895 = CARTESIAN_POINT ( 'NONE',  ( -1.166476076187854022E-15, 145.0549999999999784, 9.525000000000000355 ) ) ;
#41896 = LINE ( 'NONE', #14793, #3512 ) ;
#41897 = FILL_AREA_STYLE ('',( #67913 ) ) ;
#41898 = EDGE_LOOP ( 'NONE', ( #55214, #3108, #16003, #40088 ) ) ;
#41899 = CARTESIAN_POINT ( 'NONE',  ( 6.826472737025121695, 128.4929263765338305, -4.959722759717905660 ) ) ;
#41900 = DIRECTION ( 'NONE',  ( -0.000000000000000000, -0.000000000000000000, -1.000000000000000000 ) ) ;
#41901 = UNCERTAINTY_MEASURE_WITH_UNIT (LENGTH_MEASURE( 1.000000000000000082E-05 ), #38436, 'distance_accuracy_value', 'NONE');
#41902 = CARTESIAN_POINT ( 'NONE',  ( 23.50000000000001776, 42.00000000000000000, -28.18999999999999773 ) ) ;
#41903 = STYLED_ITEM ( 'NONE', ( #49077 ), #23760 ) ;
#41904 = CARTESIAN_POINT ( 'NONE',  ( -98.54292637653381348, 9.058813317711329915, 2.943386871421369566 ) ) ;
#41905 = DIRECTION ( 'NONE',  ( -1.000000000000000000, 0.000000000000000000, 0.000000000000000000 ) ) ;
#41906 = EDGE_CURVE ( 'NONE', #58037, #12723, #11, .T. ) ;
#41907 = DIRECTION ( 'NONE',  ( 1.073081856240828689E-16, 0.000000000000000000, -1.000000000000000000 ) ) ;
#41908 = ORIENTED_EDGE ( 'NONE', *, *, #10976, .T. ) ;
#41909 = CARTESIAN_POINT ( 'NONE',  ( -41.72781494893835230, 107.4000720140338387, -4.000000000000000000 ) ) ;
#41910 = ORIENTED_EDGE ( 'NONE', *, *, #60560, .F. ) ;
#41911 = CARTESIAN_POINT ( 'NONE',  ( -56.09292637653378222, 3.094860106618433360, 9.524999999999991473 ) ) ;
#41912 = CARTESIAN_POINT ( 'NONE',  ( 21.75000000000001066, 21.74999999999998224, -4.000000000000000000 ) ) ;
#41913 = CYLINDRICAL_SURFACE ( 'NONE', #34078, 0.5000000000000004441 ) ;
#41914 = CARTESIAN_POINT ( 'NONE',  ( -152.4550000000000125, 7.632228543268599452, -2.479861379858951942 ) ) ;
#41916 = ORIENTED_EDGE ( 'NONE', *, *, #51785, .T. ) ;
#41915 = EDGE_CURVE ( 'NONE', #9166, #8380, #14443, .T. ) ;
#41917 = SURFACE_SIDE_STYLE ('',( #36291 ) ) ;
#41918 = UNCERTAINTY_MEASURE_WITH_UNIT (LENGTH_MEASURE( 1.000000000000000082E-05 ), #63468, 'distance_accuracy_value', 'NONE');
#41919 = TOROIDAL_SURFACE ( 'NONE', #37461, 1.000000000000000000, 0.5000000000000000000 ) ;
#41920 = EDGE_CURVE ( 'NONE', #19597, #34517, #30129, .T. ) ;
#41921 = CARTESIAN_POINT ( 'NONE',  ( -4.358330484967983587, -6.451150163859152187, 0.7660251680141582087 ) ) ;
#41922 = CARTESIAN_POINT ( 'NONE',  ( -6.826472737025120807, 152.1070736234661354, 4.959722759717906548 ) ) ;
#41923 = CARTESIAN_POINT ( 'NONE',  ( 75.00000000000000000, 19.46449454893559050, 6.525737028834527109 ) ) ;
#41924 = CARTESIAN_POINT ( 'NONE',  ( 4.716976649647099507, 146.6429263765338078, -6.492361379858953008 ) ) ;
#41925 = ORIENTED_EDGE ( 'NONE', *, *, #54574, .T. ) ;
#41926 = ORIENTED_EDGE ( 'NONE', *, *, #66986, .F. ) ;
#41927 = PLANE ( 'NONE',  #63176 ) ;
#41928 = ADVANCED_FACE ( 'NONE', ( #17683 ), #44778, .F. ) ;
#41929 = VECTOR ( 'NONE', #11602, 1000.000000000000000 ) ;
#41930 = CARTESIAN_POINT ( 'NONE',  ( -66.80499999999999261, -8.437984349512085203, 5.166775262442717831E-16 ) ) ;
#41931 = VERTEX_POINT ( 'NONE', #60541 ) ;
#41932 = CARTESIAN_POINT ( 'NONE',  ( 22.25000000000000711, 34.24999999999999289, -3.750000000000000000 ) ) ;
#41933 =( NAMED_UNIT ( * ) SI_UNIT ( $, .STERADIAN. ) SOLID_ANGLE_UNIT ( ) );
#41934 = AXIS2_PLACEMENT_3D ( 'NONE', #31920, #31212, #63592 ) ;
#41935 = B_SPLINE_CURVE_WITH_KNOTS ( 'NONE', 3,
 ( #44765, #66163, #29925, #18689, #13389, #40864, #23952, #45110 ),
 .UNSPECIFIED., .F., .F.,
 ( 4, 2, 2, 4 ),
 ( 0.000000000000000000, 0.0004782788118992547534, 0.0007174182178488821031, 0.0009565576237985095069 ),
 .UNSPECIFIED. ) ;
#41936 = FACE_OUTER_BOUND ( 'NONE', #27891, .T. ) ;
#41937 = FACE_OUTER_BOUND ( 'NONE', #27047, .T. ) ;
#41938 = EDGE_LOOP ( 'NONE', ( #29020, #64803, #43837, #34149 ) ) ;
#41939 =( BOUNDED_CURVE ( )  B_SPLINE_CURVE ( 2, ( #16365, #59571, #54296, #23003, #5747, #17049, #44496, #435, #17399, #17730, #6118 ),
 .UNSPECIFIED., .F., .F. ) 
 B_SPLINE_CURVE_WITH_KNOTS ( ( 3, 2, 2, 2, 2, 3 ),
 ( 0.6521739130434630605, 0.6543478260869413088, 0.6565217391304194461, 0.6586956521738976944, 0.6608695652173758317, 0.6630434782608540800 ),
 .UNSPECIFIED. ) 
 CURVE ( )  GEOMETRIC_REPRESENTATION_ITEM ( )  RATIONAL_B_SPLINE_CURVE ( ( 1.000000000000342393, 0.9510565162948111384, 1.000000000000000000, 0.9510565162951535312, 1.000000000000000000, 0.9510565162951535312, 1.000000000000000000, 0.9510565162951535312, 1.000000000000000000, 0.9510565162955009200, 0.9999999999996526112 ) ) 
 REPRESENTATION_ITEM ( '' )  );
#41940 = VECTOR ( 'NONE', #50714, 1000.000000000000000 ) ;
#41941 = DIRECTION ( 'NONE',  ( 0.000000000000000000, 0.000000000000000000, -1.000000000000000000 ) ) ;
#41942 = DIRECTION ( 'NONE',  ( -0.7071067811865500152, 0.000000000000000000, -0.7071067811865450192 ) ) ;
#41943 = PRESENTATION_LAYER_ASSIGNMENT (  '', '', ( #235 ) ) ;
#41945 = LINE ( 'NONE', #26050, #17935 ) ;
#41944 = CARTESIAN_POINT ( 'NONE',  ( 71.49999999999998579, 119.9999999999997868, -7.500000000000000000 ) ) ;
#41946 = CARTESIAN_POINT ( 'NONE',  ( 5.598654528085805993, 147.2449999999999761, 7.705886871421374629 ) ) ;
#41947 = CARTESIAN_POINT ( 'NONE',  ( -95.09499999999999886, -2.607480562269071545, -8.024999999999991473 ) ) ;
#41948 = PRESENTATION_LAYER_ASSIGNMENT (  '', '', ( #32921 ) ) ;
#41949 = AXIS2_PLACEMENT_3D ( 'NONE', #1185, #27951, #22719 ) ;
#41950 =( NAMED_UNIT ( * ) PLANE_ANGLE_UNIT ( ) SI_UNIT ( $, .RADIAN. ) );
#41951 = UNCERTAINTY_MEASURE_WITH_UNIT (LENGTH_MEASURE( 1.000000000000000082E-05 ), #48360, 'distance_accuracy_value', 'NONE');
#41952 = CARTESIAN_POINT ( 'NONE',  ( -41.30869453359410670, 107.2693964154585871, -3.464738947915713574 ) ) ;
#41953 = CIRCLE ( 'NONE', #26171, 16.50000000000000000 ) ;
#41954 = ORIENTED_EDGE ( 'NONE', *, *, #43948, .T. ) ;
#41955 = CARTESIAN_POINT ( 'NONE',  ( -135.5929263765337964, -3.094860106618431139, -9.524999999999991473 ) ) ;
#41956 = LINE ( 'NONE', #36684, #24253 ) ;
#41957 = CARTESIAN_POINT ( 'NONE',  ( -154.9449999999999932, -9.827790563157499189E-16, -8.024999999999991473 ) ) ;
#41958 = DIRECTION ( 'NONE',  ( 0.000000000000000000, 1.000000000000000000, 0.000000000000000000 ) ) ;
#41959 = VECTOR ( 'NONE', #33372, 1000.000000000000000 ) ;
#41960 = CARTESIAN_POINT ( 'NONE',  ( 34.99999999999992895, 112.9999999999999858, 9.500000000000000000 ) ) ;
#41961 = DIRECTION ( 'NONE',  ( 8.659560562354879857E-17, 0.7071067811865517916, -0.7071067811865431318 ) ) ;
#41962 = ORIENTED_EDGE ( 'NONE', *, *, #61941, .F. ) ;
#41963 = ORIENTED_EDGE ( 'NONE', *, *, #52996, .F. ) ;
#41964 = AXIS2_PLACEMENT_3D ( 'NONE', #52791, #10560, #41546 ) ;
#41965 = DIRECTION ( 'NONE',  ( 1.000000000000000000, 0.000000000000000000, 0.000000000000000000 ) ) ;
#41966 = COLOUR_RGB ( '', 0.08235294, 0.09019608, 0.10196078) ;
#41967 =( GEOMETRIC_REPRESENTATION_CONTEXT ( 3 ) GLOBAL_UNCERTAINTY_ASSIGNED_CONTEXT ( ( #40581 ) ) GLOBAL_UNIT_ASSIGNED_CONTEXT ( ( #20096, #64060, #26424 ) ) REPRESENTATION_CONTEXT ( 'NONE', 'WORKASPACE' ) );
#41968 = DIRECTION ( 'NONE',  ( 0.000000000000000000, 0.000000000000000000, 1.000000000000000000 ) ) ;
#41969 = CARTESIAN_POINT ( 'NONE',  ( -45.91547277936962246, 9.430195807687223208, 6.000000000000001776 ) ) ;
#41970 = CARTESIAN_POINT ( 'NONE',  ( -110.0070736234661979, -8.102448949553174629, -5.886773742842741797 ) ) ;
#41971 = AXIS2_PLACEMENT_3D ( 'NONE', #2428, #12002, #55250 ) ;
#41972 = ORIENTED_EDGE ( 'NONE', *, *, #40760, .F. ) ;
#41973 = CARTESIAN_POINT ( 'NONE',  ( -146.3049999999999784, 8.437984349512086979, -1.550032578732815448E-15 ) ) ;
#41974 = PRESENTATION_LAYER_ASSIGNMENT (  '', '', ( #5965 ) ) ;
#41975 = ORIENTED_EDGE ( 'NONE', *, *, #17022, .T. ) ;
#41976 = LINE ( 'NONE', #36704, #38043 ) ;
#41977 = CARTESIAN_POINT ( 'NONE',  ( 22.50000000000000711, 33.99999999999999289, 3.750000000000000000 ) ) ;
#41978 = ORIENTED_EDGE ( 'NONE', *, *, #36758, .F. ) ;
#41979 = EDGE_CURVE ( 'NONE', #58118, #53591, #28878, .T. ) ;
#41980 = DIRECTION ( 'NONE',  ( -0.000000000000000000, 1.000000000000000000, -0.000000000000000000 ) ) ;
#41981 = LINE ( 'NONE', #19779, #54452 ) ;
#41982 = CARTESIAN_POINT ( 'NONE',  ( -10.01517768586949231, 119.1949999999999932, -6.132527647946036459E-16 ) ) ;
#41983 = PRESENTATION_STYLE_ASSIGNMENT (( #56823 ) ) ;
#41984 = ADVANCED_FACE ( 'NONE', ( #709 ), #55973, .T. ) ;
#41985 =( GEOMETRIC_REPRESENTATION_CONTEXT ( 3 ) GLOBAL_UNCERTAINTY_ASSIGNED_CONTEXT ( ( #46217 ) ) GLOBAL_UNIT_ASSIGNED_CONTEXT ( ( #8837, #62984, #41933 ) ) REPRESENTATION_CONTEXT ( 'NONE', 'WORKASPACE' ) );
#41986 = ORIENTED_EDGE ( 'NONE', *, *, #48672, .F. ) ;
#41987 = EDGE_CURVE ( 'NONE', #45556, #20287, #57871, .T. ) ;
#41988 = SURFACE_STYLE_FILL_AREA ( #20481 ) ;
#41989 = CARTESIAN_POINT ( 'NONE',  ( -8.102448949553179958, 123.6049999999999756, 5.886773742842747126 ) ) ;
#41990 = CARTESIAN_POINT ( 'NONE',  ( -69.05499999999999261, -9.827790563157499189E-16, -8.024999999999991473 ) ) ;
#41991 = CARTESIAN_POINT ( 'NONE',  ( -79.85707362346616378, -5.598654528085803328, -7.705886871421366635 ) ) ;
#41992 = VERTEX_POINT ( 'NONE', #12355 ) ;
#41993 = CARTESIAN_POINT ( 'NONE',  ( -8.102448949553181734, 150.0049999999999386, -5.886773742842749790 ) ) ;
#41994 = UNCERTAINTY_MEASURE_WITH_UNIT (LENGTH_MEASURE( 1.000000000000000082E-05 ), #51106, 'distance_accuracy_value', 'NONE');
#41995 = ADVANCED_FACE ( 'NONE', ( #17346 ), #50363, .T. ) ;
#41996 = CARTESIAN_POINT ( 'NONE',  ( -183.0516217685573679, -0.3847981879420483420, 9.473378231442628916 ) ) ;
#41997 = EDGE_CURVE ( 'NONE', #2313, #36334, #45906, .T. ) ;
#41998 = FILL_AREA_STYLE ('',( #8562 ) ) ;
#41999 = ADVANCED_FACE ( 'NONE', ( #39846 ), #1769, .T. ) ;
#42000 = ORIENTED_EDGE ( 'NONE', *, *, #2240, .T. ) ;
#42001 = MECHANICAL_DESIGN_GEOMETRIC_PRESENTATION_REPRESENTATION (  '', ( #21707 ), #304 ) ;
#42003 = STYLED_ITEM ( 'NONE', ( #62272 ), #646 ) ;
#42002 = AXIS2_PLACEMENT_3D ( 'NONE', #21955, #47334, #11381 ) ;
#42004 = SURFACE_STYLE_FILL_AREA ( #53550 ) ;
#42005 = DIRECTION ( 'NONE',  ( -0.000000000000000000, -0.000000000000000000, 1.000000000000000000 ) ) ;
#42006 = CARTESIAN_POINT ( 'NONE',  ( -177.3549999999999898, -4.716976649647093289, -6.492361379858945902 ) ) ;
#42007 = VERTEX_POINT ( 'NONE', #17999 ) ;
#42008 = CARTESIAN_POINT ( 'NONE',  ( 8.154247983011931211, 111.3129849151904978, 3.079081823141366581 ) ) ;
#42009 =( REPRESENTATION_RELATIONSHIP ('NONE','NONE', #5102, #10054 ) REPRESENTATION_RELATIONSHIP_WITH_TRANSFORMATION ( #20183 )SHAPE_REPRESENTATION_RELATIONSHIP( ) );
#42010 = CIRCLE ( 'NONE', #63292, 8.025000000000000355 ) ;
#42011 = EDGE_CURVE ( 'NONE', #47797, #25427, #22603, .T. ) ;
#42012 = DIRECTION ( 'NONE',  ( 0.000000000000000000, -1.000000000000000000, 0.000000000000000000 ) ) ;
#42013 = ORIENTED_EDGE ( 'NONE', *, *, #64121, .F. ) ;
#42014 = DIRECTION ( 'NONE',  ( 1.000000000000000000, 0.000000000000000000, 0.000000000000000000 ) ) ;
#42015 = DIRECTION ( 'NONE',  ( -1.000000000000000000, 0.000000000000000000, 0.000000000000000000 ) ) ;
#42016 = ORIENTED_EDGE ( 'NONE', *, *, #20591, .F. ) ;
#42017 = DIRECTION ( 'NONE',  ( 1.000000000000000000, 0.000000000000000000, -0.000000000000000000 ) ) ;
#42018 = CARTESIAN_POINT ( 'NONE',  ( -97.55499999999999261, 0.000000000000000000, 8.024999999999991473 ) ) ;
#42020 = ORIENTED_EDGE ( 'NONE', *, *, #14930, .T. ) ;
#42019 =( GEOMETRIC_REPRESENTATION_CONTEXT ( 3 ) GLOBAL_UNCERTAINTY_ASSIGNED_CONTEXT ( ( #13046 ) ) GLOBAL_UNIT_ASSIGNED_CONTEXT ( ( #60929, #11719, #39880 ) ) REPRESENTATION_CONTEXT ( 'NONE', 'WORKASPACE' ) );
#42021 = FILL_AREA_STYLE ('',( #20513 ) ) ;
#42022 = CARTESIAN_POINT ( 'NONE',  ( -134.7570736234661695, -5.598654528085801552, 7.705886871421367523 ) ) ;
#42023 = CIRCLE ( 'NONE', #21728, 0.5000000000000004441 ) ;
#42024 = FACE_OUTER_BOUND ( 'NONE', #38182, .T. ) ;
#42025 = CARTESIAN_POINT ( 'NONE',  ( -5.598654528085806881, 148.7449999999999761, -7.705886871421374629 ) ) ;
#42026 = CARTESIAN_POINT ( 'NONE',  ( -71.60707362346616378, -8.102448949553172852, 5.886773742842742685 ) ) ;
#42027 = AXIS2_PLACEMENT_3D ( 'NONE', #48834, #22056, #38276 ) ;
#42028 = CARTESIAN_POINT ( 'NONE',  ( -93.14292637653380780, 5.598654528085800663, -7.705886871421367523 ) ) ;
#42029 = STYLED_ITEM ( 'NONE', ( #31003 ), #31064 ) ;
#42030 = ORIENTED_EDGE ( 'NONE', *, *, #16780, .T. ) ;
#42031 = DIRECTION ( 'NONE',  ( 0.000000000000000000, 0.000000000000000000, -1.000000000000000000 ) ) ;
#42032 = CARTESIAN_POINT ( 'NONE',  ( -19.83596493880951428, -11.93243626797339907, 1.312027138233742285 ) ) ;
#42033 = SURFACE_SIDE_STYLE ('',( #57464 ) ) ;
#42034 = STYLED_ITEM ( 'NONE', ( #62602 ), #6571 ) ;
#42035 = VECTOR ( 'NONE', #66036, 1000.000000000000000 ) ;
#42036 = CARTESIAN_POINT ( 'NONE',  ( -107.0049999999999955, 6.826472737025116366, 4.959722759717898555 ) ) ;
#42037 = CARTESIAN_POINT ( 'NONE',  ( 8.102448949553181734, 117.3949999999999818, 5.886773742842750679 ) ) ;
#42038 = CARTESIAN_POINT ( 'NONE',  ( -122.6949999999999790, -8.437984349512085203, 5.166775262442717831E-16 ) ) ;
#42039 =( GEOMETRIC_REPRESENTATION_CONTEXT ( 3 ) GLOBAL_UNCERTAINTY_ASSIGNED_CONTEXT ( ( #53884 ) ) GLOBAL_UNIT_ASSIGNED_CONTEXT ( ( #50006, #34492, #61546 ) ) REPRESENTATION_CONTEXT ( 'NONE', 'WORKASPACE' ) );
#42040 = EDGE_CURVE ( 'NONE', #42614, #54767, #45954, .T. ) ;
#42041 = AXIS2_PLACEMENT_3D ( 'NONE', #24552, #68897, #30177 ) ;
#42042 =( NAMED_UNIT ( * ) SI_UNIT ( $, .STERADIAN. ) SOLID_ANGLE_UNIT ( ) );
#42043 = AXIS2_PLACEMENT_3D ( 'NONE', #497, #139, #32552 ) ;
#42044 = ORIENTED_EDGE ( 'NONE', *, *, #36629, .F. ) ;
#42045 = CARTESIAN_POINT ( 'NONE',  ( -163.3429263765337964, -9.058813317711329915, 2.943386871421371787 ) ) ;
#42046 = CARTESIAN_POINT ( 'NONE',  ( -182.5449999999999875, -7.632228543268600340, -2.479861379858950166 ) ) ;
#42047 = VECTOR ( 'NONE', #7603, 1000.000000000000000 ) ;
#42048 =( NAMED_UNIT ( * ) PLANE_ANGLE_UNIT ( ) SI_UNIT ( $, .RADIAN. ) );
#42049 = MECHANICAL_DESIGN_GEOMETRIC_PRESENTATION_REPRESENTATION (  '', ( #46522 ), #13926 ) ;
#42050 = CARTESIAN_POINT ( 'NONE',  ( -20.56347600517836938, 115.3187862480272372, -10.00000000000000000 ) ) ;
#42051 = DIRECTION ( 'NONE',  ( 0.000000000000000000, 1.000000000000000000, 0.000000000000000000 ) ) ;
#42052 = SURFACE_SIDE_STYLE ('',( #5050 ) ) ;
#42053 = ORIENTED_EDGE ( 'NONE', *, *, #26635, .T. ) ;
#42054 = CARTESIAN_POINT ( 'NONE',  ( -77.99292637653380211, 8.102448949553171076, -5.886773742842744461 ) ) ;
#42055 = CONTEXT_DEPENDENT_SHAPE_REPRESENTATION ( #1918, #7065 ) ;
#42056 = DIRECTION ( 'NONE',  ( 0.000000000000000000, 0.000000000000000000, 1.000000000000000000 ) ) ;
#42057 = DIRECTION ( 'NONE',  ( -0.000000000000000000, -0.000000000000000000, -1.000000000000000000 ) ) ;
#42058 = STYLED_ITEM ( 'NONE', ( #12704 ), #47145 ) ;
#42059 = CARTESIAN_POINT ( 'NONE',  ( -15.98999599679679839, 117.4999999999999716, -10.00000000000000000 ) ) ;
#42060 = DIRECTION ( 'NONE',  ( 0.000000000000000000, 0.000000000000000000, -1.000000000000000000 ) ) ;
#42061 =( NAMED_UNIT ( * ) PLANE_ANGLE_UNIT ( ) SI_UNIT ( $, .RADIAN. ) );
#42062 = CARTESIAN_POINT ( 'NONE',  ( -183.9550000000000125, -7.632228543268599452, 2.479861379858951054 ) ) ;
#42063 =( GEOMETRIC_REPRESENTATION_CONTEXT ( 3 ) GLOBAL_UNCERTAINTY_ASSIGNED_CONTEXT ( ( #50343 ) ) GLOBAL_UNIT_ASSIGNED_CONTEXT ( ( #22193, #17298, #17634 ) ) REPRESENTATION_CONTEXT ( 'NONE', 'WORKASPACE' ) );
#42064 = EDGE_CURVE ( 'NONE', #42205, #67224, #2456, .T. ) ;
#42065 = VERTEX_POINT ( 'NONE', #34866 ) ;
#42066 = LINE ( 'NONE', #58889, #44923 ) ;
#42067 = DIRECTION ( 'NONE',  ( 1.000000000000000000, -0.000000000000000000, -0.000000000000000000 ) ) ;
#42068 = CARTESIAN_POINT ( 'NONE',  ( -74.30707362346616662, -10.01517768586948698, 6.132527647946031529E-16 ) ) ;
#42069 = VERTEX_POINT ( 'NONE', #9448 ) ;
#42070 = CARTESIAN_POINT ( 'NONE',  ( -110.0929263765347343, 3.094860106634028885, 9.524999999988660093 ) ) ;
#42071 = VECTOR ( 'NONE', #4748, 1000.000000000000000 ) ;
#42072 = FILL_AREA_STYLE ('',( #8627 ) ) ;
#42073 = CARTESIAN_POINT ( 'NONE',  ( -8.437984349512095861, 139.8070736234661240, -5.166775262442723748E-16 ) ) ;
#42074 = CARTESIAN_POINT ( 'NONE',  ( 15.98999599679679839, 117.9999999999999716, -7.500000000000000000 ) ) ;
#42075 = EDGE_CURVE ( 'NONE', #41931, #61564, #9799, .T. ) ;
#42076 = VERTEX_POINT ( 'NONE', #29590 ) ;
#42077 = LINE ( 'NONE', #63479, #44027 ) ;
#42078 = CARTESIAN_POINT ( 'NONE',  ( -92.45499999999998408, 7.632228543268599452, -2.479861379858951942 ) ) ;
#42079 = CIRCLE ( 'NONE', #11692, 3.100000000000005418 ) ;
#42080 = UNCERTAINTY_MEASURE_WITH_UNIT (LENGTH_MEASURE( 1.000000000000000082E-05 ), #15470, 'distance_accuracy_value', 'NONE');
#42081 = CARTESIAN_POINT ( 'NONE',  ( -20.71231517720797655, 149.4999999999999716, -10.00000000000000000 ) ) ;
#42082 = EDGE_LOOP ( 'NONE', ( #66172, #14685, #30598, #53230 ) ) ;
#42083 = DIRECTION ( 'NONE',  ( 0.000000000000000000, 0.000000000000000000, 1.000000000000000000 ) ) ;
#42084 = AXIS2_PLACEMENT_3D ( 'NONE', #36142, #50073, #1801 ) ;
#42085 = CARTESIAN_POINT ( 'NONE',  ( 0.000000000000000000, -3.500000000000000000, 0.000000000000000000 ) ) ;
#42086 = DIRECTION ( 'NONE',  ( 0.000000000000000000, -1.000000000000000000, 0.000000000000000000 ) ) ;
#42087 = CARTESIAN_POINT ( 'NONE',  ( -60.16140840056181105, -7.539700457364309827, -0.01736709955687108439 ) ) ;
#42088 = EDGE_CURVE ( 'NONE', #23178, #14824, #63845, .T. ) ;
#42089 = ORIENTED_EDGE ( 'NONE', *, *, #3257, .T. ) ;
#42090 = AXIS2_PLACEMENT_3D ( 'NONE', #18054, #12762, #39539 ) ;
#42091 = CARTESIAN_POINT ( 'NONE',  ( 8.082903768654762899, -1.269775441351268174E-15, 1.082903768654759125 ) ) ;
#42092 = CARTESIAN_POINT ( 'NONE',  ( -75.14499999999999602, -4.716976649647092401, 6.492361379858946790 ) ) ;
#42093 = ORIENTED_EDGE ( 'NONE', *, *, #60557, .F. ) ;
#42094 = CARTESIAN_POINT ( 'NONE',  ( 75.00000000000000000, -2.215169945516535778E-14, 9.500000000000000000 ) ) ;
#42095 = AXIS2_PLACEMENT_3D ( 'NONE', #50204, #34360, #23125 ) ;
#42096 = CARTESIAN_POINT ( 'NONE',  ( -18.00000000000000711, 33.74999999999999289, 3.750000000000000000 ) ) ;
#42097 = LINE ( 'NONE', #63822, #7198 ) ;
#42098 = EDGE_CURVE ( 'NONE', #44763, #57684, #42517, .T. ) ;
#42099 = ORIENTED_EDGE ( 'NONE', *, *, #17046, .T. ) ;
#42100 = DIRECTION ( 'NONE',  ( 0.000000000000000000, 0.000000000000000000, 1.000000000000000000 ) ) ;
#42101 = CARTESIAN_POINT ( 'NONE',  ( 8.000000000000030198, 0.000000000000000000, 29.00402776293826079 ) ) ;
#42103 = CARTESIAN_POINT ( 'NONE',  ( 0.04677136509298115974, 68.99999999999998579, -2.000000000000000000 ) ) ;
#42102 = AXIS2_PLACEMENT_3D ( 'NONE', #21120, #15199, #52811 ) ;
#42104 = VERTEX_POINT ( 'NONE', #20325 ) ;
#42105 = CARTESIAN_POINT ( 'NONE',  ( -25.00000000000000355, 37.00000000000000000, 3.000000000000000000 ) ) ;
#42106 = VERTEX_POINT ( 'NONE', #4840 ) ;
#42107 = DIRECTION ( 'NONE',  ( 0.000000000000000000, 0.000000000000000000, 1.000000000000000000 ) ) ;
#42108 = TOROIDAL_SURFACE ( 'NONE', #11712, 13.50000000000000178, 0.5000000000000000000 ) ;
#42109 = AXIS2_PLACEMENT_3D ( 'NONE', #59283, #17132, #20990 ) ;
#42110 = CARTESIAN_POINT ( 'NONE',  ( -163.7070736234661297, -3.094860106618431139, -9.524999999999991473 ) ) ;
#42111 = CARTESIAN_POINT ( 'NONE',  ( -5.598654528085806881, 118.7449999999999903, -7.705886871421374629 ) ) ;
#42112 = CARTESIAN_POINT ( 'NONE',  ( -107.3070736234661666, -10.01517768586948698, 6.132527647946031529E-16 ) ) ;
#42113 = SURFACE_STYLE_USAGE ( .BOTH. , #52291 ) ;
#42114 =( NAMED_UNIT ( * ) PLANE_ANGLE_UNIT ( ) SI_UNIT ( $, .RADIAN. ) );
#42115 = ORIENTED_EDGE ( 'NONE', *, *, #19765, .T. ) ;
#42116 =( NAMED_UNIT ( * ) SI_UNIT ( $, .STERADIAN. ) SOLID_ANGLE_UNIT ( ) );
#42118 =( NAMED_UNIT ( * ) SI_UNIT ( $, .STERADIAN. ) SOLID_ANGLE_UNIT ( ) );
#42117 = CARTESIAN_POINT ( 'NONE',  ( 4.250000000000001776, 21.74999999999998579, -3.750000000000000000 ) ) ;
#42119 = STYLED_ITEM ( 'NONE', ( #28479 ), #38249 ) ;
#42120 = CARTESIAN_POINT ( 'NONE',  ( -139.4050000000000296, -2.607480562269069768, 8.024999999999991473 ) ) ;
#42121 = DIRECTION ( 'NONE',  ( -1.156482317317873451E-16, 1.000000000000000000, 0.000000000000000000 ) ) ;
#42122 = CARTESIAN_POINT ( 'NONE',  ( -156.5949999999999704, 2.607480562269073321, 8.024999999999991473 ) ) ;
#42123 = AXIS2_PLACEMENT_3D ( 'NONE', #66980, #44175, #43374 ) ;
#42124 = CARTESIAN_POINT ( 'NONE',  ( -138.4449999999999932, 0.000000000000000000, 8.024999999999991473 ) ) ;
#42125 = ORIENTED_EDGE ( 'NONE', *, *, #18466, .T. ) ;
#42126 = COLOUR_RGB ( '', 0.66274510, 0.83137255, 0.94901961) ;
#42127 = EDGE_CURVE ( 'NONE', #51712, #22240, #50400, .T. ) ;
#42128 = CARTESIAN_POINT ( 'NONE',  ( -45.00000000000000000, 99.99999999999992895, 10.00000000000000000 ) ) ;
#42129 = CARTESIAN_POINT ( 'NONE',  ( -60.00000000000000000, -2.024042244987997205E-14, 10.50000000000000000 ) ) ;
#42130 = AXIS2_PLACEMENT_3D ( 'NONE', #17282, #38746, #60153 ) ;
#42131 = CARTESIAN_POINT ( 'NONE',  ( -49.85499999999998266, 4.716976649647094177, 6.492361379858945902 ) ) ;
#42132 =( NAMED_UNIT ( * ) PLANE_ANGLE_UNIT ( ) SI_UNIT ( $, .RADIAN. ) );
#42133 = COLOUR_RGB ( '', 0.08235294, 0.09019608, 0.10196078) ;
#42134 = CARTESIAN_POINT ( 'NONE',  ( 9.058813317711338797, 160.9549999999999841, -2.943386871421372675 ) ) ;
#42135 = CARTESIAN_POINT ( 'NONE',  ( -51.59292637653378932, -3.094860106618431139, -9.524999999999991473 ) ) ;
#42136 = DIRECTION ( 'NONE',  ( 0.6842105263157866046, 0.7292845505553195995, 0.000000000000000000 ) ) ;
#42137 = SURFACE_SIDE_STYLE ('',( #36505 ) ) ;
#42138 = DIRECTION ( 'NONE',  ( 1.663823095317152771E-15, -2.220446049250313081E-16, -1.000000000000000000 ) ) ;
#42139 = MECHANICAL_DESIGN_GEOMETRIC_PRESENTATION_REPRESENTATION (  '', ( #20753 ), #15158 ) ;
#42140 =( NAMED_UNIT ( * ) SI_UNIT ( $, .STERADIAN. ) SOLID_ANGLE_UNIT ( ) );
#42141 = ADVANCED_FACE ( 'NONE', ( #15432 ), #56315, .F. ) ;
#42142 = CARTESIAN_POINT ( 'NONE',  ( -82.10707362346614957, 8.102448949553172852, -5.886773742842744461 ) ) ;
#42143 = EDGE_CURVE ( 'NONE', #3382, #52764, #47104, .T. ) ;
#42144 = CIRCLE ( 'NONE', #7299, 0.2499999999999997780 ) ;
#42145 = FILL_AREA_STYLE ('',( #20635 ) ) ;
#42146 = EDGE_CURVE ( 'NONE', #15159, #37491, #22334, .T. ) ;
#42147 = SURFACE_SIDE_STYLE ('',( #20636 ) ) ;
#42148 = DIRECTION ( 'NONE',  ( 0.000000000000000000, 1.000000000000000000, 0.000000000000000000 ) ) ;
#42149 = CARTESIAN_POINT ( 'NONE',  ( -75.75000000000000000, -3.585786437626905077, 19.00000000000000000 ) ) ;
#42150 = ORIENTED_EDGE ( 'NONE', *, *, #67498, .F. ) ;
#42152 = VERTEX_POINT ( 'NONE', #13403 ) ;
#42151 = AXIS2_PLACEMENT_3D ( 'NONE', #6444, #32150, #48722 ) ;
#42153 = CIRCLE ( 'NONE', #3857, 7.500000000000000000 ) ;
#42154 = DIRECTION ( 'NONE',  ( 0.000000000000000000, 1.000000000000000000, 0.000000000000000000 ) ) ;
#42155 = VECTOR ( 'NONE', #22038, 1000.000000000000000 ) ;
#42156 = CARTESIAN_POINT ( 'NONE',  ( 2.607480562269071989, 116.7070736234661581, 8.025000000000002132 ) ) ;
#42157 = EDGE_CURVE ( 'NONE', #8197, #40202, #4122, .T. ) ;
#42158 = CARTESIAN_POINT ( 'NONE',  ( -20.48327417467292832, 114.7638625681370002, 10.30663925914721268 ) ) ;
#42159 = CARTESIAN_POINT ( 'NONE',  ( 23.32272074508237480, 24.55989583710051960, -27.18999999999994088 ) ) ;
#42160 =( GEOMETRIC_REPRESENTATION_CONTEXT ( 3 ) GLOBAL_UNCERTAINTY_ASSIGNED_CONTEXT ( ( #13553 ) ) GLOBAL_UNIT_ASSIGNED_CONTEXT ( ( #25679, #62974, #67574 ) ) REPRESENTATION_CONTEXT ( 'NONE', 'WORKASPACE' ) );
#42161 = CYLINDRICAL_SURFACE ( 'NONE', #56608, 0.5000000000000004441 ) ;
#42162 = EDGE_CURVE ( 'NONE', #28673, #46816, #21170, .T. ) ;
#42163 = VERTEX_POINT ( 'NONE', #15094 ) ;
#42164 = ORIENTED_EDGE ( 'NONE', *, *, #58749, .F. ) ;
#42165 = DIRECTION ( 'NONE',  ( 0.4999999999999997780, -0.8660254037844387076, 0.000000000000000000 ) ) ;
#42166 = MECHANICAL_DESIGN_GEOMETRIC_PRESENTATION_REPRESENTATION (  '', ( #15194 ), #18511 ) ;
#42167 = DIRECTION ( 'NONE',  ( -0.000000000000000000, -0.000000000000000000, -1.000000000000000000 ) ) ;
#42168 = ORIENTED_EDGE ( 'NONE', *, *, #45629, .T. ) ;
#42169 = CARTESIAN_POINT ( 'NONE',  ( 9.058813317711337021, 118.6549999999999869, 2.943386871421375783 ) ) ;
#42170 = FILL_AREA_STYLE ('',( #58980 ) ) ;
#42171 = SURFACE_STYLE_USAGE ( .BOTH. , #68503 ) ;
#42172 = MECHANICAL_DESIGN_GEOMETRIC_PRESENTATION_REPRESENTATION (  '', ( #33138 ), #56732 ) ;
#42173 = EDGE_CURVE ( 'NONE', #17554, #52516, #26772, .T. ) ;
#42174 = CARTESIAN_POINT ( 'NONE',  ( -100.3449999999999847, 7.632228543268599452, -2.479861379858951942 ) ) ;
#42175 = ORIENTED_EDGE ( 'NONE', *, *, #67914, .T. ) ;
#42176 = DIRECTION ( 'NONE',  ( 0.000000000000000000, -0.000000000000000000, 1.000000000000000000 ) ) ;
#42177 = SURFACE_STYLE_FILL_AREA ( #19612 ) ;
#42178 = CARTESIAN_POINT ( 'NONE',  ( 4.750000000000000000, 5.970153145843347347E-16, 1.000000000000000000 ) ) ;
#42179 = AXIS2_PLACEMENT_3D ( 'NONE', #5807, #32920, #17109 ) ;
#42180 = EDGE_CURVE ( 'NONE', #30684, #31434, #13329, .T. ) ;
#42181 = VERTEX_POINT ( 'NONE', #52371 ) ;
#42182 = CARTESIAN_POINT ( 'NONE',  ( 6.826472737025119919, 151.8929263765337794, 4.959722759717908325 ) ) ;
#42183 = DIRECTION ( 'NONE',  ( -0.000000000000000000, -0.000000000000000000, -1.000000000000000000 ) ) ;
#42184 = DIRECTION ( 'NONE',  ( -1.000000000000000000, -0.000000000000000000, -0.000000000000000000 ) ) ;
#42185 = CARTESIAN_POINT ( 'NONE',  ( 27.99999999999999645, 5.000000000000000000, -72.00402776293822171 ) ) ;
#42186 = ORIENTED_EDGE ( 'NONE', *, *, #5961, .T. ) ;
#42187 = CARTESIAN_POINT ( 'NONE',  ( -45.91025672304792948, 9.422403540771743025, 3.407313310066896417 ) ) ;
#42188 = FILL_AREA_STYLE ('',( #46770 ) ) ;
#42189 = CARTESIAN_POINT ( 'NONE',  ( 30.25000000000000711, 18.74999999999997868, -4.000000000000000000 ) ) ;
#42190 = DIRECTION ( 'NONE',  ( 0.9418169057949938860, 0.000000000000000000, 0.3361263392814427542 ) ) ;
#42191 = FACE_OUTER_BOUND ( 'NONE', #37874, .T. ) ;
#42192 = CARTESIAN_POINT ( 'NONE',  ( 22.99999999999996092, 0.000000000000000000, -77.00402776293825013 ) ) ;
#42193 = CIRCLE ( 'NONE', #65675, 7.499999999999984901 ) ;
#42194 =( GEOMETRIC_REPRESENTATION_CONTEXT ( 3 ) GLOBAL_UNCERTAINTY_ASSIGNED_CONTEXT ( ( #28526 ) ) GLOBAL_UNIT_ASSIGNED_CONTEXT ( ( #3058, #60800, #3414 ) ) REPRESENTATION_CONTEXT ( 'NONE', 'WORKASPACE' ) );
#42195 = CYLINDRICAL_SURFACE ( 'NONE', #39546, 0.2500000000000002220 ) ;
#42196 = CARTESIAN_POINT ( 'NONE',  ( 0.000000000000000000, 154.4999999999999432, 0.000000000000000000 ) ) ;
#42197 = CARTESIAN_POINT ( 'NONE',  ( -40.70406133565712992, -11.89285714285713880, 3.265330863013266693 ) ) ;
#42198 = ORIENTED_EDGE ( 'NONE', *, *, #36259, .F. ) ;
#42199 = ORIENTED_EDGE ( 'NONE', *, *, #34391, .T. ) ;
#42200 = CARTESIAN_POINT ( 'NONE',  ( 48.50000000000000000, 99.99999999999992895, -7.500000000000000000 ) ) ;
#42201 = DIRECTION ( 'NONE',  ( 0.000000000000000000, 0.000000000000000000, -1.000000000000000000 ) ) ;
#42202 = FACE_OUTER_BOUND ( 'NONE', #18660, .T. ) ;
#42204 =( NAMED_UNIT ( * ) PLANE_ANGLE_UNIT ( ) SI_UNIT ( $, .RADIAN. ) );
#42203 = STYLED_ITEM ( 'NONE', ( #34969 ), #63938 ) ;
#42205 = VERTEX_POINT ( 'NONE', #52703 ) ;
#42206 =( NAMED_UNIT ( * ) SI_UNIT ( $, .STERADIAN. ) SOLID_ANGLE_UNIT ( ) );
#42207 = CARTESIAN_POINT ( 'NONE',  ( -170.7549999999999955, 4.716976649647091513, -6.492361379858946790 ) ) ;
#42208 = CARTESIAN_POINT ( 'NONE',  ( -91.19292637653379074, -10.01517768586948698, 6.132527647946031529E-16 ) ) ;
#42209 = CARTESIAN_POINT ( 'NONE',  ( -147.0570736234661808, 0.000000000000000000, 9.524999999999991473 ) ) ;
#42210 = CARTESIAN_POINT ( 'NONE',  ( -46.25707362346617657, 5.598654528085800663, -7.705886871421367523 ) ) ;
#42211 = VECTOR ( 'NONE', #39702, 1000.000000000000000 ) ;
#42212 = AXIS2_PLACEMENT_3D ( 'NONE', #27998, #17166, #5507 ) ;
#42213 = CARTESIAN_POINT ( 'NONE',  ( -170.5450000000000159, -7.632228543268600340, -2.479861379858950166 ) ) ;
#42214 = ORIENTED_EDGE ( 'NONE', *, *, #21079, .T. ) ;
#42215 =( NAMED_UNIT ( * ) SI_UNIT ( $, .STERADIAN. ) SOLID_ANGLE_UNIT ( ) );
#42216 = LINE ( 'NONE', #36585, #45949 ) ;
#42217 = CARTESIAN_POINT ( 'NONE',  ( -11.23577065669009478, 11.53784018821510848, 3.306942921224938825 ) ) ;
#42218 = CARTESIAN_POINT ( 'NONE',  ( -92.00499999999998124, 6.826472737025116366, 4.959722759717898555 ) ) ;
#42219 = CARTESIAN_POINT ( 'NONE',  ( 9.435716007889201506, 154.5000000000000000, -1.372719813851188686 ) ) ;
#42220 = CARTESIAN_POINT ( 'NONE',  ( -169.4070736234663173, 3.094860106615739515, -9.525000000001949019 ) ) ;
#42221 = CARTESIAN_POINT ( 'NONE',  ( -75.04447465168979647, 36.22723619897207925, -9.923951063982375587 ) ) ;
#42222 = AXIS2_PLACEMENT_3D ( 'NONE', #51111, #40217, #63026 ) ;
#42223 = CARTESIAN_POINT ( 'NONE',  ( -92.24499999999999034, -4.716976649647093289, -6.492361379858945902 ) ) ;
#42224 = CARTESIAN_POINT ( 'NONE',  ( -5.598654528085808657, 129.7549999999999955, 7.705886871421373741 ) ) ;
#42225 = FACE_OUTER_BOUND ( 'NONE', #18372, .T. ) ;
#42226 = CIRCLE ( 'NONE', #12981, 4.999999999999997335 ) ;
#42227 = DIRECTION ( 'NONE',  ( 0.000000000000000000, 0.000000000000000000, -1.000000000000000000 ) ) ;
#42228 = CARTESIAN_POINT ( 'NONE',  ( 2.999999999999993339, 0.000000000000000000, 24.00402776293822882 ) ) ;
#42229 = PRESENTATION_LAYER_ASSIGNMENT (  '', '', ( #63507 ) ) ;
#42230 = CARTESIAN_POINT ( 'NONE',  ( -74.09292637653381064, 3.094860106618433360, 9.524999999999991473 ) ) ;
#42231 = CARTESIAN_POINT ( 'NONE',  ( -9.250000000000003553, 0.000000000000000000, 3.750000000000000000 ) ) ;
#42232 = ORIENTED_EDGE ( 'NONE', *, *, #18449, .F. ) ;
#42233 = EDGE_CURVE ( 'NONE', #56118, #25430, #5430, .T. ) ;
#42234 = CIRCLE ( 'NONE', #10743, 8.500000000000000000 ) ;
#42235 = CARTESIAN_POINT ( 'NONE',  ( -4.716976649647098618, 133.1429263765338362, 6.492361379858953008 ) ) ;
#42236 = ADVANCED_FACE ( 'NONE', ( #15771 ), #34663, .F. ) ;
#42237 = EDGE_CURVE ( 'NONE', #11986, #5856, #55216, .T. ) ;
#42238 = PRESENTATION_STYLE_ASSIGNMENT (( #20003 ) ) ;
#42240 = SURFACE_STYLE_FILL_AREA ( #31243 ) ;
#42239 = LINE ( 'NONE', #52059, #20634 ) ;
#42241 = ORIENTED_EDGE ( 'NONE', *, *, #10731, .T. ) ;
#42242 = ORIENTED_EDGE ( 'NONE', *, *, #15659, .T. ) ;
#42243 = CARTESIAN_POINT ( 'NONE',  ( 60.00000000000000000, -2.024042244987997205E-14, 7.000000000000000000 ) ) ;
#42244 = CARTESIAN_POINT ( 'NONE',  ( -135.2929263765344388, 3.094860106608008810, -9.525000000007565859 ) ) ;
#42245 = AXIS2_PLACEMENT_3D ( 'NONE', #16977, #21899, #54584 ) ;
#42246 =( GEOMETRIC_REPRESENTATION_CONTEXT ( 3 ) GLOBAL_UNCERTAINTY_ASSIGNED_CONTEXT ( ( #41218 ) ) GLOBAL_UNIT_ASSIGNED_CONTEXT ( ( #57272, #42204, #36902 ) ) REPRESENTATION_CONTEXT ( 'NONE', 'WORKASPACE' ) );
#42247 = FACE_OUTER_BOUND ( 'NONE', #34720, .T. ) ;
#42248 = DIRECTION ( 'NONE',  ( -0.000000000000000000, -1.000000000000000000, -0.000000000000000000 ) ) ;
#42249 = FILL_AREA_STYLE_COLOUR ( '', #68927 ) ;
#42250 = EDGE_CURVE ( 'NONE', #55864, #50411, #4317, .T. ) ;
#42251 = EDGE_LOOP ( 'NONE', ( #52389, #63050, #1247, #18439 ) ) ;
#42252 = CARTESIAN_POINT ( 'NONE',  ( -119.4549999999999983, 7.632228543268599452, -2.479861379858951942 ) ) ;
#42253 = ORIENTED_EDGE ( 'NONE', *, *, #36855, .T. ) ;
#42254 = MECHANICAL_DESIGN_GEOMETRIC_PRESENTATION_REPRESENTATION (  '', ( #15317 ), #19743 ) ;
#42255 = DIRECTION ( 'NONE',  ( 0.000000000000000000, 0.000000000000000000, -1.000000000000000000 ) ) ;
#42256 = FILL_AREA_STYLE_COLOUR ( '', #60168 ) ;
#42257 = ORIENTED_EDGE ( 'NONE', *, *, #43948, .F. ) ;
#42258 = ORIENTED_EDGE ( 'NONE', *, *, #14145, .F. ) ;
#42259 = AXIS2_PLACEMENT_3D ( 'NONE', #6194, #23081, #44576 ) ;
#42260 =( BOUNDED_CURVE ( )  B_SPLINE_CURVE ( 3, ( #31216, #4476, #9453, #56933 ),
 .UNSPECIFIED., .F., .T. ) 
 B_SPLINE_CURVE_WITH_KNOTS ( ( 4, 4 ),
 ( 4.712388980384695003, 6.283185307179586232 ),
 .UNSPECIFIED. ) 
 CURVE ( )  GEOMETRIC_REPRESENTATION_ITEM ( )  RATIONAL_B_SPLINE_CURVE ( ( 1.000000000000000000, 0.8047378541243662697, 0.8047378541243662697, 1.000000000000000000 ) ) 
 REPRESENTATION_ITEM ( '' )  );
#42261 = CARTESIAN_POINT ( 'NONE',  ( -10.01517768586949231, 149.1950000000000216, -6.132527647946036459E-16 ) ) ;
#42262 = FILL_AREA_STYLE_COLOUR ( '', #14975 ) ;
#42263 = VERTEX_POINT ( 'NONE', #58311 ) ;
#42264 = CARTESIAN_POINT ( 'NONE',  ( -55.10707362346616378, 8.102448949553172852, -5.886773742842744461 ) ) ;
#42265 = CARTESIAN_POINT ( 'NONE',  ( 8.102448949553179958, 151.5049999999999955, 5.886773742842750679 ) ) ;
#42266 = DIRECTION ( 'NONE',  ( 0.000000000000000000, 0.000000000000000000, 1.000000000000000000 ) ) ;
#42267 = DIRECTION ( 'NONE',  ( -0.000000000000000000, -0.000000000000000000, 1.000000000000000000 ) ) ;
#42268 = ORIENTED_EDGE ( 'NONE', *, *, #2571, .F. ) ;
#42269 = CARTESIAN_POINT ( 'NONE',  ( -2.607480562269073765, 126.0929263765338249, -8.025000000000000355 ) ) ;
#42270 = CARTESIAN_POINT ( 'NONE',  ( -60.00000000000000000, -2.024042244987997205E-14, -9.500000000000000000 ) ) ;
#42271 = DIRECTION ( 'NONE',  ( 1.000000000000000000, 1.224646799147353207E-16, 0.000000000000000000 ) ) ;
#42272 = CARTESIAN_POINT ( 'NONE',  ( 45.00000000000000000, 10.58011009419005433, 6.521986687992751719 ) ) ;
#42273 =( GEOMETRIC_REPRESENTATION_CONTEXT ( 3 ) GLOBAL_UNCERTAINTY_ASSIGNED_CONTEXT ( ( #3846 ) ) GLOBAL_UNIT_ASSIGNED_CONTEXT ( ( #56279, #34485, #34824 ) ) REPRESENTATION_CONTEXT ( 'NONE', 'WORKASPACE' ) );
#42274 = CYLINDRICAL_SURFACE ( 'NONE', #8532, 17.99999999999999645 ) ;
#42275 = EDGE_CURVE ( 'NONE', #64972, #44684, #64273, .T. ) ;
#42276 = ORIENTED_EDGE ( 'NONE', *, *, #52605, .T. ) ;
#42277 = VECTOR ( 'NONE', #63998, 1000.000000000000000 ) ;
#42278 = LINE ( 'NONE', #4914, #5955 ) ;
#42279 = ORIENTED_EDGE ( 'NONE', *, *, #43429, .T. ) ;
#42280 = CARTESIAN_POINT ( 'NONE',  ( -55.19292637653379785, -10.01517768586948698, 6.132527647946031529E-16 ) ) ;
#42281 = DIRECTION ( 'NONE',  ( 0.000000000000000000, 0.000000000000000000, 1.000000000000000000 ) ) ;
#42282 = DIRECTION ( 'NONE',  ( 2.168404344971007882E-16, 0.000000000000000000, 1.000000000000000000 ) ) ;
#42283 = CARTESIAN_POINT ( 'NONE',  ( -151.4049999999999443, -2.607480562269069768, 8.024999999999991473 ) ) ;
#42284 = EDGE_CURVE ( 'NONE', #51627, #6348, #45175, .T. ) ;
#42285 = CIRCLE ( 'NONE', #43391, 23.00000000000000000 ) ;
#42286 = CARTESIAN_POINT ( 'NONE',  ( -87.05707362346618083, 0.000000000000000000, 9.524999999999991473 ) ) ;
#42287 = CARTESIAN_POINT ( 'NONE',  ( 60.00000000000000000, 149.4999999999999716, -10.00000000000000000 ) ) ;
#42288 = DIRECTION ( 'NONE',  ( 0.000000000000000000, -1.000000000000000000, 0.000000000000000000 ) ) ;
#42289 = CARTESIAN_POINT ( 'NONE',  ( 6.826472737025119919, 145.8929263765338078, 4.959722759717908325 ) ) ;
#42290 = ORIENTED_EDGE ( 'NONE', *, *, #34024, .T. ) ;
#42291 = VERTEX_POINT ( 'NONE', #64633 ) ;
#42292 = CARTESIAN_POINT ( 'NONE',  ( 22.31832753082305132, 26.35367636051609708, 27.48619697041611687 ) ) ;
#42293 =( LENGTH_UNIT ( ) NAMED_UNIT ( * ) SI_UNIT ( .MILLI., .METRE. ) );
#42294 = CARTESIAN_POINT ( 'NONE',  ( -69.95499999999998408, -7.632228543268599452, 2.479861379858951054 ) ) ;
#42295 = VERTEX_POINT ( 'NONE', #48143 ) ;
#42296 = CARTESIAN_POINT ( 'NONE',  ( 0.000000000000000000, 2.299999999999999822, -10.00000000000000000 ) ) ;
#42297 =( NAMED_UNIT ( * ) SI_UNIT ( $, .STERADIAN. ) SOLID_ANGLE_UNIT ( ) );
#42298 = FILL_AREA_STYLE ('',( #20792 ) ) ;
#42299 = LINE ( 'NONE', #63686, #17369 ) ;
#42300 = ORIENTED_EDGE ( 'NONE', *, *, #42088, .T. ) ;
#42301 =( LENGTH_UNIT ( ) NAMED_UNIT ( * ) SI_UNIT ( .MILLI., .METRE. ) );
#42302 = DIRECTION ( 'NONE',  ( -0.000000000000000000, -0.000000000000000000, -1.000000000000000000 ) ) ;
#42303 = DIRECTION ( 'NONE',  ( -1.000000000000000000, 0.000000000000000000, 0.000000000000000000 ) ) ;
#42305 = SURFACE_SIDE_STYLE ('',( #20799 ) ) ;
#42304 = CARTESIAN_POINT ( 'NONE',  ( -20.12916642283592950, 109.9999999999999858, -10.05319148936170137 ) ) ;
#42306 = PRESENTATION_LAYER_ASSIGNMENT (  '', '', ( #55748 ) ) ;
#42307 = CARTESIAN_POINT ( 'NONE',  ( -116.9949999999999761, -6.826472737025113702, 4.959722759717902107 ) ) ;
#42308 = CARTESIAN_POINT ( 'NONE',  ( -3.094860106618434248, 146.7950000000000159, 9.525000000000000355 ) ) ;
#42309 = CARTESIAN_POINT ( 'NONE',  ( -88.04499999999998749, 7.632228543268600340, 2.479861379858949277 ) ) ;
#42310 = EDGE_CURVE ( 'NONE', #40082, #62431, #57504, .T. ) ;
#42311 = MECHANICAL_DESIGN_GEOMETRIC_PRESENTATION_REPRESENTATION (  '', ( #6281 ), #45653 ) ;
#42312 = CIRCLE ( 'NONE', #11909, 0.5000000000000004441 ) ;
#42313 = CARTESIAN_POINT ( 'NONE',  ( 44.25000000000000000, 21.99999999999998579, 4.000000000000000000 ) ) ;
#42314 = CARTESIAN_POINT ( 'NONE',  ( 179.4361977533518484, 0.000000000000000000, 103.7004518695275550 ) ) ;
#42315 = ORIENTED_EDGE ( 'NONE', *, *, #11098, .T. ) ;
#42316 = CARTESIAN_POINT ( 'NONE',  ( -129.2929263765338135, 3.094860106618428031, -9.524999999999993250 ) ) ;
#42317 = CARTESIAN_POINT ( 'NONE',  ( -75.75000000000000000, -3.000000000000000000, 6.000000000000001776 ) ) ;
#42318 = CARTESIAN_POINT ( 'NONE',  ( -153.8949999999999818, 6.826472737025116366, 4.959722759717898555 ) ) ;
#42319 = VECTOR ( 'NONE', #35456, 1000.000000000000000 ) ;
#42320 = EDGE_CURVE ( 'NONE', #28127, #50231, #11070, .T. ) ;
#42321 =( GEOMETRIC_REPRESENTATION_CONTEXT ( 3 ) GLOBAL_UNCERTAINTY_ASSIGNED_CONTEXT ( ( #38463 ) ) GLOBAL_UNIT_ASSIGNED_CONTEXT ( ( #29674, #7520, #2886 ) ) REPRESENTATION_CONTEXT ( 'NONE', 'WORKASPACE' ) );
#42322 = CARTESIAN_POINT ( 'NONE',  ( 15.98999599679679839, 146.4999999999999716, 9.500000000000000000 ) ) ;
#42323 = PRESENTATION_STYLE_ASSIGNMENT (( #41594 ) ) ;
#42324 = EDGE_LOOP ( 'NONE', ( #53257, #32496, #52631, #68704 ) ) ;
#42325 = ORIENTED_EDGE ( 'NONE', *, *, #4109, .T. ) ;
#42326 = STYLED_ITEM ( 'NONE', ( #12075 ), #57568 ) ;
#42327 = DIRECTION ( 'NONE',  ( -0.000000000000000000, -1.000000000000000000, -0.000000000000000000 ) ) ;
#42328 = CARTESIAN_POINT ( 'NONE',  ( -45.86663432203000212, 9.244254510420724102, 6.241797924670663633 ) ) ;
#42329 = LINE ( 'NONE', #15562, #67373 ) ;
#42330 = PRESENTATION_STYLE_ASSIGNMENT (( #3919 ) ) ;
#42331 = EDGE_CURVE ( 'NONE', #23279, #60866, #55090, .T. ) ;
#42332 = ORIENTED_EDGE ( 'NONE', *, *, #20283, .T. ) ;
#42333 = CARTESIAN_POINT ( 'NONE',  ( -154.2549999999999955, -4.716976649647092401, 6.492361379858946790 ) ) ;
#42334 = ORIENTED_EDGE ( 'NONE', *, *, #20972, .F. ) ;
#42335 = VERTEX_POINT ( 'NONE', #2975 ) ;
#42336 = LINE ( 'NONE', #9244, #18053 ) ;
#42337 = CARTESIAN_POINT ( 'NONE',  ( -9.827790563157511022E-16, 113.5570736234661666, 8.025000000000000355 ) ) ;
#42338 = CARTESIAN_POINT ( 'NONE',  ( -8.102448949553181734, 121.8949999999999818, -5.886773742842749790 ) ) ;
#42339 = CARTESIAN_POINT ( 'NONE',  ( 32.00000000000000000, 42.00000000000000000, -79.00402776293826435 ) ) ;
#42340 = VERTEX_POINT ( 'NONE', #23435 ) ;
#42341 = CARTESIAN_POINT ( 'NONE',  ( -6.062177826491071286, 3.500000000000000888, 0.000000000000000000 ) ) ;
#42342 = CARTESIAN_POINT ( 'NONE',  ( 5.598654528085805993, 118.3549999999999898, 7.705886871421374629 ) ) ;
#42343 = CARTESIAN_POINT ( 'NONE',  ( -65.30499999999999261, 8.437984349512086979, -1.550032578732815448E-15 ) ) ;
#42344 = DIRECTION ( 'NONE',  ( 0.000000000000000000, -0.9396926207859082059, 0.3420201433256693790 ) ) ;
#42345 = PRODUCT_DEFINITION_SHAPE ( 'NONE', 'NONE',  #69695 ) ;
#42346 = ORIENTED_EDGE ( 'NONE', *, *, #68867, .F. ) ;
#42347 = CARTESIAN_POINT ( 'NONE',  ( 3.094860106618431583, 151.2049999999999841, 9.525000000000000355 ) ) ;
#42348 = DIRECTION ( 'NONE',  ( -0.000000000000000000, -1.000000000000000000, -0.000000000000000000 ) ) ;
#42349 = CARTESIAN_POINT ( 'NONE',  ( 5.365183871890737421, 2.392512705203734935, -4.707228941936126176 ) ) ;
#42350 = FILL_AREA_STYLE ('',( #3212 ) ) ;
#42351 = AXIS2_PLACEMENT_3D ( 'NONE', #47891, #69290, #21083 ) ;
#42352 = DIRECTION ( 'NONE',  ( -0.000000000000000000, -1.000000000000000000, -0.000000000000000000 ) ) ;
#42353 = PRESENTATION_LAYER_ASSIGNMENT (  '', '', ( #36721 ) ) ;
#42354 = ORIENTED_EDGE ( 'NONE', *, *, #55098, .F. ) ;
#42355 = CARTESIAN_POINT ( 'NONE',  ( 27.00000000000001776, 15.00000000000000000, -29.68999999999999417 ) ) ;
#42356 =( NAMED_UNIT ( * ) SI_UNIT ( $, .STERADIAN. ) SOLID_ANGLE_UNIT ( ) );
#42357 = DIRECTION ( 'NONE',  ( 0.000000000000000000, 0.000000000000000000, 1.000000000000000000 ) ) ;
#42358 = CARTESIAN_POINT ( 'NONE',  ( -46.64499999999998892, 4.716976649647091513, -6.492361379858946790 ) ) ;
#42359 = ORIENTED_EDGE ( 'NONE', *, *, #15232, .F. ) ;
#42360 = DIRECTION ( 'NONE',  ( -0.000000000000000000, 1.000000000000000000, 0.000000000000000000 ) ) ;
#42361 =( BOUNDED_CURVE ( )  B_SPLINE_CURVE ( 2, ( #29003, #8285, #51522, #39972, #18814, #40296, #2595, #24773, #61374, #2938, #50495 ),
 .UNSPECIFIED., .F., .F. ) 
 B_SPLINE_CURVE_WITH_KNOTS ( ( 3, 2, 2, 2, 2, 3 ),
 ( 0.4705882352941177516, 0.4764705882352942012, 0.4823529411764707620, 0.4882352941176472116, 0.4941176470588237724, 0.5000000000000002220 ),
 .UNSPECIFIED. ) 
 CURVE ( )  GEOMETRIC_REPRESENTATION_ITEM ( )  RATIONAL_B_SPLINE_CURVE ( ( 0.9999999999999991118, 0.9510565162951544194, 1.000000000000000000, 0.9510565162951535312, 1.000000000000000000, 0.9510565162951535312, 1.000000000000000000, 0.9510565162951535312, 1.000000000000000000, 0.9510565162951516438, 1.000000000000001776 ) ) 
 REPRESENTATION_ITEM ( '' )  );
#42362 = CARTESIAN_POINT ( 'NONE',  ( 17.25000000000000711, 25.24999999999998224, 4.000000000000000000 ) ) ;
#42363 = CARTESIAN_POINT ( 'NONE',  ( 43.75000000000000000, 18.74999999999998224, -3.750000000000000000 ) ) ;
#42364 = ORIENTED_EDGE ( 'NONE', *, *, #61667, .T. ) ;
#42365 = DIRECTION ( 'NONE',  ( 0.000000000000000000, 1.000000000000000000, 0.000000000000000000 ) ) ;
#42366 = ORIENTED_EDGE ( 'NONE', *, *, #32884, .T. ) ;
#42367 = CARTESIAN_POINT ( 'NONE',  ( -128.0070736234661979, -8.102448949553174629, -5.886773742842741797 ) ) ;
#42368 = SURFACE_SIDE_STYLE ('',( #37785 ) ) ;
#42369 = CARTESIAN_POINT ( 'NONE',  ( -97.40499999999997272, -2.607480562269069768, 8.024999999999991473 ) ) ;
#42370 = ORIENTED_EDGE ( 'NONE', *, *, #52123, .F. ) ;
#42371 = PRESENTATION_STYLE_ASSIGNMENT (( #69398 ) ) ;
#42372 = SURFACE_SIDE_STYLE ('',( #63429 ) ) ;
#42373 = CARTESIAN_POINT ( 'NONE',  ( -135.8070736234661808, 10.01517768586948698, -1.839758294383808571E-15 ) ) ;
#42374 = CARTESIAN_POINT ( 'NONE',  ( 9.058813317711338797, 150.8449999999999989, -2.943386871421372675 ) ) ;
#42375 = CARTESIAN_POINT ( 'NONE',  ( -68.15707362346616094, -9.058813317711329915, -2.943386871421370898 ) ) ;
#42376 = CARTESIAN_POINT ( 'NONE',  ( -12.74999999999999822, -3.000000000000000000, 0.000000000000000000 ) ) ;
#42377 = VERTEX_POINT ( 'NONE', #55455 ) ;
#42378 =( LENGTH_UNIT ( ) NAMED_UNIT ( * ) SI_UNIT ( .MILLI., .METRE. ) );
#42379 = VECTOR ( 'NONE', #54299, 1000.000000000000000 ) ;
#42381 = SURFACE_STYLE_USAGE ( .BOTH. , #21198 ) ;
#42380 =( NAMED_UNIT ( * ) PLANE_ANGLE_UNIT ( ) SI_UNIT ( $, .RADIAN. ) );
#42382 = CARTESIAN_POINT ( 'NONE',  ( -115.1049999999999756, -6.826472737025115478, 4.959722759717900331 ) ) ;
#42383 = CARTESIAN_POINT ( 'NONE',  ( -5.598654528085806881, 118.7449999999999903, -7.705886871421374629 ) ) ;
#42384 = CARTESIAN_POINT ( 'NONE',  ( -122.2449999999999903, -4.716976649647093289, -6.492361379858945902 ) ) ;
#42385 = EDGE_CURVE ( 'NONE', #8699, #63234, #49914, .T. ) ;
#42386 = FACE_OUTER_BOUND ( 'NONE', #33552, .T. ) ;
#42387 = EDGE_CURVE ( 'NONE', #49909, #56560, #45291, .T. ) ;
#42389 = EDGE_CURVE ( 'NONE', #23750, #60430, #29022, .T. ) ;
#42388 = DIRECTION ( 'NONE',  ( 0.000000000000000000, 0.000000000000000000, -1.000000000000000000 ) ) ;
#42390 = VERTEX_POINT ( 'NONE', #33649 ) ;
#42391 = CARTESIAN_POINT ( 'NONE',  ( -167.3929263765338078, 8.102448949553176405, 5.886773742842740909 ) ) ;
#42392 = PRESENTATION_LAYER_ASSIGNMENT (  '', '', ( #33346 ) ) ;
#42393 = ADVANCED_FACE ( 'NONE', ( #45968 ), #29069, .T. ) ;
#42394 =( GEOMETRIC_REPRESENTATION_CONTEXT ( 3 ) GLOBAL_UNCERTAINTY_ASSIGNED_CONTEXT ( ( #22231 ) ) GLOBAL_UNIT_ASSIGNED_CONTEXT ( ( #10979, #363, #1409 ) ) REPRESENTATION_CONTEXT ( 'NONE', 'WORKASPACE' ) );
#42395 = DIRECTION ( 'NONE',  ( -1.000000000000000000, -9.122956858292678705E-34, 1.300977106640434891E-16 ) ) ;
#42396 = EDGE_CURVE ( 'NONE', #16364, #45002, #52595, .T. ) ;
#42397 = MECHANICAL_DESIGN_GEOMETRIC_PRESENTATION_REPRESENTATION (  '', ( #35627 ), #48020 ) ;
#42398 = CARTESIAN_POINT ( 'NONE',  ( -20.26325459587049238, 115.0245731144845394, -10.00000000000000000 ) ) ;
#42399 = CARTESIAN_POINT ( 'NONE',  ( 71.50000000000000000, 14.49137674618942562, 7.500000000000000000 ) ) ;
#42400 = ORIENTED_EDGE ( 'NONE', *, *, #56448, .T. ) ;
#42401 = EDGE_CURVE ( 'NONE', #21177, #2846, #39652, .T. ) ;
#42402 = CARTESIAN_POINT ( 'NONE',  ( -80.99292637653380211, 8.102448949553171076, -5.886773742842744461 ) ) ;
#42403 = CONTEXT_DEPENDENT_SHAPE_REPRESENTATION ( #66707, #48069 ) ;
#42404 = DIRECTION ( 'NONE',  ( 1.000000000000000000, 0.000000000000000000, 0.000000000000000000 ) ) ;
#42405 = PRESENTATION_STYLE_ASSIGNMENT (( #69097 ) ) ;
#42406 = EDGE_CURVE ( 'NONE', #29227, #56343, #17861, .T. ) ;
#42407 = DIRECTION ( 'NONE',  ( 0.000000000000000000, -1.000000000000000000, 0.000000000000000000 ) ) ;
#42408 = DIRECTION ( 'NONE',  ( -1.000000000000000000, 0.000000000000000000, 0.000000000000000000 ) ) ;
#42409 = CARTESIAN_POINT ( 'NONE',  ( 60.00000000000000000, 1.797044900979284448E-15, -12.00000000000000000 ) ) ;
#42410 = AXIS2_PLACEMENT_3D ( 'NONE', #21521, #22221, #10633 ) ;
#42411 = CARTESIAN_POINT ( 'NONE',  ( -179.0049999999999955, 6.826472737025115478, 4.959722759717899443 ) ) ;
#42412 = VERTEX_POINT ( 'NONE', #29038 ) ;
#42413 =( NAMED_UNIT ( * ) PLANE_ANGLE_UNIT ( ) SI_UNIT ( $, .RADIAN. ) );
#42414 = FACE_OUTER_BOUND ( 'NONE', #60421, .T. ) ;
#42415 = CARTESIAN_POINT ( 'NONE',  ( -182.4570736234661865, -9.058813317711329915, 2.943386871421371787 ) ) ;
#42416 = CARTESIAN_POINT ( 'NONE',  ( 7.632228543268608334, 147.4570736234661581, -2.479861379858951942 ) ) ;
#42417 = ORIENTED_EDGE ( 'NONE', *, *, #57437, .T. ) ;
#42418 = CARTESIAN_POINT ( 'NONE',  ( -30.83671138439772719, -8.500000000000087041, -0.2331546148446474176 ) ) ;
#42419 = CARTESIAN_POINT ( 'NONE',  ( -89.15499999999998693, 7.632228543268600340, 2.479861379858949277 ) ) ;
#42420 = LINE ( 'NONE', #48044, #55552 ) ;
#42421 = ORIENTED_EDGE ( 'NONE', *, *, #38955, .F. ) ;
#42422 = CARTESIAN_POINT ( 'NONE',  ( 0.9126302363881977353, -2.499999999999996447, -9.000000000000007105 ) ) ;
#42423 = CARTESIAN_POINT ( 'NONE',  ( -54.49999999999999289, -2.024042244987997205E-14, -6.500000000000000000 ) ) ;
#42424 = DIRECTION ( 'NONE',  ( 0.7071067811865451302, 0.000000000000000000, 0.7071067811865500152 ) ) ;
#42425 = CARTESIAN_POINT ( 'NONE',  ( -60.70461754965443646, -7.499999999999992006, 0.000000000000000000 ) ) ;
#42426 = ORIENTED_EDGE ( 'NONE', *, *, #43793, .F. ) ;
#42427 = LINE ( 'NONE', #63818, #68792 ) ;
#42428 = CARTESIAN_POINT ( 'NONE',  ( -69.89499999999999602, 6.826472737025116366, 4.959722759717898555 ) ) ;
#42429 = VERTEX_POINT ( 'NONE', #56490 ) ;
#42430 = CARTESIAN_POINT ( 'NONE',  ( 15.98999599679679839, 146.4999999999999716, 7.000000000000000000 ) ) ;
#42431 =( NAMED_UNIT ( * ) SI_UNIT ( $, .STERADIAN. ) SOLID_ANGLE_UNIT ( ) );
#42432 = ORIENTED_EDGE ( 'NONE', *, *, #26438, .T. ) ;
#42433 = CARTESIAN_POINT ( 'NONE',  ( -41.49999999999997868, 10.49999999999998046, -3.000000000000000444 ) ) ;
#42434 =( GEOMETRIC_REPRESENTATION_CONTEXT ( 3 ) GLOBAL_UNCERTAINTY_ASSIGNED_CONTEXT ( ( #17195 ) ) GLOBAL_UNIT_ASSIGNED_CONTEXT ( ( #35580, #36301, #47206 ) ) REPRESENTATION_CONTEXT ( 'NONE', 'WORKASPACE' ) );
#42435 = SURFACE_SIDE_STYLE ('',( #48060 ) ) ;
#42436 = SURFACE_STYLE_USAGE ( .BOTH. , #42786 ) ;
#42437 = ORIENTED_EDGE ( 'NONE', *, *, #11940, .T. ) ;
#42438 = CIRCLE ( 'NONE', #46962, 9.000000000000007105 ) ;
#42439 = DIRECTION ( 'NONE',  ( 0.000000000000000000, 1.000000000000000000, 0.000000000000000000 ) ) ;
#42440 = ORIENTED_EDGE ( 'NONE', *, *, #64224, .F. ) ;
#42441 = FILL_AREA_STYLE_COLOUR ( '', #6591 ) ;
#42442 = CYLINDRICAL_SURFACE ( 'NONE', #12777, 1.000000000000000888 ) ;
#42443 = DIRECTION ( 'NONE',  ( 0.000000000000000000, 1.000000000000000000, -0.000000000000000000 ) ) ;
#42444 = CARTESIAN_POINT ( 'NONE',  ( -156.3570736234661922, 5.598654528085804216, 7.705886871421366635 ) ) ;
#42445 = CARTESIAN_POINT ( 'NONE',  ( -3.094860106618434248, 119.7949999999999733, 9.525000000000000355 ) ) ;
#42446 = CARTESIAN_POINT ( 'NONE',  ( -105.9570736234661865, 9.058813317711329915, -2.943386871421373119 ) ) ;
#42447 = DIRECTION ( 'NONE',  ( -1.000000000000000000, 0.000000000000000000, 0.000000000000000000 ) ) ;
#42448 = ORIENTED_EDGE ( 'NONE', *, *, #12721, .F. ) ;
#42449 = LINE ( 'NONE', #67753, #65478 ) ;
#42450 = LINE ( 'NONE', #63512, #36899 ) ;
#42451 = FILL_AREA_STYLE ('',( #59247 ) ) ;
#42452 = CIRCLE ( 'NONE', #3018, 0.2500000000000002220 ) ;
#42453 = CARTESIAN_POINT ( 'NONE',  ( -143.0050000000000239, 6.826472737025116366, 4.959722759717898555 ) ) ;
#42454 = CARTESIAN_POINT ( 'NONE',  ( 57.49999999999999289, 28.24999999999998934, -3.750000000000000000 ) ) ;
#42455 = DIRECTION ( 'NONE',  ( 0.000000000000000000, 1.000000000000000000, 0.000000000000000000 ) ) ;
#42456 = CARTESIAN_POINT ( 'NONE',  ( -157.7950000000000159, 2.607480562269068880, -8.024999999999993250 ) ) ;
#42457 = EDGE_CURVE ( 'NONE', #40929, #59357, #50538, .T. ) ;
#42458 = CARTESIAN_POINT ( 'NONE',  ( -137.5449999999999875, -7.632228543268600340, -2.479861379858950166 ) ) ;
#42459 = ORIENTED_EDGE ( 'NONE', *, *, #33865, .F. ) ;
#42460 = ADVANCED_FACE ( 'NONE', ( #23788 ), #24464, .F. ) ;
#42461 = CARTESIAN_POINT ( 'NONE',  ( 36.00000000000002842, 0.000000000000000000, 29.00402776293825724 ) ) ;
#42462 = CARTESIAN_POINT ( 'NONE',  ( 4.750000000000002665, 24.99999999999998579, 3.750000000000000000 ) ) ;
#42463 = FACE_OUTER_BOUND ( 'NONE', #49983, .T. ) ;
#42464 = UNCERTAINTY_MEASURE_WITH_UNIT (LENGTH_MEASURE( 1.000000000000000082E-05 ), #39838, 'distance_accuracy_value', 'NONE');
#42465 = CARTESIAN_POINT ( 'NONE',  ( -56.60499999999998266, 6.826472737025113702, -4.959722759717902107 ) ) ;
#42466 = LINE ( 'NONE', #37894, #64639 ) ;
#42467 = CARTESIAN_POINT ( 'NONE',  ( 17.25000000000000711, 25.24999999999998224, -4.000000000000000000 ) ) ;
#42468 = EDGE_CURVE ( 'NONE', #30840, #35810, #67320, .T. ) ;
#42469 = CARTESIAN_POINT ( 'NONE',  ( -7.342319042881618962, -2.499999999999994671, 5.282730372348551029 ) ) ;
#42470 = UNCERTAINTY_MEASURE_WITH_UNIT (LENGTH_MEASURE( 1.000000000000000082E-05 ), #67001, 'distance_accuracy_value', 'NONE');
#42471 = CARTESIAN_POINT ( 'NONE',  ( 1.700000000000067679, 50.00000000000002132, 60.00000000000001421 ) ) ;
#42472 = ADVANCED_FACE ( 'NONE', ( #18842 ), #29768, .T. ) ;
#42473 = CARTESIAN_POINT ( 'NONE',  ( -89.00707362346618368, -8.102448949553174629, -5.886773742842741797 ) ) ;
#42474 = CARTESIAN_POINT ( 'NONE',  ( 4.000000000000002665, 37.76051491742381216, -89.34202014332566932 ) ) ;
#42475 = CIRCLE ( 'NONE', #3052, 0.5000000000000004441 ) ;
#42476 = VECTOR ( 'NONE', #41837, 1000.000000000000000 ) ;
#42477 = SURFACE_STYLE_USAGE ( .BOTH. , #52997 ) ;
#42478 = CARTESIAN_POINT ( 'NONE',  ( -9.827790563157511022E-16, 139.4429263765338192, 8.025000000000000355 ) ) ;
#42479 = PLANE ( 'NONE',  #48794 ) ;
#42480 = FILL_AREA_STYLE ('',( #64595 ) ) ;
#42481 = ORIENTED_EDGE ( 'NONE', *, *, #25803, .F. ) ;
#42482 = FILL_AREA_STYLE ('',( #16084 ) ) ;
#42483 = VECTOR ( 'NONE', #61771, 1000.000000000000000 ) ;
#42484 = CARTESIAN_POINT ( 'NONE',  ( -4.716976649647098618, 110.2570736234661695, 6.492361379858953008 ) ) ;
#42485 = FACE_OUTER_BOUND ( 'NONE', #63974, .T. ) ;
#42486 = DIRECTION ( 'NONE',  ( 1.000000000000000000, 0.000000000000000000, 0.000000000000000000 ) ) ;
#42487 =( GEOMETRIC_REPRESENTATION_CONTEXT ( 3 ) GLOBAL_UNCERTAINTY_ASSIGNED_CONTEXT ( ( #63534 ) ) GLOBAL_UNIT_ASSIGNED_CONTEXT ( ( #53578, #62725, #42042 ) ) REPRESENTATION_CONTEXT ( 'NONE', 'WORKASPACE' ) );
#42488 = DIRECTION ( 'NONE',  ( -1.000000000000000000, 0.000000000000000000, 0.000000000000000000 ) ) ;
#42489 = ORIENTED_EDGE ( 'NONE', *, *, #37850, .T. ) ;
#42490 = ORIENTED_EDGE ( 'NONE', *, *, #22347, .T. ) ;
#42491 = DIRECTION ( 'NONE',  ( 1.000000000000000000, 0.000000000000000000, 0.000000000000000000 ) ) ;
#42492 =( GEOMETRIC_REPRESENTATION_CONTEXT ( 3 ) GLOBAL_UNCERTAINTY_ASSIGNED_CONTEXT ( ( #25664 ) ) GLOBAL_UNIT_ASSIGNED_CONTEXT ( ( #46318, #30081, #29753 ) ) REPRESENTATION_CONTEXT ( 'NONE', 'WORKASPACE' ) );
#42493 = DIRECTION ( 'NONE',  ( 0.000000000000000000, 0.000000000000000000, -1.000000000000000000 ) ) ;
#42494 = CARTESIAN_POINT ( 'NONE',  ( -101.8429263765338106, 9.058813317711329915, -2.943386871421373119 ) ) ;
#42495 = ORIENTED_EDGE ( 'NONE', *, *, #16078, .F. ) ;
#42496 = CARTESIAN_POINT ( 'NONE',  ( -3.094860106618432471, 122.7049999999999699, -9.525000000000000355 ) ) ;
#42497 =( NAMED_UNIT ( * ) SI_UNIT ( $, .STERADIAN. ) SOLID_ANGLE_UNIT ( ) );
#42498 = CARTESIAN_POINT ( 'NONE',  ( -105.1449999999999818, -4.716976649647092401, 6.492361379858946790 ) ) ;
#42499 = VERTEX_POINT ( 'NONE', #35041 ) ;
#42500 = EDGE_CURVE ( 'NONE', #28999, #50847, #23114, .T. ) ;
#42501 = DIRECTION ( 'NONE',  ( -1.000000000000000000, 0.000000000000000000, 0.000000000000000000 ) ) ;
#42502 = ORIENTED_EDGE ( 'NONE', *, *, #14156, .T. ) ;
#42503 = CARTESIAN_POINT ( 'NONE',  ( 7.632228543268607446, 158.0429263765338419, 2.479861379858954606 ) ) ;
#42504 = FILL_AREA_STYLE_COLOUR ( '', #25655 ) ;
#42505 = CARTESIAN_POINT ( 'NONE',  ( 6.020204320972966094, 1.861307952554195122, 7.572700244129132230 ) ) ;
#42506 = SURFACE_STYLE_FILL_AREA ( #21701 ) ;
#42507 = CARTESIAN_POINT ( 'NONE',  ( 21.02379604162863558, 114.4999999999999574, -10.00000000000000000 ) ) ;
#42508 = ORIENTED_EDGE ( 'NONE', *, *, #6344, .F. ) ;
#42509 = FACE_OUTER_BOUND ( 'NONE', #40508, .T. ) ;
#42510 = FACE_OUTER_BOUND ( 'NONE', #55275, .T. ) ;
#42511 = PRESENTATION_STYLE_ASSIGNMENT (( #4460 ) ) ;
#42512 = DIRECTION ( 'NONE',  ( -0.000000000000000000, -0.000000000000000000, -1.000000000000000000 ) ) ;
#42513 = SURFACE_SIDE_STYLE ('',( #54403 ) ) ;
#42514 = CARTESIAN_POINT ( 'NONE',  ( -126.2929263765345524, 3.094860106606193817, -9.525000000008883916 ) ) ;
#42515 = LINE ( 'NONE', #55001, #8085 ) ;
#42516 = CARTESIAN_POINT ( 'NONE',  ( 0.000000000000000000, 116.9429263765338192, -8.025000000000000355 ) ) ;
#42517 = LINE ( 'NONE', #29230, #60473 ) ;
#42518 = VERTEX_POINT ( 'NONE', #39310 ) ;
#42519 = AXIS2_PLACEMENT_3D ( 'NONE', #42362, #5008, #52876 ) ;
#42520 = ORIENTED_EDGE ( 'NONE', *, *, #54329, .T. ) ;
#42521 = DIRECTION ( 'NONE',  ( 0.000000000000000000, -1.000000000000000000, 0.000000000000000000 ) ) ;
#42522 = AXIS2_PLACEMENT_3D ( 'NONE', #6924, #5870, #23440 ) ;
#42523 = DIRECTION ( 'NONE',  ( -0.000000000000000000, -0.000000000000000000, 1.000000000000000000 ) ) ;
#42524 = DIRECTION ( 'NONE',  ( -0.000000000000000000, -1.000000000000000000, -0.000000000000000000 ) ) ;
#42525 = EDGE_CURVE ( 'NONE', #37663, #53214, #60714, .T. ) ;
#42526 = CARTESIAN_POINT ( 'NONE',  ( -9.827790563157511022E-16, 113.5570736234661666, 8.025000000000000355 ) ) ;
#42527 = EDGE_LOOP ( 'NONE', ( #16296, #53726, #9550, #38613 ) ) ;
#42528 = CARTESIAN_POINT ( 'NONE',  ( -153.4429263765338192, -1.166476076187852838E-15, -9.524999999999991473 ) ) ;
#42529 = CARTESIAN_POINT ( 'NONE',  ( -165.2050000000000125, -2.607480562269071545, -8.024999999999991473 ) ) ;
#42530 = EDGE_CURVE ( 'NONE', #62740, #10009, #31345, .T. ) ;
#42531 = CARTESIAN_POINT ( 'NONE',  ( -195.0000000000000000, 0.000000000000000000, 9.524999999999991473 ) ) ;
#42532 = DIRECTION ( 'NONE',  ( -1.000000000000000000, 0.000000000000000000, 0.000000000000000000 ) ) ;
#42533 = CARTESIAN_POINT ( 'NONE',  ( -50.30707362346617373, -10.01517768586948698, 6.132527647946031529E-16 ) ) ;
#42534 = CIRCLE ( 'NONE', #22297, 18.99999999999998934 ) ;
#42535 = CARTESIAN_POINT ( 'NONE',  ( -167.8449999999999989, -7.632228543268599452, 2.479861379858951054 ) ) ;
#42536 = EDGE_LOOP ( 'NONE', ( #49903, #23851, #22620, #32468 ) ) ;
#42537 = FACE_OUTER_BOUND ( 'NONE', #18397, .T. ) ;
#42538 = EDGE_CURVE ( 'NONE', #54457, #65703, #40367, .T. ) ;
#42539 = CARTESIAN_POINT ( 'NONE',  ( 6.000000000000017764, 43.00000000000000000, 35.50000000000000000 ) ) ;
#42540 = CARTESIAN_POINT ( 'NONE',  ( -10.03217797797695354, 11.98647912738839239, 0.6570571964558979960 ) ) ;
#42541 = CARTESIAN_POINT ( 'NONE',  ( -79.70499999999995566, 2.607480562269073321, 8.024999999999991473 ) ) ;
#42542 = CARTESIAN_POINT ( 'NONE',  ( 1.000000000000000000, 36.74999999999999289, -3.000000000000000000 ) ) ;
#42544 = CARTESIAN_POINT ( 'NONE',  ( -74.66854778504175272, 36.33518165874313866, -9.980650098286423244 ) ) ;
#42543 = CIRCLE ( 'NONE', #22311, 0.5000000000000004441 ) ;
#42545 = CARTESIAN_POINT ( 'NONE',  ( -79.79499999999998749, 2.607480562269069324, -8.024999999999993250 ) ) ;
#42546 = CARTESIAN_POINT ( 'NONE',  ( 3.094860106618431583, 127.2049999999999841, 9.525000000000000355 ) ) ;
#42547 = DIRECTION ( 'NONE',  ( 0.000000000000000000, 0.000000000000000000, 1.000000000000000000 ) ) ;
#42548 = EDGE_CURVE ( 'NONE', #13184, #65559, #68444, .T. ) ;
#42549 = PLANE ( 'NONE',  #20307 ) ;
#42550 = UNCERTAINTY_MEASURE_WITH_UNIT (LENGTH_MEASURE( 1.000000000000000082E-05 ), #56571, 'distance_accuracy_value', 'NONE');
#42551 = FACE_OUTER_BOUND ( 'NONE', #52758, .T. ) ;
#42552 =( NAMED_UNIT ( * ) PLANE_ANGLE_UNIT ( ) SI_UNIT ( $, .RADIAN. ) );
#42553 = ORIENTED_EDGE ( 'NONE', *, *, #12851, .F. ) ;
#42554 = COLOUR_RGB ( '', 0.31764706, 0.68627451, 0.89019608) ;
#42555 = ADVANCED_FACE ( 'NONE', ( #68809 ), #47751, .F. ) ;
#42556 = AXIS2_PLACEMENT_3D ( 'NONE', #59868, #6395, #65849 ) ;
#42557 = DIRECTION ( 'NONE',  ( 1.000000000000000000, 1.665334536937734495E-14, 0.000000000000000000 ) ) ;
#42559 = CARTESIAN_POINT ( 'NONE',  ( 8.046771365092977746, 72.00000000000001421, 12.50000000000000000 ) ) ;
#42558 = CARTESIAN_POINT ( 'NONE',  ( 13.25000000000000355, 28.24999999999998934, 3.750000000000000000 ) ) ;
#42560 = DIRECTION ( 'NONE',  ( 0.000000000000000000, 0.000000000000000000, 1.000000000000000000 ) ) ;
#42561 = EDGE_LOOP ( 'NONE', ( #45848, #15174, #20288, #38722 ) ) ;
#42562 = CIRCLE ( 'NONE', #12171, 8.025000000000000355 ) ;
#42563 = ORIENTED_EDGE ( 'NONE', *, *, #15906, .F. ) ;
#42564 = FACE_BOUND ( 'NONE', #47951, .T. ) ;
#42565 = CARTESIAN_POINT ( 'NONE',  ( -174.5070736234661410, 8.102448949553176405, 5.886773742842740909 ) ) ;
#42567 = CIRCLE ( 'NONE', #39194, 1.000000000000000888 ) ;
#42566 = UNCERTAINTY_MEASURE_WITH_UNIT (LENGTH_MEASURE( 1.000000000000000082E-05 ), #44030, 'distance_accuracy_value', 'NONE');
#42568 = SURFACE_SIDE_STYLE ('',( #31617 ) ) ;
#42569 = AXIS2_PLACEMENT_3D ( 'NONE', #50143, #17454, #44551 ) ;
#42570 = LINE ( 'NONE', #8789, #65544 ) ;
#42571 = ORIENTED_EDGE ( 'NONE', *, *, #22332, .F. ) ;
#42572 = CARTESIAN_POINT ( 'NONE',  ( -124.8549999999999898, 4.716976649647094177, 6.492361379858945902 ) ) ;
#42573 = ORIENTED_EDGE ( 'NONE', *, *, #47663, .T. ) ;
#42574 = ORIENTED_EDGE ( 'NONE', *, *, #68808, .T. ) ;
#42575 = CARTESIAN_POINT ( 'NONE',  ( -74.50000000000000000, -2.220952357103124925E-14, -9.500000000000000000 ) ) ;
#42576 = CARTESIAN_POINT ( 'NONE',  ( -87.50000000000000000, -6.499999999999990230, 21.00000000000000000 ) ) ;
#42577 = ORIENTED_EDGE ( 'NONE', *, *, #40277, .F. ) ;
#42578 = STYLED_ITEM ( 'NONE', ( #53982 ), #14812 ) ;
#42579 = SURFACE_SIDE_STYLE ('',( #59380 ) ) ;
#42580 = CARTESIAN_POINT ( 'NONE',  ( 8.102448949553181734, 153.3950000000000387, 5.886773742842750679 ) ) ;
#42581 = CARTESIAN_POINT ( 'NONE',  ( -83.49999999999997158, 50.00000000000000000, 12.00000000000000000 ) ) ;
#42582 = ADVANCED_FACE ( 'NONE', ( #51567 ), #41745, .F. ) ;
#42583 = VERTEX_POINT ( 'NONE', #62462 ) ;
#42584 = LINE ( 'NONE', #5932, #54629 ) ;
#42585 = CARTESIAN_POINT ( 'NONE',  ( -10.01517768586949408, 153.3050000000000068, -6.132527647946036459E-16 ) ) ;
#42586 = CARTESIAN_POINT ( 'NONE',  ( 0.000000000000000000, 42.00000000000000000, 79.00402776293826435 ) ) ;
#42587 = ORIENTED_EDGE ( 'NONE', *, *, #23658, .T. ) ;
#42588 = CARTESIAN_POINT ( 'NONE',  ( -8.437984349512095861, 129.6929263765338192, -5.166775262442723748E-16 ) ) ;
#42589 = DIRECTION ( 'NONE',  ( -1.000000000000000000, 0.000000000000000000, 0.000000000000000000 ) ) ;
#42590 = UNCERTAINTY_MEASURE_WITH_UNIT (LENGTH_MEASURE( 1.000000000000000082E-05 ), #7668, 'distance_accuracy_value', 'NONE');
#42591 = CARTESIAN_POINT ( 'NONE',  ( -75.48275862068966546, 36.00832590023090063, -9.555431496530900404 ) ) ;
#42592 =( NAMED_UNIT ( * ) PLANE_ANGLE_UNIT ( ) SI_UNIT ( $, .RADIAN. ) );
#42593 = DIRECTION ( 'NONE',  ( 1.445602896647337931E-16, -1.000000000000000000, 0.000000000000000000 ) ) ;
#42594 = VERTEX_POINT ( 'NONE', #36101 ) ;
#42595 = DIRECTION ( 'NONE',  ( 0.000000000000000000, 0.000000000000000000, -1.000000000000000000 ) ) ;
#42596 = VERTEX_POINT ( 'NONE', #13933 ) ;
#42597 = CARTESIAN_POINT ( 'NONE',  ( -61.04292637653379927, -9.058813317711329915, -2.943386871421370898 ) ) ;
#42598 = LINE ( 'NONE', #35903, #45787 ) ;
#42599 = PRESENTATION_STYLE_ASSIGNMENT (( #57709 ) ) ;
#42600 = CARTESIAN_POINT ( 'NONE',  ( -147.5049999999999955, -6.826472737025115478, -4.959722759717899443 ) ) ;
#42601 = CARTESIAN_POINT ( 'NONE',  ( -177.0570736234661808, 0.000000000000000000, 9.524999999999991473 ) ) ;
#42602 = UNCERTAINTY_MEASURE_WITH_UNIT (LENGTH_MEASURE( 1.000000000000000082E-05 ), #5705, 'distance_accuracy_value', 'NONE');
#42603 = EDGE_CURVE ( 'NONE', #47060, #61874, #37036, .T. ) ;
#42604 = VECTOR ( 'NONE', #45897, 1000.000000000000114 ) ;
#42605 = FACE_OUTER_BOUND ( 'NONE', #21716, .T. ) ;
#42606 = FACE_OUTER_BOUND ( 'NONE', #2237, .T. ) ;
#42607 = ORIENTED_EDGE ( 'NONE', *, *, #40826, .T. ) ;
#42608 = ORIENTED_EDGE ( 'NONE', *, *, #35314, .F. ) ;
#42609 = CYLINDRICAL_SURFACE ( 'NONE', #37367, 0.2500000000000002220 ) ;
#42610 = AXIS2_PLACEMENT_3D ( 'NONE', #1589, #12888, #7605 ) ;
#42611 = FILL_AREA_STYLE_COLOUR ( '', #6419 ) ;
#42612 = EDGE_CURVE ( 'NONE', #2500, #32796, #28291, .T. ) ;
#42613 = CARTESIAN_POINT ( 'NONE',  ( -64.25499999999998124, -4.716976649647092401, 6.492361379858946790 ) ) ;
#42614 = VERTEX_POINT ( 'NONE', #30427 ) ;
#42615 = DIRECTION ( 'NONE',  ( -2.168404344971009361E-16, 1.000000000000000000, 0.000000000000000000 ) ) ;
#42616 = SURFACE_STYLE_FILL_AREA ( #21116 ) ;
#42617 = EDGE_CURVE ( 'NONE', #43509, #18673, #51929, .T. ) ;
#42618 = CARTESIAN_POINT ( 'NONE',  ( 57.00000000000000000, 14.00000000000000000, -60.00402776293827145 ) ) ;
#42619 = CARTESIAN_POINT ( 'NONE',  ( 57.74999999999999289, 28.24999999999998934, 3.750000000000000000 ) ) ;
#42620 = AXIS2_PLACEMENT_3D ( 'NONE', #43292, #12230, #16531 ) ;
#42621 = PRESENTATION_STYLE_ASSIGNMENT (( #33073 ) ) ;
#42622 = ORIENTED_EDGE ( 'NONE', *, *, #67026, .T. ) ;
#42623 = ADVANCED_FACE ( 'NONE', ( #57541 ), #63883, .F. ) ;
#42624 = CARTESIAN_POINT ( 'NONE',  ( 0.000000000000000000, 152.9999999999999716, 0.000000000000000000 ) ) ;
#42625 = DIRECTION ( 'NONE',  ( -0.000000000000000000, 1.000000000000000000, -0.000000000000000000 ) ) ;
#42627 =( NAMED_UNIT ( * ) PLANE_ANGLE_UNIT ( ) SI_UNIT ( $, .RADIAN. ) );
#42626 =( BOUNDED_CURVE ( )  B_SPLINE_CURVE ( 2, ( #31946, #5894, #37278, #43594, #54431, #60061, #889, #32289, #43255, #11177, #48867 ),
 .UNSPECIFIED., .F., .F. ) 
 B_SPLINE_CURVE_WITH_KNOTS ( ( 3, 2, 2, 2, 2, 3 ),
 ( 0.3478260869565134583, 0.3499999999999916511, 0.3521739130434698994, 0.3543478260869481478, 0.3565217391304263406, 0.3586956521739045334 ),
 .UNSPECIFIED. ) 
 CURVE ( )  GEOMETRIC_REPRESENTATION_ITEM ( )  RATIONAL_B_SPLINE_CURVE ( ( 1.000000000000186295, 0.9510565162949673468, 1.000000000000000000, 0.9510565162951535312, 1.000000000000000000, 0.9510565162951535312, 1.000000000000000000, 0.9510565162951535312, 1.000000000000000000, 0.9510565162953447116, 0.9999999999998088196 ) ) 
 REPRESENTATION_ITEM ( '' )  );
#42628 = DIRECTION ( 'NONE',  ( 0.000000000000000000, 1.000000000000000000, 0.000000000000000000 ) ) ;
#42629 = CIRCLE ( 'NONE', #12223, 0.5000000000000004441 ) ;
#42630 = EDGE_CURVE ( 'NONE', #14819, #23416, #4385, .T. ) ;
#42631 = CARTESIAN_POINT ( 'NONE',  ( -123.1449999999999960, -4.716976649647092401, 6.492361379858946790 ) ) ;
#42632 = CARTESIAN_POINT ( 'NONE',  ( -1.166476076187854022E-15, 149.9449999999999932, 9.525000000000000355 ) ) ;
#42633 = CARTESIAN_POINT ( 'NONE',  ( -83.69499999999997897, -8.437984349512085203, 5.166775262442717831E-16 ) ) ;
#42634 = AXIS2_PLACEMENT_3D ( 'NONE', #43428, #64815, #59522 ) ;
#42635 = FILL_AREA_STYLE_COLOUR ( '', #5578 ) ;
#42636 = UNCERTAINTY_MEASURE_WITH_UNIT (LENGTH_MEASURE( 1.000000000000000082E-05 ), #14761, 'distance_accuracy_value', 'NONE');
#42637 = PRESENTATION_LAYER_ASSIGNMENT (  '', '', ( #33600 ) ) ;
#42638 = ORIENTED_EDGE ( 'NONE', *, *, #34062, .F. ) ;
#42639 = CARTESIAN_POINT ( 'NONE',  ( -133.9429263765338192, 0.000000000000000000, 9.524999999999991473 ) ) ;
#42640 = CARTESIAN_POINT ( 'NONE',  ( -32.76851741822840580, -9.107254030101904263, -2.000000000000000000 ) ) ;
#42641 = CARTESIAN_POINT ( 'NONE',  ( -146.6949999999999932, -8.437984349512085203, 5.166775262442717831E-16 ) ) ;
#42642 = CARTESIAN_POINT ( 'NONE',  ( 1.000000000000000000, 14.00000000000000533, 35.50000000000000000 ) ) ;
#42643 = VECTOR ( 'NONE', #27665, 1000.000000000000000 ) ;
#42644 = ADVANCED_FACE ( 'NONE', ( #33236 ), #6475, .F. ) ;
#42645 = DIRECTION ( 'NONE',  ( 1.000000000000000000, -0.000000000000000000, 0.000000000000000000 ) ) ;
#42646 = VERTEX_POINT ( 'NONE', #64882 ) ;
#42647 = ORIENTED_EDGE ( 'NONE', *, *, #55366, .F. ) ;
#42648 = EDGE_CURVE ( 'NONE', #32941, #10860, #38467, .T. ) ;
#42649 =( BOUNDED_CURVE ( )  B_SPLINE_CURVE ( 3, ( #14256, #63137, #52607, #68778 ),
 .UNSPECIFIED., .F., .F. ) 
 B_SPLINE_CURVE_WITH_KNOTS ( ( 4, 4 ),
 ( 1.570796326794896780, 2.351346768814402743 ),
 .UNSPECIFIED. ) 
 CURVE ( )  GEOMETRIC_REPRESENTATION_ITEM ( )  RATIONAL_B_SPLINE_CURVE ( ( 1.000000000000000000, 0.9498695926598449413, 0.9498695926598449413, 1.000000000000000000 ) ) 
 REPRESENTATION_ITEM ( '' )  );
#42650 = DIRECTION ( 'NONE',  ( -0.000000000000000000, -1.000000000000000000, -0.000000000000000000 ) ) ;
#42651 = AXIS2_PLACEMENT_3D ( 'NONE', #21924, #11702, #10333 ) ;
#42652 = CARTESIAN_POINT ( 'NONE',  ( 13.25000000000000355, 27.74999999999998934, -3.750000000000000000 ) ) ;
#42653 = CARTESIAN_POINT ( 'NONE',  ( -45.82474114033776402, 9.083251256839144361, 6.320036396439224546 ) ) ;
#42654 = FACE_OUTER_BOUND ( 'NONE', #21777, .T. ) ;
#42655 = FILL_AREA_STYLE ('',( #15564 ) ) ;
#42656 = AXIS2_PLACEMENT_3D ( 'NONE', #13071, #7111, #17354 ) ;
#42657 = ORIENTED_EDGE ( 'NONE', *, *, #38315, .F. ) ;
#42658 = CARTESIAN_POINT ( 'NONE',  ( -150.0550000000000068, -9.827790563157499189E-16, -8.024999999999991473 ) ) ;
#42659 = VERTEX_POINT ( 'NONE', #10406 ) ;
#42660 = CARTESIAN_POINT ( 'NONE',  ( 29.00000000000000000, 42.00000000000000000, -89.00000000000000000 ) ) ;
#42661 = CARTESIAN_POINT ( 'NONE',  ( 61.74999999999998579, 31.24999999999999289, 3.750000000000000000 ) ) ;
#42662 = ORIENTED_EDGE ( 'NONE', *, *, #48485, .T. ) ;
#42663 = CIRCLE ( 'NONE', #18996, 0.5000000000000006661 ) ;
#42664 = SURFACE_SIDE_STYLE ('',( #14496 ) ) ;
#42665 = DIRECTION ( 'NONE',  ( 1.445602896647337931E-16, -1.000000000000000000, -0.000000000000000000 ) ) ;
#42666 = VECTOR ( 'NONE', #27532, 1000.000000000000114 ) ;
#42667 = B_SPLINE_CURVE_WITH_KNOTS ( 'NONE', 3,
 ( #214, #53424, #21744, #59712, #53739, #1257, #22789, #22432 ),
 .UNSPECIFIED., .F., .F.,
 ( 4, 2, 2, 4 ),
 ( 2.544316211736855218E-07, 0.002094919859796806443, 0.003142252573884622875, 0.004189585287972439308 ),
 .UNSPECIFIED. ) ;
#42668 = CARTESIAN_POINT ( 'NONE',  ( 9.058813317711337021, 123.5449999999999875, 2.943386871421375783 ) ) ;
#42669 = SURFACE_STYLE_FILL_AREA ( #10957 ) ;
#42670 = VECTOR ( 'NONE', #59945, 1000.000000000000000 ) ;
#42671 = STYLED_ITEM ( 'NONE', ( #13101 ), #9569 ) ;
#42672 = EDGE_LOOP ( 'NONE', ( #35611, #32153, #49410, #67857 ) ) ;
#42673 = PLANE ( 'NONE',  #59996 ) ;
#42674 = CARTESIAN_POINT ( 'NONE',  ( 3.094860106618431583, 118.2049999999999699, 9.525000000000000355 ) ) ;
#42675 = CARTESIAN_POINT ( 'NONE',  ( -66.50499999999998124, -6.826472737025113702, -4.959722759717900331 ) ) ;
#42676 = CARTESIAN_POINT ( 'NONE',  ( -117.4449999999999932, 0.000000000000000000, 8.024999999999991473 ) ) ;
#42677 =( GEOMETRIC_REPRESENTATION_CONTEXT ( 3 ) GLOBAL_UNCERTAINTY_ASSIGNED_CONTEXT ( ( #15167 ) ) GLOBAL_UNIT_ASSIGNED_CONTEXT ( ( #34951, #56397, #51144 ) ) REPRESENTATION_CONTEXT ( 'NONE', 'WORKASPACE' ) );
#42678 = CARTESIAN_POINT ( 'NONE',  ( -41.00000002860135595, 108.0041655605167676, -3.103651540214122040 ) ) ;
#42679 = VERTEX_POINT ( 'NONE', #42804 ) ;
#42680 = CARTESIAN_POINT ( 'NONE',  ( 9.058813317711338797, 148.9550000000000125, -2.943386871421372675 ) ) ;
#42681 = UNCERTAINTY_MEASURE_WITH_UNIT (LENGTH_MEASURE( 1.000000000000000082E-05 ), #12308, 'distance_accuracy_value', 'NONE');
#42682 = MECHANICAL_DESIGN_GEOMETRIC_PRESENTATION_REPRESENTATION (  '', ( #58401 ), #44929 ) ;
#42683 = CARTESIAN_POINT ( 'NONE',  ( -183.0769827045555473, 0.000000000000000000, 9.448017295444435248 ) ) ;
#42684 = B_SPLINE_CURVE_WITH_KNOTS ( 'NONE', 3,
 ( #39257, #810, #22018, #55399, #27253, #48785, #64584, #6861, #65954, #33936 ),
 .UNSPECIFIED., .F., .F.,
 ( 4, 2, 2, 2, 4 ),
 ( 6.776263578034402713E-20, 0.0008170663553932240456, 0.001634132710786447874, 0.002451199066179671811, 0.003268265421572895749 ),
 .UNSPECIFIED. ) ;
#42685 = CARTESIAN_POINT ( 'NONE',  ( 10.57623092156539535, 58.31681314173471975, 6.349999999999996092 ) ) ;
#42686 = EDGE_CURVE ( 'NONE', #21155, #22693, #56062, .T. ) ;
#42687 = B_SPLINE_CURVE_WITH_KNOTS ( 'NONE', 3,
 ( #43224, #1226, #44252, #22756, #6911, #55448 ),
 .UNSPECIFIED., .F., .F.,
 ( 4, 2, 4 ),
 ( 0.004189585287972438440, 0.006269578072783812440, 0.008349570857595186441 ),
 .UNSPECIFIED. ) ;
#42688 = CARTESIAN_POINT ( 'NONE',  ( 21.50000000000001066, 24.74999999999998224, -3.750000000000000000 ) ) ;
#42689 = ORIENTED_EDGE ( 'NONE', *, *, #65772, .F. ) ;
#42690 = PRESENTATION_LAYER_ASSIGNMENT (  '', '', ( #2096 ) ) ;
#42691 = CARTESIAN_POINT ( 'NONE',  ( -44.99999999999998579, 119.9999999999999716, -9.500000000000000000 ) ) ;
#42692 = PRESENTATION_STYLE_ASSIGNMENT (( #21175 ) ) ;
#42693 = CARTESIAN_POINT ( 'NONE',  ( -47.24499999999998323, -4.716976649647093289, -6.492361379858945902 ) ) ;
#42694 = EDGE_LOOP ( 'NONE', ( #31308, #39454, #11574, #46377 ) ) ;
#42695 = FACE_OUTER_BOUND ( 'NONE', #41148, .T. ) ;
#42696 = AXIS2_PLACEMENT_3D ( 'NONE', #30994, #52491, #25705 ) ;
#42697 =( NAMED_UNIT ( * ) PLANE_ANGLE_UNIT ( ) SI_UNIT ( $, .RADIAN. ) );
#42698 = EDGE_CURVE ( 'NONE', #43549, #58151, #60519, .T. ) ;
#42699 = DIRECTION ( 'NONE',  ( 0.000000000000000000, 0.000000000000000000, 1.000000000000000000 ) ) ;
#42700 = CYLINDRICAL_SURFACE ( 'NONE', #12943, 0.5000000000000004441 ) ;
#42701 = LINE ( 'NONE', #3584, #36690 ) ;
#42702 = ORIENTED_EDGE ( 'NONE', *, *, #52562, .T. ) ;
#42703 = VECTOR ( 'NONE', #18100, 1000.000000000000000 ) ;
#42704 = CARTESIAN_POINT ( 'NONE',  ( 10.00000000000000533, 50.00000000000000000, -46.00000000000000000 ) ) ;
#42705 = EDGE_CURVE ( 'NONE', #69112, #38068, #27961, .T. ) ;
#42706 = CARTESIAN_POINT ( 'NONE',  ( -99.80499999999997840, -8.437984349512085203, 5.166775262442717831E-16 ) ) ;
#42707 = ORIENTED_EDGE ( 'NONE', *, *, #31448, .T. ) ;
#42708 = CARTESIAN_POINT ( 'NONE',  ( 35.99999999999999289, 5.000000000000000000, -72.00402776293825013 ) ) ;
#42709 = CARTESIAN_POINT ( 'NONE',  ( -135.9570736234661865, 9.058813317711329915, -2.943386871421373119 ) ) ;
#42710 = VECTOR ( 'NONE', #10393, 1000.000000000000000 ) ;
#42711 = CIRCLE ( 'NONE', #52767, 17.99999999999999645 ) ;
#42712 = FILL_AREA_STYLE ('',( #1054 ) ) ;
#42713 = CARTESIAN_POINT ( 'NONE',  ( -8.102448949553179958, 149.4949999999999761, 5.886773742842747126 ) ) ;
#42714 = CARTESIAN_POINT ( 'NONE',  ( -66.05707362346618083, 0.000000000000000000, 9.524999999999991473 ) ) ;
#42715 = VECTOR ( 'NONE', #14466, 1000.000000000000000 ) ;
#42716 = CARTESIAN_POINT ( 'NONE',  ( -80.69292637653380496, 10.01517768586948698, -1.839758294383808966E-15 ) ) ;
#42717 = ORIENTED_EDGE ( 'NONE', *, *, #829, .F. ) ;
#42718 = LINE ( 'NONE', #64116, #22631 ) ;
#42719 = DIRECTION ( 'NONE',  ( 0.000000000000000000, 0.000000000000000000, -1.000000000000000000 ) ) ;
#42720 = PRESENTATION_STYLE_ASSIGNMENT (( #42381 ) ) ;
#42721 = VECTOR ( 'NONE', #55558, 1000.000000000000000 ) ;
#42722 = EDGE_CURVE ( 'NONE', #24855, #61901, #46001, .T. ) ;
#42723 = CARTESIAN_POINT ( 'NONE',  ( -113.4549999999999841, 7.632228543268599452, -2.479861379858951942 ) ) ;
#42724 = CARTESIAN_POINT ( 'NONE',  ( -3.094860106618434248, 122.7949999999999875, 9.525000000000000355 ) ) ;
#42725 = CARTESIAN_POINT ( 'NONE',  ( -119.6950000000000074, -8.437984349512085203, 5.166775262442717831E-16 ) ) ;
#42726 = COLOUR_RGB ( '', 0.66274510, 0.83137255, 0.94901961) ;
#42727 = FACE_OUTER_BOUND ( 'NONE', #16712, .T. ) ;
#42728 = CIRCLE ( 'NONE', #23582, 0.4999999999999994449 ) ;
#42729 = B_SPLINE_CURVE_WITH_KNOTS ( 'NONE', 3,
 ( #61461, #13280, #45695, #34736, #13635, #56190, #29469, #50940, #49563, #2697, #24190, #1294, #17569, #39034, #12239, #55153, #6983, #28406, #30145, #68167, #3383, #62167, #67813, #36544, #68508, #8384, #68865, #52681, #47081, #13998 ),
 .UNSPECIFIED., .F., .F.,
 ( 4, 2, 2, 2, 2, 2, 2, 2, 2, 2, 2, 2, 2, 2, 4 ),
 ( 0.000000000000000000, 0.001317596576228367410, 0.002635193152456734821, 0.005270386304913469641, 0.006587982881141837485, 0.007905579457370203594, 0.009223176033598571438, 0.01054077260982693928, 0.01185836918605530713, 0.01317596576228367497, 0.01449356233851204108, 0.01581115891474040719, 0.01712875549096877503, 0.01844635206719714288, 0.02108154521965387856 ),
 .UNSPECIFIED. ) ;
#42730 = CARTESIAN_POINT ( 'NONE',  ( -117.4429263765338050, -1.166476076187852838E-15, -9.524999999999991473 ) ) ;
#42731 = EDGE_LOOP ( 'NONE', ( #34134, #46902, #15917, #22932 ) ) ;
#42732 = MECHANICAL_DESIGN_GEOMETRIC_PRESENTATION_REPRESENTATION (  '', ( #5598 ), #26915 ) ;
#42733 = CARTESIAN_POINT ( 'NONE',  ( -165.4429263765337907, -1.166476076187852838E-15, -9.524999999999991473 ) ) ;
#42734 = CARTESIAN_POINT ( 'NONE',  ( -174.7449999999999761, 4.716976649647094177, 6.492361379858945902 ) ) ;
#42735 = MECHANICAL_DESIGN_GEOMETRIC_PRESENTATION_REPRESENTATION (  '', ( #3311 ), #5545 ) ;
#42736 = DIRECTION ( 'NONE',  ( 0.000000000000000000, 0.000000000000000000, 1.000000000000000000 ) ) ;
#42737 = AXIS2_PLACEMENT_3D ( 'NONE', #33415, #34105, #17930 ) ;
#42738 = DIRECTION ( 'NONE',  ( 0.000000000000000000, 0.000000000000000000, 1.000000000000000000 ) ) ;
#42739 =( NAMED_UNIT ( * ) SI_UNIT ( $, .STERADIAN. ) SOLID_ANGLE_UNIT ( ) );
#42740 = EDGE_LOOP ( 'NONE', ( #16307, #15969, #55666, #52080 ) ) ;
#42741 = CARTESIAN_POINT ( 'NONE',  ( -76.34292637653379643, -9.058813317711329915, 2.943386871421371787 ) ) ;
#42742 = EDGE_CURVE ( 'NONE', #49636, #3770, #3184, .T. ) ;
#42743 = CONTEXT_DEPENDENT_SHAPE_REPRESENTATION ( #29403, #17757 ) ;
#42744 = STYLED_ITEM ( 'NONE', ( #49271 ), #16335 ) ;
#42745 = DIRECTION ( 'NONE',  ( -1.189524669241239115E-16, -1.000000000000000000, -0.000000000000000000 ) ) ;
#42746 = SURFACE_SIDE_STYLE ('',( #47692 ) ) ;
#42747 = PRESENTATION_LAYER_ASSIGNMENT (  '', '', ( #15746 ) ) ;
#42748 = CARTESIAN_POINT ( 'NONE',  ( -47.75499999999999545, 4.716976649647091513, -6.492361379858946790 ) ) ;
#42749 = CARTESIAN_POINT ( 'NONE',  ( 66.24999999999998579, 34.24999999999999289, -3.750000000000000000 ) ) ;
#42750 = CARTESIAN_POINT ( 'NONE',  ( -177.3549999999999898, -4.716976649647093289, -6.492361379858945902 ) ) ;
#42751 = ORIENTED_EDGE ( 'NONE', *, *, #13090, .F. ) ;
#42752 = DIRECTION ( 'NONE',  ( 0.000000000000000000, 0.000000000000000000, -1.000000000000000000 ) ) ;
#42753 = SURFACE_STYLE_USAGE ( .BOTH. , #32470 ) ;
#42754 = PRESENTATION_STYLE_ASSIGNMENT (( #64843 ) ) ;
#42755 = CARTESIAN_POINT ( 'NONE',  ( 52.75000000000000000, 24.99999999999998579, -3.750000000000000000 ) ) ;
#42756 = VECTOR ( 'NONE', #62620, 1000.000000000000000 ) ;
#42757 = DIRECTION ( 'NONE',  ( 0.000000000000000000, -1.000000000000000000, 0.000000000000000000 ) ) ;
#42758 = CARTESIAN_POINT ( 'NONE',  ( -6.826472737025120807, 145.5070736234661410, -4.959722759717907437 ) ) ;
#42759 =( BOUNDED_CURVE ( )  B_SPLINE_CURVE ( 2, ( #36448, #57869, #69113, #5068, #16361, #25482, #37836, #9330, #20919, #31100, #4014 ),
 .UNSPECIFIED., .F., .F. ) 
 B_SPLINE_CURVE_WITH_KNOTS ( ( 3, 2, 2, 2, 2, 3 ),
 ( 0.5869565217391166101, 0.5891304347825948584, 0.5913043478260731067, 0.5934782608695512440, 0.5956521739130294923, 0.5978260869565077407 ),
 .UNSPECIFIED. ) 
 CURVE ( )  GEOMETRIC_REPRESENTATION_ITEM ( )  RATIONAL_B_SPLINE_CURVE ( ( 1.000000000000312417, 0.9510565162948411144, 1.000000000000000000, 0.9510565162951535312, 1.000000000000000000, 0.9510565162951535312, 1.000000000000000000, 0.9510565162951535312, 1.000000000000000000, 0.9510565162954685015, 0.9999999999996850297 ) ) 
 REPRESENTATION_ITEM ( '' )  );
#42760 = ORIENTED_EDGE ( 'NONE', *, *, #10360, .T. ) ;
#42761 = CONICAL_SURFACE ( 'NONE', #2211, 4.000000000000000000, 0.7853981633974482790 ) ;
#42762 = CARTESIAN_POINT ( 'NONE',  ( -31.24938216804229185, -8.559564029643235372, -0.5720419862225104568 ) ) ;
#42763 = CARTESIAN_POINT ( 'NONE',  ( -92.60499999999998977, 6.826472737025113702, -4.959722759717902107 ) ) ;
#42764 = UNCERTAINTY_MEASURE_WITH_UNIT (LENGTH_MEASURE( 1.000000000000000082E-05 ), #6882, 'distance_accuracy_value', 'NONE');
#42765 = SURFACE_STYLE_FILL_AREA ( #67 ) ;
#42766 = ORIENTED_EDGE ( 'NONE', *, *, #5956, .F. ) ;
#42767 = FILL_AREA_STYLE ('',( #36790 ) ) ;
#42768 = DIRECTION ( 'NONE',  ( -1.000000000000000000, 0.000000000000000000, 0.000000000000000000 ) ) ;
#42769 = DIRECTION ( 'NONE',  ( 1.000000000000000000, -0.000000000000000000, 0.000000000000000000 ) ) ;
#42770 = FACE_OUTER_BOUND ( 'NONE', #24179, .T. ) ;
#42771 = EDGE_CURVE ( 'NONE', #14819, #3572, #59413, .T. ) ;
#42772 =( GEOMETRIC_REPRESENTATION_CONTEXT ( 3 ) GLOBAL_UNCERTAINTY_ASSIGNED_CONTEXT ( ( #15330 ) ) GLOBAL_UNIT_ASSIGNED_CONTEXT ( ( #37642, #45239, #32299 ) ) REPRESENTATION_CONTEXT ( 'NONE', 'WORKASPACE' ) );
#42773 = CARTESIAN_POINT ( 'NONE',  ( 0.9126302363882010660, -2.499999999999998224, 9.000000000000003553 ) ) ;
#42774 = VERTEX_POINT ( 'NONE', #32514 ) ;
#42775 = CARTESIAN_POINT ( 'NONE',  ( 17.15973193263811680, -3.000000000000000000, -2.000000000000000000 ) ) ;
#42776 = CARTESIAN_POINT ( 'NONE',  ( -69.44499999999999318, 0.000000000000000000, 8.024999999999991473 ) ) ;
#42778 = ORIENTED_EDGE ( 'NONE', *, *, #63905, .T. ) ;
#42777 =( GEOMETRIC_REPRESENTATION_CONTEXT ( 3 ) GLOBAL_UNCERTAINTY_ASSIGNED_CONTEXT ( ( #10969 ) ) GLOBAL_UNIT_ASSIGNED_CONTEXT ( ( #60412, #17550, #12928 ) ) REPRESENTATION_CONTEXT ( 'NONE', 'WORKASPACE' ) );
#42779 =( LENGTH_UNIT ( ) NAMED_UNIT ( * ) SI_UNIT ( .MILLI., .METRE. ) );
#42780 = SURFACE_SIDE_STYLE ('',( #5087 ) ) ;
#42781 = AXIS2_PLACEMENT_3D ( 'NONE', #19755, #46898, #52150 ) ;
#42782 = ORIENTED_EDGE ( 'NONE', *, *, #23092, .F. ) ;
#42783 = DIRECTION ( 'NONE',  ( 1.000000000000000000, 0.000000000000000000, 0.000000000000000000 ) ) ;
#42784 = SURFACE_STYLE_USAGE ( .BOTH. , #68100 ) ;
#42785 = AXIS2_PLACEMENT_3D ( 'NONE', #19847, #30375, #46644 ) ;
#42787 = EDGE_CURVE ( 'NONE', #16782, #49325, #59243, .T. ) ;
#42786 = SURFACE_SIDE_STYLE ('',( #32178 ) ) ;
#42788 = ORIENTED_EDGE ( 'NONE', *, *, #21851, .F. ) ;
#42789 = FACE_OUTER_BOUND ( 'NONE', #37928, .T. ) ;
#42790 = EDGE_CURVE ( 'NONE', #60536, #33822, #11066, .T. ) ;
#42791 = AXIS2_PLACEMENT_3D ( 'NONE', #4518, #10858, #59355 ) ;
#42792 = ORIENTED_EDGE ( 'NONE', *, *, #30720, .T. ) ;
#42793 =( LENGTH_UNIT ( ) NAMED_UNIT ( * ) SI_UNIT ( .MILLI., .METRE. ) );
#42794 = CARTESIAN_POINT ( 'NONE',  ( 35.99999999999999289, 5.000000000000000000, 24.00402776293825369 ) ) ;
#42796 = AXIS2_PLACEMENT_3D ( 'NONE', #38305, #59707, #38999 ) ;
#42795 = CARTESIAN_POINT ( 'NONE',  ( 27.00000000000001776, -60.04052944165106709, 35.50000000000000000 ) ) ;
#42797 = CARTESIAN_POINT ( 'NONE',  ( -155.6070736234661922, -8.102448949553172852, 5.886773742842742685 ) ) ;
#42798 = EDGE_CURVE ( 'NONE', #31700, #61072, #11772, .T. ) ;
#42799 = COLOUR_RGB ( '', 0.31764706, 0.68627451, 0.89019608) ;
#42800 = CARTESIAN_POINT ( 'NONE',  ( -10.01517768586949408, 122.1949999999999648, -6.132527647946036459E-16 ) ) ;
#42801 = CARTESIAN_POINT ( 'NONE',  ( -98.45707362346617231, -9.058813317711329915, 2.943386871421371787 ) ) ;
#42802 = AXIS2_PLACEMENT_3D ( 'NONE', #46725, #68135, #58256 ) ;
#42803 = EDGE_CURVE ( 'NONE', #54767, #34141, #53802, .T. ) ;
#42804 = CARTESIAN_POINT ( 'NONE',  ( 7.000000000000017764, 42.74314482547740113, 27.71473342867655987 ) ) ;
#42805 = ORIENTED_EDGE ( 'NONE', *, *, #18869, .T. ) ;
#42806 = AXIS2_PLACEMENT_3D ( 'NONE', #9388, #31152, #35059 ) ;
#42807 = FACE_OUTER_BOUND ( 'NONE', #4129, .T. ) ;
#42808 = CARTESIAN_POINT ( 'NONE',  ( -9.827790563157511022E-16, 131.5570736234661524, 8.025000000000000355 ) ) ;
#42809 = EDGE_CURVE ( 'NONE', #21436, #37680, #62780, .T. ) ;
#42810 = CARTESIAN_POINT ( 'NONE',  ( -138.6550000000000011, -7.632228543268600340, -2.479861379858950166 ) ) ;
#42811 = PRESENTATION_STYLE_ASSIGNMENT (( #32199 ) ) ;
#42812 = CARTESIAN_POINT ( 'NONE',  ( 48.75000000000000000, 22.24999999999998579, -3.750000000000000000 ) ) ;
#42813 = CYLINDRICAL_SURFACE ( 'NONE', #43310, 0.2500000000000002220 ) ;
#42814 = CARTESIAN_POINT ( 'NONE',  ( -149.8449999999999989, -7.632228543268599452, 2.479861379858951054 ) ) ;
#42815 = CARTESIAN_POINT ( 'NONE',  ( -140.8449999999999989, -7.632228543268599452, 2.479861379858951054 ) ) ;
#42816 = MECHANICAL_DESIGN_GEOMETRIC_PRESENTATION_REPRESENTATION (  '', ( #48425 ), #16922 ) ;
#42817 = ORIENTED_EDGE ( 'NONE', *, *, #33928, .T. ) ;
#42818 = DIRECTION ( 'NONE',  ( 0.000000000000000000, 1.000000000000000000, 0.000000000000000000 ) ) ;
#42819 = VECTOR ( 'NONE', #25399, 1000.000000000000000 ) ;
#42820 = CARTESIAN_POINT ( 'NONE',  ( -57.20499999999996987, -2.607480562269071545, -8.024999999999991473 ) ) ;
#42821 = CARTESIAN_POINT ( 'NONE',  ( -20.12916642283592950, 110.4999999999999858, -10.05319148936170137 ) ) ;
#42822 = DIRECTION ( 'NONE',  ( 0.000000000000000000, 1.000000000000000000, -0.000000000000000000 ) ) ;
#42823 = PRESENTATION_LAYER_ASSIGNMENT (  '', '', ( #6801 ) ) ;
#42824 =( LENGTH_UNIT ( ) NAMED_UNIT ( * ) SI_UNIT ( .MILLI., .METRE. ) );
#42825 = DIRECTION ( 'NONE',  ( 0.000000000000000000, 0.6691306063588591257, -0.7431448254773933559 ) ) ;
#42826 = VECTOR ( 'NONE', #18563, 1000.000000000000000 ) ;
#42827 = B_SPLINE_CURVE_WITH_KNOTS ( 'NONE', 3,
 ( #58632, #15064, #62850, #9771, #53367, #26264, #63562, #47435 ),
 .UNSPECIFIED., .F., .F.,
 ( 4, 2, 2, 4 ),
 ( 0.005458618329390014547, 0.006805794425120373359, 0.008152970520850733038, 0.01084732271231145413 ),
 .UNSPECIFIED. ) ;
#42828 = DIRECTION ( 'NONE',  ( 1.000000000000000000, 0.000000000000000000, 0.000000000000000000 ) ) ;
#42829 = DIRECTION ( 'NONE',  ( -1.000000000000000000, 0.000000000000000000, 0.000000000000000000 ) ) ;
#42830 = VECTOR ( 'NONE', #6778, 1000.000000000000000 ) ;
#42831 = DIRECTION ( 'NONE',  ( 1.000000000000000000, 0.000000000000000000, -1.300977106640434891E-16 ) ) ;
#42832 = DIRECTION ( 'NONE',  ( -1.000000000000000000, 0.000000000000000000, 0.000000000000000000 ) ) ;
#42833 = LINE ( 'NONE', #63875, #50841 ) ;
#42834 = ORIENTED_EDGE ( 'NONE', *, *, #12392, .F. ) ;
#42835 = AXIS2_PLACEMENT_3D ( 'NONE', #60329, #33601, #6867 ) ;
#42836 = CARTESIAN_POINT ( 'NONE',  ( -8.437984349512095861, 118.8070736234661666, -5.166775262442723748E-16 ) ) ;
#42837 = EDGE_LOOP ( 'NONE', ( #24510, #23692, #8495, #4477, #62919, #43562, #53961, #5460, #5149, #63027, #28607, #50123, #26661 ) ) ;
#42838 =( NAMED_UNIT ( * ) PLANE_ANGLE_UNIT ( ) SI_UNIT ( $, .RADIAN. ) );
#42839 =( LENGTH_UNIT ( ) NAMED_UNIT ( * ) SI_UNIT ( .MILLI., .METRE. ) );
#42840 = AXIS2_PLACEMENT_3D ( 'NONE', #59977, #7217, #49786 ) ;
#42841 = SURFACE_STYLE_USAGE ( .BOTH. , #38248 ) ;
#42842 = ORIENTED_EDGE ( 'NONE', *, *, #60494, .T. ) ;
#42843 = ORIENTED_EDGE ( 'NONE', *, *, #25453, .T. ) ;
#42844 = DIRECTION ( 'NONE',  ( -0.000000000000000000, -0.000000000000000000, -1.000000000000000000 ) ) ;
#42845 = DIRECTION ( 'NONE',  ( 0.000000000000000000, 0.000000000000000000, -1.000000000000000000 ) ) ;
#42846 = SURFACE_STYLE_USAGE ( .BOTH. , #47796 ) ;
#42847 = VERTEX_POINT ( 'NONE', #18093 ) ;
#42848 = CARTESIAN_POINT ( 'NONE',  ( -3.094860106618434248, 117.9049999999999727, 9.525000000000000355 ) ) ;
#42849 = DIRECTION ( 'NONE',  ( 0.000000000000000000, 0.000000000000000000, 1.000000000000000000 ) ) ;
#42850 = ORIENTED_EDGE ( 'NONE', *, *, #28148, .T. ) ;
#42851 = ADVANCED_FACE ( 'NONE', ( #12448 ), #12805, .F. ) ;
#42852 = PRESENTATION_LAYER_ASSIGNMENT (  '', '', ( #2255 ) ) ;
#42853 = CYLINDRICAL_SURFACE ( 'NONE', #21572, 5.000000000000004441 ) ;
#42854 = CARTESIAN_POINT ( 'NONE',  ( -97.49499999999999034, 6.826472737025113702, -4.959722759717902107 ) ) ;
#42855 = EDGE_LOOP ( 'NONE', ( #52116, #8017, #33446, #21226, #294 ) ) ;
#42856 = ADVANCED_FACE ( 'NONE', ( #39581 ), #39933, .F. ) ;
#42857 = CARTESIAN_POINT ( 'NONE',  ( 7.398009814270800177, 153.1301383316707359, 3.525480039724990355 ) ) ;
#42858 = DIRECTION ( 'NONE',  ( -1.000000000000000000, 0.000000000000000000, 0.000000000000000000 ) ) ;
#42859 = STYLED_ITEM ( 'NONE', ( #61037 ), #45582 ) ;
#42860 =( GEOMETRIC_REPRESENTATION_CONTEXT ( 3 ) GLOBAL_UNCERTAINTY_ASSIGNED_CONTEXT ( ( #29929 ) ) GLOBAL_UNIT_ASSIGNED_CONTEXT ( ( #47582, #26723, #26398 ) ) REPRESENTATION_CONTEXT ( 'NONE', 'WORKASPACE' ) );
#42861 = ORIENTED_EDGE ( 'NONE', *, *, #50830, .F. ) ;
#42862 = CARTESIAN_POINT ( 'NONE',  ( 2.607480562269071989, 151.5929263765337680, 8.025000000000002132 ) ) ;
#42863 =( NAMED_UNIT ( * ) PLANE_ANGLE_UNIT ( ) SI_UNIT ( $, .RADIAN. ) );
#42864 = EDGE_CURVE ( 'NONE', #37240, #43509, #35532, .T. ) ;
#42865 = COLOUR_RGB ( '', 0.40784314, 0.44705882, 0.49803922) ;
#42866 = FILL_AREA_STYLE_COLOUR ( '', #773 ) ;
#42867 = AXIS2_PLACEMENT_3D ( 'NONE', #26422, #15909, #69014 ) ;
#42868 = LINE ( 'NONE', #30864, #38651 ) ;
#42869 = EDGE_CURVE ( 'NONE', #11358, #10407, #40425, .T. ) ;
#42870 = ORIENTED_EDGE ( 'NONE', *, *, #17548, .F. ) ;
#42871 = CARTESIAN_POINT ( 'NONE',  ( -195.0000000000000000, 1.166476076187852838E-15, -9.524999999999991473 ) ) ;
#42872 = CARTESIAN_POINT ( 'NONE',  ( 34.99999999999992895, 112.9999999999999858, 7.000000000000000000 ) ) ;
#42873 = FILL_AREA_STYLE_COLOUR ( '', #49059 ) ;
#42874 = AXIS2_PLACEMENT_3D ( 'NONE', #46996, #15652, #52598 ) ;
#42875 = FACE_OUTER_BOUND ( 'NONE', #21792, .T. ) ;
#42876 = AXIS2_PLACEMENT_3D ( 'NONE', #11099, #15390, #5818 ) ;
#42877 = CARTESIAN_POINT ( 'NONE',  ( 12.50000000000000533, 28.24999999999998224, -3.750000000000000000 ) ) ;
#42878 = ADVANCED_FACE ( 'NONE', ( #40256 ), #40071, .T. ) ;
#42879 = CARTESIAN_POINT ( 'NONE',  ( -59.90707362346617515, -3.094860106618429807, 9.524999999999991473 ) ) ;
#42880 = DIRECTION ( 'NONE',  ( -1.156482317317873451E-16, 1.000000000000000000, 0.000000000000000000 ) ) ;
#42881 = CARTESIAN_POINT ( 'NONE',  ( -5.237322049151774905, 153.2151860177439460, -6.367445604021556349 ) ) ;
#42882 = ORIENTED_EDGE ( 'NONE', *, *, #5445, .F. ) ;
#42883 = VERTEX_POINT ( 'NONE', #4299 ) ;
#42884 = DIRECTION ( 'NONE',  ( 0.000000000000000000, 1.000000000000000000, -0.000000000000000000 ) ) ;
#42885 = CARTESIAN_POINT ( 'NONE',  ( 93.00000000000000000, 14.00000000000000000, 0.000000000000000000 ) ) ;
#42886 = CARTESIAN_POINT ( 'NONE',  ( -170.9070736234663173, -3.094860106616059703, 9.525000000001714540 ) ) ;
#42887 = CYLINDRICAL_SURFACE ( 'NONE', #23112, 0.2500000000000002220 ) ;
#42888 = ORIENTED_EDGE ( 'NONE', *, *, #20348, .F. ) ;
#42889 = CARTESIAN_POINT ( 'NONE',  ( -154.3429263765337964, -9.058813317711329915, 2.943386871421371787 ) ) ;
#42890 = CARTESIAN_POINT ( 'NONE',  ( -168.2050000000000125, -2.607480562269071545, -8.024999999999991473 ) ) ;
#42891 = LINE ( 'NONE', #42531, #8258 ) ;
#42892 = FACE_OUTER_BOUND ( 'NONE', #64710, .T. ) ;
#42893 = CARTESIAN_POINT ( 'NONE',  ( -49.70707362346615810, -3.094860106618431139, -9.524999999999991473 ) ) ;
#42894 = CARTESIAN_POINT ( 'NONE',  ( -170.6949999999999932, -8.437984349512086979, 5.166775262442717831E-16 ) ) ;
#42895 =( GEOMETRIC_REPRESENTATION_CONTEXT ( 3 ) GLOBAL_UNCERTAINTY_ASSIGNED_CONTEXT ( ( #64318 ) ) GLOBAL_UNIT_ASSIGNED_CONTEXT ( ( #35349, #56804, #61019 ) ) REPRESENTATION_CONTEXT ( 'NONE', 'WORKASPACE' ) );
#42896 = ORIENTED_EDGE ( 'NONE', *, *, #66217, .T. ) ;
#42897 = FACE_OUTER_BOUND ( 'NONE', #60444, .T. ) ;
#42898 = DIRECTION ( 'NONE',  ( 0.000000000000000000, 0.000000000000000000, 1.000000000000000000 ) ) ;
#42899 = CARTESIAN_POINT ( 'NONE',  ( -82.25499999999998124, -4.716976649647092401, 6.492361379858946790 ) ) ;
#42900 = FACE_OUTER_BOUND ( 'NONE', #30689, .T. ) ;
#42901 = CARTESIAN_POINT ( 'NONE',  ( 60.00000000000000000, 149.4999999999999716, -10.00000000000000000 ) ) ;
#42902 = MECHANICAL_DESIGN_GEOMETRIC_PRESENTATION_REPRESENTATION (  '', ( #51854 ), #68728 ) ;
#42903 = CARTESIAN_POINT ( 'NONE',  ( -75.00000000000000000, 35.50862325381056905, -9.500000000000000000 ) ) ;
#42904 = CARTESIAN_POINT ( 'NONE',  ( -83.39499999999998181, -6.826472737025113702, -4.959722759717900331 ) ) ;
#42905 = CARTESIAN_POINT ( 'NONE',  ( -8.102448949553181734, 132.6050000000000182, 5.886773742842747126 ) ) ;
#42906 = FILL_AREA_STYLE_COLOUR ( '', #34236 ) ;
#42907 = CARTESIAN_POINT ( 'NONE',  ( -170.5429263765338135, 9.058813317711329915, 2.943386871421369566 ) ) ;
#42908 =( GEOMETRIC_REPRESENTATION_CONTEXT ( 3 ) GLOBAL_UNCERTAINTY_ASSIGNED_CONTEXT ( ( #10849 ) ) GLOBAL_UNIT_ASSIGNED_CONTEXT ( ( #35251, #13431, #39513 ) ) REPRESENTATION_CONTEXT ( 'NONE', 'WORKASPACE' ) );
#42909 = EDGE_CURVE ( 'NONE', #55165, #30878, #9024, .T. ) ;
#42910 = CARTESIAN_POINT ( 'NONE',  ( -14.98999599679679662, 118.4999999999999716, 9.500000000000000000 ) ) ;
#42911 = ORIENTED_EDGE ( 'NONE', *, *, #37222, .T. ) ;
#42912 = DIRECTION ( 'NONE',  ( -1.000000000000000000, 0.000000000000000000, 0.000000000000000000 ) ) ;
#42913 = AXIS2_PLACEMENT_3D ( 'NONE', #6067, #69072, #63765 ) ;
#42914 = SURFACE_STYLE_USAGE ( .BOTH. , #25718 ) ;
#42915 = FILL_AREA_STYLE_COLOUR ( '', #41651 ) ;
#42916 = PRESENTATION_LAYER_ASSIGNMENT (  '', '', ( #17036 ) ) ;
#42917 = CARTESIAN_POINT ( 'NONE',  ( 45.00000000000000000, 10.69371294336137979, -6.585786437626905077 ) ) ;
#42918 = VERTEX_POINT ( 'NONE', #35320 ) ;
#42919 = ORIENTED_EDGE ( 'NONE', *, *, #66827, .F. ) ;
#42920 = LINE ( 'NONE', #16854, #20610 ) ;
#42921 = CIRCLE ( 'NONE', #24873, 5.000000000000004441 ) ;
#42922 = CARTESIAN_POINT ( 'NONE',  ( -9.827790563157511022E-16, 130.4429263765338192, 8.025000000000000355 ) ) ;
#42923 = TOROIDAL_SURFACE ( 'NONE', #15995, 26.49999999999999645, 0.5000000000000000000 ) ;
#42924 = LINE ( 'NONE', #31966, #45025 ) ;
#42925 = STYLED_ITEM ( 'NONE', ( #7559 ), #52940 ) ;
#42926 =( NAMED_UNIT ( * ) SI_UNIT ( $, .STERADIAN. ) SOLID_ANGLE_UNIT ( ) );
#42927 = CARTESIAN_POINT ( 'NONE',  ( -69.50707362346615525, 8.102448949553176405, 5.886773742842740909 ) ) ;
#42928 = ORIENTED_EDGE ( 'NONE', *, *, #49802, .F. ) ;
#42929 = CARTESIAN_POINT ( 'NONE',  ( -122.3049999999999926, 8.437984349512086979, -1.550032578732815448E-15 ) ) ;
#42931 = ADVANCED_FACE ( 'NONE', ( #67668 ), #9283, .F. ) ;
#42930 = ORIENTED_EDGE ( 'NONE', *, *, #39228, .T. ) ;
#42932 = LINE ( 'NONE', #5563, #65739 ) ;
#42933 = CIRCLE ( 'NONE', #66482, 10.00000000000000000 ) ;
#42934 = EDGE_CURVE ( 'NONE', #149, #12986, #63435, .T. ) ;
#42935 = ORIENTED_EDGE ( 'NONE', *, *, #8831, .F. ) ;
#42936 = DIRECTION ( 'NONE',  ( -1.239088197126290817E-16, 0.000000000000000000, -1.000000000000000000 ) ) ;
#42937 = ORIENTED_EDGE ( 'NONE', *, *, #8602, .T. ) ;
#42938 = CARTESIAN_POINT ( 'NONE',  ( 5.598654528085809545, 151.1449999999999818, -7.705886871421373741 ) ) ;
#42939 = EDGE_CURVE ( 'NONE', #9250, #61196, #14547, .T. ) ;
#42940 = VERTEX_POINT ( 'NONE', #9642 ) ;
#42941 =( GEOMETRIC_REPRESENTATION_CONTEXT ( 3 ) GLOBAL_UNCERTAINTY_ASSIGNED_CONTEXT ( ( #16698 ) ) GLOBAL_UNIT_ASSIGNED_CONTEXT ( ( #940, #33391, #54820 ) ) REPRESENTATION_CONTEXT ( 'NONE', 'WORKASPACE' ) );
#42942 = DIRECTION ( 'NONE',  ( 1.000000000000000000, 0.000000000000000000, 0.000000000000000000 ) ) ;
#42943 = FILL_AREA_STYLE_COLOUR ( '', #47437 ) ;
#42944 = DIRECTION ( 'NONE',  ( 1.000000000000000000, -0.000000000000000000, -1.300977106640434891E-16 ) ) ;
#42945 = CARTESIAN_POINT ( 'NONE',  ( 15.48999599679679662, 118.4999999999999716, -9.500000000000000000 ) ) ;
#42946 = ORIENTED_EDGE ( 'NONE', *, *, #42406, .F. ) ;
#42947 = CARTESIAN_POINT ( 'NONE',  ( -9.827790563157511022E-16, 130.4429263765338192, 8.025000000000000355 ) ) ;
#42948 = FILL_AREA_STYLE_COLOUR ( '', #40027 ) ;
#42949 = VECTOR ( 'NONE', #57079, 1000.000000000000000 ) ;
#42950 = CARTESIAN_POINT ( 'NONE',  ( 5.196152422706636465, -9.000000000000005329, 1.392304845413258274 ) ) ;
#42951 = ORIENTED_EDGE ( 'NONE', *, *, #36353, .T. ) ;
#42952 = DIRECTION ( 'NONE',  ( 0.000000000000000000, -1.000000000000000000, 0.000000000000000000 ) ) ;
#42953 = ADVANCED_FACE ( 'NONE', ( #68365 ), #40610, .T. ) ;
#42954 = EDGE_LOOP ( 'NONE', ( #60801, #17270, #28129, #53312 ) ) ;
#42955 = CYLINDRICAL_SURFACE ( 'NONE', #62957, 1.000000000000000888 ) ;
#42956 = CARTESIAN_POINT ( 'NONE',  ( -44.50000000000000000, 99.99999999999992895, 3.500000000000000000 ) ) ;
#42957 = DIRECTION ( 'NONE',  ( 0.000000000000000000, 0.000000000000000000, -1.000000000000000000 ) ) ;
#42959 = CARTESIAN_POINT ( 'NONE',  ( -142.8550000000000182, 4.716976649647094177, 6.492361379858945902 ) ) ;
#42958 = COLOUR_RGB ( '', 0.08235294, 0.09019608, 0.10196078) ;
#42960 = CARTESIAN_POINT ( 'NONE',  ( 34.99999999999992895, 112.9999999999999858, 7.500000000000000000 ) ) ;
#42961 = DIRECTION ( 'NONE',  ( -1.000000000000000000, 0.000000000000000000, 0.000000000000000000 ) ) ;
#42962 =( BOUNDED_CURVE ( )  B_SPLINE_CURVE ( 2, ( #9988, #4687, #68737, #21204, #52568, #63778, #15624, #10334, #31767, #4311, #42730 ),
 .UNSPECIFIED., .F., .F. ) 
 B_SPLINE_CURVE_WITH_KNOTS ( ( 3, 2, 2, 2, 2, 3 ),
 ( 0.4782608695652060260, 0.4804347826086842188, 0.4826086956521624116, 0.4847826086956406044, 0.4869565217391188527, 0.4891304347825970456 ),
 .UNSPECIFIED. ) 
 CURVE ( )  GEOMETRIC_REPRESENTATION_ITEM ( )  RATIONAL_B_SPLINE_CURVE ( ( 1.000000000000256239, 0.9510565162948972917, 1.000000000000000000, 0.9510565162951535312, 1.000000000000000000, 0.9510565162951535312, 1.000000000000000000, 0.9510565162951535312, 1.000000000000000000, 0.9510565162954159879, 0.9999999999997375433 ) ) 
 REPRESENTATION_ITEM ( '' )  );
#42963 = COLOUR_RGB ( '', 0.66274510, 0.83137255, 0.94901961) ;
#42964 = VECTOR ( 'NONE', #50815, 1000.000000000000000 ) ;
#42965 = DIRECTION ( 'NONE',  ( -1.189524669241239115E-16, -1.000000000000000000, 0.000000000000000000 ) ) ;
#42966 = EDGE_CURVE ( 'NONE', #31846, #62231, #10084, .T. ) ;
#42967 = VERTEX_POINT ( 'NONE', #24730 ) ;
#42968 = CIRCLE ( 'NONE', #20422, 111.0000000000000142 ) ;
#42969 = ORIENTED_EDGE ( 'NONE', *, *, #61057, .F. ) ;
#42970 = CARTESIAN_POINT ( 'NONE',  ( 23.50000000000001776, 24.55989583710066171, 27.18999999999999062 ) ) ;
#42971 = CARTESIAN_POINT ( 'NONE',  ( 3.749999999999999556, 33.74999999999998579, 4.000000000000000000 ) ) ;
#42972 = CARTESIAN_POINT ( 'NONE',  ( -59.90499999999997982, 2.607480562269068880, -8.024999999999993250 ) ) ;
#42973 = VERTEX_POINT ( 'NONE', #19105 ) ;
#42974 = DIRECTION ( 'NONE',  ( 0.000000000000000000, 1.000000000000000000, -0.000000000000000000 ) ) ;
#42975 = SURFACE_STYLE_USAGE ( .BOTH. , #59096 ) ;
#42976 = DIRECTION ( 'NONE',  ( 0.000000000000000000, 0.000000000000000000, -1.000000000000000000 ) ) ;
#42977 = PRESENTATION_LAYER_ASSIGNMENT (  '', '', ( #64245 ) ) ;
#42978 = AXIS2_PLACEMENT_3D ( 'NONE', #66241, #21006, #22654 ) ;
#42979 = DIRECTION ( 'NONE',  ( 0.000000000000000000, 0.000000000000000000, 1.000000000000000000 ) ) ;
#42980 = CARTESIAN_POINT ( 'NONE',  ( -111.4429263765338050, -1.166476076187852838E-15, -9.524999999999991473 ) ) ;
#42981 = VERTEX_POINT ( 'NONE', #41661 ) ;
#42982 = CARTESIAN_POINT ( 'NONE',  ( 3.999798566743338668, 49.09558629977726696, -7.322456175549363344 ) ) ;
#42983 = SURFACE_STYLE_USAGE ( .BOTH. , #58767 ) ;
#42984 = CIRCLE ( 'NONE', #56373, 0.2500000000000002220 ) ;
#42985 = FILL_AREA_STYLE_COLOUR ( '', #40451 ) ;
#42986 = CARTESIAN_POINT ( 'NONE',  ( -107.5449999999999875, -7.632228543268600340, -2.479861379858950166 ) ) ;
#42987 = CARTESIAN_POINT ( 'NONE',  ( -3.094860106618432471, 154.5949999999999704, -9.525000000000000355 ) ) ;
#42988 = CARTESIAN_POINT ( 'NONE',  ( -87.14499999999998181, -4.716976649647092401, 6.492361379858946790 ) ) ;
#42989 = CIRCLE ( 'NONE', #56379, 7.499999999999985789 ) ;
#42990 = CARTESIAN_POINT ( 'NONE',  ( -4.716976649647098618, 113.2570736234661553, 6.492361379858953008 ) ) ;
#42991 = DIRECTION ( 'NONE',  ( 1.000000000000000000, 0.000000000000000000, 0.000000000000000000 ) ) ;
#42992 = DIRECTION ( 'NONE',  ( -0.000000000000000000, -0.000000000000000000, -1.000000000000000000 ) ) ;
#42993 = EDGE_CURVE ( 'NONE', #8709, #20853, #41536, .T. ) ;
#42994 = PRESENTATION_LAYER_ASSIGNMENT (  '', '', ( #57555 ) ) ;
#42995 = CARTESIAN_POINT ( 'NONE',  ( -74.50000000000000000, -2.220952357103124925E-14, 6.500000000000000000 ) ) ;
#42996 = ORIENTED_EDGE ( 'NONE', *, *, #57178, .T. ) ;
#42997 = CARTESIAN_POINT ( 'NONE',  ( -136.1929263765337907, -10.01517768586948698, 6.132527647946031529E-16 ) ) ;
#42998 = CARTESIAN_POINT ( 'NONE',  ( -145.0449999999999875, 7.632228543268600340, 2.479861379858949277 ) ) ;
#42999 = LINE ( 'NONE', #38416, #65061 ) ;
#43000 = COLOUR_RGB ( '', 0.40784314, 0.44705882, 0.49803922) ;
#43001 = CARTESIAN_POINT ( 'NONE',  ( -87.50000000000000000, -3.500000000000000000, 24.00000000000000000 ) ) ;
#43002 = EDGE_LOOP ( 'NONE', ( #9, #38201, #66515, #51838 ) ) ;
#43003 = ORIENTED_EDGE ( 'NONE', *, *, #66733, .T. ) ;
#43004 = AXIS2_PLACEMENT_3D ( 'NONE', #59356, #11195, #48530 ) ;
#43005 = CARTESIAN_POINT ( 'NONE',  ( 4.682380833558961619, -2.003239292658529624, 5.889878495889163901 ) ) ;
#43006 = PRODUCT_DEFINITION ( 'UNKNOWN', '', #24745, #1533 ) ;
#43007 = CIRCLE ( 'NONE', #65452, 3.499999999999999556 ) ;
#43008 = ADVANCED_FACE ( 'NONE', ( #46247 ), #30346, .T. ) ;
#43009 = EDGE_CURVE ( 'NONE', #26367, #57528, #30562, .T. ) ;
#43010 = DIRECTION ( 'NONE',  ( 1.000000000000000000, -1.156482317317873451E-16, 0.000000000000000000 ) ) ;
#43011 = DIRECTION ( 'NONE',  ( -0.000000000000000000, 1.000000000000000000, 0.000000000000000000 ) ) ;
#43012 = FACE_OUTER_BOUND ( 'NONE', #40483, .T. ) ;
#43013 =( GEOMETRIC_REPRESENTATION_CONTEXT ( 3 ) GLOBAL_UNCERTAINTY_ASSIGNED_CONTEXT ( ( #28591 ) ) GLOBAL_UNIT_ASSIGNED_CONTEXT ( ( #22298, #38174, #49391 ) ) REPRESENTATION_CONTEXT ( 'NONE', 'WORKASPACE' ) );
#43014 = FACE_OUTER_BOUND ( 'NONE', #44947, .T. ) ;
#43015 = CARTESIAN_POINT ( 'NONE',  ( 39.74999999999999289, 18.74999999999997868, -4.000000000000000000 ) ) ;
#43016 = EDGE_LOOP ( 'NONE', ( #58467, #24754, #9577 ) ) ;
#43017 = CARTESIAN_POINT ( 'NONE',  ( -147.5049999999999955, -6.826472737025113702, -4.959722759717900331 ) ) ;
#43018 = EDGE_CURVE ( 'NONE', #44052, #41519, #32805, .T. ) ;
#43019 = EDGE_CURVE ( 'NONE', #24199, #25898, #49027, .T. ) ;
#43020 = ORIENTED_EDGE ( 'NONE', *, *, #50669, .T. ) ;
#43021 =( NAMED_UNIT ( * ) SI_UNIT ( $, .STERADIAN. ) SOLID_ANGLE_UNIT ( ) );
#43022 = FILL_AREA_STYLE_COLOUR ( '', #38881 ) ;
#43023 = AXIS2_PLACEMENT_3D ( 'NONE', #46122, #29909, #62943 ) ;
#43024 = ORIENTED_EDGE ( 'NONE', *, *, #4513, .F. ) ;
#43025 = CARTESIAN_POINT ( 'NONE',  ( -57.48951619522433276, -8.499999999999994671, -0.6003161102123086845 ) ) ;
#43026 =( LENGTH_UNIT ( ) NAMED_UNIT ( * ) SI_UNIT ( .MILLI., .METRE. ) );
#43027 = CARTESIAN_POINT ( 'NONE',  ( 3.094860106618431583, 117.0949999999999989, 9.525000000000000355 ) ) ;
#43028 =( NAMED_UNIT ( * ) SI_UNIT ( $, .STERADIAN. ) SOLID_ANGLE_UNIT ( ) );
#43029 = VERTEX_POINT ( 'NONE', #15614 ) ;
#43030 = CARTESIAN_POINT ( 'NONE',  ( -40.99999999999998579, 107.7459666924148394, -3.000000000000000444 ) ) ;
#43032 = ADVANCED_FACE ( 'NONE', ( #38124 ), #15718, .T. ) ;
#43031 = CARTESIAN_POINT ( 'NONE',  ( -3.094860106618432471, 128.7049999999999841, -9.525000000000000355 ) ) ;
#43033 = CARTESIAN_POINT ( 'NONE',  ( -66.05499999999999261, -9.827790563157499189E-16, -8.024999999999991473 ) ) ;
#43034 = CARTESIAN_POINT ( 'NONE',  ( -121.1949999999999790, 8.437984349512085203, -1.550032578732815448E-15 ) ) ;
#43035 = CARTESIAN_POINT ( 'NONE',  ( -41.21690152797611262, 107.8360404011451834, -3.444195824416889096 ) ) ;
#43036 = EDGE_LOOP ( 'NONE', ( #4194, #244, #57833, #7533, #13270, #26325, #20450, #24099, #60530, #16701, #23769, #27208, #49562, #63841, #64866, #58127, #15433, #47950, #11206, #48616, #59580, #24890, #6623, #5586, #35226, #21400, #21015, #44975, #46746, #5144, #58082, #61407, #41427, #46333, #13729, #65796, #2880, #40662, #16956, #16225, #13708, #66476, #64602, #53435, #16301, #49156, #9710, #60218, #33638, #16158, #53194, #34256, #22164, #55556, #67742, #762, #47580, #45925, #39691, #52163, #56745, #39174, #26181, #59383, #19385, #65148, #15776, #9543, #52903, #54016, #65918, #2624, #11937, #63306, #8481, #25546, #35344, #3827, #39453, #68544, #6264, #36088, #58124, #45800, #3642, #45469, #25748, #8912, #54626, #48032, #1923, #11992, #48980, #43070, #18420, #61157 ) ) ;
#43037 = CARTESIAN_POINT ( 'NONE',  ( -8.102448949553181734, 147.0049999999999955, -5.886773742842749790 ) ) ;
#43038 = FACE_OUTER_BOUND ( 'NONE', #6275, .T. ) ;
#43039 = EDGE_CURVE ( 'NONE', #21950, #51841, #21914, .T. ) ;
#43040 = CIRCLE ( 'NONE', #35148, 0.7499999999999997780 ) ;
#43041 =( NAMED_UNIT ( * ) PLANE_ANGLE_UNIT ( ) SI_UNIT ( $, .RADIAN. ) );
#43042 = STYLED_ITEM ( 'NONE', ( #63170 ), #19408 ) ;
#43043 =( NAMED_UNIT ( * ) SI_UNIT ( $, .STERADIAN. ) SOLID_ANGLE_UNIT ( ) );
#43044 = ORIENTED_EDGE ( 'NONE', *, *, #38574, .T. ) ;
#43045 = LINE ( 'NONE', #65835, #60309 ) ;
#43046 = CARTESIAN_POINT ( 'NONE',  ( -168.8049999999999500, -8.437984349512085203, 5.166775262442717831E-16 ) ) ;
#43047 = ORIENTED_EDGE ( 'NONE', *, *, #7557, .F. ) ;
#43048 = CARTESIAN_POINT ( 'NONE',  ( -88.40707362346616094, 3.094860106618428031, -9.524999999999993250 ) ) ;
#43049 = AXIS2_PLACEMENT_3D ( 'NONE', #4581, #14447, #25010 ) ;
#43050 = STYLED_ITEM ( 'NONE', ( #66685 ), #252 ) ;
#43051 =( NAMED_UNIT ( * ) SI_UNIT ( $, .STERADIAN. ) SOLID_ANGLE_UNIT ( ) );
#43052 = FILL_AREA_STYLE ('',( #37779 ) ) ;
#43053 =( BOUNDED_CURVE ( )  B_SPLINE_CURVE ( 2, ( #11110, #12147, #43872, #33614, #60001, #59281, #26916, #33281, #48806, #32229, #28308 ),
 .UNSPECIFIED., .F., .F. ) 
 B_SPLINE_CURVE_WITH_KNOTS ( ( 3, 2, 2, 2, 2, 3 ),
 ( 0.5588235294117649410, 0.5647058823529413907, 0.5705882352941178404, 0.5764705882352942901, 0.5823529411764708508, 0.5882352941176473005 ),
 .UNSPECIFIED. ) 
 CURVE ( )  GEOMETRIC_REPRESENTATION_ITEM ( )  RATIONAL_B_SPLINE_CURVE ( ( 0.9999999999999981126, 0.9510565162951554186, 1.000000000000000000, 0.9510565162951535312, 1.000000000000000000, 0.9510565162951535312, 1.000000000000000000, 0.9510565162951535312, 1.000000000000000000, 0.9510565162951516438, 1.000000000000001776 ) ) 
 REPRESENTATION_ITEM ( '' )  );
#43054 = ORIENTED_EDGE ( 'NONE', *, *, #829, .T. ) ;
#43055 = CIRCLE ( 'NONE', #2519, 7.000000000000001776 ) ;
#43056 = FILL_AREA_STYLE ('',( #4288 ) ) ;
#43057 = SURFACE_SIDE_STYLE ('',( #58153 ) ) ;
#43058 = CARTESIAN_POINT ( 'NONE',  ( -86.15499999999998693, 7.632228543268600340, 2.479861379858949277 ) ) ;
#43059 = ORIENTED_EDGE ( 'NONE', *, *, #41088, .F. ) ;
#43060 = CARTESIAN_POINT ( 'NONE',  ( 22.99999999999995026, 0.000000000000000000, -32.00402776293824303 ) ) ;
#43061 =( NAMED_UNIT ( * ) SI_UNIT ( $, .STERADIAN. ) SOLID_ANGLE_UNIT ( ) );
#43062 = CARTESIAN_POINT ( 'NONE',  ( -135.0570736234661808, 0.000000000000000000, 9.524999999999991473 ) ) ;
#43063 = CONICAL_SURFACE ( 'NONE', #47528, 5.000000000000000000, 0.7853981633974415066 ) ;
#43064 = EDGE_CURVE ( 'NONE', #32747, #1828, #66197, .T. ) ;
#43065 = CARTESIAN_POINT ( 'NONE',  ( 7.632228543268607446, 144.1570736234661751, 2.479861379858954606 ) ) ;
#43066 = SURFACE_SIDE_STYLE ('',( #43421 ) ) ;
#43067 = CARTESIAN_POINT ( 'NONE',  ( -69.95707362346617231, 9.058813317711329915, -2.943386871421373119 ) ) ;
#43068 = AXIS2_PLACEMENT_3D ( 'NONE', #47450, #10124, #57967 ) ;
#43069 = CARTESIAN_POINT ( 'NONE',  ( -54.54999176738918010, -9.007918291183415249, 4.145374715402367016 ) ) ;
#43070 = ORIENTED_EDGE ( 'NONE', *, *, #20260, .F. ) ;
#43071 = DIRECTION ( 'NONE',  ( 0.000000000000000000, 0.000000000000000000, 1.000000000000000000 ) ) ;
#43072 = CARTESIAN_POINT ( 'NONE',  ( 57.49999999999998579, 30.74999999999999289, 4.000000000000000000 ) ) ;
#43073 = FILL_AREA_STYLE ('',( #37798 ) ) ;
#43074 = CARTESIAN_POINT ( 'NONE',  ( -108.0549999999999784, -9.827790563157499189E-16, -8.024999999999991473 ) ) ;
#43075 = CARTESIAN_POINT ( 'NONE',  ( -1.166476076187854022E-15, 122.9449999999999790, 9.525000000000000355 ) ) ;
#43076 = CIRCLE ( 'NONE', #52025, 0.2500000000000002220 ) ;
#43077 = CARTESIAN_POINT ( 'NONE',  ( -112.6449999999999960, 4.716976649647091513, -6.492361379858946790 ) ) ;
#43078 = CIRCLE ( 'NONE', #18326, 1.000000000000000888 ) ;
#43079 = CYLINDRICAL_SURFACE ( 'NONE', #943, 8.025000000000000355 ) ;
#43080 = VECTOR ( 'NONE', #40861, 1000.000000000000114 ) ;
#43082 = LINE ( 'NONE', #64130, #24645 ) ;
#43081 = CARTESIAN_POINT ( 'NONE',  ( -33.69829734337137239, -9.571662231021266010, -3.215428675379258916 ) ) ;
#43083 = CARTESIAN_POINT ( 'NONE',  ( -158.0929263765338249, 3.094860106618433360, 9.524999999999991473 ) ) ;
#43084 =( NAMED_UNIT ( * ) SI_UNIT ( $, .STERADIAN. ) SOLID_ANGLE_UNIT ( ) );
#43085 = CARTESIAN_POINT ( 'NONE',  ( -171.5949999999999704, 2.607480562269073321, 8.024999999999991473 ) ) ;
#43086 = STYLED_ITEM ( 'NONE', ( #38419 ), #29449 ) ;
#43087 = CARTESIAN_POINT ( 'NONE',  ( 10.00000000000002132, 50.00000000000000000, 65.00000000000000000 ) ) ;
#43088 = CARTESIAN_POINT ( 'NONE',  ( -61.94292637653379785, 0.000000000000000000, 9.524999999999991473 ) ) ;
#43089 = SURFACE_STYLE_USAGE ( .BOTH. , #42052 ) ;
#43090 = ORIENTED_EDGE ( 'NONE', *, *, #36594, .T. ) ;
#43091 = CARTESIAN_POINT ( 'NONE',  ( -77.24292637653380211, 5.598654528085804216, 7.705886871421366635 ) ) ;
#43092 = CARTESIAN_POINT ( 'NONE',  ( 3.749999999999999556, 33.74999999999998579, 3.750000000000000000 ) ) ;
#43093 =( NAMED_UNIT ( * ) PLANE_ANGLE_UNIT ( ) SI_UNIT ( $, .RADIAN. ) );
#43094 = ADVANCED_FACE ( 'NONE', ( #64811 ), #26478, .F. ) ;
#43095 = DIRECTION ( 'NONE',  ( 0.000000000000000000, 0.000000000000000000, 1.000000000000000000 ) ) ;
#43096 = CARTESIAN_POINT ( 'NONE',  ( 16.75000000000000711, 27.74999999999998224, -3.750000000000000000 ) ) ;
#43097 = CARTESIAN_POINT ( 'NONE',  ( 0.000000000000000000, 125.9429263765338192, -8.025000000000000355 ) ) ;
#43098 = CARTESIAN_POINT ( 'NONE',  ( -178.4050000000000011, -2.607480562269069768, 8.024999999999991473 ) ) ;
#43099 = EDGE_CURVE ( 'NONE', #52924, #43736, #27501, .T. ) ;
#43100 = VERTEX_POINT ( 'NONE', #26795 ) ;
#43101 = CARTESIAN_POINT ( 'NONE',  ( 13.75000000000000533, 30.74999999999999289, 3.750000000000000000 ) ) ;
#43102 = DIRECTION ( 'NONE',  ( 0.000000000000000000, 0.000000000000000000, -1.000000000000000000 ) ) ;
#43103 = DIRECTION ( 'NONE',  ( 0.000000000000000000, 0.000000000000000000, 1.000000000000000000 ) ) ;
#43104 = DIRECTION ( 'NONE',  ( -1.000000000000000000, 1.084202172485504434E-16, 0.000000000000000000 ) ) ;
#43105 = MECHANICAL_DESIGN_GEOMETRIC_PRESENTATION_REPRESENTATION (  '', ( #54287 ), #26220 ) ;
#43106 = FILL_AREA_STYLE ('',( #6445 ) ) ;
#43107 = CARTESIAN_POINT ( 'NONE',  ( 4.716976649647099507, 147.7570736234661695, -6.492361379858953008 ) ) ;
#43108 = AXIS2_PLACEMENT_3D ( 'NONE', #31736, #4659, #31044 ) ;
#43109 = ORIENTED_EDGE ( 'NONE', *, *, #68830, .T. ) ;
#43110 = CARTESIAN_POINT ( 'NONE',  ( -53.60138881051016568, -9.947368421052624754, -7.000000000000000000 ) ) ;
#43111 = CARTESIAN_POINT ( 'NONE',  ( -96.95499999999998408, -7.632228543268599452, 2.479861379858951054 ) ) ;
#43112 =( NAMED_UNIT ( * ) SI_UNIT ( $, .STERADIAN. ) SOLID_ANGLE_UNIT ( ) );
#43113 = VERTEX_POINT ( 'NONE', #716 ) ;
#43114 = EDGE_CURVE ( 'NONE', #45514, #17985, #68686, .T. ) ;
#43115 = CIRCLE ( 'NONE', #53229, 1.000000000000000888 ) ;
#43116 = DIRECTION ( 'NONE',  ( 1.000000000000000000, 0.000000000000000000, 0.000000000000000000 ) ) ;
#43117 = FILL_AREA_STYLE_COLOUR ( '', #17638 ) ;
#43118 = FILL_AREA_STYLE ('',( #5749 ) ) ;
#43119 = ORIENTED_EDGE ( 'NONE', *, *, #28062, .F. ) ;
#43120 = PRESENTATION_LAYER_ASSIGNMENT (  '', '', ( #44273 ) ) ;
#43121 = DIRECTION ( 'NONE',  ( 0.000000000000000000, 0.000000000000000000, 1.000000000000000000 ) ) ;
#43122 = CARTESIAN_POINT ( 'NONE',  ( -61.34499999999998465, 7.632228543268599452, -2.479861379858951942 ) ) ;
#43123 = ORIENTED_EDGE ( 'NONE', *, *, #68968, .F. ) ;
#43124 = AXIS2_PLACEMENT_3D ( 'NONE', #66424, #1307, #60782 ) ;
#43125 = PRESENTATION_STYLE_ASSIGNMENT (( #20579 ) ) ;
#43126 = CARTESIAN_POINT ( 'NONE',  ( 3.000000000000002665, 38.00000000000000711, -90.00000000000000000 ) ) ;
#43127 = EDGE_LOOP ( 'NONE', ( #28755, #68230, #58196, #12712 ) ) ;
#43128 =( NAMED_UNIT ( * ) SI_UNIT ( $, .STERADIAN. ) SOLID_ANGLE_UNIT ( ) );
#43129 = SURFACE_STYLE_USAGE ( .BOTH. , #21613 ) ;
#43130 = ORIENTED_EDGE ( 'NONE', *, *, #41473, .T. ) ;
#43131 = CIRCLE ( 'NONE', #47611, 0.9999999999999995559 ) ;
#43132 =( GEOMETRIC_REPRESENTATION_CONTEXT ( 3 ) GLOBAL_UNCERTAINTY_ASSIGNED_CONTEXT ( ( #29288 ) ) GLOBAL_UNIT_ASSIGNED_CONTEXT ( ( #66486, #61884, #44726 ) ) REPRESENTATION_CONTEXT ( 'NONE', 'WORKASPACE' ) );
#43133 = DIRECTION ( 'NONE',  ( 1.300977106640434891E-16, 0.000000000000000000, 1.000000000000000000 ) ) ;
#43134 = CARTESIAN_POINT ( 'NONE',  ( -120.0549999999999926, -9.827790563157499189E-16, -8.024999999999991473 ) ) ;
#43135 = ORIENTED_EDGE ( 'NONE', *, *, #23282, .T. ) ;
#43136 = ADVANCED_FACE ( 'NONE', ( #21 ), #55645, .T. ) ;
#43137 = SURFACE_STYLE_USAGE ( .BOTH. , #43490 ) ;
#43138 = VERTEX_POINT ( 'NONE', #44783 ) ;
#43139 = DIRECTION ( 'NONE',  ( 0.000000000000000000, 0.000000000000000000, 1.000000000000000000 ) ) ;
#43140 = DIRECTION ( 'NONE',  ( -0.000000000000000000, 1.000000000000000000, -0.000000000000000000 ) ) ;
#43141 = CARTESIAN_POINT ( 'NONE',  ( -74.99999999999998579, 50.00000000000000000, -6.500000000000000000 ) ) ;
#43142 = CARTESIAN_POINT ( 'NONE',  ( -164.4570736234661865, -9.058813317711329915, 2.943386871421371787 ) ) ;
#43143 = EDGE_CURVE ( 'NONE', #38534, #22897, #33616, .T. ) ;
#43144 = CARTESIAN_POINT ( 'NONE',  ( -1.166476076187854022E-15, 131.9449999999999932, 9.525000000000000355 ) ) ;
#43145 = CARTESIAN_POINT ( 'NONE',  ( -93.35707362346617799, 5.598654528085804216, 7.705886871421366635 ) ) ;
#43146 = MECHANICAL_DESIGN_GEOMETRIC_PRESENTATION_REPRESENTATION (  '', ( #58808 ), #27340 ) ;
#43147 = CIRCLE ( 'NONE', #26209, 0.5000000000000004441 ) ;
#43148 = FILL_AREA_STYLE ('',( #54674 ) ) ;
#43149 = EDGE_LOOP ( 'NONE', ( #67635, #21535, #58299, #4756 ) ) ;
#43150 = FILL_AREA_STYLE ('',( #16401 ) ) ;
#43152 = SURFACE_STYLE_USAGE ( .BOTH. , #789 ) ;
#43151 = DIRECTION ( 'NONE',  ( 1.300977106640434891E-16, 0.000000000000000000, 1.000000000000000000 ) ) ;
#43153 = CARTESIAN_POINT ( 'NONE',  ( -22.75000000000000711, 34.24999999999999289, -4.000000000000000000 ) ) ;
#43154 = CIRCLE ( 'NONE', #53355, 0.2500000000000002220 ) ;
#43155 = CARTESIAN_POINT ( 'NONE',  ( -136.2549999999999955, -4.716976649647092401, 6.492361379858946790 ) ) ;
#43156 = CARTESIAN_POINT ( 'NONE',  ( 39.49999999999999289, 16.24999999999997513, -3.750000000000000000 ) ) ;
#43157 = CARTESIAN_POINT ( 'NONE',  ( -34.99999999999992184, 110.4999999999999858, -9.500000000000000000 ) ) ;
#43158 = CARTESIAN_POINT ( 'NONE',  ( -145.0449999999999875, 7.632228543268600340, 2.479861379858949277 ) ) ;
#43159 = MECHANICAL_DESIGN_GEOMETRIC_PRESENTATION_REPRESENTATION (  '', ( #361 ), #39775 ) ;
#43160 = CIRCLE ( 'NONE', #30730, 0.5000000000000004441 ) ;
#43161 = CARTESIAN_POINT ( 'NONE',  ( -137.9949999999999477, -6.826472737025113702, 4.959722759717902107 ) ) ;
#43162 = ORIENTED_EDGE ( 'NONE', *, *, #50290, .T. ) ;
#43163 = CARTESIAN_POINT ( 'NONE',  ( 45.65811388296465623, 10.21937129432153135, -3.824795692829479954 ) ) ;
#43164 = AXIS2_PLACEMENT_3D ( 'NONE', #24303, #7775, #66533 ) ;
#43165 = DIRECTION ( 'NONE',  ( 0.000000000000000000, -0.7071067811865469066, -0.7071067811865482389 ) ) ;
#43166 = CIRCLE ( 'NONE', #47645, 1.499999999999997780 ) ;
#43167 = CARTESIAN_POINT ( 'NONE',  ( 4.750000000000002665, 22.24999999999998579, 3.750000000000000000 ) ) ;
#43168 = UNCERTAINTY_MEASURE_WITH_UNIT (LENGTH_MEASURE( 1.000000000000000082E-05 ), #37204, 'distance_accuracy_value', 'NONE');
#43169 = CARTESIAN_POINT ( 'NONE',  ( -58.85499999999998977, 4.716976649647094177, 6.492361379858945902 ) ) ;
#43170 =( LENGTH_UNIT ( ) NAMED_UNIT ( * ) SI_UNIT ( .MILLI., .METRE. ) );
#43171 = CARTESIAN_POINT ( 'NONE',  ( -62.24499999999998323, -4.716976649647093289, -6.492361379858945902 ) ) ;
#43172 = AXIS2_PLACEMENT_3D ( 'NONE', #14856, #64054, #10608 ) ;
#43173 = CARTESIAN_POINT ( 'NONE',  ( 39.49999999999999289, 18.74999999999997868, -3.750000000000000000 ) ) ;
#43174 = PRESENTATION_STYLE_ASSIGNMENT (( #64905 ) ) ;
#43175 = EDGE_CURVE ( 'NONE', #6283, #51146, #8930, .T. ) ;
#43176 = LINE ( 'NONE', #65609, #55941 ) ;
#43177 = CARTESIAN_POINT ( 'NONE',  ( -109.1929263765337907, -10.01517768586948698, 6.132527647946031529E-16 ) ) ;
#43178 = DIRECTION ( 'NONE',  ( 1.000000000000000000, 3.592223921739384069E-17, 2.549661825396426903E-17 ) ) ;
#43179 =( BOUNDED_CURVE ( )  B_SPLINE_CURVE ( 3, ( #4723, #5395, #26835, #48374 ),
 .UNSPECIFIED., .F., .F. ) 
 B_SPLINE_CURVE_WITH_KNOTS ( ( 4, 4 ),
 ( 0.000000000000000000, 1.570796326794896558 ),
 .UNSPECIFIED. ) 
 CURVE ( )  GEOMETRIC_REPRESENTATION_ITEM ( )  RATIONAL_B_SPLINE_CURVE ( ( 1.000000000000000000, 0.8047378541243649375, 0.8047378541243649375, 1.000000000000000000 ) ) 
 REPRESENTATION_ITEM ( '' )  );
#43180 = STYLED_ITEM ( 'NONE', ( #41242 ), #31349 ) ;
#43181 = CARTESIAN_POINT ( 'NONE',  ( 69.99999999999998579, 36.75000000000000000, 4.000000000000000000 ) ) ;
#43182 = CARTESIAN_POINT ( 'NONE',  ( 27.00000000000001776, 15.00000000000000000, -29.68999999999999417 ) ) ;
#43183 = CONICAL_SURFACE ( 'NONE', #3772, 7.000000000000000888, 0.7853981633974500554 ) ;
#43184 = AXIS2_PLACEMENT_3D ( 'NONE', #7994, #67089, #39348 ) ;
#43185 = CARTESIAN_POINT ( 'NONE',  ( -71.50000000000000000, 14.49137674618942562, 9.500000000000000000 ) ) ;
#43186 = ADVANCED_FACE ( 'NONE', ( #12033 ), #28542, .F. ) ;
#43187 = LINE ( 'NONE', #37907, #46506 ) ;
#43188 = DIRECTION ( 'NONE',  ( 0.000000000000000000, 1.000000000000000000, 0.000000000000000000 ) ) ;
#43189 = VERTEX_POINT ( 'NONE', #1425 ) ;
#43190 = AXIS2_PLACEMENT_3D ( 'NONE', #34833, #18333, #8477 ) ;
#43191 = EDGE_CURVE ( 'NONE', #58659, #67644, #26765, .T. ) ;
#43192 = CARTESIAN_POINT ( 'NONE',  ( 8.437984349512095861, 117.3070736234661666, 1.550032578732817026E-15 ) ) ;
#43193 = STYLED_ITEM ( 'NONE', ( #26880 ), #26973 ) ;
#43194 = ADVANCED_FACE ( 'NONE', ( #39856 ), #61579, .T. ) ;
#43195 = CARTESIAN_POINT ( 'NONE',  ( -19.98198699191933869, 115.0278726071232711, 9.999999999996266098 ) ) ;
#43196 = CARTESIAN_POINT ( 'NONE',  ( 75.00000000000000000, 20.22733879051553885, -6.503618960537654203 ) ) ;
#43197 = CARTESIAN_POINT ( 'NONE',  ( 4.000000000000030198, 38.70020753820971748, 89.00000000000000000 ) ) ;
#43198 = ORIENTED_EDGE ( 'NONE', *, *, #52814, .T. ) ;
#43199 = ORIENTED_EDGE ( 'NONE', *, *, #1587, .T. ) ;
#43200 = CARTESIAN_POINT ( 'NONE',  ( -11.74999999999999645, -4.000000000000000000, 19.00000000000000000 ) ) ;
#43201 = EDGE_CURVE ( 'NONE', #66680, #49089, #35230, .T. ) ;
#43202 = CARTESIAN_POINT ( 'NONE',  ( 0.000000000000000000, 154.4999999999999432, 0.000000000000000000 ) ) ;
#43203 = AXIS2_PLACEMENT_3D ( 'NONE', #25934, #69222, #31204 ) ;
#43204 = ORIENTED_EDGE ( 'NONE', *, *, #23461, .T. ) ;
#43205 = CARTESIAN_POINT ( 'NONE',  ( -9.058813317711337021, 126.1549999999999869, -2.943386871421374895 ) ) ;
#43206 = PRESENTATION_LAYER_ASSIGNMENT (  '', '', ( #4982 ) ) ;
#43207 = COLOUR_RGB ( '', 0.72549020, 0.75294118, 0.79215686) ;
#43208 = CYLINDRICAL_SURFACE ( 'NONE', #26029, 9.524999999999991473 ) ;
#43209 = CARTESIAN_POINT ( 'NONE',  ( -102.7449999999999903, 4.716976649647094177, 6.492361379858945902 ) ) ;
#43210 = ORIENTED_EDGE ( 'NONE', *, *, #47280, .T. ) ;
#43211 = FILL_AREA_STYLE_COLOUR ( '', #55752 ) ;
#43212 = CYLINDRICAL_SURFACE ( 'NONE', #37468, 0.5000000000000004441 ) ;
#43213 = ORIENTED_EDGE ( 'NONE', *, *, #53475, .F. ) ;
#43214 = DIRECTION ( 'NONE',  ( 0.000000000000000000, 0.000000000000000000, 1.000000000000000000 ) ) ;
#43215 = SURFACE_STYLE_USAGE ( .BOTH. , #26937 ) ;
#43216 =( NAMED_UNIT ( * ) PLANE_ANGLE_UNIT ( ) SI_UNIT ( $, .RADIAN. ) );
#43217 = AXIS2_PLACEMENT_3D ( 'NONE', #37648, #30921, #47511 ) ;
#43218 = ORIENTED_EDGE ( 'NONE', *, *, #10653, .T. ) ;
#43219 = CARTESIAN_POINT ( 'NONE',  ( 20.30219483484659548, 114.9087424184428130, -10.36565267485733877 ) ) ;
#43220 = ORIENTED_EDGE ( 'NONE', *, *, #16406, .T. ) ;
#43221 = CARTESIAN_POINT ( 'NONE',  ( 28.00000000000002842, 43.00000000000000000, 79.00402776293826435 ) ) ;
#43222 = CARTESIAN_POINT ( 'NONE',  ( 69.99999999999998579, 1.000000000000008438, 4.000000000000000000 ) ) ;
#43223 = LINE ( 'NONE', #64627, #40943 ) ;
#43224 = CARTESIAN_POINT ( 'NONE',  ( -6.062177826491069510, -2.500000000000000000, 3.499999999999999556 ) ) ;
#43225 = CYLINDRICAL_SURFACE ( 'NONE', #67967, 15.00000000000000000 ) ;
#43226 = DIRECTION ( 'NONE',  ( -0.000000000000000000, -1.000000000000000000, -0.000000000000000000 ) ) ;
#43228 = CARTESIAN_POINT ( 'NONE',  ( -54.49999999999999289, -2.024042244987997205E-14, -6.500000000000000000 ) ) ;
#43227 = CIRCLE ( 'NONE', #63417, 0.2500000000000002220 ) ;
#43229 = DIRECTION ( 'NONE',  ( -1.000000000000000000, 0.000000000000000000, 0.000000000000000000 ) ) ;
#43230 = CARTESIAN_POINT ( 'NONE',  ( -5.461490429277642278, 153.8976665511306692, 7.076668351203482032 ) ) ;
#43231 = ORIENTED_EDGE ( 'NONE', *, *, #61166, .F. ) ;
#43232 = ORIENTED_EDGE ( 'NONE', *, *, #35156, .F. ) ;
#43233 = CARTESIAN_POINT ( 'NONE',  ( -48.05707362346617373, 0.000000000000000000, 9.524999999999991473 ) ) ;
#43234 = DIRECTION ( 'NONE',  ( -0.000000000000000000, -1.000000000000000000, 0.000000000000000000 ) ) ;
#43235 = DIRECTION ( 'NONE',  ( -0.000000000000000000, -0.000000000000000000, 1.000000000000000000 ) ) ;
#43236 = AXIS2_PLACEMENT_3D ( 'NONE', #61613, #13442, #2851 ) ;
#43237 = ORIENTED_EDGE ( 'NONE', *, *, #39352, .T. ) ;
#43238 = CARTESIAN_POINT ( 'NONE',  ( -172.2549999999999955, -4.716976649647092401, 6.492361379858946790 ) ) ;
#43239 = CARTESIAN_POINT ( 'NONE',  ( 0.000000000000000000, 154.9999999999999716, -22.49999999999999645 ) ) ;
#43240 = FACE_OUTER_BOUND ( 'NONE', #10448, .T. ) ;
#43241 = CARTESIAN_POINT ( 'NONE',  ( -175.9449999999999932, -9.827790563157499189E-16, -8.024999999999991473 ) ) ;
#43242 = CARTESIAN_POINT ( 'NONE',  ( -164.0949999999999989, -2.607480562269071545, -8.024999999999991473 ) ) ;
#43243 = ORIENTED_EDGE ( 'NONE', *, *, #4942, .F. ) ;
#43244 = PRESENTATION_STYLE_ASSIGNMENT (( #65676 ) ) ;
#43245 = AXIS2_PLACEMENT_3D ( 'NONE', #57619, #24895, #18915 ) ;
#43246 =( NAMED_UNIT ( * ) SI_UNIT ( $, .STERADIAN. ) SOLID_ANGLE_UNIT ( ) );
#43247 = CARTESIAN_POINT ( 'NONE',  ( -4.716976649647097730, 150.2429263765338021, -6.492361379858953896 ) ) ;
#43248 = CARTESIAN_POINT ( 'NONE',  ( -80.60499999999996135, 6.826472737025113702, -4.959722759717902107 ) ) ;
#43249 = CARTESIAN_POINT ( 'NONE',  ( 1.000000000000000000, 43.00000000000000000, -35.50000000000000000 ) ) ;
#43250 = FILL_AREA_STYLE ('',( #37273 ) ) ;
#43251 = CARTESIAN_POINT ( 'NONE',  ( -75.00000000000000000, 35.50862325239523898, -9.539713813943809129 ) ) ;
#43252 = AXIS2_PLACEMENT_3D ( 'NONE', #51764, #41568, #47213 ) ;
#43253 = CARTESIAN_POINT ( 'NONE',  ( -76.64499999999999602, 4.716976649647091513, -6.492361379858946790 ) ) ;
#43254 = CARTESIAN_POINT ( 'NONE',  ( -5.598654528085808657, 135.7549999999999955, 7.705886871421373741 ) ) ;
#43255 = CARTESIAN_POINT ( 'NONE',  ( -133.8570736234661638, -5.598654528085803328, -7.705886871421366635 ) ) ;
#43256 = EDGE_CURVE ( 'NONE', #65411, #44314, #14833, .T. ) ;
#43257 = CARTESIAN_POINT ( 'NONE',  ( -171.1429263765338078, 5.598654528085800663, -7.705886871421367523 ) ) ;
#43258 = SURFACE_STYLE_USAGE ( .BOTH. , #48520 ) ;
#43259 = UNCERTAINTY_MEASURE_WITH_UNIT (LENGTH_MEASURE( 1.000000000000000082E-05 ), #62247, 'distance_accuracy_value', 'NONE');
#43260 = EDGE_CURVE ( 'NONE', #33694, #46319, #9564, .T. ) ;
#43261 = SURFACE_STYLE_USAGE ( .BOTH. , #64305 ) ;
#43262 = PRESENTATION_STYLE_ASSIGNMENT (( #51691 ) ) ;
#43263 = ADVANCED_FACE ( 'NONE', ( #34875 ), #19387, .F. ) ;
#43264 = ORIENTED_EDGE ( 'NONE', *, *, #68796, .T. ) ;
#43265 = CARTESIAN_POINT ( 'NONE',  ( -22.75000000000000711, 36.75000000000000000, 4.000000000000000000 ) ) ;
#43266 = EDGE_CURVE ( 'NONE', #38501, #50095, #38085, .T. ) ;
#43267 = AXIS2_PLACEMENT_3D ( 'NONE', #40009, #40688, #46327 ) ;
#43268 = AXIS2_PLACEMENT_3D ( 'NONE', #43462, #48719, #5387 ) ;
#43269 = EDGE_CURVE ( 'NONE', #631, #3378, #11065, .T. ) ;
#43270 = EDGE_CURVE ( 'NONE', #46307, #34430, #16233, .T. ) ;
#43272 =( NAMED_UNIT ( * ) SI_UNIT ( $, .STERADIAN. ) SOLID_ANGLE_UNIT ( ) );
#43271 = CARTESIAN_POINT ( 'NONE',  ( 36.00000000000002842, 0.000000000000000000, -32.00402776293825724 ) ) ;
#43273 = CARTESIAN_POINT ( 'NONE',  ( 18.25000000000000711, 33.74999999999999289, 3.750000000000000000 ) ) ;
#43274 = EDGE_LOOP ( 'NONE', ( #17632, #22132, #60856, #7009, #2440 ) ) ;
#43275 = ORIENTED_EDGE ( 'NONE', *, *, #54397, .T. ) ;
#43276 = FACE_OUTER_BOUND ( 'NONE', #34591, .T. ) ;
#43277 = AXIS2_PLACEMENT_3D ( 'NONE', #38554, #49093, #65226 ) ;
#43278 = EDGE_CURVE ( 'NONE', #4438, #43113, #50396, .T. ) ;
#43279 = CARTESIAN_POINT ( 'NONE',  ( -34.99999999999992895, 113.4999999999999858, -7.500000000000000000 ) ) ;
#43280 = VECTOR ( 'NONE', #43786, 1000.000000000000000 ) ;
#43281 = EDGE_CURVE ( 'NONE', #53207, #2615, #56004, .T. ) ;
#43282 = DIRECTION ( 'NONE',  ( 0.000000000000000000, 1.000000000000000000, -0.000000000000000000 ) ) ;
#43283 = DIRECTION ( 'NONE',  ( -1.000000000000000000, 0.000000000000000000, 0.000000000000000000 ) ) ;
#43284 = DIRECTION ( 'NONE',  ( 0.000000000000000000, 0.000000000000000000, -1.000000000000000000 ) ) ;
#43285 = SURFACE_STYLE_USAGE ( .BOTH. , #38681 ) ;
#43286 = ORIENTED_EDGE ( 'NONE', *, *, #36499, .T. ) ;
#43287 = CARTESIAN_POINT ( 'NONE',  ( -109.2549999999999955, -4.716976649647092401, 6.492361379858946790 ) ) ;
#43288 = ORIENTED_EDGE ( 'NONE', *, *, #40370, .F. ) ;
#43289 = CARTESIAN_POINT ( 'NONE',  ( 0.000000000000000000, 152.9999999999999716, 8.025000000000000355 ) ) ;
#43290 = CARTESIAN_POINT ( 'NONE',  ( -15.98999599679679839, 118.4999999999999716, -9.500000000000000000 ) ) ;
#43291 = ORIENTED_EDGE ( 'NONE', *, *, #13330, .F. ) ;
#43292 = CARTESIAN_POINT ( 'NONE',  ( 74.99999999999998579, 50.00000000000000000, 10.00000000000000000 ) ) ;
#43293 = CARTESIAN_POINT ( 'NONE',  ( 8.082903768654761123, 1.417096231345241097, 9.294316082458970795E-16 ) ) ;
#43294 = ORIENTED_EDGE ( 'NONE', *, *, #15996, .T. ) ;
#43295 =( LENGTH_UNIT ( ) NAMED_UNIT ( * ) SI_UNIT ( .MILLI., .METRE. ) );
#43296 = CARTESIAN_POINT ( 'NONE',  ( 5.598654528085809545, 160.1449999999999818, -7.705886871421373741 ) ) ;
#43297 = PLANE ( 'NONE',  #53127 ) ;
#43298 = CONICAL_SURFACE ( 'NONE', #12901, 4.499999999999976019, 0.7853981633974412846 ) ;
#43299 = ORIENTED_EDGE ( 'NONE', *, *, #1916, .F. ) ;
#43300 = STYLED_ITEM ( 'NONE', ( #8413 ), #8233 ) ;
#43301 = FILL_AREA_STYLE_COLOUR ( '', #47982 ) ;
#43302 = SURFACE_SIDE_STYLE ('',( #5933 ) ) ;
#43303 = CARTESIAN_POINT ( 'NONE',  ( 0.000000000000000000, 87.30187232391182306, 8.025000000000000355 ) ) ;
#43304 = CARTESIAN_POINT ( 'NONE',  ( -181.1929263765338192, -10.01517768586948698, 6.132527647946031529E-16 ) ) ;
#43305 = ORIENTED_EDGE ( 'NONE', *, *, #4913, .T. ) ;
#43306 = CARTESIAN_POINT ( 'NONE',  ( -7.632228543268607446, 123.5429263765338135, -2.479861379858953718 ) ) ;
#43307 = DIRECTION ( 'NONE',  ( -0.4999999999999999445, 0.000000000000000000, -0.8660254037844385966 ) ) ;
#43308 = DIRECTION ( 'NONE',  ( -0.8753987966738354665, 3.570037141435574061E-13, -0.4834014344020927112 ) ) ;
#43309 = B_SPLINE_CURVE_WITH_KNOTS ( 'NONE', 3,
 ( #19216, #3717, #29796, #50907, #30459, #13961, #14665, #35433 ),
 .UNSPECIFIED., .F., .F.,
 ( 4, 2, 2, 4 ),
 ( -6.733023926838822157E-06, 0.0008427316310560363033, 0.001267463958547469620, 0.001692196286038903045 ),
 .UNSPECIFIED. ) ;
#43310 = AXIS2_PLACEMENT_3D ( 'NONE', #46796, #8756, #16057 ) ;
#43311 = CARTESIAN_POINT ( 'NONE',  ( 4.716976649647096842, 124.7429263765338163, 6.492361379858953896 ) ) ;
#43312 = DIRECTION ( 'NONE',  ( 1.000000000000000000, 0.000000000000000000, 0.000000000000000000 ) ) ;
#43313 = ORIENTED_EDGE ( 'NONE', *, *, #51958, .F. ) ;
#43314 = DIRECTION ( 'NONE',  ( 0.000000000000000000, 0.000000000000000000, 1.000000000000000000 ) ) ;
#43315 = ORIENTED_EDGE ( 'NONE', *, *, #40690, .F. ) ;
#43316 =( GEOMETRIC_REPRESENTATION_CONTEXT ( 3 ) GLOBAL_UNCERTAINTY_ASSIGNED_CONTEXT ( ( #17856 ) ) GLOBAL_UNIT_ASSIGNED_CONTEXT ( ( #56252, #67166, #28825 ) ) REPRESENTATION_CONTEXT ( 'NONE', 'WORKASPACE' ) );
#43317 = CARTESIAN_POINT ( 'NONE',  ( -18.25000000000000711, 33.74999999999999289, -3.750000000000000000 ) ) ;
#43318 = DIRECTION ( 'NONE',  ( 1.000000000000000000, 0.000000000000000000, 0.000000000000000000 ) ) ;
#43319 = AXIS2_PLACEMENT_3D ( 'NONE', #18577, #14324, #8376 ) ;
#43320 = CARTESIAN_POINT ( 'NONE',  ( -142.1049999999999613, -6.826472737025115478, 4.959722759717900331 ) ) ;
#43321 = CARTESIAN_POINT ( 'NONE',  ( -72.00000000000000000, 35.92875272052971525, -7.000000000000000000 ) ) ;
#43322 = UNCERTAINTY_MEASURE_WITH_UNIT (LENGTH_MEASURE( 1.000000000000000082E-05 ), #26400, 'distance_accuracy_value', 'NONE');
#43323 = ADVANCED_FACE ( 'NONE', ( #11260 ), #10921, .F. ) ;
#43324 = CARTESIAN_POINT ( 'NONE',  ( -7.632228543268607446, 115.6570736234661467, -2.479861379858953718 ) ) ;
#43325 = FILL_AREA_STYLE ('',( #54145 ) ) ;
#43326 = ORIENTED_EDGE ( 'NONE', *, *, #16727, .T. ) ;
#43327 = ORIENTED_EDGE ( 'NONE', *, *, #15295, .T. ) ;
#43328 = CARTESIAN_POINT ( 'NONE',  ( -45.00000000000000000, 8.062885781073935831, 3.611004237778676185 ) ) ;
#43329 = CARTESIAN_POINT ( 'NONE',  ( -4.041451884327378785, 1.417096231345241542, 7.000000000000000000 ) ) ;
#43330 = CARTESIAN_POINT ( 'NONE',  ( -54.95499999999997698, -7.632228543268599452, 2.479861379858951054 ) ) ;
#43331 = ORIENTED_EDGE ( 'NONE', *, *, #49812, .T. ) ;
#43332 = DIRECTION ( 'NONE',  ( 0.000000000000000000, 1.000000000000000000, -0.000000000000000000 ) ) ;
#43333 = FILL_AREA_STYLE_COLOUR ( '', #38309 ) ;
#43334 = CARTESIAN_POINT ( 'NONE',  ( -25.00000000000000000, 0.000000000000000000, 3.000000000000000000 ) ) ;
#43335 = CARTESIAN_POINT ( 'NONE',  ( -60.44292637653379785, -1.166476076187852838E-15, -9.524999999999991473 ) ) ;
#43336 = AXIS2_PLACEMENT_3D ( 'NONE', #33471, #2070, #29572 ) ;
#43337 = DIRECTION ( 'NONE',  ( 0.000000000000000000, 1.000000000000000000, 0.000000000000000000 ) ) ;
#43338 = PRESENTATION_LAYER_ASSIGNMENT (  '', '', ( #8441 ) ) ;
#43339 = VERTEX_POINT ( 'NONE', #64030 ) ;
#43340 = CARTESIAN_POINT ( 'NONE',  ( -4.250000000000001776, 22.24999999999998579, 3.750000000000000000 ) ) ;
#43341 = MECHANICAL_DESIGN_GEOMETRIC_PRESENTATION_REPRESENTATION (  '', ( #3936 ), #39950 ) ;
#43342 = CARTESIAN_POINT ( 'NONE',  ( 3.062992266794108520, 51.20951172609373003, -7.099524902877636379 ) ) ;
#43343 = CYLINDRICAL_SURFACE ( 'NONE', #32536, 5.000000000000004441 ) ;
#43344 = CARTESIAN_POINT ( 'NONE',  ( -15.48999599679679662, 146.9999999999999716, -7.000000000000000000 ) ) ;
#43345 = EDGE_CURVE ( 'NONE', #19358, #61162, #15534, .T. ) ;
#43346 = CARTESIAN_POINT ( 'NONE',  ( -112.9449999999999932, -9.827790563157499189E-16, -8.024999999999991473 ) ) ;
#43347 = CARTESIAN_POINT ( 'NONE',  ( 3.094860106618431583, 159.0949999999999420, 9.525000000000000355 ) ) ;
#43348 = CARTESIAN_POINT ( 'NONE',  ( -89.39499999999996760, -6.826472737025115478, -4.959722759717899443 ) ) ;
#43349 = DIRECTION ( 'NONE',  ( 1.000000000000000000, 0.000000000000000000, 0.000000000000000000 ) ) ;
#43350 = LINE ( 'NONE', #42313, #35945 ) ;
#43351 = CARTESIAN_POINT ( 'NONE',  ( 25.00000000000001421, 42.00000000000000000, 34.49999999999999289 ) ) ;
#43352 = UNCERTAINTY_MEASURE_WITH_UNIT (LENGTH_MEASURE( 1.000000000000000082E-05 ), #53743, 'distance_accuracy_value', 'NONE');
#43353 = EDGE_CURVE ( 'NONE', #18998, #18360, #15876, .T. ) ;
#43354 = STYLED_ITEM ( 'NONE', ( #53557 ), #27838 ) ;
#43356 = SURFACE_STYLE_FILL_AREA ( #48957 ) ;
#43355 =( REPRESENTATION_RELATIONSHIP ('NONE','NONE', #5102, #31597 ) REPRESENTATION_RELATIONSHIP_WITH_TRANSFORMATION ( #63106 )SHAPE_REPRESENTATION_RELATIONSHIP( ) );
#43357 = AXIS2_PLACEMENT_3D ( 'NONE', #35825, #57990, #26294 ) ;
#43358 = ORIENTED_EDGE ( 'NONE', *, *, #19029, .T. ) ;
#43359 = CARTESIAN_POINT ( 'NONE',  ( -123.2929263765337993, 3.094860106618428031, -9.524999999999993250 ) ) ;
#43360 = SURFACE_STYLE_USAGE ( .BOTH. , #38754 ) ;
#43361 = CARTESIAN_POINT ( 'NONE',  ( -150.1450000000000102, -4.716976649647092401, 6.492361379858946790 ) ) ;
#43362 = AXIS2_PLACEMENT_3D ( 'NONE', #53988, #66277, #27237 ) ;
#43363 = ADVANCED_FACE ( 'NONE', ( #53816 ), #7705, .F. ) ;
#43364 = CARTESIAN_POINT ( 'NONE',  ( -66.35707362346616378, 5.598654528085804216, 7.705886871421366635 ) ) ;
#43365 = CARTESIAN_POINT ( 'NONE',  ( -195.0000000000000000, 0.000000000000000000, 9.524999999999991473 ) ) ;
#43366 = EDGE_LOOP ( 'NONE', ( #5017, #65874, #43605, #22730 ) ) ;
#43367 = EDGE_LOOP ( 'NONE', ( #64758, #24178, #53702 ) ) ;
#43368 = AXIS2_PLACEMENT_3D ( 'NONE', #64962, #16485, #21358 ) ;
#43369 = CARTESIAN_POINT ( 'NONE',  ( 30.25000000000000711, 18.74999999999997868, 3.750000000000000000 ) ) ;
#43370 = EDGE_CURVE ( 'NONE', #40236, #67406, #21164, .T. ) ;
#43371 = DIRECTION ( 'NONE',  ( 1.000000000000000000, 0.000000000000000000, 0.000000000000000000 ) ) ;
#43372 = CARTESIAN_POINT ( 'NONE',  ( -45.00000000000000000, 9.484039020261588959, 6.483595844450460888 ) ) ;
#43373 = CARTESIAN_POINT ( 'NONE',  ( -129.2070736234668402, 3.094860106629659491, 9.524999999991834443 ) ) ;
#43374 = DIRECTION ( 'NONE',  ( 0.000000000000000000, 0.000000000000000000, 1.000000000000000000 ) ) ;
#43375 = ORIENTED_EDGE ( 'NONE', *, *, #5219, .F. ) ;
#43376 = CARTESIAN_POINT ( 'NONE',  ( -137.9049999999999727, 2.607480562269069324, -8.024999999999993250 ) ) ;
#43377 = ORIENTED_EDGE ( 'NONE', *, *, #6677, .T. ) ;
#43378 = AXIS2_PLACEMENT_3D ( 'NONE', #41523, #67538, #19695 ) ;
#43379 = ORIENTED_EDGE ( 'NONE', *, *, #19129, .F. ) ;
#43380 = CARTESIAN_POINT ( 'NONE',  ( -142.4070736234666583, 3.094860106610092920, -9.525000000006050627 ) ) ;
#43381 = EDGE_LOOP ( 'NONE', ( #44854, #55854, #10101, #63483 ) ) ;
#43382 = COLOUR_RGB ( '', 0.31764706, 0.68627451, 0.89019608) ;
#43383 = FILL_AREA_STYLE ('',( #11302 ) ) ;
#43384 = CARTESIAN_POINT ( 'NONE',  ( 9.058813317711337021, 126.5449999999999875, 2.943386871421375783 ) ) ;
#43385 = CARTESIAN_POINT ( 'NONE',  ( 0.000000000000000000, 42.00000000000000000, -75.00000000000001421 ) ) ;
#43386 = PRESENTATION_LAYER_ASSIGNMENT (  '', '', ( #64666 ) ) ;
#43387 =( BOUNDED_CURVE ( )  B_SPLINE_CURVE ( 3, ( #18547, #28013, #66366, #24152 ),
 .UNSPECIFIED., .F., .F. ) 
 B_SPLINE_CURVE_WITH_KNOTS ( ( 4, 4 ),
 ( 0.000000000000000000, 1.570796326794896558 ),
 .UNSPECIFIED. ) 
 CURVE ( )  GEOMETRIC_REPRESENTATION_ITEM ( )  RATIONAL_B_SPLINE_CURVE ( ( 1.000000000000000000, 0.8047378541243649375, 0.8047378541243649375, 1.000000000000000000 ) ) 
 REPRESENTATION_ITEM ( '' )  );
#43388 = ORIENTED_EDGE ( 'NONE', *, *, #57754, .T. ) ;
#43389 = CARTESIAN_POINT ( 'NONE',  ( 0.000000000000000000, 134.5549999999999784, -9.525000000000000355 ) ) ;
#43390 = CARTESIAN_POINT ( 'NONE',  ( -66.35499999999998977, -4.716976649647093289, -6.492361379858945902 ) ) ;
#43391 = AXIS2_PLACEMENT_3D ( 'NONE', #65522, #33510, #50061 ) ;
#43392 = CARTESIAN_POINT ( 'NONE',  ( -118.6449999999999818, 4.716976649647091513, -6.492361379858946790 ) ) ;
#43393 = DIRECTION ( 'NONE',  ( 1.000000000000000000, -0.000000000000000000, 0.000000000000000000 ) ) ;
#43394 = ORIENTED_EDGE ( 'NONE', *, *, #54782, .F. ) ;
#43395 = CARTESIAN_POINT ( 'NONE',  ( -8.102448949553181734, 144.0050000000000239, -5.886773742842749790 ) ) ;
#43396 = DIRECTION ( 'NONE',  ( -1.156482317317870344E-15, -1.000000000000000000, -0.000000000000000000 ) ) ;
#43397 = UNCERTAINTY_MEASURE_WITH_UNIT (LENGTH_MEASURE( 1.000000000000000082E-05 ), #7052, 'distance_accuracy_value', 'NONE');
#43398 = FILL_AREA_STYLE_COLOUR ( '', #53548 ) ;
#43399 = DIRECTION ( 'NONE',  ( 0.000000000000000000, 0.000000000000000000, -1.000000000000000000 ) ) ;
#43400 = SURFACE_STYLE_FILL_AREA ( #5334 ) ;
#43401 = ORIENTED_EDGE ( 'NONE', *, *, #23196, .F. ) ;
#43402 = CYLINDRICAL_SURFACE ( 'NONE', #55371, 1.000000000000000888 ) ;
#43403 = CARTESIAN_POINT ( 'NONE',  ( -174.3549999999999898, -4.716976649647093289, -6.492361379858945902 ) ) ;
#43404 = EDGE_LOOP ( 'NONE', ( #58868, #21721, #22720, #40568 ) ) ;
#43405 = DIRECTION ( 'NONE',  ( -0.000000000000000000, 0.000000000000000000, -1.000000000000000000 ) ) ;
#43406 = UNCERTAINTY_MEASURE_WITH_UNIT (LENGTH_MEASURE( 1.000000000000000082E-05 ), #55608, 'distance_accuracy_value', 'NONE');
#43407 = EDGE_CURVE ( 'NONE', #24199, #29573, #27067, .T. ) ;
#43408 = CARTESIAN_POINT ( 'NONE',  ( 0.000000000000000000, 114.9999999999999574, 0.000000000000000000 ) ) ;
#43409 = CARTESIAN_POINT ( 'NONE',  ( -195.0000000000000000, 0.000000000000000000, 0.000000000000000000 ) ) ;
#43410 = CARTESIAN_POINT ( 'NONE',  ( -19.00000000000000000, 8.000000000000000000, 4.000000000000000000 ) ) ;
#43411 = CARTESIAN_POINT ( 'NONE',  ( -77.54292637653379927, 9.058813317711329915, 2.943386871421369566 ) ) ;
#43412 = ADVANCED_FACE ( 'NONE', ( #9901 ), #58414, .T. ) ;
#43413 = ORIENTED_EDGE ( 'NONE', *, *, #53541, .T. ) ;
#43414 = FILL_AREA_STYLE_COLOUR ( '', #13648 ) ;
#43415 = CYLINDRICAL_SURFACE ( 'NONE', #16737, 0.5000000000000004441 ) ;
#43416 = CARTESIAN_POINT ( 'NONE',  ( -80.75499999999999545, 4.716976649647091513, -6.492361379858946790 ) ) ;
#43417 = VERTEX_POINT ( 'NONE', #1337 ) ;
#43418 = CARTESIAN_POINT ( 'NONE',  ( -34.99999999999992895, 112.4999999999999858, 10.00000000000000000 ) ) ;
#43419 = CARTESIAN_POINT ( 'NONE',  ( -2.607480562269064439, 112.2929263765338135, 8.025000000000007461 ) ) ;
#43420 = DIRECTION ( 'NONE',  ( -0.000000000000000000, -0.000000000000000000, -1.000000000000000000 ) ) ;
#43421 = SURFACE_STYLE_FILL_AREA ( #38813 ) ;
#43422 = CARTESIAN_POINT ( 'NONE',  ( -67.55707362346618083, -1.166476076187852838E-15, -9.524999999999991473 ) ) ;
#43423 = DIRECTION ( 'NONE',  ( -1.000000000000000000, 0.000000000000000000, 0.000000000000000000 ) ) ;
#43424 = ORIENTED_EDGE ( 'NONE', *, *, #21596, .T. ) ;
#43425 = FACE_OUTER_BOUND ( 'NONE', #35130, .T. ) ;
#43426 = FILL_AREA_STYLE_COLOUR ( '', #38123 ) ;
#43428 = CARTESIAN_POINT ( 'NONE',  ( 39.74999999999999289, 18.74999999999997868, -3.750000000000000000 ) ) ;
#43427 = SPHERICAL_SURFACE ( 'NONE', #31319, 1.000000000000000000 ) ;
#43429 = EDGE_CURVE ( 'NONE', #53864, #1748, #6214, .T. ) ;
#43430 = AXIS2_PLACEMENT_3D ( 'NONE', #47169, #20748, #31627 ) ;
#43431 = CARTESIAN_POINT ( 'NONE',  ( -101.0049999999999812, 6.826472737025116366, 4.959722759717898555 ) ) ;
#43432 = ADVANCED_FACE ( 'NONE', ( #966 ), #32401, .T. ) ;
#43433 = CARTESIAN_POINT ( 'NONE',  ( 9.058813317711338797, 132.8449999999999989, -2.943386871421372675 ) ) ;
#43434 = CARTESIAN_POINT ( 'NONE',  ( -112.4949999999999761, 6.826472737025113702, -4.959722759717902107 ) ) ;
#43435 = CARTESIAN_POINT ( 'NONE',  ( -74.75000000000000000, -0.9999999999999995559, 5.000000000000001776 ) ) ;
#43436 = PRESENTATION_LAYER_ASSIGNMENT (  '', '', ( #63549 ) ) ;
#43438 = CYLINDRICAL_SURFACE ( 'NONE', #32529, 1.000000000000000000 ) ;
#43437 = LINE ( 'NONE', #17697, #53680 ) ;
#43439 = ADVANCED_FACE ( 'NONE', ( #60145 ), #50291, .F. ) ;
#43440 = CARTESIAN_POINT ( 'NONE',  ( -162.4429263765338192, -1.166476076187852838E-15, -9.524999999999991473 ) ) ;
#43441 = CARTESIAN_POINT ( 'NONE',  ( -173.9949999999999761, -6.826472737025115478, 4.959722759717900331 ) ) ;
#43442 = EDGE_CURVE ( 'NONE', #25944, #53365, #68378, .T. ) ;
#43443 = CARTESIAN_POINT ( 'NONE',  ( -2.607480562269032021, 148.2070736234661581, -8.025000000000032330 ) ) ;
#43444 = EDGE_CURVE ( 'NONE', #60007, #7926, #55196, .T. ) ;
#43445 = CARTESIAN_POINT ( 'NONE',  ( -42.59563188260839439, -13.96749343005688715, 0.7786704236754057318 ) ) ;
#43446 = ORIENTED_EDGE ( 'NONE', *, *, #32884, .F. ) ;
#43447 = CARTESIAN_POINT ( 'NONE',  ( 71.49999999999998579, 64.07124727947029896, -7.500000000000000000 ) ) ;
#43448 = EDGE_LOOP ( 'NONE', ( #26818, #22207, #6905, #55536 ) ) ;
#43449 = CARTESIAN_POINT ( 'NONE',  ( -79.19292637653379074, -10.01517768586948698, 6.132527647946031529E-16 ) ) ;
#43450 = DIRECTION ( 'NONE',  ( 0.000000000000000000, 1.000000000000000000, -0.000000000000000000 ) ) ;
#43451 = CARTESIAN_POINT ( 'NONE',  ( 24.21231517720798010, 113.4999999999999858, 9.500000000000000000 ) ) ;
#43452 = AXIS2_PLACEMENT_3D ( 'NONE', #44866, #38902, #66273 ) ;
#43453 = EDGE_CURVE ( 'NONE', #33557, #42181, #39415, .T. ) ;
#43454 = CARTESIAN_POINT ( 'NONE',  ( -75.48275862068965125, 63.99167409976910648, -9.500000000000001776 ) ) ;
#43455 = DIRECTION ( 'NONE',  ( -0.000000000000000000, 0.000000000000000000, -1.000000000000000000 ) ) ;
#43456 = CONICAL_SURFACE ( 'NONE', #52411, 9.000000000000007105, 0.7853981633974500554 ) ;
#43457 = EDGE_LOOP ( 'NONE', ( #10867, #69030, #34282 ) ) ;
#43458 = CARTESIAN_POINT ( 'NONE',  ( -176.7549999999999955, 4.716976649647091513, -6.492361379858946790 ) ) ;
#43459 = AXIS2_PLACEMENT_3D ( 'NONE', #5157, #58985, #42501 ) ;
#43460 = ORIENTED_EDGE ( 'NONE', *, *, #10823, .F. ) ;
#43461 = CARTESIAN_POINT ( 'NONE',  ( 34.99999999999992895, 112.4999999999999858, 10.00000000000000000 ) ) ;
#43462 = CARTESIAN_POINT ( 'NONE',  ( 0.000000000000000000, 0.000000000000000000, 0.000000000000000000 ) ) ;
#43463 = CARTESIAN_POINT ( 'NONE',  ( 69.99999999999998579, 1.000000000000008438, 3.000000000000000000 ) ) ;
#43464 = CARTESIAN_POINT ( 'NONE',  ( 3.749999999999999556, 34.24999999999998579, -3.750000000000000000 ) ) ;
#43465 = CARTESIAN_POINT ( 'NONE',  ( -2.607480562269075097, 143.4070736234661751, 8.025000000000000355 ) ) ;
#43466 = ORIENTED_EDGE ( 'NONE', *, *, #29852, .T. ) ;
#43467 = CARTESIAN_POINT ( 'NONE',  ( -89.90499999999997272, 2.607480562269069324, -8.024999999999993250 ) ) ;
#43468 = UNCERTAINTY_MEASURE_WITH_UNIT (LENGTH_MEASURE( 1.000000000000000082E-05 ), #10217, 'distance_accuracy_value', 'NONE');
#43469 = CARTESIAN_POINT ( 'NONE',  ( 18.25000000000000711, 33.74999999999999289, 3.750000000000000000 ) ) ;
#43470 = EDGE_LOOP ( 'NONE', ( #62688, #9705, #23860, #17447 ) ) ;
#43471 = DIRECTION ( 'NONE',  ( 0.000000000000000000, 0.000000000000000000, 1.000000000000000000 ) ) ;
#43472 = AXIS2_PLACEMENT_3D ( 'NONE', #23405, #45942, #18145 ) ;
#43473 = SURFACE_SIDE_STYLE ('',( #28931 ) ) ;
#43474 = CARTESIAN_POINT ( 'NONE',  ( 30.50000000000000711, 18.74999999999997868, -3.750000000000000000 ) ) ;
#43475 = LINE ( 'NONE', #48381, #39000 ) ;
#43476 = CARTESIAN_POINT ( 'NONE',  ( 24.08647788275853685, 27.27834388199489268, -27.25847631938719218 ) ) ;
#43477 = ORIENTED_EDGE ( 'NONE', *, *, #44645, .T. ) ;
#43478 = CARTESIAN_POINT ( 'NONE',  ( -62.84499999999998465, -7.632228543268599452, 2.479861379858951054 ) ) ;
#43479 = ORIENTED_EDGE ( 'NONE', *, *, #69557, .F. ) ;
#43480 = CARTESIAN_POINT ( 'NONE',  ( 48.00000000000000000, 13.41640786499872284, -7.000000000000000000 ) ) ;
#43481 = EDGE_CURVE ( 'NONE', #11857, #49555, #34101, .T. ) ;
#43482 = DIRECTION ( 'NONE',  ( -0.000000000000000000, -1.000000000000000000, -0.000000000000000000 ) ) ;
#43483 = ORIENTED_EDGE ( 'NONE', *, *, #43801, .F. ) ;
#43484 = ORIENTED_EDGE ( 'NONE', *, *, #7684, .T. ) ;
#43485 = DIRECTION ( 'NONE',  ( 1.000000000000000000, 0.000000000000000000, 0.000000000000000000 ) ) ;
#43486 = LINE ( 'NONE', #59588, #31176 ) ;
#43487 = CARTESIAN_POINT ( 'NONE',  ( -117.9549999999999841, -7.632228543268599452, 2.479861379858951054 ) ) ;
#43488 = ORIENTED_EDGE ( 'NONE', *, *, #5464, .T. ) ;
#43489 =( NAMED_UNIT ( * ) SI_UNIT ( $, .STERADIAN. ) SOLID_ANGLE_UNIT ( ) );
#43490 = SURFACE_SIDE_STYLE ('',( #5768 ) ) ;
#43491 = SURFACE_STYLE_FILL_AREA ( #6143 ) ;
#43492 = DIRECTION ( 'NONE',  ( -1.000000000000000000, 0.000000000000000000, 0.000000000000000000 ) ) ;
#43493 = SURFACE_STYLE_FILL_AREA ( #38891 ) ;
#43494 = CARTESIAN_POINT ( 'NONE',  ( -158.0070736234661695, -8.102448949553172852, -5.886773742842741797 ) ) ;
#43495 = CARTESIAN_POINT ( 'NONE',  ( 0.000000000000000000, 136.4449999999999932, -9.525000000000000355 ) ) ;
#43496 = CARTESIAN_POINT ( 'NONE',  ( -94.85707362346616378, -5.598654528085803328, -7.705886871421366635 ) ) ;
#43497 = EDGE_CURVE ( 'NONE', #41337, #17478, #44015, .T. ) ;
#43498 = CARTESIAN_POINT ( 'NONE',  ( 23.71231517720798010, 117.9999999999999716, -9.500000000000000000 ) ) ;
#43499 = VERTEX_POINT ( 'NONE', #60814 ) ;
#43500 = AXIS2_PLACEMENT_3D ( 'NONE', #39645, #61062, #29031 ) ;
#43501 = EDGE_CURVE ( 'NONE', #48146, #68819, #21307, .T. ) ;
#43502 = CARTESIAN_POINT ( 'NONE',  ( -133.5549999999999784, 0.000000000000000000, 8.024999999999991473 ) ) ;
#43503 = CARTESIAN_POINT ( 'NONE',  ( -86.45707362346617231, -9.058813317711329915, 2.943386871421371787 ) ) ;
#43504 = ADVANCED_FACE ( 'NONE', ( #49257 ), #59798, .T. ) ;
#43505 = AXIS2_PLACEMENT_3D ( 'NONE', #2078, #40166, #61561 ) ;
#43506 = CARTESIAN_POINT ( 'NONE',  ( 3.414213562373098032, 34.36176364315826248, -80.00402776293826435 ) ) ;
#43507 = CARTESIAN_POINT ( 'NONE',  ( -147.2949999999999591, -2.607480562269069768, 8.024999999999991473 ) ) ;
#43508 = CARTESIAN_POINT ( 'NONE',  ( -135.4449999999999932, 0.000000000000000000, 8.024999999999991473 ) ) ;
#43509 = VERTEX_POINT ( 'NONE', #23889 ) ;
#43510 = CARTESIAN_POINT ( 'NONE',  ( 45.65811388300841855, 10.21937129433612057, -4.000000000000003553 ) ) ;
#43511 =( NAMED_UNIT ( * ) PLANE_ANGLE_UNIT ( ) SI_UNIT ( $, .RADIAN. ) );
#43512 = ADVANCED_FACE ( 'NONE', ( #67860 ), #14369, .F. ) ;
#43513 = CARTESIAN_POINT ( 'NONE',  ( 2.999999999999994671, 5.000000000000000000, -24.00402776293822527 ) ) ;
#43514 = CARTESIAN_POINT ( 'NONE',  ( -51.50499999999999545, -6.826472737025115478, -4.959722759717899443 ) ) ;
#43515 = CARTESIAN_POINT ( 'NONE',  ( -57.89499999999996760, 6.826472737025116366, 4.959722759717898555 ) ) ;
#43516 = EDGE_CURVE ( 'NONE', #5028, #45388, #19292, .T. ) ;
#43517 = CIRCLE ( 'NONE', #17682, 5.500000000000005329 ) ;
#43518 = DIRECTION ( 'NONE',  ( 0.000000000000000000, 0.000000000000000000, -1.000000000000000000 ) ) ;
#43519 = CARTESIAN_POINT ( 'NONE',  ( -102.9570736234661723, 9.058813317711329915, -2.943386871421373119 ) ) ;
#43520 = SURFACE_SIDE_STYLE ('',( #6171 ) ) ;
#43521 = CARTESIAN_POINT ( 'NONE',  ( 4.750000000000002665, 0.000000000000000000, 4.000000000000000000 ) ) ;
#43522 = CARTESIAN_POINT ( 'NONE',  ( -102.7429263765338021, -5.598654528085803328, -7.705886871421366635 ) ) ;
#43523 = CARTESIAN_POINT ( 'NONE',  ( 1.700000000000102540, 49.99999999999982947, -59.99999999999958078 ) ) ;
#43524 = SURFACE_STYLE_USAGE ( .BOTH. , #489 ) ;
#43525 = CIRCLE ( 'NONE', #37902, 0.2500000000000002220 ) ;
#43526 = LINE ( 'NONE', #10433, #20225 ) ;
#43527 = SURFACE_STYLE_FILL_AREA ( #49455 ) ;
#43528 = DIRECTION ( 'NONE',  ( 1.000000000000000000, 0.000000000000000000, 0.000000000000000000 ) ) ;
#43529 = EDGE_CURVE ( 'NONE', #26425, #18324, #14741, .T. ) ;
#43530 = VERTEX_POINT ( 'NONE', #8760 ) ;
#43531 = SURFACE_SIDE_STYLE ('',( #498 ) ) ;
#43532 = ORIENTED_EDGE ( 'NONE', *, *, #5187, .T. ) ;
#43533 =( NAMED_UNIT ( * ) SI_UNIT ( $, .STERADIAN. ) SOLID_ANGLE_UNIT ( ) );
#43534 = ADVANCED_FACE ( 'NONE', ( #35841 ), #67151, .T. ) ;
#43535 = CARTESIAN_POINT ( 'NONE',  ( 6.826472737025121695, 111.6070736234661354, -4.959722759717905660 ) ) ;
#43536 = DIRECTION ( 'NONE',  ( -1.000000000000000000, 0.000000000000000000, 0.000000000000000000 ) ) ;
#43537 = CARTESIAN_POINT ( 'NONE',  ( 10.99999999999999645, 11.99999999999999289, -4.000000000000000000 ) ) ;
#43538 = EDGE_LOOP ( 'NONE', ( #41597, #29641, #8652, #22127 ) ) ;
#43539 = VERTEX_POINT ( 'NONE', #62215 ) ;
#43540 = CARTESIAN_POINT ( 'NONE',  ( -5.356721384544675502, -2.367558512213879141, -4.721886399977922366 ) ) ;
#43541 = CARTESIAN_POINT ( 'NONE',  ( -34.99999999999999289, 99.99999999999998579, -7.500000000000000000 ) ) ;
#43542 = CARTESIAN_POINT ( 'NONE',  ( -75.50000000000000000, 35.50862325381056905, -6.499999999999999112 ) ) ;
#43543 = ORIENTED_EDGE ( 'NONE', *, *, #37320, .T. ) ;
#43544 = CARTESIAN_POINT ( 'NONE',  ( 27.00000000000001776, 14.00000000000000000, -29.68999999999999417 ) ) ;
#43545 = CIRCLE ( 'NONE', #39070, 5.249999999999991118 ) ;
#43546 = CARTESIAN_POINT ( 'NONE',  ( -119.1570736234661751, -9.058813317711329915, -2.943386871421370898 ) ) ;
#43547 = CARTESIAN_POINT ( 'NONE',  ( -195.0000000000000000, 0.000000000000000000, 0.000000000000000000 ) ) ;
#43548 = CARTESIAN_POINT ( 'NONE',  ( -94.79499999999997328, 2.607480562269068880, -8.024999999999993250 ) ) ;
#43549 = VERTEX_POINT ( 'NONE', #8426 ) ;
#43550 = CARTESIAN_POINT ( 'NONE',  ( 24.21231517720798010, 113.4999999999999858, -10.00000000000000000 ) ) ;
#43551 = SURFACE_STYLE_FILL_AREA ( #520 ) ;
#43552 = DIRECTION ( 'NONE',  ( 1.000000000000000000, 0.000000000000000000, 0.000000000000000000 ) ) ;
#43553 = ORIENTED_EDGE ( 'NONE', *, *, #62862, .T. ) ;
#43554 = CARTESIAN_POINT ( 'NONE',  ( -6.826472737025120807, 159.9929263765338021, 4.959722759717906548 ) ) ;
#43555 = B_SPLINE_CURVE_WITH_KNOTS ( 'NONE', 3,
 ( #32998, #890, #1618, #65689, #65343, #28371, #39680, #23459, #49188, #66374, #33675, #22434, #49530, #66029 ),
 .UNSPECIFIED., .F., .F.,
 ( 4, 2, 2, 2, 2, 2, 4 ),
 ( 1.226634733346699349E-18, 0.002172676916775652042, 0.003259015375163478497, 0.004345353833551304952, 0.005431692291939130973, 0.006518030750326958729, 0.008690707667102608169 ),
 .UNSPECIFIED. ) ;
#43556 = CARTESIAN_POINT ( 'NONE',  ( -24.21231517720798010, 112.9999999999999858, -9.500000000000000000 ) ) ;
#43557 = VECTOR ( 'NONE', #31280, 1000.000000000000000 ) ;
#43558 = CARTESIAN_POINT ( 'NONE',  ( 36.00000000000002842, 5.000000000000000000, -32.00402776293825724 ) ) ;
#43559 = ORIENTED_EDGE ( 'NONE', *, *, #19549, .T. ) ;
#43560 = ADVANCED_FACE ( 'NONE', ( #40797 ), #27910, .T. ) ;
#43561 = DIRECTION ( 'NONE',  ( -1.000000000000000000, -0.000000000000000000, -0.000000000000000000 ) ) ;
#43562 = ORIENTED_EDGE ( 'NONE', *, *, #63159, .T. ) ;
#43563 = CARTESIAN_POINT ( 'NONE',  ( -165.9570736234661865, 9.058813317711329915, -2.943386871421373119 ) ) ;
#43564 = DIRECTION ( 'NONE',  ( 0.000000000000000000, -1.000000000000000000, -0.000000000000000000 ) ) ;
#43565 = DIRECTION ( 'NONE',  ( 0.000000000000000000, 0.000000000000000000, 1.000000000000000000 ) ) ;
#43566 = EDGE_CURVE ( 'NONE', #38934, #8229, #61497, .T. ) ;
#43567 = DIRECTION ( 'NONE',  ( -0.000000000000000000, 1.000000000000000000, -0.000000000000000000 ) ) ;
#43568 = CARTESIAN_POINT ( 'NONE',  ( -3.648904307674157188, 153.9880311262221824, 8.259051035474737290 ) ) ;
#43569 = ORIENTED_EDGE ( 'NONE', *, *, #9365, .T. ) ;
#43570 = SURFACE_SIDE_STYLE ('',( #1234 ) ) ;
#43571 = DIRECTION ( 'NONE',  ( -1.000000000000000000, 0.000000000000000000, 0.000000000000000000 ) ) ;
#43572 = ORIENTED_EDGE ( 'NONE', *, *, #68830, .F. ) ;
#43573 = SURFACE_STYLE_FILL_AREA ( #546 ) ;
#43574 = EDGE_CURVE ( 'NONE', #52546, #34410, #14482, .T. ) ;
#43575 = CARTESIAN_POINT ( 'NONE',  ( -169.4049999999999727, -2.607480562269069768, 8.024999999999991473 ) ) ;
#43576 = DIRECTION ( 'NONE',  ( 0.000000000000000000, 0.000000000000000000, 1.000000000000000000 ) ) ;
#43577 = CARTESIAN_POINT ( 'NONE',  ( 0.000000000000000000, 87.30187232391182306, 0.000000000000000000 ) ) ;
#43578 = CARTESIAN_POINT ( 'NONE',  ( -177.5950000000000273, 2.607480562269073321, 8.024999999999991473 ) ) ;
#43579 = CARTESIAN_POINT ( 'NONE',  ( -171.2950000000000159, -2.607480562269069768, 8.024999999999991473 ) ) ;
#43580 = ORIENTED_EDGE ( 'NONE', *, *, #33826, .F. ) ;
#43581 =( NAMED_UNIT ( * ) SI_UNIT ( $, .STERADIAN. ) SOLID_ANGLE_UNIT ( ) );
#43582 = CARTESIAN_POINT ( 'NONE',  ( 44.67254323996743182, 10.47540843667325383, 3.522617369932174558 ) ) ;
#43583 = CARTESIAN_POINT ( 'NONE',  ( -49.12162162162162105, 13.70805908423323238, 10.00000000000000000 ) ) ;
#43584 = FILL_AREA_STYLE ('',( #5887 ) ) ;
#43585 = CARTESIAN_POINT ( 'NONE',  ( -78.50499999999996703, -6.826472737025115478, -4.959722759717899443 ) ) ;
#43586 = CARTESIAN_POINT ( 'NONE',  ( 24.70573118280081815, 26.17819722711635677, 27.49997435685320113 ) ) ;
#43587 = LINE ( 'NONE', #43928, #36027 ) ;
#43588 = AXIS2_PLACEMENT_3D ( 'NONE', #61468, #6293, #49225 ) ;
#43589 =( GEOMETRIC_REPRESENTATION_CONTEXT ( 3 ) GLOBAL_UNCERTAINTY_ASSIGNED_CONTEXT ( ( #22791 ) ) GLOBAL_UNIT_ASSIGNED_CONTEXT ( ( #6639, #39064, #43653 ) ) REPRESENTATION_CONTEXT ( 'NONE', 'WORKASPACE' ) );
#43590 = EDGE_CURVE ( 'NONE', #45103, #26681, #60512, .T. ) ;
#43591 = CARTESIAN_POINT ( 'NONE',  ( -84.44499999999999318, 0.000000000000000000, 8.024999999999991473 ) ) ;
#43592 = CARTESIAN_POINT ( 'NONE',  ( 0.000000000000000000, 137.5549999999999784, -9.525000000000000355 ) ) ;
#43593 = COLOUR_RGB ( '', 0.09019608, 0.27058824, 0.51372549) ;
#43594 = CARTESIAN_POINT ( 'NONE',  ( -134.6070736234661638, -8.102448949553174629, 5.886773742842742685 ) ) ;
#43595 = DIRECTION ( 'NONE',  ( -1.000000000000000000, -0.000000000000000000, -0.000000000000000000 ) ) ;
#43596 = DIRECTION ( 'NONE',  ( 1.000000000000000000, 0.000000000000000000, 0.000000000000000000 ) ) ;
#43597 = ORIENTED_EDGE ( 'NONE', *, *, #10768, .F. ) ;
#43598 = CARTESIAN_POINT ( 'NONE',  ( -2.607480562269115509, 132.0929263765338249, -8.024999999999970157 ) ) ;
#43599 =( NAMED_UNIT ( * ) SI_UNIT ( $, .STERADIAN. ) SOLID_ANGLE_UNIT ( ) );
#43600 = STYLED_ITEM ( 'NONE', ( #2915 ), #67510 ) ;
#43601 = COLOUR_RGB ( '', 0.31764706, 0.68627451, 0.89019608) ;
#43602 = FILL_AREA_STYLE ('',( #64310 ) ) ;
#43603 =( NAMED_UNIT ( * ) SI_UNIT ( $, .STERADIAN. ) SOLID_ANGLE_UNIT ( ) );
#43604 = VERTEX_POINT ( 'NONE', #25606 ) ;
#43605 = ORIENTED_EDGE ( 'NONE', *, *, #48109, .T. ) ;
#43606 = CARTESIAN_POINT ( 'NONE',  ( -7.632228543268607446, 135.5429263765338135, -2.479861379858953718 ) ) ;
#43607 = DIRECTION ( 'NONE',  ( -1.000000000000000000, -0.000000000000000000, -0.000000000000000000 ) ) ;
#43608 =( NAMED_UNIT ( * ) PLANE_ANGLE_UNIT ( ) SI_UNIT ( $, .RADIAN. ) );
#43609 = ORIENTED_EDGE ( 'NONE', *, *, #60652, .F. ) ;
#43610 = CARTESIAN_POINT ( 'NONE',  ( -116.3049999999999784, 8.437984349512086979, -1.550032578732815448E-15 ) ) ;
#43611 = VERTEX_POINT ( 'NONE', #10499 ) ;
#43612 =( NAMED_UNIT ( * ) PLANE_ANGLE_UNIT ( ) SI_UNIT ( $, .RADIAN. ) );
#43613 =( NAMED_UNIT ( * ) SI_UNIT ( $, .STERADIAN. ) SOLID_ANGLE_UNIT ( ) );
#43614 = EDGE_LOOP ( 'NONE', ( #60102, #62080, #39062, #23308 ) ) ;
#43615 = CARTESIAN_POINT ( 'NONE',  ( 3.000000000000000444, 3.673940397442059868E-16, 52.50000000000000000 ) ) ;
#43616 = CARTESIAN_POINT ( 'NONE',  ( -60.00000000000000000, -2.024042244987997205E-14, 11.50000000000000000 ) ) ;
#43617 = ORIENTED_EDGE ( 'NONE', *, *, #37933, .F. ) ;
#43618 = LINE ( 'NONE', #66407, #64717 ) ;
#43619 = CARTESIAN_POINT ( 'NONE',  ( 8.102448949553181734, 156.3950000000000102, 5.886773742842750679 ) ) ;
#43620 =( LENGTH_UNIT ( ) NAMED_UNIT ( * ) SI_UNIT ( .MILLI., .METRE. ) );
#43621 = EDGE_LOOP ( 'NONE', ( #6749, #53631, #13633, #69618 ) ) ;
#43622 = ORIENTED_EDGE ( 'NONE', *, *, #24963, .F. ) ;
#43623 = CARTESIAN_POINT ( 'NONE',  ( 30.99999999999999289, 0.000000000000000000, -37.00402776293829277 ) ) ;
#43624 = CARTESIAN_POINT ( 'NONE',  ( -151.8570736234661638, -5.598654528085803328, -7.705886871421366635 ) ) ;
#43625 = CARTESIAN_POINT ( 'NONE',  ( 57.00000000000000000, 14.00000000000000000, -60.00402776293825724 ) ) ;
#43626 = ORIENTED_EDGE ( 'NONE', *, *, #64564, .F. ) ;
#43627 = CARTESIAN_POINT ( 'NONE',  ( 7.632228543268608334, 140.3429263765338249, -2.479861379858951942 ) ) ;
#43628 = CARTESIAN_POINT ( 'NONE',  ( -54.10983016445163685, -9.443832887532138898, -2.000000000000000000 ) ) ;
#43629 = DIRECTION ( 'NONE',  ( -1.000000000000000000, 0.000000000000000000, 0.000000000000000000 ) ) ;
#43630 = VECTOR ( 'NONE', #26537, 1000.000000000000000 ) ;
#43631 = AXIS2_PLACEMENT_3D ( 'NONE', #44612, #17836, #39314 ) ;
#43632 = CARTESIAN_POINT ( 'NONE',  ( -105.2929263765348082, 3.094860106601757366, -9.525000000012106227 ) ) ;
#43633 = ORIENTED_EDGE ( 'NONE', *, *, #52474, .F. ) ;
#43634 = EDGE_CURVE ( 'NONE', #22236, #65737, #10150, .T. ) ;
#43635 = FILL_AREA_STYLE ('',( #32678 ) ) ;
#43636 = ORIENTED_EDGE ( 'NONE', *, *, #16908, .T. ) ;
#43637 = CARTESIAN_POINT ( 'NONE',  ( -49.94292637653380496, 0.000000000000000000, 9.524999999999991473 ) ) ;
#43638 = CARTESIAN_POINT ( 'NONE',  ( 0.000000000000000000, -4.000000000000000000, 7.000000000000001776 ) ) ;
#43639 = FACE_OUTER_BOUND ( 'NONE', #7011, .T. ) ;
#43640 = COLOUR_RGB ( '', 0.66274510, 0.83137255, 0.94901961) ;
#43641 = CARTESIAN_POINT ( 'NONE',  ( -140.7549999999999955, 4.716976649647091513, -6.492361379858946790 ) ) ;
#43642 = SURFACE_SIDE_STYLE ('',( #69631 ) ) ;
#43643 = EDGE_LOOP ( 'NONE', ( #65986, #40056, #67298 ) ) ;
#43644 =( NAMED_UNIT ( * ) SI_UNIT ( $, .STERADIAN. ) SOLID_ANGLE_UNIT ( ) );
#43645 = SURFACE_STYLE_FILL_AREA ( #629 ) ;
#43646 = CARTESIAN_POINT ( 'NONE',  ( 41.05143861928668514, 107.9622656938502416, 3.673005875158968259 ) ) ;
#43647 = ORIENTED_EDGE ( 'NONE', *, *, #3368, .F. ) ;
#43648 = CIRCLE ( 'NONE', #60403, 0.2500000000000002220 ) ;
#43649 = EDGE_CURVE ( 'NONE', #28025, #27009, #42216, .T. ) ;
#43650 = ORIENTED_EDGE ( 'NONE', *, *, #58093, .F. ) ;
#43651 = LINE ( 'NONE', #7012, #47454 ) ;
#43652 = AXIS2_PLACEMENT_3D ( 'NONE', #2332, #29475, #39611 ) ;
#43653 =( NAMED_UNIT ( * ) SI_UNIT ( $, .STERADIAN. ) SOLID_ANGLE_UNIT ( ) );
#43654 = CARTESIAN_POINT ( 'NONE',  ( -61.10499999999997556, -6.826472737025115478, 4.959722759717900331 ) ) ;
#43655 = ORIENTED_EDGE ( 'NONE', *, *, #60110, .T. ) ;
#43656 = DIRECTION ( 'NONE',  ( -0.000000000000000000, -1.000000000000000000, -0.000000000000000000 ) ) ;
#43657 = EDGE_CURVE ( 'NONE', #67877, #60124, #10700, .T. ) ;
#43658 =( NAMED_UNIT ( * ) PLANE_ANGLE_UNIT ( ) SI_UNIT ( $, .RADIAN. ) );
#43659 = CARTESIAN_POINT ( 'NONE',  ( 27.99999999999998934, 5.000000000000000000, 37.00402776293829277 ) ) ;
#43660 = EDGE_CURVE ( 'NONE', #19239, #57600, #58269, .T. ) ;
#43661 = ADVANCED_FACE ( 'NONE', ( #42897, #63937 ), #15449, .T. ) ;
#43662 = LINE ( 'NONE', #38735, #64309 ) ;
#43663 = CARTESIAN_POINT ( 'NONE',  ( -128.6929263765337907, 10.01517768586948698, -1.839758294383808966E-15 ) ) ;
#43664 = EDGE_LOOP ( 'NONE', ( #62877, #62449, #33925, #57310 ) ) ;
#43665 = EDGE_CURVE ( 'NONE', #26930, #6265, #48225, .T. ) ;
#43666 = CARTESIAN_POINT ( 'NONE',  ( 0.000000000000000000, 2.500000000000000000, 0.000000000000000000 ) ) ;
#43667 = CARTESIAN_POINT ( 'NONE',  ( -7.794228634059947147, 2.500000000000000000, -4.500000000000000000 ) ) ;
#43668 = LINE ( 'NONE', #9983, #22455 ) ;
#43669 = LINE ( 'NONE', #60818, #64067 ) ;
#43670 = CARTESIAN_POINT ( 'NONE',  ( -110.3949999999999818, -6.826472737025113702, -4.959722759717900331 ) ) ;
#43671 = CARTESIAN_POINT ( 'NONE',  ( -3.094860106618434248, 111.9050000000000011, 9.525000000000000355 ) ) ;
#43672 = CARTESIAN_POINT ( 'NONE',  ( -90.59499999999999886, 2.607480562269073321, 8.024999999999991473 ) ) ;
#43673 = LINE ( 'NONE', #32721, #5009 ) ;
#43674 = VECTOR ( 'NONE', #28491, 1000.000000000000000 ) ;
#43675 = DIRECTION ( 'NONE',  ( 0.000000000000000000, 0.000000000000000000, -1.000000000000000000 ) ) ;
#43676 = PLANE ( 'NONE',  #25827 ) ;
#43677 =( BOUNDED_CURVE ( )  B_SPLINE_CURVE ( 2, ( #17498, #55789, #56125, #18516, #40003, #61398, #44596, #38971, #13213, #1578, #34669 ),
 .UNSPECIFIED., .F., .F. ) 
 B_SPLINE_CURVE_WITH_KNOTS ( ( 3, 2, 2, 2, 2, 3 ),
 ( 0.3369565217391224943, 0.3391304347826006316, 0.3413043478260788244, 0.3434782608695570172, 0.3456521739130352100, 0.3478260869565133473 ),
 .UNSPECIFIED. ) 
 CURVE ( )  GEOMETRIC_REPRESENTATION_ITEM ( )  RATIONAL_B_SPLINE_CURVE ( ( 1.000000000000178746, 0.9510565162949747853, 1.000000000000000000, 0.9510565162951535312, 1.000000000000000000, 0.9510565162951535312, 1.000000000000000000, 0.9510565162951535312, 1.000000000000000000, 0.9510565162953422691, 0.9999999999998112621 ) ) 
 REPRESENTATION_ITEM ( '' )  );
#43678 = DIRECTION ( 'NONE',  ( 1.224646799147353207E-16, 1.000000000000000000, -0.000000000000000000 ) ) ;
#43679 = VECTOR ( 'NONE', #6538, 1000.000000000000000 ) ;
#43680 = LINE ( 'NONE', #32042, #43838 ) ;
#43681 = ORIENTED_EDGE ( 'NONE', *, *, #6203, .T. ) ;
#43682 = CARTESIAN_POINT ( 'NONE',  ( -121.0429263765337993, -9.058813317711329915, -2.943386871421370898 ) ) ;
#43683 = CARTESIAN_POINT ( 'NONE',  ( -148.4950000000000045, 6.826472737025113702, -4.959722759717902107 ) ) ;
#43684 = DIRECTION ( 'NONE',  ( 1.000000000000000000, -0.000000000000000000, -0.000000000000000000 ) ) ;
#43685 =( GEOMETRIC_REPRESENTATION_CONTEXT ( 3 ) GLOBAL_UNCERTAINTY_ASSIGNED_CONTEXT ( ( #69172 ) ) GLOBAL_UNIT_ASSIGNED_CONTEXT ( ( #20524, #52557, #47667 ) ) REPRESENTATION_CONTEXT ( 'NONE', 'WORKASPACE' ) );
#43686 = CYLINDRICAL_SURFACE ( 'NONE', #1438, 15.00000000000000000 ) ;
#43687 = CARTESIAN_POINT ( 'NONE',  ( -5.196152422706634688, 9.000000000000008882, 7.500000000000000000 ) ) ;
#43688 = ORIENTED_EDGE ( 'NONE', *, *, #57582, .T. ) ;
#43689 = TOROIDAL_SURFACE ( 'NONE', #59379, 1.000000000000000000, 0.5000000000000000000 ) ;
#43690 = ORIENTED_EDGE ( 'NONE', *, *, #69308, .F. ) ;
#43691 = DIRECTION ( 'NONE',  ( -0.000000000000000000, -0.000000000000000000, -1.000000000000000000 ) ) ;
#43692 = FILL_AREA_STYLE_COLOUR ( '', #28535 ) ;
#43693 = MECHANICAL_DESIGN_GEOMETRIC_PRESENTATION_REPRESENTATION (  '', ( #59337 ), #23398 ) ;
#43694 = FACE_OUTER_BOUND ( 'NONE', #32009, .T. ) ;
#43695 = VECTOR ( 'NONE', #69324, 1000.000000000000000 ) ;
#43696 = FILL_AREA_STYLE_COLOUR ( '', #8245 ) ;
#43697 = DIRECTION ( 'NONE',  ( -0.000000000000000000, 1.000000000000000000, -0.000000000000000000 ) ) ;
#43698 = ORIENTED_EDGE ( 'NONE', *, *, #57703, .T. ) ;
#43699 = CARTESIAN_POINT ( 'NONE',  ( -136.8550000000000182, 4.716976649647094177, 6.492361379858945902 ) ) ;
#43700 = ORIENTED_EDGE ( 'NONE', *, *, #23920, .T. ) ;
#43701 = EDGE_LOOP ( 'NONE', ( #3658, #5613, #41548, #8476 ) ) ;
#43702 = SPHERICAL_SURFACE ( 'NONE', #34626, 1.000000000000000000 ) ;
#43703 = DIRECTION ( 'NONE',  ( 0.000000000000000000, 0.000000000000000000, 1.000000000000000000 ) ) ;
#43704 = VERTEX_POINT ( 'NONE', #42539 ) ;
#43705 = FACE_OUTER_BOUND ( 'NONE', #26346, .T. ) ;
#43706 = CARTESIAN_POINT ( 'NONE',  ( -5.598654528085808657, 128.6449999999999818, 7.705886871421373741 ) ) ;
#43707 = FACE_OUTER_BOUND ( 'NONE', #65716, .T. ) ;
#43708 = ORIENTED_EDGE ( 'NONE', *, *, #28814, .F. ) ;
#43709 = SURFACE_STYLE_USAGE ( .BOTH. , #33124 ) ;
#43710 = CARTESIAN_POINT ( 'NONE',  ( -8.102448949553179958, 129.6049999999999613, 5.886773742842747126 ) ) ;
#43711 = CARTESIAN_POINT ( 'NONE',  ( -53.15499999999997982, 7.632228543268600340, 2.479861379858949277 ) ) ;
#43712 = CARTESIAN_POINT ( 'NONE',  ( -119.8449999999999989, -7.632228543268599452, 2.479861379858951054 ) ) ;
#43713 = CARTESIAN_POINT ( 'NONE',  ( -51.84221223720477667, -9.947368421052628307, 4.481646853389226415 ) ) ;
#43714 = VERTEX_POINT ( 'NONE', #4138 ) ;
#43715 = CARTESIAN_POINT ( 'NONE',  ( 0.000000000000000000, 158.5550000000000068, -9.525000000000000355 ) ) ;
#43716 = LINE ( 'NONE', #33469, #49066 ) ;
#43717 = VECTOR ( 'NONE', #2637, 1000.000000000000000 ) ;
#43718 = DIRECTION ( 'NONE',  ( 0.6216216216216174928, 0.7833176619561892373, 0.000000000000000000 ) ) ;
#43719 = EDGE_CURVE ( 'NONE', #5856, #18813, #4834, .T. ) ;
#43720 = TOROIDAL_SURFACE ( 'NONE', #6584, 14.49999999999999822, 0.5000000000000000000 ) ;
#43721 = FILL_AREA_STYLE_COLOUR ( '', #17196 ) ;
#43722 = EDGE_LOOP ( 'NONE', ( #1794, #24138, #25742, #49199 ) ) ;
#43723 = CARTESIAN_POINT ( 'NONE',  ( -33.42999993322085572, -9.448433432980072766, -2.594157102514449420 ) ) ;
#43724 = CARTESIAN_POINT ( 'NONE',  ( -169.1049999999999613, -6.826472737025115478, 4.959722759717900331 ) ) ;
#43725 = ORIENTED_EDGE ( 'NONE', *, *, #35689, .T. ) ;
#43726 = DIRECTION ( 'NONE',  ( 0.000000000000000000, 0.000000000000000000, -1.000000000000000000 ) ) ;
#43727 = ADVANCED_FACE ( 'NONE', ( #28975 ), #22082, .T. ) ;
#43728 = FACE_OUTER_BOUND ( 'NONE', #53013, .T. ) ;
#43729 = CARTESIAN_POINT ( 'NONE',  ( 24.21231517720798010, 112.4999999999999858, -10.00000000000000000 ) ) ;
#43730 = VERTEX_POINT ( 'NONE', #43583 ) ;
#43731 =( GEOMETRIC_REPRESENTATION_CONTEXT ( 3 ) GLOBAL_UNCERTAINTY_ASSIGNED_CONTEXT ( ( #61593 ) ) GLOBAL_UNIT_ASSIGNED_CONTEXT ( ( #26895, #6859, #60323 ) ) REPRESENTATION_CONTEXT ( 'NONE', 'WORKASPACE' ) );
#43732 = VECTOR ( 'NONE', #34878, 1000.000000000000000 ) ;
#43733 = CARTESIAN_POINT ( 'NONE',  ( -45.91547277936962246, 9.430195807687217879, -3.611004237778682402 ) ) ;
#43734 = DIRECTION ( 'NONE',  ( 0.000000000000000000, 1.000000000000000000, -0.000000000000000000 ) ) ;
#43735 = CARTESIAN_POINT ( 'NONE',  ( -89.90499999999998693, 2.607480562269068880, -8.024999999999993250 ) ) ;
#43736 = VERTEX_POINT ( 'NONE', #7545 ) ;
#43737 = DIRECTION ( 'NONE',  ( -0.000000000000000000, -1.000000000000000000, -0.000000000000000000 ) ) ;
#43738 = ADVANCED_FACE ( 'NONE', ( #16829 ), #50813, .T. ) ;
#43739 = CARTESIAN_POINT ( 'NONE',  ( -21.02379604162863913, 110.4999999999999858, -9.500000000000000000 ) ) ;
#43740 = COLOUR_RGB ( '', 0.40784314, 0.44705882, 0.49803922) ;
#43741 = CARTESIAN_POINT ( 'NONE',  ( -60.00000000000000000, -2.024042244987997205E-14, 12.00000000000000000 ) ) ;
#43742 =( NAMED_UNIT ( * ) PLANE_ANGLE_UNIT ( ) SI_UNIT ( $, .RADIAN. ) );
#43743 = CARTESIAN_POINT ( 'NONE',  ( -64.85707362346616378, -5.598654528085803328, -7.705886871421366635 ) ) ;
#43744 = PRESENTATION_LAYER_ASSIGNMENT (  '', '', ( #58305 ) ) ;
#43745 = ADVANCED_FACE ( 'NONE', ( #32614 ), #61671, .T. ) ;
#43746 = CARTESIAN_POINT ( 'NONE',  ( -75.75000000000000000, -4.000000000000000000, 19.00000000000000000 ) ) ;
#43747 = EDGE_LOOP ( 'NONE', ( #36116, #34008, #37030, #66571 ) ) ;
#43748 =( NAMED_UNIT ( * ) PLANE_ANGLE_UNIT ( ) SI_UNIT ( $, .RADIAN. ) );
#43749 = PRESENTATION_LAYER_ASSIGNMENT (  '', '', ( #69505 ) ) ;
#43750 = CARTESIAN_POINT ( 'NONE',  ( -99.80499999999997840, -8.437984349512085203, 5.166775262442717831E-16 ) ) ;
#43751 = CARTESIAN_POINT ( 'NONE',  ( 8.102448949553183510, 132.9949999999999477, -5.886773742842746238 ) ) ;
#43752 = CARTESIAN_POINT ( 'NONE',  ( -119.9949999999999903, -6.826472737025115478, 4.959722759717900331 ) ) ;
#43753 = FACE_OUTER_BOUND ( 'NONE', #7112, .T. ) ;
#43755 = DIRECTION ( 'NONE',  ( -1.000000000000000000, -0.000000000000000000, -0.000000000000000000 ) ) ;
#43754 = PRESENTATION_STYLE_ASSIGNMENT (( #33837 ) ) ;
#43756 = CARTESIAN_POINT ( 'NONE',  ( -152.9929263765337737, 8.102448949553171076, -5.886773742842744461 ) ) ;
#43757 = SURFACE_SIDE_STYLE ('',( #55659 ) ) ;
#43758 = CARTESIAN_POINT ( 'NONE',  ( -180.5949999999999704, 2.607480562269073321, 8.024999999999991473 ) ) ;
#43759 = AXIS2_PLACEMENT_3D ( 'NONE', #49423, #16399, #27226 ) ;
#43760 = DIRECTION ( 'NONE',  ( 0.000000000000000000, 0.000000000000000000, -1.000000000000000000 ) ) ;
#43761 = PRESENTATION_LAYER_ASSIGNMENT (  '', '', ( #65050 ) ) ;
#43762 = PRESENTATION_LAYER_ASSIGNMENT (  '', '', ( #49356 ) ) ;
#43763 = CARTESIAN_POINT ( 'NONE',  ( 7.566679973970428463, 4.894125840469273570, -3.502763581212283073E-15 ) ) ;
#43764 = EDGE_LOOP ( 'NONE', ( #2729, #43899, #22026 ) ) ;
#43765 =( NAMED_UNIT ( * ) PLANE_ANGLE_UNIT ( ) SI_UNIT ( $, .RADIAN. ) );
#43766 = FILL_AREA_STYLE_COLOUR ( '', #27138 ) ;
#43767 = EDGE_LOOP ( 'NONE', ( #23877, #27769, #60783, #65565 ) ) ;
#43768 = CARTESIAN_POINT ( 'NONE',  ( -67.94292637653380496, 0.000000000000000000, 9.524999999999991473 ) ) ;
#43769 = PRESENTATION_LAYER_ASSIGNMENT (  '', '', ( #41660 ) ) ;
#43770 =( BOUNDED_CURVE ( )  B_SPLINE_CURVE ( 2, ( #62028, #39936, #34602, #24063, #57106, #35323, #2905, #8248, #13493, #14211, #61338 ),
 .UNSPECIFIED., .F., .F. ) 
 B_SPLINE_CURVE_WITH_KNOTS ( ( 3, 2, 2, 2, 2, 3 ),
 ( 0.2058823529411763498, 0.2117647058823528272, 0.2176470588235293047, 0.2235294117647058099, 0.2294117647058822596, 0.2352941176470587370 ),
 .UNSPECIFIED. ) 
 CURVE ( )  GEOMETRIC_REPRESENTATION_ITEM ( )  RATIONAL_B_SPLINE_CURVE ( ( 1.000000000000000888, 0.9510565162951526430, 1.000000000000000000, 0.9510565162951535312, 1.000000000000000000, 0.9510565162951535312, 1.000000000000000000, 0.9510565162951535312, 1.000000000000000000, 0.9510565162951541973, 0.9999999999999993339 ) ) 
 REPRESENTATION_ITEM ( '' )  );
#43771 = EDGE_CURVE ( 'NONE', #25571, #47549, #40315, .T. ) ;
#43772 = VECTOR ( 'NONE', #21953, 1000.000000000000000 ) ;
#43773 = DIRECTION ( 'NONE',  ( 0.000000000000000000, 0.000000000000000000, 1.000000000000000000 ) ) ;
#43774 = DIRECTION ( 'NONE',  ( -1.000000000000000000, -0.000000000000000000, 1.300977106640434891E-16 ) ) ;
#43775 = CIRCLE ( 'NONE', #2088, 15.00000000000000000 ) ;
#43776 = CARTESIAN_POINT ( 'NONE',  ( 75.15811388300841145, 19.52565835097472302, 6.000000000000000888 ) ) ;
#43777 = ORIENTED_EDGE ( 'NONE', *, *, #51542, .F. ) ;
#43778 = CARTESIAN_POINT ( 'NONE',  ( -165.8049999999999784, -8.437984349512086979, 5.166775262442717831E-16 ) ) ;
#43779 = VERTEX_POINT ( 'NONE', #24403 ) ;
#43780 =( NAMED_UNIT ( * ) PLANE_ANGLE_UNIT ( ) SI_UNIT ( $, .RADIAN. ) );
#43781 = CARTESIAN_POINT ( 'NONE',  ( -60.00000000000000000, -2.024042244987997205E-14, -12.00000000000000000 ) ) ;
#43782 = SURFACE_STYLE_USAGE ( .BOTH. , #50758 ) ;
#43783 = SPHERICAL_SURFACE ( 'NONE', #59914, 0.2500000000000000000 ) ;
#43784 = CARTESIAN_POINT ( 'NONE',  ( 16.00000000000001776, 15.00000000000000000, -33.68999999999999773 ) ) ;
#43785 =( GEOMETRIC_REPRESENTATION_CONTEXT ( 3 ) GLOBAL_UNCERTAINTY_ASSIGNED_CONTEXT ( ( #10902 ) ) GLOBAL_UNIT_ASSIGNED_CONTEXT ( ( #66272, #49428, #3246 ) ) REPRESENTATION_CONTEXT ( 'NONE', 'WORKASPACE' ) );
#43786 = DIRECTION ( 'NONE',  ( -5.782411586589351722E-16, 1.000000000000000000, 0.000000000000000000 ) ) ;
#43787 = CARTESIAN_POINT ( 'NONE',  ( -2.607480562269073765, 157.2070736234661297, -8.025000000000000355 ) ) ;
#43788 = ORIENTED_EDGE ( 'NONE', *, *, #59447, .F. ) ;
#43789 = SURFACE_STYLE_USAGE ( .BOTH. , #27545 ) ;
#43790 = CARTESIAN_POINT ( 'NONE',  ( -81.20499999999998408, -2.607480562269071545, -8.024999999999991473 ) ) ;
#43791 = DIRECTION ( 'NONE',  ( -0.000000000000000000, -0.000000000000000000, 1.000000000000000000 ) ) ;
#43792 = EDGE_CURVE ( 'NONE', #19502, #14179, #49305, .T. ) ;
#43793 = EDGE_CURVE ( 'NONE', #65002, #37693, #18462, .T. ) ;
#43794 = CARTESIAN_POINT ( 'NONE',  ( -113.9070736234670278, -3.094860106604178096, 9.525000000010345858 ) ) ;
#43795 = VERTEX_POINT ( 'NONE', #40623 ) ;
#43796 = TOROIDAL_SURFACE ( 'NONE', #57259, 4.000000000000000000, 1.000000000000000000 ) ;
#43798 = CARTESIAN_POINT ( 'NONE',  ( -65.09499999999998465, -2.607480562269071545, -8.024999999999991473 ) ) ;
#43797 = PRESENTATION_LAYER_ASSIGNMENT (  '', '', ( #28006 ) ) ;
#43799 = ORIENTED_EDGE ( 'NONE', *, *, #41743, .F. ) ;
#43800 = DIRECTION ( 'NONE',  ( -1.000000000000000000, 0.000000000000000000, 0.000000000000000000 ) ) ;
#43801 = EDGE_CURVE ( 'NONE', #49707, #34861, #23722, .T. ) ;
#43802 = CARTESIAN_POINT ( 'NONE',  ( -45.00000000000000000, 9.609158271987121580, -6.330303435919273802 ) ) ;
#43803 = EDGE_LOOP ( 'NONE', ( #54280, #52279 ) ) ;
#43804 =( NAMED_UNIT ( * ) SI_UNIT ( $, .STERADIAN. ) SOLID_ANGLE_UNIT ( ) );
#43805 = FACE_OUTER_BOUND ( 'NONE', #16646, .T. ) ;
#43806 = ORIENTED_EDGE ( 'NONE', *, *, #4335, .T. ) ;
#43807 = STYLED_ITEM ( 'NONE', ( #28958 ), #42856 ) ;
#43808 = CARTESIAN_POINT ( 'NONE',  ( 45.00000000000000000, 9.916356254361716083, -6.999999999944073181 ) ) ;
#43809 = CARTESIAN_POINT ( 'NONE',  ( -44.99999999999998579, 119.9999999999999716, 7.500000000000000000 ) ) ;
#43810 = CARTESIAN_POINT ( 'NONE',  ( -116.3049999999999784, 8.437984349512085203, -1.550032578732815448E-15 ) ) ;
#43811 = EDGE_LOOP ( 'NONE', ( #21964, #9131, #65838, #46123 ) ) ;
#43812 = LINE ( 'NONE', #22318, #10324 ) ;
#43813 = VECTOR ( 'NONE', #8941, 1000.000000000000000 ) ;
#43814 = EDGE_CURVE ( 'NONE', #27631, #17965, #61345, .T. ) ;
#43815 = CARTESIAN_POINT ( 'NONE',  ( -159.8929263765337794, -8.102448949553174629, -5.886773742842741797 ) ) ;
#43816 = FILL_AREA_STYLE ('',( #22673 ) ) ;
#43817 = DIRECTION ( 'NONE',  ( 0.000000000000000000, 0.000000000000000000, 1.000000000000000000 ) ) ;
#43818 = STYLED_ITEM ( 'NONE', ( #23015 ), #10844 ) ;
#43819 = CARTESIAN_POINT ( 'NONE',  ( -151.4070736234661751, 3.094860106618428031, -9.524999999999993250 ) ) ;
#43820 = PRESENTATION_LAYER_ASSIGNMENT (  '', '', ( #29077 ) ) ;
#43821 = CARTESIAN_POINT ( 'NONE',  ( 5.598654528085809545, 133.1449999999999818, -7.705886871421373741 ) ) ;
#43822 = PRESENTATION_LAYER_ASSIGNMENT (  '', '', ( #65100 ) ) ;
#43823 = CARTESIAN_POINT ( 'NONE',  ( -97.55707362346618083, -1.166476076187852838E-15, -9.524999999999991473 ) ) ;
#43825 = EDGE_CURVE ( 'NONE', #26176, #16496, #39944, .T. ) ;
#43824 =( GEOMETRIC_REPRESENTATION_CONTEXT ( 3 ) GLOBAL_UNCERTAINTY_ASSIGNED_CONTEXT ( ( #48213 ) ) GLOBAL_UNIT_ASSIGNED_CONTEXT ( ( #86, #48396, #58563 ) ) REPRESENTATION_CONTEXT ( 'NONE', 'WORKASPACE' ) );
#43826 =( LENGTH_UNIT ( ) NAMED_UNIT ( * ) SI_UNIT ( .MILLI., .METRE. ) );
#43827 = VERTEX_POINT ( 'NONE', #7887 ) ;
#43828 = MECHANICAL_DESIGN_GEOMETRIC_PRESENTATION_REPRESENTATION (  '', ( #41559 ), #7822 ) ;
#43829 = LINE ( 'NONE', #11776, #13287 ) ;
#43830 = LINE ( 'NONE', #5431, #63567 ) ;
#43831 = CARTESIAN_POINT ( 'NONE',  ( -127.5550000000000068, 0.000000000000000000, 8.024999999999991473 ) ) ;
#43832 = DIRECTION ( 'NONE',  ( -1.000000000000000000, -0.000000000000000000, 1.300977106640434891E-16 ) ) ;
#43833 =( NAMED_UNIT ( * ) SI_UNIT ( $, .STERADIAN. ) SOLID_ANGLE_UNIT ( ) );
#43834 = CARTESIAN_POINT ( 'NONE',  ( -140.6949999999999363, -8.437984349512085203, 5.166775262442717831E-16 ) ) ;
#43835 = CONICAL_SURFACE ( 'NONE', #19064, 6.999999999999997335, 0.7853981633974500554 ) ;
#43836 = CARTESIAN_POINT ( 'NONE',  ( -132.5949999999999989, 2.607480562269072433, 8.024999999999991473 ) ) ;
#43837 = ORIENTED_EDGE ( 'NONE', *, *, #31759, .F. ) ;
#43838 = VECTOR ( 'NONE', #53506, 1000.000000000000000 ) ;
#43839 = PLANE ( 'NONE',  #61668 ) ;
#43840 = FILL_AREA_STYLE_COLOUR ( '', #28913 ) ;
#43841 = UNCERTAINTY_MEASURE_WITH_UNIT (LENGTH_MEASURE( 1.000000000000000082E-05 ), #32162, 'distance_accuracy_value', 'NONE');
#43842 = CARTESIAN_POINT ( 'NONE',  ( -183.1429263765338078, 5.598654528085800663, -7.705886871421367523 ) ) ;
#43843 = FILL_AREA_STYLE ('',( #39603 ) ) ;
#43844 = CARTESIAN_POINT ( 'NONE',  ( -58.34499999999997755, 7.632228543268599452, -2.479861379858951942 ) ) ;
#43845 = CARTESIAN_POINT ( 'NONE',  ( 0.000000000000000000, 30.74999999999999289, 4.000000000000000000 ) ) ;
#43846 = CARTESIAN_POINT ( 'NONE',  ( -178.5570736234661808, -1.166476076187852838E-15, -9.524999999999991473 ) ) ;
#43847 = PRESENTATION_STYLE_ASSIGNMENT (( #27602 ) ) ;
#43848 = PRESENTATION_STYLE_ASSIGNMENT (( #38586 ) ) ;
#43849 =( GEOMETRIC_REPRESENTATION_CONTEXT ( 3 ) GLOBAL_UNCERTAINTY_ASSIGNED_CONTEXT ( ( #6049 ) ) GLOBAL_UNIT_ASSIGNED_CONTEXT ( ( #38544, #59586, #771 ) ) REPRESENTATION_CONTEXT ( 'NONE', 'WORKASPACE' ) );
#43850 = VECTOR ( 'NONE', #61569, 1000.000000000000000 ) ;
#43851 = CARTESIAN_POINT ( 'NONE',  ( -102.8929263765338078, -8.102448949553172852, -5.886773742842741797 ) ) ;
#43852 = DIRECTION ( 'NONE',  ( -1.249000902703301108E-16, 0.8519903597659395089, 0.5235574723618271475 ) ) ;
#43853 = DIRECTION ( 'NONE',  ( 0.000000000000000000, 0.000000000000000000, -1.000000000000000000 ) ) ;
#43854 = CARTESIAN_POINT ( 'NONE',  ( 0.000000000000000000, 111.9999999999999858, 0.000000000000000000 ) ) ;
#43855 = EDGE_CURVE ( 'NONE', #32455, #4040, #557, .T. ) ;
#43856 = VECTOR ( 'NONE', #13079, 1000.000000000000000 ) ;
#43857 = DIRECTION ( 'NONE',  ( 1.000000000000000000, 0.000000000000000000, 0.000000000000000000 ) ) ;
#43858 = FACE_OUTER_BOUND ( 'NONE', #30501, .T. ) ;
#43859 = CARTESIAN_POINT ( 'NONE',  ( 0.000000000000000000, 0.000000000000000000, 0.000000000000000000 ) ) ;
#43860 = ORIENTED_EDGE ( 'NONE', *, *, #3288, .T. ) ;
#43861 = DIRECTION ( 'NONE',  ( -0.000000000000000000, 0.6691306063588591257, -0.7431448254773933559 ) ) ;
#43862 = SPHERICAL_SURFACE ( 'NONE', #41889, 0.2500000000000000000 ) ;
#43863 = MECHANICAL_DESIGN_GEOMETRIC_PRESENTATION_REPRESENTATION (  '', ( #34826 ), #12373 ) ;
#43864 = ORIENTED_EDGE ( 'NONE', *, *, #63932, .F. ) ;
#43865 = CARTESIAN_POINT ( 'NONE',  ( -45.50000000000000711, 9.708372675170615196, 6.000000000000000888 ) ) ;
#43866 = AXIS2_PLACEMENT_3D ( 'NONE', #68234, #3456, #36250 ) ;
#43867 = CARTESIAN_POINT ( 'NONE',  ( 6.826472737025121695, 126.6070736234661638, -4.959722759717905660 ) ) ;
#43868 = PRODUCT_DEFINITION ( 'UNKNOWN', '', #66328, #38924 ) ;
#43869 = EDGE_CURVE ( 'NONE', #32404, #60894, #69512, .T. ) ;
#43871 = CIRCLE ( 'NONE', #21318, 1.000000000000000888 ) ;
#43870 = LINE ( 'NONE', #33280, #56264 ) ;
#43872 = CARTESIAN_POINT ( 'NONE',  ( 4.716976649647096842, 137.8570736234661638, 6.492361379858953896 ) ) ;
#43873 = AXIS2_PLACEMENT_3D ( 'NONE', #3355, #8691, #14667 ) ;
#43874 = ORIENTED_EDGE ( 'NONE', *, *, #13104, .T. ) ;
#43875 = ORIENTED_EDGE ( 'NONE', *, *, #68314, .T. ) ;
#43876 = CARTESIAN_POINT ( 'NONE',  ( 71.49999999999998579, 119.9999999999997868, 7.000000000000000000 ) ) ;
#43877 = EDGE_CURVE ( 'NONE', #37203, #42205, #59406, .T. ) ;
#43878 = FILL_AREA_STYLE_COLOUR ( '', #65296 ) ;
#43879 = ORIENTED_EDGE ( 'NONE', *, *, #48241, .F. ) ;
#43880 = EDGE_CURVE ( 'NONE', #60935, #12490, #7211, .T. ) ;
#43881 = CARTESIAN_POINT ( 'NONE',  ( -8.750000000000001776, 25.24999999999998934, -4.000000000000000000 ) ) ;
#43882 = DIRECTION ( 'NONE',  ( 1.000000000000000000, -0.000000000000000000, 0.000000000000000000 ) ) ;
#43883 = VECTOR ( 'NONE', #67172, 1000.000000000000000 ) ;
#43884 = CARTESIAN_POINT ( 'NONE',  ( 7.632228543268608334, 149.3429263765338249, -2.479861379858951942 ) ) ;
#43885 = CARTESIAN_POINT ( 'NONE',  ( -91.34499999999998465, 7.632228543268599452, -2.479861379858951942 ) ) ;
#43886 = EDGE_LOOP ( 'NONE', ( #27298, #69184, #35651, #34764 ) ) ;
#43887 = STYLED_ITEM ( 'NONE', ( #571 ), #16682 ) ;
#43888 = STYLED_ITEM ( 'NONE', ( #61275 ), #12828 ) ;
#43889 = CARTESIAN_POINT ( 'NONE',  ( 45.00000000000000000, 9.801220280675936536, 6.455927277201578107 ) ) ;
#43890 = EDGE_CURVE ( 'NONE', #25427, #45842, #11169, .T. ) ;
#43891 = ORIENTED_EDGE ( 'NONE', *, *, #63786, .F. ) ;
#43892 = DIRECTION ( 'NONE',  ( 0.000000000000000000, 0.000000000000000000, 1.000000000000000000 ) ) ;
#43893 = DIRECTION ( 'NONE',  ( -0.000000000000000000, -1.000000000000000000, 0.000000000000000000 ) ) ;
#43894 = AXIS2_PLACEMENT_3D ( 'NONE', #30448, #19909, #41765 ) ;
#43895 = EDGE_CURVE ( 'NONE', #60834, #5568, #66645, .T. ) ;
#43896 = DIRECTION ( 'NONE',  ( -5.782411586589351722E-16, -1.000000000000000000, 0.000000000000000000 ) ) ;
#43897 = ORIENTED_EDGE ( 'NONE', *, *, #56861, .F. ) ;
#43898 = SURFACE_STYLE_FILL_AREA ( #17495 ) ;
#43899 = ORIENTED_EDGE ( 'NONE', *, *, #18459, .T. ) ;
#43900 = DIRECTION ( 'NONE',  ( 0.000000000000000000, 0.000000000000000000, 1.000000000000000000 ) ) ;
#43901 = CARTESIAN_POINT ( 'NONE',  ( -13.50000000000000355, 27.99999999999998934, 4.000000000000000000 ) ) ;
#43902 = LINE ( 'NONE', #69543, #15086 ) ;
#43903 = SURFACE_SIDE_STYLE ('',( #48482 ) ) ;
#43904 = CARTESIAN_POINT ( 'NONE',  ( 60.00000000000000000, 1.797044900979284448E-15, 10.00000000000000000 ) ) ;
#43905 = TOROIDAL_SURFACE ( 'NONE', #22528, 4.750000000000000000, 0.2500000000000000000 ) ;
#43906 = CARTESIAN_POINT ( 'NONE',  ( 68.99999999999998579, 1.000000000000008438, 3.000000000000000000 ) ) ;
#43907 = PRESENTATION_STYLE_ASSIGNMENT (( #54738 ) ) ;
#43908 = CARTESIAN_POINT ( 'NONE',  ( -114.8929263765337936, -8.102448949553174629, -5.886773742842741797 ) ) ;
#43909 = ORIENTED_EDGE ( 'NONE', *, *, #58232, .F. ) ;
#43910 = CARTESIAN_POINT ( 'NONE',  ( 48.50000000000000000, 14.49137674618942562, 7.500000000000000000 ) ) ;
#43911 = FILL_AREA_STYLE ('',( #11854 ) ) ;
#43912 = FILL_AREA_STYLE_COLOUR ( '', #41059 ) ;
#43913 = ORIENTED_EDGE ( 'NONE', *, *, #39982, .T. ) ;
#43914 = CARTESIAN_POINT ( 'NONE',  ( -158.3049999999999500, 8.437984349512085203, -1.550032578732815448E-15 ) ) ;
#43915 = CARTESIAN_POINT ( 'NONE',  ( -22.75000000000000711, 36.75000000000000000, -4.000000000000000000 ) ) ;
#43916 = CARTESIAN_POINT ( 'NONE',  ( -183.8457661644624750, -8.375912622596889179, -2.295903050784204869 ) ) ;
#43917 = MECHANICAL_DESIGN_GEOMETRIC_PRESENTATION_REPRESENTATION (  '', ( #29294 ), #4540 ) ;
#43918 = CARTESIAN_POINT ( 'NONE',  ( -174.7449999999999761, 4.716976649647094177, 6.492361379858945902 ) ) ;
#43919 = CARTESIAN_POINT ( 'NONE',  ( -161.9950000000000045, -6.826472737025113702, 4.959722759717902107 ) ) ;
#43920 = EDGE_CURVE ( 'NONE', #24250, #41177, #24073, .T. ) ;
#43921 = EDGE_LOOP ( 'NONE', ( #16250, #48665, #2769, #42359 ) ) ;
#43922 = CYLINDRICAL_SURFACE ( 'NONE', #30192, 8.025000000000000355 ) ;
#43923 = FACE_OUTER_BOUND ( 'NONE', #42740, .T. ) ;
#43924 =( LENGTH_UNIT ( ) NAMED_UNIT ( * ) SI_UNIT ( .MILLI., .METRE. ) );
#43925 = CARTESIAN_POINT ( 'NONE',  ( -85.70499999999999829, 2.607480562269073321, 8.024999999999991473 ) ) ;
#43926 = CARTESIAN_POINT ( 'NONE',  ( 24.50471495965034308, 26.85083734004840750, 27.39802421297251200 ) ) ;
#43927 = AXIS2_PLACEMENT_3D ( 'NONE', #69433, #42407, #36774 ) ;
#43928 = CARTESIAN_POINT ( 'NONE',  ( -22.75000000000000711, 34.24999999999999289, -4.000000000000000000 ) ) ;
#43929 = CARTESIAN_POINT ( 'NONE',  ( -82.64499999999998181, 4.716976649647091513, -6.492361379858946790 ) ) ;
#43930 = CARTESIAN_POINT ( 'NONE',  ( 8.102448949553183510, 140.1049999999999898, -5.886773742842746238 ) ) ;
#43931 = STYLED_ITEM ( 'NONE', ( #15870 ), #17692 ) ;
#43932 = UNCERTAINTY_MEASURE_WITH_UNIT (LENGTH_MEASURE( 1.000000000000000082E-05 ), #17754, 'distance_accuracy_value', 'NONE');
#43933 = VECTOR ( 'NONE', #6500, 1000.000000000000000 ) ;
#43935 = CARTESIAN_POINT ( 'NONE',  ( -24.21231517720798010, 112.4999999999999858, 9.500000000000000000 ) ) ;
#43934 =( GEOMETRIC_REPRESENTATION_CONTEXT ( 3 ) GLOBAL_UNCERTAINTY_ASSIGNED_CONTEXT ( ( #130 ) ) GLOBAL_UNIT_ASSIGNED_CONTEXT ( ( #4411, #2389, #57566 ) ) REPRESENTATION_CONTEXT ( 'NONE', 'WORKASPACE' ) );
#43936 = CARTESIAN_POINT ( 'NONE',  ( 25.75000000000001066, 19.24999999999997868, 4.000000000000000000 ) ) ;
#43937 = ORIENTED_EDGE ( 'NONE', *, *, #44287, .F. ) ;
#43938 = FACE_OUTER_BOUND ( 'NONE', #29627, .T. ) ;
#43939 = COLOUR_RGB ( '', 0.40784314, 0.44705882, 0.49803922) ;
#43940 = ADVANCED_FACE ( 'NONE', ( #66995 ), #29119, .T. ) ;
#43941 = DIRECTION ( 'NONE',  ( 1.000000000000000000, 0.000000000000000000, 0.000000000000000000 ) ) ;
#43942 = CARTESIAN_POINT ( 'NONE',  ( -6.826472737025120807, 136.5070736234661410, -4.959722759717907437 ) ) ;
#43943 = ORIENTED_EDGE ( 'NONE', *, *, #32023, .F. ) ;
#43944 = ORIENTED_EDGE ( 'NONE', *, *, #16019, .F. ) ;
#43945 = CARTESIAN_POINT ( 'NONE',  ( -2.607480562268991608, 136.2929263765338135, 8.025000000000060751 ) ) ;
#43946 = FILL_AREA_STYLE_COLOUR ( '', #61123 ) ;
#43947 = AXIS2_PLACEMENT_3D ( 'NONE', #41612, #10281, #63029 ) ;
#43948 = EDGE_CURVE ( 'NONE', #1567, #39120, #18988, .T. ) ;
#43949 =( GEOMETRIC_REPRESENTATION_CONTEXT ( 3 ) GLOBAL_UNCERTAINTY_ASSIGNED_CONTEXT ( ( #45471 ) ) GLOBAL_UNIT_ASSIGNED_CONTEXT ( ( #34102, #32710, #54166 ) ) REPRESENTATION_CONTEXT ( 'NONE', 'WORKASPACE' ) );
#43950 =( LENGTH_UNIT ( ) NAMED_UNIT ( * ) SI_UNIT ( .MILLI., .METRE. ) );
#43951 = PRESENTATION_STYLE_ASSIGNMENT (( #65709 ) ) ;
#43952 = CARTESIAN_POINT ( 'NONE',  ( 13.50000000000000355, 27.74999999999998934, -3.750000000000000000 ) ) ;
#43953 = CARTESIAN_POINT ( 'NONE',  ( -70.40707362346617515, 3.094860106618428031, -9.524999999999993250 ) ) ;
#43954 = ORIENTED_EDGE ( 'NONE', *, *, #17795, .F. ) ;
#43955 = AXIS2_PLACEMENT_3D ( 'NONE', #67506, #57655, #30906 ) ;
#43956 = CARTESIAN_POINT ( 'NONE',  ( -113.4549999999999841, 7.632228543268599452, -2.479861379858951942 ) ) ;
#43957 = ORIENTED_EDGE ( 'NONE', *, *, #36890, .F. ) ;
#43958 =( LENGTH_UNIT ( ) NAMED_UNIT ( * ) SI_UNIT ( .MILLI., .METRE. ) );
#43959 = EDGE_CURVE ( 'NONE', #69341, #41724, #20531, .T. ) ;
#43960 = VERTEX_POINT ( 'NONE', #47309 ) ;
#43961 =( LENGTH_UNIT ( ) NAMED_UNIT ( * ) SI_UNIT ( .MILLI., .METRE. ) );
#43962 = CARTESIAN_POINT ( 'NONE',  ( -68.60707362346616378, -8.102448949553174629, 5.886773742842742685 ) ) ;
#43963 = ORIENTED_EDGE ( 'NONE', *, *, #64526, .F. ) ;
#43964 = CARTESIAN_POINT ( 'NONE',  ( 0.000000000000000000, 0.000000000000000000, 0.000000000000000000 ) ) ;
#43965 = PRESENTATION_LAYER_ASSIGNMENT (  '', '', ( #4600 ) ) ;
#43966 = CARTESIAN_POINT ( 'NONE',  ( 3.094860106618435136, 157.2949999999999591, -9.525000000000000355 ) ) ;
#43967 = DIRECTION ( 'NONE',  ( -1.000000000000000000, 0.000000000000000000, 0.000000000000000000 ) ) ;
#43968 = ORIENTED_EDGE ( 'NONE', *, *, #53556, .T. ) ;
#43969 = AXIS2_PLACEMENT_3D ( 'NONE', #28740, #29439, #66035 ) ;
#43970 = VERTEX_POINT ( 'NONE', #63089 ) ;
#43971 = CYLINDRICAL_SURFACE ( 'NONE', #6330, 9.524999999999991473 ) ;
#43972 = FACE_OUTER_BOUND ( 'NONE', #48144, .T. ) ;
#43973 = DIRECTION ( 'NONE',  ( -0.000000000000000000, -0.000000000000000000, -1.000000000000000000 ) ) ;
#43974 = EDGE_LOOP ( 'NONE', ( #39692, #59738, #21717, #9786 ) ) ;
#43975 = CARTESIAN_POINT ( 'NONE',  ( -6.826472737025120807, 135.3929263765338362, -4.959722759717907437 ) ) ;
#43976 = DIRECTION ( 'NONE',  ( -0.000000000000000000, -0.000000000000000000, 1.000000000000000000 ) ) ;
#43977 = DIRECTION ( 'NONE',  ( -1.000000000000000000, -0.000000000000000000, -0.000000000000000000 ) ) ;
#43978 = AXIS2_PLACEMENT_3D ( 'NONE', #8370, #51607, #3366 ) ;
#43979 = ADVANCED_FACE ( 'NONE', ( #9656 ), #69081, .T. ) ;
#43980 = DIRECTION ( 'NONE',  ( 0.000000000000000000, 0.000000000000000000, 1.000000000000000000 ) ) ;
#43981 = ORIENTED_EDGE ( 'NONE', *, *, #53310, .T. ) ;
#43982 = VECTOR ( 'NONE', #22058, 1000.000000000000000 ) ;
#43983 = ORIENTED_EDGE ( 'NONE', *, *, #7449, .F. ) ;
#43984 = CARTESIAN_POINT ( 'NONE',  ( -48.74292637653379501, -5.598654528085803328, -7.705886871421366635 ) ) ;
#43985 = CARTESIAN_POINT ( 'NONE',  ( 15.48999599679679662, 146.4999999999999716, -9.500000000000000000 ) ) ;
#43986 = DIRECTION ( 'NONE',  ( 0.000000000000000000, 0.000000000000000000, 1.000000000000000000 ) ) ;
#43987 = CARTESIAN_POINT ( 'NONE',  ( -145.2549999999999955, -4.716976649647092401, 6.492361379858946790 ) ) ;
#43988 = CARTESIAN_POINT ( 'NONE',  ( -7.566679973970432016, -2.499999999999994671, -4.894125840469273570 ) ) ;
#43989 = LINE ( 'NONE', #11936, #23806 ) ;
#43990 = UNCERTAINTY_MEASURE_WITH_UNIT (LENGTH_MEASURE( 1.000000000000000082E-05 ), #58330, 'distance_accuracy_value', 'NONE');
#43991 = ORIENTED_EDGE ( 'NONE', *, *, #19312, .T. ) ;
#43992 = PRESENTATION_LAYER_ASSIGNMENT (  '', '', ( #4616 ) ) ;
#43993 = CARTESIAN_POINT ( 'NONE',  ( -6.826472737025120807, 115.5070736234661553, -4.959722759717907437 ) ) ;
#43994 = CARTESIAN_POINT ( 'NONE',  ( 10.00000000000001776, 17.78868675966041835, -5.824939844684579265E-16 ) ) ;
#43995 = DIRECTION ( 'NONE',  ( 0.000000000000000000, 0.000000000000000000, 1.000000000000000000 ) ) ;
#43996 = B_SPLINE_CURVE_WITH_KNOTS ( 'NONE', 3,
 ( #52189, #58144, #40948, #19448, #15591, #68014, #57444, #14900 ),
 .UNSPECIFIED., .F., .F.,
 ( 4, 2, 2, 4 ),
 ( 0.000000000000000000, 0.0004249208466734696334, 0.0008498416933469392668, 0.001699683386693891327 ),
 .UNSPECIFIED. ) ;
#43997 = ORIENTED_EDGE ( 'NONE', *, *, #27065, .F. ) ;
#43998 = PRESENTATION_LAYER_ASSIGNMENT (  '', '', ( #52952 ) ) ;
#43999 =( GEOMETRIC_REPRESENTATION_CONTEXT ( 3 ) GLOBAL_UNCERTAINTY_ASSIGNED_CONTEXT ( ( #35637 ) ) GLOBAL_UNIT_ASSIGNED_CONTEXT ( ( #55967, #67220, #45117 ) ) REPRESENTATION_CONTEXT ( 'NONE', 'WORKASPACE' ) );
#44000 = VERTEX_POINT ( 'NONE', #52900 ) ;
#44001 = CARTESIAN_POINT ( 'NONE',  ( -45.91409082377983708, 9.428132016590232922, 3.509142856994616810 ) ) ;
#44002 = CARTESIAN_POINT ( 'NONE',  ( -51.20707362346615099, 3.094860106618433360, 9.524999999999991473 ) ) ;
#44003 = CARTESIAN_POINT ( 'NONE',  ( -52.40499999999998693, -2.607480562269069768, 8.024999999999991473 ) ) ;
#44004 = ORIENTED_EDGE ( 'NONE', *, *, #57916, .T. ) ;
#44005 = SURFACE_SIDE_STYLE ('',( #28084 ) ) ;
#44006 = DIRECTION ( 'NONE',  ( -1.000000000000000000, 0.000000000000000000, -0.000000000000000000 ) ) ;
#44007 = DIRECTION ( 'NONE',  ( 0.000000000000000000, 0.000000000000000000, -1.000000000000000000 ) ) ;
#44008 = DIRECTION ( 'NONE',  ( 0.000000000000000000, 0.000000000000000000, 1.000000000000000000 ) ) ;
#44009 = CARTESIAN_POINT ( 'NONE',  ( 15.98999599679679839, 118.4999999999999716, 7.500000000000000000 ) ) ;
#44010 = EDGE_CURVE ( 'NONE', #60379, #41992, #68820, .T. ) ;
#44011 = CARTESIAN_POINT ( 'NONE',  ( -129.1429263765338078, 5.598654528085800663, -7.705886871421367523 ) ) ;
#44012 = ORIENTED_EDGE ( 'NONE', *, *, #36605, .T. ) ;
#44013 = VECTOR ( 'NONE', #34650, 1000.000000000000000 ) ;
#44014 = PRESENTATION_LAYER_ASSIGNMENT (  '', '', ( #65298 ) ) ;
#44015 = LINE ( 'NONE', #6656, #51656 ) ;
#44016 = LINE ( 'NONE', #65427, #27004 ) ;
#44017 = DIRECTION ( 'NONE',  ( -0.000000000000000000, -1.000000000000000000, -0.000000000000000000 ) ) ;
#44018 = CARTESIAN_POINT ( 'NONE',  ( -9.827790563157511022E-16, 112.4429263765338192, 8.025000000000000355 ) ) ;
#44019 = CIRCLE ( 'NONE', #1218, 5.500000000000001776 ) ;
#44020 = CARTESIAN_POINT ( 'NONE',  ( -105.2949999999999875, -2.607480562269069768, 8.024999999999991473 ) ) ;
#44021 = CARTESIAN_POINT ( 'NONE',  ( 8.102448949553183510, 159.9950000000000330, -5.886773742842746238 ) ) ;
#44022 = CARTESIAN_POINT ( 'NONE',  ( -77.84499999999998465, -7.632228543268599452, 2.479861379858951054 ) ) ;
#44023 = CIRCLE ( 'NONE', #60825, 0.5000000000000004441 ) ;
#44024 = CYLINDRICAL_SURFACE ( 'NONE', #49977, 0.2500000000000002220 ) ;
#44025 = CARTESIAN_POINT ( 'NONE',  ( 0.000000000000000000, 140.9429263765338192, -8.025000000000000355 ) ) ;
#44026 = DIRECTION ( 'NONE',  ( -0.000000000000000000, 1.000000000000000000, -0.000000000000000000 ) ) ;
#44027 = VECTOR ( 'NONE', #15328, 1000.000000000000000 ) ;
#44028 = DIRECTION ( 'NONE',  ( 0.000000000000000000, 0.000000000000000000, 1.000000000000000000 ) ) ;
#44029 = UNCERTAINTY_MEASURE_WITH_UNIT (LENGTH_MEASURE( 1.000000000000000082E-05 ), #14697, 'distance_accuracy_value', 'NONE');
#44030 =( LENGTH_UNIT ( ) NAMED_UNIT ( * ) SI_UNIT ( .MILLI., .METRE. ) );
#44031 = ORIENTED_EDGE ( 'NONE', *, *, #43880, .F. ) ;
#44032 = CARTESIAN_POINT ( 'NONE',  ( -122.2429263765338021, 5.598654528085804216, 7.705886871421366635 ) ) ;
#44033 = FILL_AREA_STYLE ('',( #16928 ) ) ;
#44034 = CARTESIAN_POINT ( 'NONE',  ( -149.5449999999999875, -7.632228543268600340, -2.479861379858950166 ) ) ;
#44035 = PRESENTATION_LAYER_ASSIGNMENT (  '', '', ( #57495 ) ) ;
#44036 = EDGE_CURVE ( 'NONE', #15405, #52477, #62723, .T. ) ;
#44037 = CYLINDRICAL_SURFACE ( 'NONE', #67786, 8.025000000000000355 ) ;
#44038 = FILL_AREA_STYLE ('',( #22536 ) ) ;
#44039 = VERTEX_POINT ( 'NONE', #52565 ) ;
#44040 = EDGE_LOOP ( 'NONE', ( #49820, #10256, #67091, #51883 ) ) ;
#44041 = DIRECTION ( 'NONE',  ( -1.000000000000000000, 0.000000000000000000, 0.000000000000000000 ) ) ;
#44042 = STYLED_ITEM ( 'NONE', ( #57978 ), #25220 ) ;
#44043 = DIRECTION ( 'NONE',  ( -0.000000000000000000, -0.000000000000000000, 1.000000000000000000 ) ) ;
#44044 = FILL_AREA_STYLE_COLOUR ( '', #37101 ) ;
#44045 = CIRCLE ( 'NONE', #137, 0.9999999999999986677 ) ;
#44046 = CARTESIAN_POINT ( 'NONE',  ( -116.8429263765338106, 9.058813317711329915, -2.943386871421373119 ) ) ;
#44047 = CARTESIAN_POINT ( 'NONE',  ( -195.0000000000000000, 0.000000000000000000, 9.524999999999991473 ) ) ;
#44048 = ORIENTED_EDGE ( 'NONE', *, *, #30154, .F. ) ;
#44049 = CARTESIAN_POINT ( 'NONE',  ( -141.8050000000000068, -8.437984349512086979, 5.166775262442717831E-16 ) ) ;
#44050 = ORIENTED_EDGE ( 'NONE', *, *, #20591, .T. ) ;
#44051 = EDGE_CURVE ( 'NONE', #69365, #22057, #26140, .T. ) ;
#44052 = VERTEX_POINT ( 'NONE', #58172 ) ;
#44053 = CARTESIAN_POINT ( 'NONE',  ( -15.00000000000000000, 8.000000000000000000, -3.500000000000017764 ) ) ;
#44054 = DIRECTION ( 'NONE',  ( 0.000000000000000000, 0.000000000000000000, 1.000000000000000000 ) ) ;
#44055 = ORIENTED_EDGE ( 'NONE', *, *, #62089, .F. ) ;
#44056 = AXIS2_PLACEMENT_3D ( 'NONE', #24256, #28832, #8088 ) ;
#44057 = CARTESIAN_POINT ( 'NONE',  ( 57.00000000000000000, 14.00000000000000000, -72.50402776293826435 ) ) ;
#44058 = ADVANCED_FACE ( 'NONE', ( #42386 ), #3982, .F. ) ;
#44059 = CARTESIAN_POINT ( 'NONE',  ( -3.094860106618432471, 127.5949999999999847, -9.525000000000000355 ) ) ;
#44060 = CYLINDRICAL_SURFACE ( 'NONE', #43023, 4.999999999999997335 ) ;
#44061 = ORIENTED_EDGE ( 'NONE', *, *, #43814, .F. ) ;
#44062 = CIRCLE ( 'NONE', #19289, 0.5000000000000004441 ) ;
#44063 = CARTESIAN_POINT ( 'NONE',  ( -21.02379604162863913, 114.4999999999999574, 10.50000000000000000 ) ) ;
#44065 = ADVANCED_FACE ( 'NONE', ( #42727 ), #43079, .F. ) ;
#44064 = CARTESIAN_POINT ( 'NONE',  ( -8.102448949553179958, 132.0049999999999670, -5.886773742842749790 ) ) ;
#44066 = CARTESIAN_POINT ( 'NONE',  ( -54.50499999999998835, -6.826472737025113702, -4.959722759717900331 ) ) ;
#44067 = CARTESIAN_POINT ( 'NONE',  ( -41.13967244528112133, 107.8968002066633431, -3.376844662570002598 ) ) ;
#44068 = VERTEX_POINT ( 'NONE', #65156 ) ;
#44069 = CARTESIAN_POINT ( 'NONE',  ( -5.598654528085808657, 153.7549999999999670, 7.705886871421373741 ) ) ;
#44070 = CARTESIAN_POINT ( 'NONE',  ( 0.000000000000000000, -2.500000000000000000, 0.000000000000000000 ) ) ;
#44071 = UNCERTAINTY_MEASURE_WITH_UNIT (LENGTH_MEASURE( 1.000000000000000082E-05 ), #62098, 'distance_accuracy_value', 'NONE');
#44072 = FILL_AREA_STYLE ('',( #54892 ) ) ;
#44073 = VECTOR ( 'NONE', #36668, 1000.000000000000000 ) ;
#44074 = EDGE_CURVE ( 'NONE', #68774, #23185, #48268, .T. ) ;
#44075 = FILL_AREA_STYLE_COLOUR ( '', #7005 ) ;
#44076 = ORIENTED_EDGE ( 'NONE', *, *, #28569, .T. ) ;
#44077 = MECHANICAL_DESIGN_GEOMETRIC_PRESENTATION_REPRESENTATION (  '', ( #19303 ), #48592 ) ;
#44078 = DIRECTION ( 'NONE',  ( 1.000000000000000000, 0.000000000000000000, 0.000000000000000000 ) ) ;
#44079 = ORIENTED_EDGE ( 'NONE', *, *, #60170, .F. ) ;
#44080 = DIRECTION ( 'NONE',  ( 0.000000000000000000, 1.000000000000000000, -0.000000000000000000 ) ) ;
#44081 = CARTESIAN_POINT ( 'NONE',  ( -167.6050000000000182, 6.826472737025113702, -4.959722759717902107 ) ) ;
#44083 = ORIENTED_EDGE ( 'NONE', *, *, #54774, .T. ) ;
#44082 = AXIS2_PLACEMENT_3D ( 'NONE', #55154, #55861, #6984 ) ;
#44084 = DIRECTION ( 'NONE',  ( 0.000000000000000000, 1.000000000000000000, -0.000000000000000000 ) ) ;
#44085 = UNCERTAINTY_MEASURE_WITH_UNIT (LENGTH_MEASURE( 1.000000000000000082E-05 ), #48135, 'distance_accuracy_value', 'NONE');
#44086 = AXIS2_PLACEMENT_3D ( 'NONE', #19346, #14093, #52091 ) ;
#44087 = DIRECTION ( 'NONE',  ( 0.000000000000000000, 1.000000000000000000, 0.000000000000000000 ) ) ;
#44088 = SURFACE_SIDE_STYLE ('',( #6389 ) ) ;
#44089 = CARTESIAN_POINT ( 'NONE',  ( -102.0570736234661808, 0.000000000000000000, 9.524999999999991473 ) ) ;
#44090 = CARTESIAN_POINT ( 'NONE',  ( -78.29292637653377085, 3.094860106618428031, -9.524999999999993250 ) ) ;
#44091 = CIRCLE ( 'NONE', #37362, 0.2500000000000002220 ) ;
#44092 = EDGE_LOOP ( 'NONE', ( #5484, #12575, #18528, #14775 ) ) ;
#44093 = PLANE ( 'NONE',  #52988 ) ;
#44094 = CARTESIAN_POINT ( 'NONE',  ( -7.342319042881618962, 2.499999999999994671, 5.282730372348551029 ) ) ;
#44095 = CARTESIAN_POINT ( 'NONE',  ( -85.55499999999999261, 0.000000000000000000, 8.024999999999991473 ) ) ;
#44096 = ORIENTED_EDGE ( 'NONE', *, *, #26932, .F. ) ;
#44097 = SURFACE_STYLE_FILL_AREA ( #65140 ) ;
#44098 = COLOUR_RGB ( '', 0.31764706, 0.68627451, 0.89019608) ;
#44099 =( BOUNDED_CURVE ( )  B_SPLINE_CURVE ( 3, ( #58415, #43342, #30982, #42982 ),
 .UNSPECIFIED., .F., .F. ) 
 B_SPLINE_CURVE_WITH_KNOTS ( ( 4, 4 ),
 ( 3.043785426622117374, 4.712388980384689674 ),
 .UNSPECIFIED. ) 
 CURVE ( )  GEOMETRIC_REPRESENTATION_ITEM ( )  RATIONAL_B_SPLINE_CURVE ( ( 1.000000000000000000, 0.7811300729168891843, 0.7811300729168891843, 1.000000000000000000 ) ) 
 REPRESENTATION_ITEM ( '' )  );
#44100 =( NAMED_UNIT ( * ) PLANE_ANGLE_UNIT ( ) SI_UNIT ( $, .RADIAN. ) );
#44101 = SPHERICAL_SURFACE ( 'NONE', #25210, 0.5000000000000000000 ) ;
#44102 = CARTESIAN_POINT ( 'NONE',  ( -53.15707362346616804, -9.058813317711329915, -2.943386871421370898 ) ) ;
#44103 = AXIS2_PLACEMENT_3D ( 'NONE', #49412, #63583, #1495 ) ;
#44104 = SURFACE_STYLE_USAGE ( .BOTH. , #22600 ) ;
#44105 = ORIENTED_EDGE ( 'NONE', *, *, #60971, .T. ) ;
#44106 = DIRECTION ( 'NONE',  ( 0.000000000000000000, 0.000000000000000000, 1.000000000000000000 ) ) ;
#44107 = VECTOR ( 'NONE', #45543, 1000.000000000000000 ) ;
#44108 = SURFACE_STYLE_FILL_AREA ( #55986 ) ;
#44109 = CARTESIAN_POINT ( 'NONE',  ( -104.0049999999999812, 6.826472737025116366, 4.959722759717898555 ) ) ;
#44110 = CARTESIAN_POINT ( 'NONE',  ( 8.102448949553181734, 126.3949999999999818, 5.886773742842750679 ) ) ;
#44111 = CARTESIAN_POINT ( 'NONE',  ( -115.4949999999999903, 6.826472737025113702, -4.959722759717902107 ) ) ;
#44112 =( GEOMETRIC_REPRESENTATION_CONTEXT ( 3 ) GLOBAL_UNCERTAINTY_ASSIGNED_CONTEXT ( ( #26987 ) ) GLOBAL_UNIT_ASSIGNED_CONTEXT ( ( #22106, #27692, #64314 ) ) REPRESENTATION_CONTEXT ( 'NONE', 'WORKASPACE' ) );
#44113 = FILL_AREA_STYLE_COLOUR ( '', #15716 ) ;
#44115 = CARTESIAN_POINT ( 'NONE',  ( -17.64912285177511819, 11.22500550600073588, -4.243648409907320840 ) ) ;
#44114 = DIRECTION ( 'NONE',  ( 1.000000000000000000, -0.000000000000000000, 0.000000000000000000 ) ) ;
#44116 = CARTESIAN_POINT ( 'NONE',  ( -152.3929263765338078, 8.102448949553176405, 5.886773742842740909 ) ) ;
#44117 = CARTESIAN_POINT ( 'NONE',  ( -179.5450000000000159, -7.632228543268600340, -2.479861379858950166 ) ) ;
#44118 = DIRECTION ( 'NONE',  ( 1.000000000000000000, -0.000000000000000000, -1.300977106640434891E-16 ) ) ;
#44119 = STYLED_ITEM ( 'NONE', ( #47621 ), #22638 ) ;
#44120 = EDGE_CURVE ( 'NONE', #3393, #45684, #4413, .T. ) ;
#44121 = CARTESIAN_POINT ( 'NONE',  ( -43.26576733027980026, -14.00568869182241016, 2.673603619738250892 ) ) ;
#44122 = ORIENTED_EDGE ( 'NONE', *, *, #462, .F. ) ;
#44123 = DIRECTION ( 'NONE',  ( 0.000000000000000000, 0.000000000000000000, -1.000000000000000000 ) ) ;
#44124 = VERTEX_POINT ( 'NONE', #64484 ) ;
#44125 = CARTESIAN_POINT ( 'NONE',  ( -70.19292637653380496, -10.01517768586948698, 6.132527647946031529E-16 ) ) ;
#44127 = EDGE_CURVE ( 'NONE', #30006, #17294, #54606, .T. ) ;
#44126 = PRESENTATION_STYLE_ASSIGNMENT (( #1446 ) ) ;
#44128 = STYLED_ITEM ( 'NONE', ( #21968 ), #54665 ) ;
#44129 = ADVANCED_FACE ( 'NONE', ( #43753 ), #27844, .F. ) ;
#44130 = CARTESIAN_POINT ( 'NONE',  ( 86.21825843581743243, 5.000000000000000000, -39.83014742847162637 ) ) ;
#44131 = SURFACE_STYLE_USAGE ( .BOTH. , #22628 ) ;
#44132 = DIRECTION ( 'NONE',  ( 0.000000000000000000, 0.000000000000000000, 1.000000000000000000 ) ) ;
#44133 = EDGE_CURVE ( 'NONE', #60291, #22530, #15977, .T. ) ;
#44134 = DIRECTION ( 'NONE',  ( -1.000000000000000000, 0.000000000000000000, 0.000000000000000000 ) ) ;
#44135 = ORIENTED_EDGE ( 'NONE', *, *, #55760, .F. ) ;
#44136 = CARTESIAN_POINT ( 'NONE',  ( -167.3049999999999784, 8.437984349512086979, -1.550032578732815448E-15 ) ) ;
#44137 = ADVANCED_FACE ( 'NONE', ( #58862 ), #37806, .T. ) ;
#44138 = ORIENTED_EDGE ( 'NONE', *, *, #65850, .F. ) ;
#44139 = VECTOR ( 'NONE', #67064, 1000.000000000000000 ) ;
#44140 = CARTESIAN_POINT ( 'NONE',  ( 4.250000000000001776, 21.74999999999998579, -4.000000000000000000 ) ) ;
#44141 =( NAMED_UNIT ( * ) PLANE_ANGLE_UNIT ( ) SI_UNIT ( $, .RADIAN. ) );
#44143 = EDGE_CURVE ( 'NONE', #35442, #29587, #53907, .T. ) ;
#44142 = DIRECTION ( 'NONE',  ( -0.000000000000000000, -1.000000000000000000, 0.000000000000000000 ) ) ;
#44144 =( NAMED_UNIT ( * ) SI_UNIT ( $, .STERADIAN. ) SOLID_ANGLE_UNIT ( ) );
#44145 = CARTESIAN_POINT ( 'NONE',  ( -6.826472737025120807, 151.5070736234661979, -4.959722759717907437 ) ) ;
#44146 = AXIS2_PLACEMENT_3D ( 'NONE', #53892, #49331, #37441 ) ;
#44147 = ORIENTED_EDGE ( 'NONE', *, *, #59279, .F. ) ;
#44149 = EDGE_CURVE ( 'NONE', #31454, #42659, #22422, .T. ) ;
#44148 = FACE_OUTER_BOUND ( 'NONE', #65286, .T. ) ;
#44150 = CARTESIAN_POINT ( 'NONE',  ( -79.40499999999998693, -2.607480562269069768, 8.024999999999991473 ) ) ;
#44151 = UNCERTAINTY_MEASURE_WITH_UNIT (LENGTH_MEASURE( 1.000000000000000082E-05 ), #5018, 'distance_accuracy_value', 'NONE');
#44152 = CARTESIAN_POINT ( 'NONE',  ( -45.99999999999999289, 0.000000000000000000, 9.525000000000000355 ) ) ;
#44153 =( LENGTH_UNIT ( ) NAMED_UNIT ( * ) SI_UNIT ( .MILLI., .METRE. ) );
#44154 = CYLINDRICAL_SURFACE ( 'NONE', #9187, 0.5000000000000000000 ) ;
#44155 = CARTESIAN_POINT ( 'NONE',  ( -14.98999599679679662, 118.4999999999999716, 10.00000000000000000 ) ) ;
#44156 = CARTESIAN_POINT ( 'NONE',  ( 3.499999999999999112, 33.99999999999998579, 3.750000000000000000 ) ) ;
#44157 = FACE_OUTER_BOUND ( 'NONE', #44652, .T. ) ;
#44158 = VERTEX_POINT ( 'NONE', #38828 ) ;
#44159 = AXIS2_PLACEMENT_3D ( 'NONE', #44218, #44567, #56100 ) ;
#44160 = CARTESIAN_POINT ( 'NONE',  ( 12.50000000000000355, 30.74999999999998579, 4.000000000000000000 ) ) ;
#44161 = CARTESIAN_POINT ( 'NONE',  ( -58.94499999999998607, -9.827790563157499189E-16, -8.024999999999991473 ) ) ;
#44162 = ORIENTED_EDGE ( 'NONE', *, *, #40004, .F. ) ;
#44163 = B_SPLINE_CURVE_WITH_KNOTS ( 'NONE', 3,
 ( #22629, #28207, #12395, #56350, #34218, #28568, #12056, #6779 ),
 .UNSPECIFIED., .F., .F.,
 ( 4, 2, 2, 4 ),
 ( 0.000000000000000000, 0.0003517464476818396276, 0.0005276196715227495209, 0.0007034928953636595227 ),
 .UNSPECIFIED. ) ;
#44164 = DIRECTION ( 'NONE',  ( -1.000000000000000000, 0.000000000000000000, 0.000000000000000000 ) ) ;
#44165 = CARTESIAN_POINT ( 'NONE',  ( -45.00000000000000000, -2.024042244987997205E-14, 9.500000000000000000 ) ) ;
#44166 = CARTESIAN_POINT ( 'NONE',  ( -45.00000000000000000, 9.581012678897851131, -6.371410634540580098 ) ) ;
#44167 = ORIENTED_EDGE ( 'NONE', *, *, #12464, .T. ) ;
#44168 = CARTESIAN_POINT ( 'NONE',  ( 53.25000000000005684, 1.231653667943533289E-13, 3.750000000000000000 ) ) ;
#44169 = ORIENTED_EDGE ( 'NONE', *, *, #14469, .T. ) ;
#44170 = CARTESIAN_POINT ( 'NONE',  ( -74.29271480430246299, 8.623151806617508797, 6.441684343570472926 ) ) ;
#44171 = CARTESIAN_POINT ( 'NONE',  ( -112.2549999999999955, -4.716976649647092401, 6.492361379858946790 ) ) ;
#44172 = ORIENTED_EDGE ( 'NONE', *, *, #56645, .F. ) ;
#44173 = PRESENTATION_LAYER_ASSIGNMENT (  '', '', ( #40788 ) ) ;
#44174 = PRESENTATION_STYLE_ASSIGNMENT (( #61328 ) ) ;
#44175 = DIRECTION ( 'NONE',  ( -1.000000000000000000, 0.000000000000000000, 0.000000000000000000 ) ) ;
#44176 = CARTESIAN_POINT ( 'NONE',  ( -195.0000000000000000, 0.000000000000000000, 0.000000000000000000 ) ) ;
#44177 = CARTESIAN_POINT ( 'NONE',  ( -153.6570736234661751, 9.058813317711329915, 2.943386871421369566 ) ) ;
#44178 =( GEOMETRIC_REPRESENTATION_CONTEXT ( 3 ) GLOBAL_UNCERTAINTY_ASSIGNED_CONTEXT ( ( #11662 ) ) GLOBAL_UNIT_ASSIGNED_CONTEXT ( ( #11321, #65836, #32781 ) ) REPRESENTATION_CONTEXT ( 'NONE', 'WORKASPACE' ) );
#44179 = CARTESIAN_POINT ( 'NONE',  ( 9.058813317711337021, 135.5449999999999875, 2.943386871421375783 ) ) ;
#44180 = CARTESIAN_POINT ( 'NONE',  ( -94.25707362346618368, 5.598654528085800663, -7.705886871421367523 ) ) ;
#44181 = EDGE_CURVE ( 'NONE', #29534, #66538, #53846, .T. ) ;
#44182 = STYLED_ITEM ( 'NONE', ( #16295 ), #54983 ) ;
#44183 = CARTESIAN_POINT ( 'NONE',  ( -54.37283216165869248, -9.131344072907124243, -2.873593582808337210 ) ) ;
#44184 = ORIENTED_EDGE ( 'NONE', *, *, #50791, .F. ) ;
#44185 = DIRECTION ( 'NONE',  ( 0.000000000000000000, 0.000000000000000000, 1.000000000000000000 ) ) ;
#44186 = CARTESIAN_POINT ( 'NONE',  ( 22.00000000000002132, 42.00000000000000000, 75.00000000000000000 ) ) ;
#44187 = PRESENTATION_LAYER_ASSIGNMENT (  '', '', ( #4808 ) ) ;
#44188 = CARTESIAN_POINT ( 'NONE',  ( -134.4549999999999841, 7.632228543268599452, -2.479861379858951942 ) ) ;
#44189 = DIRECTION ( 'NONE',  ( 0.000000000000000000, 0.000000000000000000, -1.000000000000000000 ) ) ;
#44190 = LINE ( 'NONE', #38906, #12297 ) ;
#44191 = SURFACE_SIDE_STYLE ('',( #1153 ) ) ;
#44192 = CARTESIAN_POINT ( 'NONE',  ( -146.0949999999999989, -2.607480562269071545, -8.024999999999991473 ) ) ;
#44193 = CARTESIAN_POINT ( 'NONE',  ( -127.9449999999999790, -9.827790563157499189E-16, -8.024999999999991473 ) ) ;
#44194 = EDGE_LOOP ( 'NONE', ( #2429, #45010, #13412, #52620 ) ) ;
#44195 = FACE_OUTER_BOUND ( 'NONE', #46240, .T. ) ;
#44196 =( BOUNDED_CURVE ( )  B_SPLINE_CURVE ( 2, ( #62655, #19761, #45831, #2116, #67978, #41257, #2489, #3536, #13433, #13087, #45150 ),
 .UNSPECIFIED., .F., .F. ) 
 B_SPLINE_CURVE_WITH_KNOTS ( ( 3, 2, 2, 2, 2, 3 ),
 ( 0.3529411764705882582, 0.3588235294117647078, 0.3647058823529411575, 0.3705882352941177182, 0.3764705882352941679, 0.3823529411764706176 ),
 .UNSPECIFIED. ) 
 CURVE ( )  GEOMETRIC_REPRESENTATION_ITEM ( )  RATIONAL_B_SPLINE_CURVE ( ( 1.000000000000000000, 0.9510565162951535312, 1.000000000000000000, 0.9510565162951535312, 1.000000000000000000, 0.9510565162951535312, 1.000000000000000000, 0.9510565162951535312, 1.000000000000000000, 0.9510565162951530871, 1.000000000000000444 ) ) 
 REPRESENTATION_ITEM ( '' )  );
#44197 = CARTESIAN_POINT ( 'NONE',  ( -179.6929263765337907, 10.01517768586948698, -1.839758294383808571E-15 ) ) ;
#44198 =( NAMED_UNIT ( * ) SI_UNIT ( $, .STERADIAN. ) SOLID_ANGLE_UNIT ( ) );
#44199 = CARTESIAN_POINT ( 'NONE',  ( -56.54499999999998749, -7.632228543268600340, -2.479861379858950166 ) ) ;
#44200 = ADVANCED_FACE ( 'NONE', ( #50381 ), #40189, .T. ) ;
#44201 = CYLINDRICAL_SURFACE ( 'NONE', #35448, 0.5000000000000004441 ) ;
#44202 = AXIS2_PLACEMENT_3D ( 'NONE', #35359, #9324, #45928 ) ;
#44203 = DIRECTION ( 'NONE',  ( -1.000000000000000000, 0.000000000000000000, 0.000000000000000000 ) ) ;
#44204 =( NAMED_UNIT ( * ) SI_UNIT ( $, .STERADIAN. ) SOLID_ANGLE_UNIT ( ) );
#44205 = CARTESIAN_POINT ( 'NONE',  ( -91.49292637653378790, -8.102448949553172852, 5.886773742842742685 ) ) ;
#44206 = PRODUCT_CONTEXT ( 'NONE', #32097, 'mechanical' ) ;
#44208 = EDGE_CURVE ( 'NONE', #9417, #31048, #30277, .T. ) ;
#44207 = FACE_OUTER_BOUND ( 'NONE', #9329, .T. ) ;
#44209 = DIRECTION ( 'NONE',  ( 1.000000000000000000, 0.000000000000000000, 0.000000000000000000 ) ) ;
#44210 = CARTESIAN_POINT ( 'NONE',  ( 44.25000000000000000, 21.99999999999998579, 3.750000000000000000 ) ) ;
#44211 = CARTESIAN_POINT ( 'NONE',  ( 61.74999999999998579, 31.24999999999999289, 3.750000000000000000 ) ) ;
#44212 = DIRECTION ( 'NONE',  ( 0.000000000000000000, 0.000000000000000000, 1.000000000000000000 ) ) ;
#44213 = CARTESIAN_POINT ( 'NONE',  ( 39.74999999999999289, 18.74999999999997868, 3.750000000000000000 ) ) ;
#44214 = CIRCLE ( 'NONE', #50749, 0.5000000000000004441 ) ;
#44215 = ORIENTED_EDGE ( 'NONE', *, *, #31735, .T. ) ;
#44216 = CARTESIAN_POINT ( 'NONE',  ( 82.09357085539566867, 5.000000000000000000, -37.00402776293823592 ) ) ;
#44217 = ADVANCED_FACE ( 'NONE', ( #66191 ), #2158, .F. ) ;
#44218 = CARTESIAN_POINT ( 'NONE',  ( -23.21231517720797655, 117.4999999999999716, 7.500000000000000000 ) ) ;
#44219 = ORIENTED_EDGE ( 'NONE', *, *, #19814, .F. ) ;
#44220 = CARTESIAN_POINT ( 'NONE',  ( -34.99999999999992184, 112.9999999999999858, -9.500000000000000000 ) ) ;
#44221 = AXIS2_PLACEMENT_3D ( 'NONE', #27729, #37684, #59082 ) ;
#44222 = CARTESIAN_POINT ( 'NONE',  ( -7.632228543268608334, 127.9570736234661439, 2.479861379858952830 ) ) ;
#44223 = CONICAL_SURFACE ( 'NONE', #11584, 9.000000000000000000, 0.7853981633974500554 ) ;
#44225 = EDGE_CURVE ( 'NONE', #17714, #63631, #23632, .T. ) ;
#44224 = DIRECTION ( 'NONE',  ( 1.000000000000000000, 0.000000000000000000, 0.000000000000000000 ) ) ;
#44227 =( NAMED_UNIT ( * ) PLANE_ANGLE_UNIT ( ) SI_UNIT ( $, .RADIAN. ) );
#44226 = CIRCLE ( 'NONE', #26340, 1.000000000000000888 ) ;
#44228 = ORIENTED_EDGE ( 'NONE', *, *, #3789, .F. ) ;
#44229 = STYLED_ITEM ( 'NONE', ( #22923 ), #6402 ) ;
#44230 = DIRECTION ( 'NONE',  ( 1.000000000000000000, 0.000000000000000000, -0.000000000000000000 ) ) ;
#44231 = CIRCLE ( 'NONE', #13859, 0.5000000000000004441 ) ;
#44232 = DIRECTION ( 'NONE',  ( -0.000000000000000000, 0.3420201433256629953, 0.9396926207859104263 ) ) ;
#44233 = ORIENTED_EDGE ( 'NONE', *, *, #66319, .T. ) ;
#44234 = DIRECTION ( 'NONE',  ( 0.000000000000000000, 1.000000000000000000, 0.000000000000000000 ) ) ;
#44235 = CARTESIAN_POINT ( 'NONE',  ( -94.40707362346725517, 3.094860106600277661, -9.525000000013180923 ) ) ;
#44236 = DIRECTION ( 'NONE',  ( 0.000000000000000000, 1.000000000000000000, 0.000000000000000000 ) ) ;
#44237 = CARTESIAN_POINT ( 'NONE',  ( -86.69499999999999318, -8.437984349512085203, 5.166775262442717831E-16 ) ) ;
#44238 = ORIENTED_EDGE ( 'NONE', *, *, #66932, .T. ) ;
#44239 = CIRCLE ( 'NONE', #40869, 4.499999999999997335 ) ;
#44240 = CARTESIAN_POINT ( 'NONE',  ( -20.57648123223228964, 114.5812418126072174, -10.27659574468084891 ) ) ;
#44241 = PRESENTATION_LAYER_ASSIGNMENT (  '', '', ( #16157 ) ) ;
#44242 = CARTESIAN_POINT ( 'NONE',  ( 44.99999999999999289, 9.905302582397009559, 6.348323522273335406 ) ) ;
#44243 = FILL_AREA_STYLE_COLOUR ( '', #35147 ) ;
#44244 = VERTEX_POINT ( 'NONE', #66557 ) ;
#44245 = FACE_OUTER_BOUND ( 'NONE', #47090, .T. ) ;
#44246 = LINE ( 'NONE', #33635, #67246 ) ;
#44247 = ORIENTED_EDGE ( 'NONE', *, *, #5192, .F. ) ;
#44248 = CARTESIAN_POINT ( 'NONE',  ( 0.000000000000000000, 0.000000000000000000, 0.000000000000000000 ) ) ;
#44249 = EDGE_LOOP ( 'NONE', ( #60003, #60210, #62883, #49140 ) ) ;
#44250 = FILL_AREA_STYLE_COLOUR ( '', #21488 ) ;
#44251 = PLANE ( 'NONE',  #51006 ) ;
#44252 = CARTESIAN_POINT ( 'NONE',  ( -5.365183871890740974, -2.392512705203733159, 4.707228941936125288 ) ) ;
#44253 = VECTOR ( 'NONE', #589, 1000.000000000000000 ) ;
#44254 = CARTESIAN_POINT ( 'NONE',  ( -182.0070736234661979, -8.102448949553172852, -5.886773742842741797 ) ) ;
#44255 = CARTESIAN_POINT ( 'NONE',  ( -195.0000000000000000, 0.000000000000000000, 0.000000000000000000 ) ) ;
#44256 = CARTESIAN_POINT ( 'NONE',  ( 11.00000000000001776, 16.44305403005404287, 6.465863758942333782E-16 ) ) ;
#44257 = EDGE_CURVE ( 'NONE', #20808, #15660, #51650, .T. ) ;
#44258 = AXIS2_PLACEMENT_3D ( 'NONE', #4284, #47646, #69053 ) ;
#44259 = AXIS2_PLACEMENT_3D ( 'NONE', #67279, #29282, #66228 ) ;
#44260 = CARTESIAN_POINT ( 'NONE',  ( -67.94292637653380496, 0.000000000000000000, 9.524999999999991473 ) ) ;
#44261 = CARTESIAN_POINT ( 'NONE',  ( -6.050614363280173436, 153.8633571366135584, 6.516612769276303396 ) ) ;
#44262 = B_SPLINE_CURVE_WITH_KNOTS ( 'NONE', 3,
 ( #43385, #64431, #53198, #68678, #32759, #16281, #20478, #54210 ),
 .UNSPECIFIED., .F., .F.,
 ( 4, 2, 2, 4 ),
 ( -6.733023926831683363E-06, 0.0008427316310560315328, 0.001267463958547471355, 0.001692196286038911502 ),
 .UNSPECIFIED. ) ;
#44263 = ORIENTED_EDGE ( 'NONE', *, *, #18817, .F. ) ;
#44264 = DIRECTION ( 'NONE',  ( 0.000000000000000000, 0.000000000000000000, 1.000000000000000000 ) ) ;
#44265 = SURFACE_STYLE_FILL_AREA ( #43911 ) ;
#44266 =( LENGTH_UNIT ( ) NAMED_UNIT ( * ) SI_UNIT ( .MILLI., .METRE. ) );
#44267 = ORIENTED_EDGE ( 'NONE', *, *, #43260, .T. ) ;
#44268 = AXIS2_PLACEMENT_3D ( 'NONE', #25128, #24416, #68060 ) ;
#44269 = CARTESIAN_POINT ( 'NONE',  ( -164.1550000000000011, 7.632228543268600340, 2.479861379858949277 ) ) ;
#44270 = FACE_OUTER_BOUND ( 'NONE', #34056, .T. ) ;
#44271 = CARTESIAN_POINT ( 'NONE',  ( -183.6019133891463468, -5.474665737238584740, -7.053184183476749247 ) ) ;
#44272 = CARTESIAN_POINT ( 'NONE',  ( -175.7950000000000159, 2.607480562269068880, -8.024999999999993250 ) ) ;
#44273 = STYLED_ITEM ( 'NONE', ( #15426 ), #36673 ) ;
#44274 = CARTESIAN_POINT ( 'NONE',  ( -155.5449999999999875, -7.632228543268600340, -2.479861379858950166 ) ) ;
#44275 = VERTEX_POINT ( 'NONE', #54930 ) ;
#44276 = FACE_OUTER_BOUND ( 'NONE', #61522, .T. ) ;
#44277 = CARTESIAN_POINT ( 'NONE',  ( 44.40987964080542127, 10.30029937056511713, 3.500456542365121937 ) ) ;
#44278 = CARTESIAN_POINT ( 'NONE',  ( -9.827790563157511022E-16, 151.4429263765338192, 8.025000000000000355 ) ) ;
#44279 =( GEOMETRIC_REPRESENTATION_CONTEXT ( 3 ) GLOBAL_UNCERTAINTY_ASSIGNED_CONTEXT ( ( #24360 ) ) GLOBAL_UNIT_ASSIGNED_CONTEXT ( ( #62928, #21770, #48540 ) ) REPRESENTATION_CONTEXT ( 'NONE', 'WORKASPACE' ) );
#44280 = CARTESIAN_POINT ( 'NONE',  ( -70.55499999999999261, 0.000000000000000000, 8.024999999999991473 ) ) ;
#44281 = CARTESIAN_POINT ( 'NONE',  ( -35.65778776279521622, -9.947368421052628307, 4.481646853389228191 ) ) ;
#44282 = DIRECTION ( 'NONE',  ( -0.000000000000000000, -1.000000000000000000, -0.000000000000000000 ) ) ;
#44283 = AXIS2_PLACEMENT_3D ( 'NONE', #17894, #34063, #61464 ) ;
#44284 = EDGE_CURVE ( 'NONE', #13679, #17136, #34814, .T. ) ;
#44285 = VECTOR ( 'NONE', #28379, 1000.000000000000000 ) ;
#44286 = CARTESIAN_POINT ( 'NONE',  ( -67.04499999999997328, 7.632228543268600340, 2.479861379858949277 ) ) ;
#44287 = EDGE_CURVE ( 'NONE', #1680, #17724, #29247, .T. ) ;
#44288 = CARTESIAN_POINT ( 'NONE',  ( 9.058813317711337021, 133.6550000000000011, 2.943386871421375783 ) ) ;
#44289 = CARTESIAN_POINT ( 'NONE',  ( -8.437984349512095861, 126.6929263765338192, -5.166775262442723748E-16 ) ) ;
#44290 = MECHANICAL_DESIGN_GEOMETRIC_PRESENTATION_REPRESENTATION (  '', ( #55481 ), #42039 ) ;
#44291 = CARTESIAN_POINT ( 'NONE',  ( 0.000000000000000000, -1.999999999999999556, 3.000000000000000444 ) ) ;
#44292 = MECHANICAL_DESIGN_GEOMETRIC_PRESENTATION_REPRESENTATION (  '', ( #38717 ), #36460 ) ;
#44293 = LINE ( 'NONE', #39008, #5724 ) ;
#44294 = CIRCLE ( 'NONE', #13915, 0.5000000000000004441 ) ;
#44295 = ORIENTED_EDGE ( 'NONE', *, *, #22574, .F. ) ;
#44296 = EDGE_CURVE ( 'NONE', #45684, #26721, #17695, .T. ) ;
#44297 = CARTESIAN_POINT ( 'NONE',  ( -50.69292637653379785, 10.01517768586948698, -1.839758294383808966E-15 ) ) ;
#44298 = EDGE_CURVE ( 'NONE', #37840, #10308, #39163, .T. ) ;
#44299 = CIRCLE ( 'NONE', #50983, 0.5000000000000004441 ) ;
#44300 = DIRECTION ( 'NONE',  ( 0.000000000000000000, 0.000000000000000000, 1.000000000000000000 ) ) ;
#44301 = DIRECTION ( 'NONE',  ( 0.000000000000000000, 1.000000000000000000, -0.000000000000000000 ) ) ;
#44302 = ADVANCED_FACE ( 'NONE', ( #8167 ), #7850, .T. ) ;
#44303 =( NAMED_UNIT ( * ) PLANE_ANGLE_UNIT ( ) SI_UNIT ( $, .RADIAN. ) );
#44304 = ORIENTED_EDGE ( 'NONE', *, *, #55663, .T. ) ;
#44306 = ORIENTED_EDGE ( 'NONE', *, *, #17862, .F. ) ;
#44305 = COLOUR_RGB ( '', 0.72549020, 0.75294118, 0.79215686) ;
#44307 = STYLED_ITEM ( 'NONE', ( #27267 ), #61927 ) ;
#44308 = FACE_OUTER_BOUND ( 'NONE', #32396, .T. ) ;
#44309 = ADVANCED_FACE ( 'NONE', ( #23985 ), #19748, .T. ) ;
#44310 = SURFACE_SIDE_STYLE ('',( #34042 ) ) ;
#44311 = CARTESIAN_POINT ( 'NONE',  ( 0.000000000000000000, -2.500000000000000000, 0.000000000000000000 ) ) ;
#44312 = EDGE_LOOP ( 'NONE', ( #23343, #6363, #13179, #54586 ) ) ;
#44313 = CARTESIAN_POINT ( 'NONE',  ( -108.5049999999999812, -6.826472737025113702, -4.959722759717900331 ) ) ;
#44314 = VERTEX_POINT ( 'NONE', #41243 ) ;
#44315 = CARTESIAN_POINT ( 'NONE',  ( 3.000000000000002665, 0.000000000000000000, -89.00000000000000000 ) ) ;
#44316 = FILL_AREA_STYLE ('',( #6602 ) ) ;
#44317 = ORIENTED_EDGE ( 'NONE', *, *, #25012, .F. ) ;
#44318 = FILL_AREA_STYLE_COLOUR ( '', #60526 ) ;
#44319 = DIRECTION ( 'NONE',  ( 0.000000000000000000, 1.000000000000000000, 0.000000000000000000 ) ) ;
#44320 = ORIENTED_EDGE ( 'NONE', *, *, #49675, .T. ) ;
#44321 = AXIS2_PLACEMENT_3D ( 'NONE', #41382, #15355, #52284 ) ;
#44322 = FILL_AREA_STYLE ('',( #39028 ) ) ;
#44323 = CARTESIAN_POINT ( 'NONE',  ( 9.058813317711338797, 156.8449999999999704, -2.943386871421372675 ) ) ;
#44324 = DIRECTION ( 'NONE',  ( -0.000000000000000000, -1.000000000000000000, 0.000000000000000000 ) ) ;
#44325 = EDGE_LOOP ( 'NONE', ( #14316, #27982, #62375, #677 ) ) ;
#44326 = VECTOR ( 'NONE', #30084, 1000.000000000000000 ) ;
#44327 = ORIENTED_EDGE ( 'NONE', *, *, #36989, .F. ) ;
#44328 = PRESENTATION_STYLE_ASSIGNMENT (( #37669 ) ) ;
#44329 = LINE ( 'NONE', #39037, #11639 ) ;
#44330 = VECTOR ( 'NONE', #40188, 1000.000000000000000 ) ;
#44331 = ORIENTED_EDGE ( 'NONE', *, *, #14538, .F. ) ;
#44332 = CARTESIAN_POINT ( 'NONE',  ( -7.632228543268607446, 138.5429263765338135, -2.479861379858953718 ) ) ;
#44333 = CYLINDRICAL_SURFACE ( 'NONE', #52527, 9.524999999999991473 ) ;
#44334 = CARTESIAN_POINT ( 'NONE',  ( 0.000000000000000000, 0.000000000000000000, 0.2499999999999941436 ) ) ;
#44335 = CARTESIAN_POINT ( 'NONE',  ( 57.00000000000000000, 5.000000000000000000, 60.00402776293825724 ) ) ;
#44336 = CARTESIAN_POINT ( 'NONE',  ( -48.81081081081080697, 14.09971791521133255, 7.500000000000000000 ) ) ;
#44337 = ORIENTED_EDGE ( 'NONE', *, *, #38652, .T. ) ;
#44338 = SURFACE_SIDE_STYLE ('',( #48918 ) ) ;
#44339 = ORIENTED_EDGE ( 'NONE', *, *, #7937, .F. ) ;
#44340 = CARTESIAN_POINT ( 'NONE',  ( -52.04292637653379217, -9.058813317711329915, -2.943386871421370898 ) ) ;
#44341 = CARTESIAN_POINT ( 'NONE',  ( -75.75000000000000000, -4.000000000000000000, 6.000000000000001776 ) ) ;
#44342 = DIRECTION ( 'NONE',  ( -1.000000000000000000, -0.000000000000000000, -0.000000000000000000 ) ) ;
#44343 = CARTESIAN_POINT ( 'NONE',  ( -132.9549999999999841, -7.632228543268599452, 2.479861379858951054 ) ) ;
#44344 =( NAMED_UNIT ( * ) PLANE_ANGLE_UNIT ( ) SI_UNIT ( $, .RADIAN. ) );
#44345 = CARTESIAN_POINT ( 'NONE',  ( 10.00000000000001776, 43.00000000000000000, 29.68999999999999417 ) ) ;
#44346 = ORIENTED_EDGE ( 'NONE', *, *, #65686, .T. ) ;
#44347 = AXIS2_PLACEMENT_3D ( 'NONE', #21125, #20798, #52482 ) ;
#44348 = CARTESIAN_POINT ( 'NONE',  ( -9.827790563157511022E-16, 140.5570736234661524, 8.025000000000000355 ) ) ;
#44349 = CARTESIAN_POINT ( 'NONE',  ( -107.3070736234661524, -10.01517768586948698, 6.132527647946031529E-16 ) ) ;
#44350 = FACE_OUTER_BOUND ( 'NONE', #3486, .T. ) ;
#44351 = ORIENTED_EDGE ( 'NONE', *, *, #807, .F. ) ;
#44352 = VERTEX_POINT ( 'NONE', #52489 ) ;
#44353 = CARTESIAN_POINT ( 'NONE',  ( -44.99310538600512643, 9.606306540395133098, 3.226244738077002072 ) ) ;
#44355 = CARTESIAN_POINT ( 'NONE',  ( -52.70499999999996277, 2.607480562269073321, 8.024999999999991473 ) ) ;
#44354 = MECHANICAL_DESIGN_GEOMETRIC_PRESENTATION_REPRESENTATION (  '', ( #51040 ), #15116 ) ;
#44356 = ORIENTED_EDGE ( 'NONE', *, *, #25023, .F. ) ;
#44357 = CARTESIAN_POINT ( 'NONE',  ( 25.75000000000001066, 0.000000000000000000, 3.750000000000000000 ) ) ;
#44358 = CARTESIAN_POINT ( 'NONE',  ( 60.00000000000000000, 147.4999999999999716, -9.500000000000000000 ) ) ;
#44359 = SURFACE_STYLE_USAGE ( .BOTH. , #22863 ) ;
#44360 = AXIS2_PLACEMENT_3D ( 'NONE', #52930, #25477, #25139 ) ;
#44361 = LINE ( 'NONE', #39410, #32900 ) ;
#44362 = CARTESIAN_POINT ( 'NONE',  ( 54.99999999999999289, 2.409368300552961372E-15, 11.50000000000003730 ) ) ;
#44363 = ORIENTED_EDGE ( 'NONE', *, *, #11696, .F. ) ;
#44364 = EDGE_CURVE ( 'NONE', #17013, #39245, #37087, .T. ) ;
#44365 =( NAMED_UNIT ( * ) PLANE_ANGLE_UNIT ( ) SI_UNIT ( $, .RADIAN. ) );
#44366 = SURFACE_SIDE_STYLE ('',( #12278 ) ) ;
#44367 =( NAMED_UNIT ( * ) SI_UNIT ( $, .STERADIAN. ) SOLID_ANGLE_UNIT ( ) );
#44368 = CARTESIAN_POINT ( 'NONE',  ( 57.00000000000000000, 0.000000000000000000, -79.00402776293826435 ) ) ;
#44369 = SURFACE_STYLE_USAGE ( .BOTH. , #49607 ) ;
#44370 = EDGE_CURVE ( 'NONE', #15255, #68401, #67599, .T. ) ;
#44371 = EDGE_CURVE ( 'NONE', #24181, #13131, #54986, .T. ) ;
#44372 = AXIS2_PLACEMENT_3D ( 'NONE', #2401, #34813, #35866 ) ;
#44373 = CARTESIAN_POINT ( 'NONE',  ( -103.0449999999999875, 7.632228543268600340, 2.479861379858949277 ) ) ;
#44374 = CARTESIAN_POINT ( 'NONE',  ( 9.058813317711338797, 153.8449999999999704, -2.943386871421372675 ) ) ;
#44375 = CARTESIAN_POINT ( 'NONE',  ( -82.79499999999998749, 2.607480562269068880, -8.024999999999993250 ) ) ;
#44376 = EDGE_CURVE ( 'NONE', #63964, #39801, #9909, .T. ) ;
#44377 = FILL_AREA_STYLE ('',( #48952 ) ) ;
#44378 = CARTESIAN_POINT ( 'NONE',  ( -34.99999999999992895, 110.4999999999999858, 10.00000000000000000 ) ) ;
#44379 = AXIS2_PLACEMENT_3D ( 'NONE', #28953, #34262, #28249 ) ;
#44380 = SURFACE_STYLE_USAGE ( .BOTH. , #66469 ) ;
#44381 = DIRECTION ( 'NONE',  ( -0.000000000000000000, 1.000000000000000000, -0.000000000000000000 ) ) ;
#44382 = CIRCLE ( 'NONE', #36492, 1.000000000000000888 ) ;
#44383 = CARTESIAN_POINT ( 'NONE',  ( 40.82991390394946052, 108.1252238755516970, -3.311222316328668480 ) ) ;
#44384 = EDGE_LOOP ( 'NONE', ( #15518, #31430, #25505, #878, #14854, #27405 ) ) ;
#44385 = CARTESIAN_POINT ( 'NONE',  ( -125.3929263765338220, 8.102448949553176405, 5.886773742842740909 ) ) ;
#44386 = COLOUR_RGB ( '', 0.09019608, 0.27058824, 0.51372549) ;
#44387 =( NAMED_UNIT ( * ) SI_UNIT ( $, .STERADIAN. ) SOLID_ANGLE_UNIT ( ) );
#44388 = CARTESIAN_POINT ( 'NONE',  ( -133.4950000000000045, 6.826472737025113702, -4.959722759717902107 ) ) ;
#44389 = FACE_OUTER_BOUND ( 'NONE', #45018, .T. ) ;
#44390 = EDGE_CURVE ( 'NONE', #68594, #54457, #30275, .T. ) ;
#44391 = CARTESIAN_POINT ( 'NONE',  ( -9.250000000000003553, 27.99999999999998934, -3.750000000000000000 ) ) ;
#44392 = CARTESIAN_POINT ( 'NONE',  ( -172.9429263765337907, 0.000000000000000000, 9.524999999999991473 ) ) ;
#44393 = EDGE_LOOP ( 'NONE', ( #50707, #60765, #33485, #57881 ) ) ;
#44394 = VERTEX_POINT ( 'NONE', #9214 ) ;
#44395 = DIRECTION ( 'NONE',  ( 0.000000000000000000, 0.000000000000000000, 1.000000000000000000 ) ) ;
#44396 = DIRECTION ( 'NONE',  ( -0.000000000000000000, 1.000000000000000000, -0.000000000000000000 ) ) ;
#44397 = PRESENTATION_LAYER_ASSIGNMENT (  '', '', ( #64537 ) ) ;
#44398 = DIRECTION ( 'NONE',  ( -1.000000000000000000, 0.000000000000000000, 0.000000000000000000 ) ) ;
#44399 = PRESENTATION_STYLE_ASSIGNMENT (( #18657 ) ) ;
#44400 = B_SPLINE_CURVE_WITH_KNOTS ( 'NONE', 3,
 ( #66350, #44945, #55457, #34353, #29041, #7281, #55803, #24139 ),
 .UNSPECIFIED., .F., .F.,
 ( 4, 2, 2, 4 ),
 ( 4.336808689942017736E-19, 0.0004249208466734718018, 0.0008498416933469431700, 0.001699683386693885906 ),
 .UNSPECIFIED. ) ;
#44401 = CARTESIAN_POINT ( 'NONE',  ( -50.00707362346617657, -8.102448949553174629, -5.886773742842741797 ) ) ;
#44402 = CARTESIAN_POINT ( 'NONE',  ( -150.4429263765338192, -1.166476076187852838E-15, -9.524999999999991473 ) ) ;
#44403 = ORIENTED_EDGE ( 'NONE', *, *, #48539, .F. ) ;
#44404 = CARTESIAN_POINT ( 'NONE',  ( -146.0049999999999955, 6.826472737025115478, 4.959722759717899443 ) ) ;
#44405 = VERTEX_POINT ( 'NONE', #29955 ) ;
#44406 = EDGE_CURVE ( 'NONE', #28960, #27631, #15211, .T. ) ;
#44407 = EDGE_LOOP ( 'NONE', ( #49679, #15488, #69278 ) ) ;
#44408 = DIRECTION ( 'NONE',  ( -0.000000000000000000, -0.000000000000000000, -1.000000000000000000 ) ) ;
#44409 =( NAMED_UNIT ( * ) PLANE_ANGLE_UNIT ( ) SI_UNIT ( $, .RADIAN. ) );
#44410 = ORIENTED_EDGE ( 'NONE', *, *, #42686, .T. ) ;
#44411 = VECTOR ( 'NONE', #9847, 1000.000000000000114 ) ;
#44412 = COLOUR_RGB ( '', 0.66274510, 0.83137255, 0.94901961) ;
#44413 = AXIS2_PLACEMENT_3D ( 'NONE', #43541, #55334, #13819 ) ;
#44414 =( NAMED_UNIT ( * ) PLANE_ANGLE_UNIT ( ) SI_UNIT ( $, .RADIAN. ) );
#44415 = ADVANCED_FACE ( 'NONE', ( #51773 ), #24327, .F. ) ;
#44416 = CARTESIAN_POINT ( 'NONE',  ( 9.058813317711338797, 129.8449999999999989, -2.943386871421372675 ) ) ;
#44417 = CARTESIAN_POINT ( 'NONE',  ( 47.50000000000000000, 13.41640786499872284, 9.500000000000000000 ) ) ;
#44418 = ORIENTED_EDGE ( 'NONE', *, *, #17203, .F. ) ;
#44419 = FILL_AREA_STYLE_COLOUR ( '', #21804 ) ;
#44420 = CARTESIAN_POINT ( 'NONE',  ( 5.598654528085805993, 127.3549999999999898, 7.705886871421374629 ) ) ;
#44421 = CARTESIAN_POINT ( 'NONE',  ( -53.75499999999999545, 4.716976649647091513, -6.492361379858946790 ) ) ;
#44422 = CARTESIAN_POINT ( 'NONE',  ( 41.36364127011594150, 107.7184400395433386, -3.928466540244119454 ) ) ;
#44423 = VERTEX_POINT ( 'NONE', #3894 ) ;
#44424 = CARTESIAN_POINT ( 'NONE',  ( -8.102448949553181734, 153.6049999999999898, 5.886773742842747126 ) ) ;
#44425 = CARTESIAN_POINT ( 'NONE',  ( 7.750000000000000000, 33.74999999999998579, -3.750000000000000000 ) ) ;
#44426 = STYLED_ITEM ( 'NONE', ( #18521 ), #2245 ) ;
#44427 = CARTESIAN_POINT ( 'NONE',  ( -87.59292637653381064, -3.094860106618431139, -9.524999999999991473 ) ) ;
#44428 = FILL_AREA_STYLE_COLOUR ( '', #9229 ) ;
#44429 = COLOUR_RGB ( '', 0.72549020, 0.75294118, 0.79215686) ;
#44430 = DIRECTION ( 'NONE',  ( 0.000000000000000000, 0.000000000000000000, 1.000000000000000000 ) ) ;
#44431 = VERTEX_POINT ( 'NONE', #46537 ) ;
#44432 = AXIS2_PLACEMENT_3D ( 'NONE', #2691, #61456, #8014 ) ;
#44433 = CYLINDRICAL_SURFACE ( 'NONE', #46433, 5.000000000000000000 ) ;
#44434 = ORIENTED_EDGE ( 'NONE', *, *, #25721, .F. ) ;
#44435 = CARTESIAN_POINT ( 'NONE',  ( -34.17996781353688363, -10.00128081186360696, -3.271960291194134562 ) ) ;
#44436 = CARTESIAN_POINT ( 'NONE',  ( -173.9049999999999727, 2.607480562269068880, -8.024999999999993250 ) ) ;
#44437 = ORIENTED_EDGE ( 'NONE', *, *, #51736, .F. ) ;
#44438 = DIRECTION ( 'NONE',  ( -1.000000000000000000, 0.000000000000000000, 0.000000000000000000 ) ) ;
#44439 = SURFACE_STYLE_FILL_AREA ( #11677 ) ;
#44440 = ORIENTED_EDGE ( 'NONE', *, *, #28000, .F. ) ;
#44441 = ORIENTED_EDGE ( 'NONE', *, *, #12101, .T. ) ;
#44442 = CARTESIAN_POINT ( 'NONE',  ( -45.00000000000000000, 9.696030919201687581, -3.569498281159027453 ) ) ;
#44443 =( NAMED_UNIT ( * ) SI_UNIT ( $, .STERADIAN. ) SOLID_ANGLE_UNIT ( ) );
#44444 = CARTESIAN_POINT ( 'NONE',  ( -88.55499999999999261, 0.000000000000000000, 8.024999999999991473 ) ) ;
#44445 = ORIENTED_EDGE ( 'NONE', *, *, #57027, .F. ) ;
#44446 = EDGE_CURVE ( 'NONE', #42679, #17912, #40895, .T. ) ;
#44447 = DIRECTION ( 'NONE',  ( 0.000000000000000000, 0.000000000000000000, -1.000000000000000000 ) ) ;
#44448 = LINE ( 'NONE', #27148, #31943 ) ;
#44449 = MECHANICAL_DESIGN_GEOMETRIC_PRESENTATION_REPRESENTATION (  '', ( #5065 ), #63517 ) ;
#44450 = AXIS2_PLACEMENT_3D ( 'NONE', #36886, #58304, #22063 ) ;
#44451 = EDGE_CURVE ( 'NONE', #64475, #49204, #67962, .T. ) ;
#44452 = PRESENTATION_STYLE_ASSIGNMENT (( #44104 ) ) ;
#44453 = ORIENTED_EDGE ( 'NONE', *, *, #67935, .F. ) ;
#44454 = CYLINDRICAL_SURFACE ( 'NONE', #58625, 0.2500000000000002220 ) ;
#44456 = DIRECTION ( 'NONE',  ( 1.000000000000000000, 0.000000000000000000, -0.000000000000000000 ) ) ;
#44455 = SURFACE_SIDE_STYLE ('',( #22954 ) ) ;
#44457 = STYLED_ITEM ( 'NONE', ( #17441 ), #63878 ) ;
#44458 = EDGE_CURVE ( 'NONE', #7834, #12513, #11220, .T. ) ;
#44459 = CARTESIAN_POINT ( 'NONE',  ( 9.058813317711337021, 129.5449999999999875, 2.943386871421375783 ) ) ;
#44460 = CARTESIAN_POINT ( 'NONE',  ( -102.2949999999999733, -2.607480562269069768, 8.024999999999991473 ) ) ;
#44461 = CIRCLE ( 'NONE', #56768, 13.50000000000000533 ) ;
#44462 = CIRCLE ( 'NONE', #36628, 13.99999999999999822 ) ;
#44463 = DIRECTION ( 'NONE',  ( 1.000000000000000000, -0.000000000000000000, 0.000000000000000000 ) ) ;
#44464 = CARTESIAN_POINT ( 'NONE',  ( -155.2429263765338021, 5.598654528085804216, 7.705886871421366635 ) ) ;
#44465 =( NAMED_UNIT ( * ) SI_UNIT ( $, .STERADIAN. ) SOLID_ANGLE_UNIT ( ) );
#44466 = CARTESIAN_POINT ( 'NONE',  ( -168.7450000000000045, 4.716976649647094177, 6.492361379858945902 ) ) ;
#44467 = EDGE_CURVE ( 'NONE', #61113, #26732, #46891, .T. ) ;
#44468 = MECHANICAL_DESIGN_GEOMETRIC_PRESENTATION_REPRESENTATION (  '', ( #16336 ), #32065 ) ;
#44469 = PRESENTATION_STYLE_ASSIGNMENT (( #38498 ) ) ;
#44470 = AXIS2_PLACEMENT_3D ( 'NONE', #38456, #6380, #69383 ) ;
#44471 = CARTESIAN_POINT ( 'NONE',  ( -21.02379604162863913, 114.4999999999999574, 10.00000000000000000 ) ) ;
#44472 = EDGE_LOOP ( 'NONE', ( #74, #20181 ) ) ;
#44473 = DIRECTION ( 'NONE',  ( 1.000000000000000000, 0.000000000000000000, 0.000000000000000000 ) ) ;
#44474 = ORIENTED_EDGE ( 'NONE', *, *, #13911, .T. ) ;
#44475 = CARTESIAN_POINT ( 'NONE',  ( -66.89292637653377938, -8.102448949553172852, -5.886773742842741797 ) ) ;
#44476 = AXIS2_PLACEMENT_3D ( 'NONE', #65816, #34145, #61225 ) ;
#44477 = AXIS2_PLACEMENT_3D ( 'NONE', #15708, #10428, #11794 ) ;
#44478 = LINE ( 'NONE', #61610, #60730 ) ;
#44479 = CARTESIAN_POINT ( 'NONE',  ( -142.6429263765338078, -5.598654528085801552, 7.705886871421367523 ) ) ;
#44480 = FILL_AREA_STYLE_COLOUR ( '', #60570 ) ;
#44481 = CYLINDRICAL_SURFACE ( 'NONE', #3828, 0.4999999999999995004 ) ;
#44482 = ORIENTED_EDGE ( 'NONE', *, *, #19275, .F. ) ;
#44483 = CARTESIAN_POINT ( 'NONE',  ( -173.4549999999999841, 7.632228543268599452, -2.479861379858951942 ) ) ;
#44484 = ORIENTED_EDGE ( 'NONE', *, *, #43719, .T. ) ;
#44485 = DIRECTION ( 'NONE',  ( 0.000000000000000000, 0.000000000000000000, -1.000000000000000000 ) ) ;
#44486 = DIRECTION ( 'NONE',  ( -0.000000000000000000, -0.000000000000000000, 1.000000000000000000 ) ) ;
#44487 = DIRECTION ( 'NONE',  ( -1.000000000000000000, -0.000000000000000000, -0.000000000000000000 ) ) ;
#44488 = SURFACE_STYLE_USAGE ( .BOTH. , #3829 ) ;
#44489 = CARTESIAN_POINT ( 'NONE',  ( 60.00000000000000000, 1.797044900979284448E-15, 10.00000000000000000 ) ) ;
#44490 = CARTESIAN_POINT ( 'NONE',  ( -6.826472737025120807, 149.1070736234661354, 4.959722759717906548 ) ) ;
#44491 =( GEOMETRIC_REPRESENTATION_CONTEXT ( 3 ) GLOBAL_UNCERTAINTY_ASSIGNED_CONTEXT ( ( #14433 ) ) GLOBAL_UNIT_ASSIGNED_CONTEXT ( ( #48150, #5871, #33321 ) ) REPRESENTATION_CONTEXT ( 'NONE', 'WORKASPACE' ) );
#44492 = ORIENTED_EDGE ( 'NONE', *, *, #41079, .F. ) ;
#44493 =( NAMED_UNIT ( * ) SI_UNIT ( $, .STERADIAN. ) SOLID_ANGLE_UNIT ( ) );
#44494 = CARTESIAN_POINT ( 'NONE',  ( -79.25499999999999545, -4.716976649647092401, 6.492361379858946790 ) ) ;
#44495 = CARTESIAN_POINT ( 'NONE',  ( -9.058813317711338797, 126.4549999999999841, 2.943386871421373563 ) ) ;
#44496 = CARTESIAN_POINT ( 'NONE',  ( -92.15707362346617515, -9.058813317711329915, -2.943386871421370898 ) ) ;
#44497 = AXIS2_PLACEMENT_3D ( 'NONE', #60322, #28283, #56706 ) ;
#44498 = CARTESIAN_POINT ( 'NONE',  ( -113.8429263765337964, 9.058813317711329915, -2.943386871421373119 ) ) ;
#44499 = LINE ( 'NONE', #18064, #65545 ) ;
#44500 = DIRECTION ( 'NONE',  ( 0.000000000000000000, 0.000000000000000000, 1.000000000000000000 ) ) ;
#44501 = AXIS2_PLACEMENT_3D ( 'NONE', #64237, #57590, #151 ) ;
#44502 = ORIENTED_EDGE ( 'NONE', *, *, #29118, .F. ) ;
#44503 = CIRCLE ( 'NONE', #9687, 13.00000000000000178 ) ;
#44504 = DIRECTION ( 'NONE',  ( 1.000000000000000000, 0.000000000000000000, 0.000000000000000000 ) ) ;
#44505 = CARTESIAN_POINT ( 'NONE',  ( -58.04499999999998749, 7.632228543268600340, 2.479861379858949277 ) ) ;
#44506 = ORIENTED_EDGE ( 'NONE', *, *, #11029, .F. ) ;
#44507 =( BOUNDED_SURFACE ( )  B_SPLINE_SURFACE ( 3, 2, ( 
 ( #33463, #18677, #28856 ),
 ( #29564, #12683, #33799 ),
 ( #44422, #44754, #17979 ),
 ( #13042, #65824, #56289 ),
 ( #65471, #34154, #51034 ),
 ( #7076, #7754, #39124 ),
 ( #66514, #2793, #55612 ),
 ( #60514, #28507, #17322 ) ),
 .UNSPECIFIED., .F., .F., .F. ) 
 B_SPLINE_SURFACE_WITH_KNOTS ( ( 4, 2, 2, 4 ),
 ( 3, 3 ),
 ( 0.0006464147718099828898, 0.001546301970866985689, 0.001996245570395487143, 0.002446189169923988597 ),
 ( 0.000000000000000000, 1.000000000000000000 ),
 .UNSPECIFIED. ) 
 GEOMETRIC_REPRESENTATION_ITEM ( )  RATIONAL_B_SPLINE_SURFACE ( (
 ( 1.000000000000000000, 0.7071067811865475727, 1.000000000000000000),
 ( 1.000000000000000000, 0.7604340084997890381, 1.000000000000000000),
 ( 1.000000000000000000, 0.8048286378023303822, 1.000000000000000000),
 ( 1.000000000000000000, 0.8534265415375306141, 1.000000000000000000),
 ( 1.000000000000000000, 0.8663147087829253801, 1.000000000000000000),
 ( 1.000000000000000000, 0.8838688826992951997, 1.000000000000000000),
 ( 1.000000000000000000, 0.8885266032451287765, 1.000000000000000000),
 ( 1.000000000000000000, 0.8885233166386380388, 1.000000000000000000) ) ) 
 REPRESENTATION_ITEM ( '' )  SURFACE ( )  );
#44508 = CARTESIAN_POINT ( 'NONE',  ( 0.000000000000000000, 43.00000000000000000, 0.000000000000000000 ) ) ;
#44509 = DIRECTION ( 'NONE',  ( 1.000000000000000000, 0.000000000000000000, 0.000000000000000000 ) ) ;
#44510 = CARTESIAN_POINT ( 'NONE',  ( 45.00000000000000000, 10.69371294336137801, -6.000000000000000000 ) ) ;
#44511 = ORIENTED_EDGE ( 'NONE', *, *, #53472, .T. ) ;
#44512 = CARTESIAN_POINT ( 'NONE',  ( -51.89499999999998892, 6.826472737025115478, 4.959722759717899443 ) ) ;
#44513 = FACE_OUTER_BOUND ( 'NONE', #60898, .T. ) ;
#44514 = VERTEX_POINT ( 'NONE', #4227 ) ;
#44515 = VECTOR ( 'NONE', #18978, 1000.000000000000000 ) ;
#44516 = FACE_OUTER_BOUND ( 'NONE', #35807, .T. ) ;
#44517 = CARTESIAN_POINT ( 'NONE',  ( -114.9549999999999841, -7.632228543268599452, 2.479861379858951054 ) ) ;
#44518 = ORIENTED_EDGE ( 'NONE', *, *, #57762, .F. ) ;
#44519 = PLANE ( 'NONE',  #13712 ) ;
#44520 = ADVANCED_FACE ( 'NONE', ( #63699 ), #26730, .T. ) ;
#44521 = CARTESIAN_POINT ( 'NONE',  ( -96.44292637653380496, -1.166476076187852838E-15, -9.524999999999991473 ) ) ;
#44522 = STYLED_ITEM ( 'NONE', ( #50359 ), #1783 ) ;
#44523 = CARTESIAN_POINT ( 'NONE',  ( -146.0070736234661410, -8.102448949553172852, -5.886773742842741797 ) ) ;
#44524 = LINE ( 'NONE', #65928, #59743 ) ;
#44525 = CARTESIAN_POINT ( 'NONE',  ( 9.058813317711338797, 132.8449999999999989, -2.943386871421372675 ) ) ;
#44526 = VECTOR ( 'NONE', #58046, 1000.000000000000000 ) ;
#44527 = CARTESIAN_POINT ( 'NONE',  ( -87.35707362346617799, 5.598654528085804216, 7.705886871421366635 ) ) ;
#44528 = VECTOR ( 'NONE', #45508, 1000.000000000000000 ) ;
#44529 = CARTESIAN_POINT ( 'NONE',  ( -53.18756747357344494, -10.02680648607920588, -3.499999999999314770 ) ) ;
#44530 = ORIENTED_EDGE ( 'NONE', *, *, #59944, .F. ) ;
#44531 = LINE ( 'NONE', #1508, #65017 ) ;
#44532 = SURFACE_SIDE_STYLE ('',( #23035 ) ) ;
#44533 = SURFACE_SIDE_STYLE ('',( #60637 ) ) ;
#44534 = CARTESIAN_POINT ( 'NONE',  ( -127.1050000000000040, -6.826472737025115478, 4.959722759717900331 ) ) ;
#44535 = EDGE_CURVE ( 'NONE', #59509, #47453, #10929, .T. ) ;
#44536 = DIRECTION ( 'NONE',  ( 0.000000000000000000, 0.000000000000000000, -1.000000000000000000 ) ) ;
#44537 = CARTESIAN_POINT ( 'NONE',  ( -82.55707362346618083, -1.166476076187852838E-15, -9.524999999999991473 ) ) ;
#44538 = CARTESIAN_POINT ( 'NONE',  ( -133.4950000000000045, 6.826472737025113702, -4.959722759717902107 ) ) ;
#44539 = EDGE_CURVE ( 'NONE', #48229, #24594, #56152, .T. ) ;
#44540 = CARTESIAN_POINT ( 'NONE',  ( -131.3949999999999818, -6.826472737025113702, -4.959722759717900331 ) ) ;
#44541 = ADVANCED_FACE ( 'NONE', ( #5284 ), #58776, .F. ) ;
#44542 = ORIENTED_EDGE ( 'NONE', *, *, #40826, .F. ) ;
#44543 = DIRECTION ( 'NONE',  ( 0.000000000000000000, 0.000000000000000000, 1.000000000000000000 ) ) ;
#44544 = VECTOR ( 'NONE', #45975, 1000.000000000000000 ) ;
#44545 =( LENGTH_UNIT ( ) NAMED_UNIT ( * ) SI_UNIT ( .MILLI., .METRE. ) );
#44546 = ADVANCED_FACE ( 'NONE', ( #31687 ), #37721, .T. ) ;
#44547 = DIRECTION ( 'NONE',  ( -0.000000000000000000, -1.000000000000000000, -0.000000000000000000 ) ) ;
#44548 = UNCERTAINTY_MEASURE_WITH_UNIT (LENGTH_MEASURE( 1.000000000000000082E-05 ), #10763, 'distance_accuracy_value', 'NONE');
#44549 = CARTESIAN_POINT ( 'NONE',  ( -182.3929263765338078, 8.102448949553176405, 5.886773742842740909 ) ) ;
#44550 = CARTESIAN_POINT ( 'NONE',  ( -56.39499999999997470, -6.826472737025115478, -4.959722759717899443 ) ) ;
#44551 = DIRECTION ( 'NONE',  ( 1.000000000000000000, 0.000000000000000000, 0.000000000000000000 ) ) ;
#44552 = CARTESIAN_POINT ( 'NONE',  ( 23.71231517720798010, 117.9999999999999716, 9.500000000000000000 ) ) ;
#44553 =( GEOMETRIC_REPRESENTATION_CONTEXT ( 3 ) GLOBAL_UNCERTAINTY_ASSIGNED_CONTEXT ( ( #3895 ) ) GLOBAL_UNIT_ASSIGNED_CONTEXT ( ( #29993, #67638, #40230 ) ) REPRESENTATION_CONTEXT ( 'NONE', 'WORKASPACE' ) );
#44554 = AXIS2_PLACEMENT_3D ( 'NONE', #44671, #33382, #54478 ) ;
#44555 = DIRECTION ( 'NONE',  ( -1.000000000000000000, 0.000000000000000000, 0.000000000000000000 ) ) ;
#44556 = UNCERTAINTY_MEASURE_WITH_UNIT (LENGTH_MEASURE( 1.000000000000000082E-05 ), #27433, 'distance_accuracy_value', 'NONE');
#44557 = CARTESIAN_POINT ( 'NONE',  ( -95.39292637653380780, 8.102448949553176405, 5.886773742842740909 ) ) ;
#44558 = APPLICATION_PROTOCOL_DEFINITION ( 'draft international standard', 'automotive_design', 1998, #17723 ) ;
#44559 = PRESENTATION_STYLE_ASSIGNMENT (( #34632 ) ) ;
#44560 =( NAMED_UNIT ( * ) PLANE_ANGLE_UNIT ( ) SI_UNIT ( $, .RADIAN. ) );
#44561 = CARTESIAN_POINT ( 'NONE',  ( 17.00000000000000711, 24.99999999999998224, 3.750000000000000000 ) ) ;
#44562 = CARTESIAN_POINT ( 'NONE',  ( 57.00000000000000000, 0.000000000000000000, -77.00402776293825013 ) ) ;
#44563 = CARTESIAN_POINT ( 'NONE',  ( -163.9429263765338192, 0.000000000000000000, 9.524999999999991473 ) ) ;
#44564 = AXIS2_PLACEMENT_3D ( 'NONE', #39706, #41101, #62509 ) ;
#44565 = EDGE_LOOP ( 'NONE', ( #20357, #29550 ) ) ;
#44566 =( NAMED_UNIT ( * ) SI_UNIT ( $, .STERADIAN. ) SOLID_ANGLE_UNIT ( ) );
#44567 = DIRECTION ( 'NONE',  ( 0.000000000000000000, 0.000000000000000000, 1.000000000000000000 ) ) ;
#44568 = MECHANICAL_DESIGN_GEOMETRIC_PRESENTATION_REPRESENTATION (  '', ( #60239 ), #28782 ) ;
#44569 = ORIENTED_EDGE ( 'NONE', *, *, #50069, .T. ) ;
#44570 = FACE_BOUND ( 'NONE', #54875, .T. ) ;
#44571 = CARTESIAN_POINT ( 'NONE',  ( 7.632228543268608334, 120.4570736234661723, -2.479861379858951942 ) ) ;
#44572 = CARTESIAN_POINT ( 'NONE',  ( 20.74185979783655043, 149.7721295005298714, 9.939118314201632387 ) ) ;
#44573 = FILL_AREA_STYLE_COLOUR ( '', #5839 ) ;
#44574 = SURFACE_SIDE_STYLE ('',( #22729 ) ) ;
#44575 = ORIENTED_EDGE ( 'NONE', *, *, #43792, .F. ) ;
#44576 = DIRECTION ( 'NONE',  ( 0.000000000000000000, 0.000000000000000000, 1.000000000000000000 ) ) ;
#44577 = ORIENTED_EDGE ( 'NONE', *, *, #53058, .F. ) ;
#44578 =( LENGTH_UNIT ( ) NAMED_UNIT ( * ) SI_UNIT ( .MILLI., .METRE. ) );
#44579 = CARTESIAN_POINT ( 'NONE',  ( -93.65707362346617515, 9.058813317711329915, 2.943386871421369566 ) ) ;
#44580 = CARTESIAN_POINT ( 'NONE',  ( 40.99999999999998579, 107.7459666924148252, -3.000000000000000444 ) ) ;
#44581 = CARTESIAN_POINT ( 'NONE',  ( -93.89499999999998181, 6.826472737025116366, 4.959722759717898555 ) ) ;
#44582 = VERTEX_POINT ( 'NONE', #5624 ) ;
#44583 = CARTESIAN_POINT ( 'NONE',  ( 0.000000000000000000, 122.9429263765338192, -8.025000000000000355 ) ) ;
#44584 = SURFACE_SIDE_STYLE ('',( #43551 ) ) ;
#44585 = UNCERTAINTY_MEASURE_WITH_UNIT (LENGTH_MEASURE( 1.000000000000000082E-05 ), #41801, 'distance_accuracy_value', 'NONE');
#44586 = EDGE_LOOP ( 'NONE', ( #43957, #49942, #62656, #19413 ) ) ;
#44587 = CARTESIAN_POINT ( 'NONE',  ( -2.607480562269075097, 160.2929263765337851, 8.025000000000000355 ) ) ;
#44588 = DIRECTION ( 'NONE',  ( -0.000000000000000000, 1.000000000000000000, -0.000000000000000000 ) ) ;
#44589 = AXIS2_PLACEMENT_3D ( 'NONE', #4043, #68437, #41736 ) ;
#44590 =( NAMED_UNIT ( * ) PLANE_ANGLE_UNIT ( ) SI_UNIT ( $, .RADIAN. ) );
#44591 = EDGE_LOOP ( 'NONE', ( #25310, #48828, #61258, #11900 ) ) ;
#44592 = STYLED_ITEM ( 'NONE', ( #57602 ), #3197 ) ;
#44593 = CYLINDRICAL_SURFACE ( 'NONE', #46538, 0.9999999999999974465 ) ;
#44595 = VERTEX_POINT ( 'NONE', #37369 ) ;
#44594 = ADVANCED_FACE ( 'NONE', ( #54177, #59808 ), #43676, .F. ) ;
#44596 = CARTESIAN_POINT ( 'NONE',  ( -137.5429263765338135, 9.058813317711329915, 2.943386871421369566 ) ) ;
#44597 = STYLED_ITEM ( 'NONE', ( #35985 ), #50051 ) ;
#44598 = CARTESIAN_POINT ( 'NONE',  ( 0.000000000000000000, 2.299999999999999822, -10.00000000000000000 ) ) ;
#44599 = CARTESIAN_POINT ( 'NONE',  ( 1.000000000000000000, 42.00000000000000000, 79.00402776293826435 ) ) ;
#44600 = PRESENTATION_STYLE_ASSIGNMENT (( #533 ) ) ;
#44601 = FACE_OUTER_BOUND ( 'NONE', #43036, .T. ) ;
#44602 = FILL_AREA_STYLE_COLOUR ( '', #11775 ) ;
#44603 = DIRECTION ( 'NONE',  ( -0.5000000000000003331, 0.8660254037844383745, 0.000000000000000000 ) ) ;
#44604 = EDGE_CURVE ( 'NONE', #62964, #31013, #61706, .T. ) ;
#44605 =( BOUNDED_CURVE ( )  B_SPLINE_CURVE ( 2, ( #40583, #61999, #33544, #28227, #44498, #65902, #17733, #33877, #55341, #50091, #1821 ),
 .UNSPECIFIED., .F., .F. ) 
 B_SPLINE_CURVE_WITH_KNOTS ( ( 3, 2, 2, 2, 2, 3 ),
 ( 0.5108695652173792512, 0.5130434782608574995, 0.5152173913043356368, 0.5173913043478138851, 0.5195652173912920224, 0.5217391304347702707 ),
 .UNSPECIFIED. ) 
 CURVE ( )  GEOMETRIC_REPRESENTATION_ITEM ( )  RATIONAL_B_SPLINE_CURVE ( ( 1.000000000000272449, 0.9510565162948810825, 1.000000000000000000, 0.9510565162951535312, 1.000000000000000000, 0.9510565162951535312, 1.000000000000000000, 0.9510565162951535312, 1.000000000000000000, 0.9510565162954309759, 0.9999999999997225553 ) ) 
 REPRESENTATION_ITEM ( '' )  );
#44606 = CARTESIAN_POINT ( 'NONE',  ( -110.7570736234661837, -5.598654528085801552, 7.705886871421367523 ) ) ;
#44607 = FILL_AREA_STYLE ('',( #8663 ) ) ;
#44608 = CARTESIAN_POINT ( 'NONE',  ( 9.827790563157511022E-16, 87.30187232391182306, -8.025000000000000355 ) ) ;
#44609 = VERTEX_POINT ( 'NONE', #16588 ) ;
#44610 = DIRECTION ( 'NONE',  ( 1.000000000000000000, 0.000000000000000000, 0.000000000000000000 ) ) ;
#44611 = CARTESIAN_POINT ( 'NONE',  ( -8.750000000000001776, 25.24999999999998934, 4.000000000000000000 ) ) ;
#44612 = CARTESIAN_POINT ( 'NONE',  ( 7.750000000000001776, 31.24999999999998579, 3.750000000000000000 ) ) ;
#44613 = FACE_OUTER_BOUND ( 'NONE', #63467, .T. ) ;
#44614 = ORIENTED_EDGE ( 'NONE', *, *, #18883, .F. ) ;
#44615 = CARTESIAN_POINT ( 'NONE',  ( -156.8050000000000068, -8.437984349512085203, 5.166775262442717831E-16 ) ) ;
#44616 = FACE_OUTER_BOUND ( 'NONE', #6308, .T. ) ;
#44617 = CARTESIAN_POINT ( 'NONE',  ( -174.4449999999999932, 0.000000000000000000, 8.024999999999991473 ) ) ;
#44618 = EDGE_CURVE ( 'NONE', #32368, #61460, #48252, .T. ) ;
#44619 = CARTESIAN_POINT ( 'NONE',  ( -155.8449999999999704, -7.632228543268599452, 2.479861379858951054 ) ) ;
#44620 = EDGE_LOOP ( 'NONE', ( #53767, #17070, #65642, #61981 ) ) ;
#44621 =( NAMED_UNIT ( * ) PLANE_ANGLE_UNIT ( ) SI_UNIT ( $, .RADIAN. ) );
#44622 = PRESENTATION_LAYER_ASSIGNMENT (  '', '', ( #5238 ) ) ;
#44623 = ADVANCED_FACE ( 'NONE', ( #37017 ), #6691, .T. ) ;
#44624 = CARTESIAN_POINT ( 'NONE',  ( -7.632228543268608334, 150.8429263765338249, 2.479861379858952830 ) ) ;
#44625 = CARTESIAN_POINT ( 'NONE',  ( -71.30499999999997840, 8.437984349512085203, -1.550032578732815448E-15 ) ) ;
#44626 = CARTESIAN_POINT ( 'NONE',  ( -39.06014859142244688, -13.20604375391146945, 2.745267173635231650 ) ) ;
#44627 = AXIS2_PLACEMENT_3D ( 'NONE', #49387, #1113, #27885 ) ;
#44628 = CARTESIAN_POINT ( 'NONE',  ( -73.34499999999999886, 7.632228543268599452, -2.479861379858951942 ) ) ;
#44629 = CARTESIAN_POINT ( 'NONE',  ( 5.598654528085805993, 151.3549999999999898, 7.705886871421374629 ) ) ;
#44630 = CARTESIAN_POINT ( 'NONE',  ( -2.754976799268631815, 2.005084411318701409, -7.000000000000003553 ) ) ;
#44631 = DIRECTION ( 'NONE',  ( 0.5792071321891931746, -0.5736185108958206103, -0.5792071321891952840 ) ) ;
#44632 = UNCERTAINTY_MEASURE_WITH_UNIT (LENGTH_MEASURE( 1.000000000000000082E-05 ), #60415, 'distance_accuracy_value', 'NONE');
#44633 = DIRECTION ( 'NONE',  ( 0.000000000000000000, 1.000000000000000000, 0.000000000000000000 ) ) ;
#44634 = SURFACE_STYLE_FILL_AREA ( #22442 ) ;
#44635 = CARTESIAN_POINT ( 'NONE',  ( 59.00000000000000000, 11.99999999999999822, -4.000000000000000000 ) ) ;
#44636 = MECHANICAL_DESIGN_GEOMETRIC_PRESENTATION_REPRESENTATION (  '', ( #51330 ), #50226 ) ;
#44637 = DIRECTION ( 'NONE',  ( -0.000000000000000000, -1.000000000000000000, -0.000000000000000000 ) ) ;
#44638 =( GEOMETRIC_REPRESENTATION_CONTEXT ( 3 ) GLOBAL_UNCERTAINTY_ASSIGNED_CONTEXT ( ( #8646 ) ) GLOBAL_UNIT_ASSIGNED_CONTEXT ( ( #26456, #37063, #26103 ) ) REPRESENTATION_CONTEXT ( 'NONE', 'WORKASPACE' ) );
#44639 = CARTESIAN_POINT ( 'NONE',  ( -120.4429263765338050, -1.166476076187852838E-15, -9.524999999999991473 ) ) ;
#44640 = VECTOR ( 'NONE', #46133, 1000.000000000000000 ) ;
#44641 = CYLINDRICAL_SURFACE ( 'NONE', #47477, 1.000000000000000888 ) ;
#44642 = VERTEX_POINT ( 'NONE', #27076 ) ;
#44643 = ORIENTED_EDGE ( 'NONE', *, *, #58678, .F. ) ;
#44644 = CARTESIAN_POINT ( 'NONE',  ( 0.4142135623730956451, 13.99999999999999645, -35.49999999999999289 ) ) ;
#44645 = EDGE_CURVE ( 'NONE', #62912, #12986, #994, .T. ) ;
#44646 = DIRECTION ( 'NONE',  ( 0.000000000000000000, 0.000000000000000000, 1.000000000000000000 ) ) ;
#44647 = DIRECTION ( 'NONE',  ( -1.000000000000000000, -0.000000000000000000, -0.000000000000000000 ) ) ;
#44648 = CARTESIAN_POINT ( 'NONE',  ( 4.357963766315031684, -6.451785339198144342, 0.7663918866669806595 ) ) ;
#44649 =( LENGTH_UNIT ( ) NAMED_UNIT ( * ) SI_UNIT ( .MILLI., .METRE. ) );
#44650 = ORIENTED_EDGE ( 'NONE', *, *, #28585, .T. ) ;
#44651 = CARTESIAN_POINT ( 'NONE',  ( -108.9549999999999983, -7.632228543268599452, 2.479861379858951054 ) ) ;
#44652 = EDGE_LOOP ( 'NONE', ( #11036, #1129, #1486, #15736 ) ) ;
#44653 = SURFACE_STYLE_USAGE ( .BOTH. , #54110 ) ;
#44654 = CIRCLE ( 'NONE', #64838, 112.9999999999981526 ) ;
#44655 = CARTESIAN_POINT ( 'NONE',  ( 22.25000000000000711, 34.24999999999999289, 3.750000000000000000 ) ) ;
#44656 = ORIENTED_EDGE ( 'NONE', *, *, #23360, .T. ) ;
#44657 = SURFACE_SIDE_STYLE ('',( #38689 ) ) ;
#44658 = DIRECTION ( 'NONE',  ( 0.000000000000000000, 1.000000000000000000, -0.000000000000000000 ) ) ;
#44659 = ORIENTED_EDGE ( 'NONE', *, *, #40209, .T. ) ;
#44660 = DIRECTION ( 'NONE',  ( 1.000000000000000000, 0.000000000000000000, 0.000000000000000000 ) ) ;
#44661 = DIRECTION ( 'NONE',  ( 0.000000000000000000, -0.000000000000000000, 1.000000000000000000 ) ) ;
#44662 = ORIENTED_EDGE ( 'NONE', *, *, #67032, .T. ) ;
#44663 = ORIENTED_EDGE ( 'NONE', *, *, #29598, .F. ) ;
#44664 = CARTESIAN_POINT ( 'NONE',  ( -74.35456378092618479, 8.376853334107019933, -6.482973932537273498 ) ) ;
#44665 = FACE_OUTER_BOUND ( 'NONE', #77, .T. ) ;
#44666 = LINE ( 'NONE', #66059, #11481 ) ;
#44667 = DIRECTION ( 'NONE',  ( 1.000000000000000000, 0.000000000000000000, -0.000000000000000000 ) ) ;
#44668 = VERTEX_POINT ( 'NONE', #26058 ) ;
#44669 = CARTESIAN_POINT ( 'NONE',  ( 2.607480562269071989, 139.5929263765337964, 8.025000000000002132 ) ) ;
#44670 = CARTESIAN_POINT ( 'NONE',  ( -195.0000000000000000, 1.166476076187852838E-15, -9.524999999999991473 ) ) ;
#44671 = CARTESIAN_POINT ( 'NONE',  ( 12.72792206135785698, 115.4999999999999574, 10.50000000000000000 ) ) ;
#44672 = ADVANCED_FACE ( 'NONE', ( #47592 ), #66248, .T. ) ;
#44673 =( NAMED_UNIT ( * ) SI_UNIT ( $, .STERADIAN. ) SOLID_ANGLE_UNIT ( ) );
#44674 = CARTESIAN_POINT ( 'NONE',  ( -9.827790563157511022E-16, 115.4429263765338192, 8.025000000000000355 ) ) ;
#44675 = EDGE_CURVE ( 'NONE', #59308, #52155, #43350, .T. ) ;
#44676 = ORIENTED_EDGE ( 'NONE', *, *, #28729, .F. ) ;
#44677 = ORIENTED_EDGE ( 'NONE', *, *, #59269, .F. ) ;
#44678 = FILL_AREA_STYLE_COLOUR ( '', #30 ) ;
#44679 =( NAMED_UNIT ( * ) PLANE_ANGLE_UNIT ( ) SI_UNIT ( $, .RADIAN. ) );
#44680 = DIRECTION ( 'NONE',  ( 0.5000000000000003331, 0.8660254037844384856, 0.000000000000000000 ) ) ;
#44681 = CARTESIAN_POINT ( 'NONE',  ( -129.3549999999999898, -4.716976649647093289, -6.492361379858945902 ) ) ;
#44682 = FACE_OUTER_BOUND ( 'NONE', #66943, .T. ) ;
#44683 = CARTESIAN_POINT ( 'NONE',  ( -76.75000000000000000, 4.336808689942018722E-16, 6.000000000000001776 ) ) ;
#44684 = VERTEX_POINT ( 'NONE', #48612 ) ;
#44685 = B_SPLINE_CURVE_WITH_KNOTS ( 'NONE', 3,
 ( #26784, #48313, #7, #704, #54233, #6053 ),
 .UNSPECIFIED., .F., .F.,
 ( 4, 2, 4 ),
 ( 0.005386537104126975541, 0.008060814333094815098, 0.01073509156206265379 ),
 .UNSPECIFIED. ) ;
#44686 = ADVANCED_FACE ( 'NONE', ( #53165 ), #307, .T. ) ;
#44687 = CARTESIAN_POINT ( 'NONE',  ( -106.4929263765338021, -8.102448949553174629, 5.886773742842742685 ) ) ;
#44688 = CARTESIAN_POINT ( 'NONE',  ( -108.0570736234661666, 0.000000000000000000, 9.524999999999991473 ) ) ;
#44689 =( LENGTH_UNIT ( ) NAMED_UNIT ( * ) SI_UNIT ( .MILLI., .METRE. ) );
#44690 = EDGE_LOOP ( 'NONE', ( #9695, #12601, #40526, #13934 ) ) ;
#44691 = EDGE_LOOP ( 'NONE', ( #62844, #53831, #68894, #37667 ) ) ;
#44692 = LINE ( 'NONE', #28795, #6976 ) ;
#44693 = AXIS2_PLACEMENT_3D ( 'NONE', #26957, #36901, #4475 ) ;
#44694 = DIRECTION ( 'NONE',  ( 0.000000000000000000, 0.000000000000000000, -1.000000000000000000 ) ) ;
#44695 = CARTESIAN_POINT ( 'NONE',  ( -50.60499999999996845, 6.826472737025113702, -4.959722759717902107 ) ) ;
#44696 = VERTEX_POINT ( 'NONE', #61191 ) ;
#44697 = CARTESIAN_POINT ( 'NONE',  ( 51.49999999999998579, 2.837994680254535968E-15, -10.49999999999999822 ) ) ;
#44698 = FILL_AREA_STYLE_COLOUR ( '', #36072 ) ;
#44700 = COLOUR_RGB ( '', 0.08235294, 0.09019608, 0.10196078) ;
#44699 = CARTESIAN_POINT ( 'NONE',  ( 71.18918918918917882, 14.09971791521133255, 9.500000000000000000 ) ) ;
#44701 = DIRECTION ( 'NONE',  ( 0.000000000000000000, 0.000000000000000000, -1.000000000000000000 ) ) ;
#44702 = ADVANCED_FACE ( 'NONE', ( #38749, #12998 ), #12647, .T. ) ;
#44703 = CARTESIAN_POINT ( 'NONE',  ( -182.9949999999999761, -6.826472737025113702, 4.959722759717902107 ) ) ;
#44704 = VERTEX_POINT ( 'NONE', #7390 ) ;
#44705 = DIRECTION ( 'NONE',  ( 0.000000000000000000, 1.000000000000000000, 0.000000000000000000 ) ) ;
#44706 = ADVANCED_FACE ( 'NONE', ( #33420 ), #49970, .T. ) ;
#44707 = CARTESIAN_POINT ( 'NONE',  ( 2.607480562269113733, 116.7070736234661723, 8.024999999999973710 ) ) ;
#44708 = CARTESIAN_POINT ( 'NONE',  ( -34.99999999999992895, 112.9999999999999858, 7.500000000000000000 ) ) ;
#44710 = FACE_OUTER_BOUND ( 'NONE', #40921, .T. ) ;
#44709 = AXIS2_PLACEMENT_3D ( 'NONE', #40626, #25113, #34287 ) ;
#44711 = CIRCLE ( 'NONE', #7594, 0.2500000000000002220 ) ;
#44712 = CARTESIAN_POINT ( 'NONE',  ( -95.54499999999998749, -7.632228543268600340, -2.479861379858950166 ) ) ;
#44713 = CARTESIAN_POINT ( 'NONE',  ( 9.058813317711338797, 115.9549999999999841, -2.943386871421372675 ) ) ;
#44714 = CARTESIAN_POINT ( 'NONE',  ( -80.84499999999998465, -7.632228543268599452, 2.479861379858951054 ) ) ;
#44715 = CARTESIAN_POINT ( 'NONE',  ( 10.00000000000000711, 50.00000000000000000, -60.00000000000000000 ) ) ;
#44716 = CARTESIAN_POINT ( 'NONE',  ( -8.437984349512095861, 141.6929263765338192, -5.166775262442723748E-16 ) ) ;
#44717 = CARTESIAN_POINT ( 'NONE',  ( -4.500000000000002665, 21.74999999999998579, -3.750000000000000000 ) ) ;
#44718 = UNCERTAINTY_MEASURE_WITH_UNIT (LENGTH_MEASURE( 1.000000000000000082E-05 ), #9193, 'distance_accuracy_value', 'NONE');
#44719 =( NAMED_UNIT ( * ) PLANE_ANGLE_UNIT ( ) SI_UNIT ( $, .RADIAN. ) );
#44720 = DIRECTION ( 'NONE',  ( 0.000000000000000000, 0.000000000000000000, 1.000000000000000000 ) ) ;
#44721 = ORIENTED_EDGE ( 'NONE', *, *, #32228, .F. ) ;
#44722 = CARTESIAN_POINT ( 'NONE',  ( -128.9929263765338305, 8.102448949553171076, -5.886773742842744461 ) ) ;
#44723 =( NAMED_UNIT ( * ) PLANE_ANGLE_UNIT ( ) SI_UNIT ( $, .RADIAN. ) );
#44724 = CARTESIAN_POINT ( 'NONE',  ( -140.0949999999999989, -2.607480562269071545, -8.024999999999991473 ) ) ;
#44725 = FACE_OUTER_BOUND ( 'NONE', #57773, .T. ) ;
#44726 =( NAMED_UNIT ( * ) SI_UNIT ( $, .STERADIAN. ) SOLID_ANGLE_UNIT ( ) );
#44727 = CARTESIAN_POINT ( 'NONE',  ( -173.5429263765338135, 9.058813317711329915, 2.943386871421369566 ) ) ;
#44728 = VERTEX_POINT ( 'NONE', #23547 ) ;
#44729 = ORIENTED_EDGE ( 'NONE', *, *, #61417, .F. ) ;
#44730 = CARTESIAN_POINT ( 'NONE',  ( -47.71347897792735182, -13.42724224818812218, 0.9185643661976420349 ) ) ;
#44731 = FACE_OUTER_BOUND ( 'NONE', #58995, .T. ) ;
#44732 = EDGE_CURVE ( 'NONE', #12986, #28296, #60663, .T. ) ;
#44733 =( GEOMETRIC_REPRESENTATION_CONTEXT ( 3 ) GLOBAL_UNCERTAINTY_ASSIGNED_CONTEXT ( ( #57931 ) ) GLOBAL_UNIT_ASSIGNED_CONTEXT ( ( #35758, #24149, #57195 ) ) REPRESENTATION_CONTEXT ( 'NONE', 'WORKASPACE' ) );
#44734 = CYLINDRICAL_SURFACE ( 'NONE', #30437, 8.025000000000000355 ) ;
#44735 = COLOUR_RGB ( '', 0.40784314, 0.44705882, 0.49803922) ;
#44736 = DIRECTION ( 'NONE',  ( -0.000000000000000000, -0.000000000000000000, 1.000000000000000000 ) ) ;
#44737 = PRESENTATION_STYLE_ASSIGNMENT (( #49991 ) ) ;
#44738 = VERTEX_POINT ( 'NONE', #39085 ) ;
#44739 = CARTESIAN_POINT ( 'NONE',  ( -143.1549999999999727, 7.632228543268600340, 2.479861379858949277 ) ) ;
#44740 = ORIENTED_EDGE ( 'NONE', *, *, #12101, .F. ) ;
#44741 = ORIENTED_EDGE ( 'NONE', *, *, #21562, .T. ) ;
#44742 = CARTESIAN_POINT ( 'NONE',  ( 34.99999999999992895, 110.4999999999999858, -9.500000000000000000 ) ) ;
#44743 = FACE_BOUND ( 'NONE', #36062, .T. ) ;
#44744 = ORIENTED_EDGE ( 'NONE', *, *, #64011, .T. ) ;
#44745 = PRODUCT_DEFINITION_SHAPE ( 'NONE', 'NONE',  #69722 ) ;
#44746 = DIRECTION ( 'NONE',  ( 1.000000000000000000, 0.000000000000000000, 0.000000000000000000 ) ) ;
#44747 = DIRECTION ( 'NONE',  ( -1.000000000000000000, -0.000000000000000000, -0.000000000000000000 ) ) ;
#44748 = CARTESIAN_POINT ( 'NONE',  ( 0.000000000000000000, 133.4449999999999932, -9.525000000000000355 ) ) ;
#44749 = LINE ( 'NONE', #17650, #62033 ) ;
#44750 = ORIENTED_EDGE ( 'NONE', *, *, #10624, .F. ) ;
#44751 = EDGE_CURVE ( 'NONE', #57062, #27715, #54851, .T. ) ;
#44752 = CARTESIAN_POINT ( 'NONE',  ( 5.598654528085805993, 139.3549999999999898, 7.705886871421374629 ) ) ;
#44753 = CARTESIAN_POINT ( 'NONE',  ( -55.40499999999997272, -2.607480562269069768, 8.024999999999991473 ) ) ;
#44754 = CARTESIAN_POINT ( 'NONE',  ( 41.47640344042797977, 107.6239624391513132, -3.580003982101955806 ) ) ;
#44755 = ORIENTED_EDGE ( 'NONE', *, *, #65927, .T. ) ;
#44756 = CARTESIAN_POINT ( 'NONE',  ( -6.826472737025120807, 111.3929263765337936, -4.959722759717907437 ) ) ;
#44757 = DIRECTION ( 'NONE',  ( -0.000000000000000000, -0.000000000000000000, -1.000000000000000000 ) ) ;
#44758 = UNCERTAINTY_MEASURE_WITH_UNIT (LENGTH_MEASURE( 1.000000000000000082E-05 ), #30737, 'distance_accuracy_value', 'NONE');
#44759 = VECTOR ( 'NONE', #24329, 1000.000000000000000 ) ;
#44760 = VECTOR ( 'NONE', #41036, 1000.000000000000000 ) ;
#44761 = ADVANCED_FACE ( 'NONE', ( #18639 ), #45414, .T. ) ;
#44762 = ADVANCED_FACE ( 'NONE', ( #27764 ), #60478, .F. ) ;
#44763 = VERTEX_POINT ( 'NONE', #17937 ) ;
#44764 = ORIENTED_EDGE ( 'NONE', *, *, #56526, .T. ) ;
#44765 = CARTESIAN_POINT ( 'NONE',  ( 19.89974874213239886, 114.9999999999999574, 10.49999999999999645 ) ) ;
#44766 = CARTESIAN_POINT ( 'NONE',  ( -34.99999999999992895, 113.4999999999999858, 7.000000000000000000 ) ) ;
#44767 = CARTESIAN_POINT ( 'NONE',  ( -158.6050000000000182, 6.826472737025113702, -4.959722759717902107 ) ) ;
#44768 = EDGE_LOOP ( 'NONE', ( #53002, #56661, #39463, #34919, #53361, #3105 ) ) ;
#44769 = DIRECTION ( 'NONE',  ( 1.000000000000000000, 0.000000000000000000, -1.300977106640434891E-16 ) ) ;
#44770 = UNCERTAINTY_MEASURE_WITH_UNIT (LENGTH_MEASURE( 1.000000000000000082E-05 ), #20334, 'distance_accuracy_value', 'NONE');
#44771 = EDGE_CURVE ( 'NONE', #12385, #38874, #40532, .T. ) ;
#44772 =( NAMED_UNIT ( * ) SI_UNIT ( $, .STERADIAN. ) SOLID_ANGLE_UNIT ( ) );
#44773 = DIRECTION ( 'NONE',  ( 0.000000000000000000, 0.000000000000000000, 1.000000000000000000 ) ) ;
#44774 = ORIENTED_EDGE ( 'NONE', *, *, #12860, .T. ) ;
#44776 = EDGE_CURVE ( 'NONE', #53321, #36102, #10130, .T. ) ;
#44775 = EDGE_LOOP ( 'NONE', ( #9115, #9923, #29841, #60269 ) ) ;
#44777 = CARTESIAN_POINT ( 'NONE',  ( -45.13108574187265987, 8.257324008952721783, -3.517130741219093526 ) ) ;
#44778 = CYLINDRICAL_SURFACE ( 'NONE', #52665, 0.2500000000000002220 ) ;
#44779 = CARTESIAN_POINT ( 'NONE',  ( -74.90499999999997272, 2.607480562269068880, -8.024999999999993250 ) ) ;
#44780 = ORIENTED_EDGE ( 'NONE', *, *, #14885, .T. ) ;
#44781 = DIRECTION ( 'NONE',  ( 0.000000000000000000, 0.000000000000000000, 1.000000000000000000 ) ) ;
#44782 =( GEOMETRIC_REPRESENTATION_CONTEXT ( 3 ) GLOBAL_UNCERTAINTY_ASSIGNED_CONTEXT ( ( #39142 ) ) GLOBAL_UNIT_ASSIGNED_CONTEXT ( ( #22990, #43780, #34225 ) ) REPRESENTATION_CONTEXT ( 'NONE', 'WORKASPACE' ) );
#44783 = CARTESIAN_POINT ( 'NONE',  ( -9.250000000000003553, 27.74999999999998934, 4.000000000000000000 ) ) ;
#44784 = VERTEX_POINT ( 'NONE', #56957 ) ;
#44785 = DIRECTION ( 'NONE',  ( -1.000000000000000000, 0.000000000000000000, 0.000000000000000000 ) ) ;
#44786 = COLOUR_RGB ( '', 0.66274510, 0.83137255, 0.94901961) ;
#44788 = SURFACE_STYLE_FILL_AREA ( #1781 ) ;
#44787 = CARTESIAN_POINT ( 'NONE',  ( -53.90707362346616094, -3.094860106618429807, 9.524999999999991473 ) ) ;
#44789 =( GEOMETRIC_REPRESENTATION_CONTEXT ( 3 ) GLOBAL_UNCERTAINTY_ASSIGNED_CONTEXT ( ( #62822 ) ) GLOBAL_UNIT_ASSIGNED_CONTEXT ( ( #12110, #27914, #22683 ) ) REPRESENTATION_CONTEXT ( 'NONE', 'WORKASPACE' ) );
#44790 = EDGE_CURVE ( 'NONE', #58402, #66309, #37833, .T. ) ;
#44791 = CARTESIAN_POINT ( 'NONE',  ( 8.102448949553181734, 135.3950000000000102, 5.886773742842750679 ) ) ;
#44792 = CARTESIAN_POINT ( 'NONE',  ( -102.7449999999999903, 4.716976649647094177, 6.492361379858945902 ) ) ;
#44793 = CIRCLE ( 'NONE', #40297, 0.2500000000000002220 ) ;
#44794 = SURFACE_SIDE_STYLE ('',( #28185 ) ) ;
#44795 = ADVANCED_FACE ( 'NONE', ( #63276 ), #46086, .T. ) ;
#44796 =( GEOMETRIC_REPRESENTATION_CONTEXT ( 3 ) GLOBAL_UNCERTAINTY_ASSIGNED_CONTEXT ( ( #63570 ) ) GLOBAL_UNIT_ASSIGNED_CONTEXT ( ( #29101, #3390, #34742 ) ) REPRESENTATION_CONTEXT ( 'NONE', 'WORKASPACE' ) );
#44798 = DIRECTION ( 'NONE',  ( -1.000000000000000000, 0.000000000000000000, 0.000000000000000000 ) ) ;
#44797 = DIRECTION ( 'NONE',  ( -1.000000000000000000, 0.000000000000000000, 0.000000000000000000 ) ) ;
#44799 = CARTESIAN_POINT ( 'NONE',  ( -149.9929263765338021, 8.102448949553171076, -5.886773742842744461 ) ) ;
#44800 = CARTESIAN_POINT ( 'NONE',  ( -170.9950000000000330, -6.826472737025115478, 4.959722759717900331 ) ) ;
#44801 = VECTOR ( 'NONE', #59097, 1000.000000000000000 ) ;
#44802 = LINE ( 'NONE', #17704, #9664 ) ;
#44803 = CARTESIAN_POINT ( 'NONE',  ( -195.0000000000000000, 0.000000000000000000, 0.000000000000000000 ) ) ;
#44804 = ORIENTED_EDGE ( 'NONE', *, *, #2739, .T. ) ;
#44805 = ORIENTED_EDGE ( 'NONE', *, *, #15823, .T. ) ;
#44806 = CARTESIAN_POINT ( 'NONE',  ( -63.44292637653379785, -1.166476076187852838E-15, -9.524999999999991473 ) ) ;
#44807 = CYLINDRICAL_SURFACE ( 'NONE', #36539, 4.999999999999997335 ) ;
#44808 = COLOUR_RGB ( '', 0.72549020, 0.75294118, 0.79215686) ;
#44809 = LINE ( 'NONE', #22982, #56113 ) ;
#44810 = CARTESIAN_POINT ( 'NONE',  ( -78.89292637653380780, -8.102448949553174629, -5.886773742842741797 ) ) ;
#44811 = AXIS2_PLACEMENT_3D ( 'NONE', #57983, #47827, #63246 ) ;
#44812 = ORIENTED_EDGE ( 'NONE', *, *, #101, .T. ) ;
#44813 = CARTESIAN_POINT ( 'NONE',  ( -174.2050000000000125, -2.607480562269071545, -8.024999999999991473 ) ) ;
#44814 = ORIENTED_EDGE ( 'NONE', *, *, #30321, .T. ) ;
#44815 = CARTESIAN_POINT ( 'NONE',  ( 74.89452121010485541, 14.00000000000000000, 66.39042820928573008 ) ) ;
#44817 = EDGE_CURVE ( 'NONE', #36852, #31700, #29238, .T. ) ;
#44816 = CARTESIAN_POINT ( 'NONE',  ( 23.21231517720797655, 117.4999999999999716, -9.500000000000000000 ) ) ;
#44818 = CARTESIAN_POINT ( 'NONE',  ( 27.00000000000001776, 14.00000000000000000, 29.68999999999999417 ) ) ;
#44819 = CARTESIAN_POINT ( 'NONE',  ( 18.25000000000000711, 33.74999999999999289, -3.750000000000000000 ) ) ;
#44820 = CARTESIAN_POINT ( 'NONE',  ( 4.716976649647096842, 152.8570736234661638, 6.492361379858953896 ) ) ;
#44821 = AXIS2_PLACEMENT_3D ( 'NONE', #64626, #60028, #5858 ) ;
#44822 = ORIENTED_EDGE ( 'NONE', *, *, #36079, .F. ) ;
#44823 = EDGE_CURVE ( 'NONE', #26409, #45813, #6748, .T. ) ;
#44824 = DIRECTION ( 'NONE',  ( -1.000000000000000000, 0.000000000000000000, 0.000000000000000000 ) ) ;
#44825 = CARTESIAN_POINT ( 'NONE',  ( -9.827790563157511022E-16, 136.4429263765338192, 8.025000000000000355 ) ) ;
#44826 = CARTESIAN_POINT ( 'NONE',  ( -84.20499999999995566, -2.607480562269071545, -8.024999999999991473 ) ) ;
#44827 = FACE_OUTER_BOUND ( 'NONE', #61638, .T. ) ;
#44828 = CARTESIAN_POINT ( 'NONE',  ( 5.598654528085809545, 131.2549999999999955, -7.705886871421373741 ) ) ;
#44829 = UNCERTAINTY_MEASURE_WITH_UNIT (LENGTH_MEASURE( 1.000000000000000082E-05 ), #25654, 'distance_accuracy_value', 'NONE');
#44830 = AXIS2_PLACEMENT_3D ( 'NONE', #47400, #64582, #36504 ) ;
#44831 = DIRECTION ( 'NONE',  ( 1.000000000000000000, 0.000000000000000000, 0.000000000000000000 ) ) ;
#44832 = EDGE_CURVE ( 'NONE', #8511, #22643, #51704, .T. ) ;
#44833 = CARTESIAN_POINT ( 'NONE',  ( -169.3429263765337964, -9.058813317711329915, 2.943386871421371787 ) ) ;
#44834 = DIRECTION ( 'NONE',  ( 0.000000000000000000, 0.000000000000000000, -1.000000000000000000 ) ) ;
#44835 = SURFACE_SIDE_STYLE ('',( #60955 ) ) ;
#44836 = ORIENTED_EDGE ( 'NONE', *, *, #22975, .F. ) ;
#44837 = MECHANICAL_DESIGN_GEOMETRIC_PRESENTATION_REPRESENTATION (  '', ( #37016 ), #56029 ) ;
#44838 =( NAMED_UNIT ( * ) PLANE_ANGLE_UNIT ( ) SI_UNIT ( $, .RADIAN. ) );
#44839 = CARTESIAN_POINT ( 'NONE',  ( -52.04499999999998039, 7.632228543268600340, 2.479861379858949277 ) ) ;
#44840 = EDGE_LOOP ( 'NONE', ( #18158, #10278, #65272, #68176 ) ) ;
#44841 = FACE_OUTER_BOUND ( 'NONE', #61888, .T. ) ;
#44842 = DIRECTION ( 'NONE',  ( -0.000000000000000000, -0.6449798928094537809, 0.7641995406119435064 ) ) ;
#44843 = CARTESIAN_POINT ( 'NONE',  ( -138.9570736234661865, 9.058813317711329915, -2.943386871421373119 ) ) ;
#44844 =( NAMED_UNIT ( * ) PLANE_ANGLE_UNIT ( ) SI_UNIT ( $, .RADIAN. ) );
#44845 = VERTEX_POINT ( 'NONE', #9482 ) ;
#44846 = CARTESIAN_POINT ( 'NONE',  ( -53.01121866695765306, -10.53184416402257284, 3.891476709836705794 ) ) ;
#44847 = CARTESIAN_POINT ( 'NONE',  ( -58.19499999999999318, 8.437984349512086979, -1.550032578732815448E-15 ) ) ;
#44848 =( NAMED_UNIT ( * ) SI_UNIT ( $, .STERADIAN. ) SOLID_ANGLE_UNIT ( ) );
#44849 = VERTEX_POINT ( 'NONE', #14050 ) ;
#44850 = PRESENTATION_LAYER_ASSIGNMENT (  '', '', ( #5456 ) ) ;
#44851 = ADVANCED_FACE ( 'NONE', ( #35511 ), #29872, .T. ) ;
#44852 = CARTESIAN_POINT ( 'NONE',  ( -75.00000000000000000, 8.092690183933195058, 5.807220890438696159 ) ) ;
#44853 = CARTESIAN_POINT ( 'NONE',  ( -113.6049999999999898, 6.826472737025113702, -4.959722759717902107 ) ) ;
#44854 = ORIENTED_EDGE ( 'NONE', *, *, #65348, .F. ) ;
#44855 = CARTESIAN_POINT ( 'NONE',  ( -9.827790563157511022E-16, 119.5570736234661524, 8.025000000000000355 ) ) ;
#44856 = CARTESIAN_POINT ( 'NONE',  ( 21.75000000000001066, 21.99999999999998224, 4.000000000000000000 ) ) ;
#44857 = CARTESIAN_POINT ( 'NONE',  ( -152.4570736234661581, -9.058813317711329915, 2.943386871421371787 ) ) ;
#44858 = CARTESIAN_POINT ( 'NONE',  ( 4.041451884327376121, 7.000000000000007105, 7.500000000000000000 ) ) ;
#44859 = CARTESIAN_POINT ( 'NONE',  ( -9.058813317711337021, 146.0449999999999875, -2.943386871421374895 ) ) ;
#44860 = CARTESIAN_POINT ( 'NONE',  ( -87.05707362346618083, 0.000000000000000000, 9.524999999999991473 ) ) ;
#44861 = AXIS2_PLACEMENT_3D ( 'NONE', #34784, #8061, #2741 ) ;
#44862 = DIRECTION ( 'NONE',  ( 0.000000000000000000, 0.000000000000000000, -1.000000000000000000 ) ) ;
#44863 = ORIENTED_EDGE ( 'NONE', *, *, #23980, .F. ) ;
#44865 = SURFACE_SIDE_STYLE ('',( #1510 ) ) ;
#44864 = DIRECTION ( 'NONE',  ( 0.000000000000000000, 0.000000000000000000, -1.000000000000000000 ) ) ;
#44866 = CARTESIAN_POINT ( 'NONE',  ( -34.99999999999999289, 99.99999999999998579, 3.500000000000000000 ) ) ;
#44867 = CARTESIAN_POINT ( 'NONE',  ( -126.2049999999999841, -2.607480562269071545, -8.024999999999991473 ) ) ;
#44868 = DIRECTION ( 'NONE',  ( 1.000000000000000000, 0.000000000000000000, 0.000000000000000000 ) ) ;
#44869 = LINE ( 'NONE', #65588, #42703 ) ;
#44870 = CARTESIAN_POINT ( 'NONE',  ( -137.0949999999999989, -2.607480562269071545, -8.024999999999991473 ) ) ;
#44871 = AXIS2_PLACEMENT_3D ( 'NONE', #18977, #62256, #34823 ) ;
#44872 = CARTESIAN_POINT ( 'NONE',  ( -133.4950000000000045, 6.826472737025113702, -4.959722759717902107 ) ) ;
#44873 = CARTESIAN_POINT ( 'NONE',  ( 93.00000000000000000, 13.00000000000000178, 0.000000000000000000 ) ) ;
#44874 = EDGE_CURVE ( 'NONE', #60366, #8099, #58429, .T. ) ;
#44875 = VERTEX_POINT ( 'NONE', #57295 ) ;
#44876 = DIRECTION ( 'NONE',  ( 0.000000000000000000, 1.000000000000000000, -0.000000000000000000 ) ) ;
#44877 = DIRECTION ( 'NONE',  ( 0.000000000000000000, 0.000000000000000000, 1.000000000000000000 ) ) ;
#44878 = CARTESIAN_POINT ( 'NONE',  ( -135.4429263765338192, -1.166476076187852838E-15, -9.524999999999991473 ) ) ;
#44879 = CARTESIAN_POINT ( 'NONE',  ( -179.2429263765338021, 5.598654528085804216, 7.705886871421366635 ) ) ;
#44880 =( BOUNDED_CURVE ( )  B_SPLINE_CURVE ( 2, ( #44563, #34993, #65959, #8278, #17790, #33945, #55404, #25133, #19144, #62420, #14952 ),
 .UNSPECIFIED., .F., .F. ) 
 B_SPLINE_CURVE_WITH_KNOTS ( ( 3, 2, 2, 2, 2, 3 ),
 ( 0.1521739130434745513, 0.1543478260869527441, 0.1565217391304309924, 0.1586956521739091852, 0.1608695652173874058, 0.1630434782608656263 ),
 .UNSPECIFIED. ) 
 CURVE ( )  GEOMETRIC_REPRESENTATION_ITEM ( )  RATIONAL_B_SPLINE_CURVE ( ( 1.000000000000083711, 0.9510565162950698204, 1.000000000000000000, 0.9510565162951535312, 1.000000000000000000, 0.9510565162951535312, 1.000000000000000000, 0.9510565162951535312, 1.000000000000000000, 0.9510565162952422380, 0.9999999999999112932 ) ) 
 REPRESENTATION_ITEM ( '' )  );
#44881 = FILL_AREA_STYLE ('',( #33591 ) ) ;
#44882 = CARTESIAN_POINT ( 'NONE',  ( -52.79499999999997328, 2.607480562269068880, -8.024999999999993250 ) ) ;
#44883 = COLOUR_RGB ( '', 0.31764706, 0.68627451, 0.89019608) ;
#44884 = CARTESIAN_POINT ( 'NONE',  ( 10.58578643762692195, 17.78868675966042190, -3.198396408832238080E-15 ) ) ;
#44885 = CARTESIAN_POINT ( 'NONE',  ( 52.75000000000000000, 24.74999999999998224, -4.000000000000000000 ) ) ;
#44886 = SURFACE_SIDE_STYLE ('',( #60324 ) ) ;
#44887 = CARTESIAN_POINT ( 'NONE',  ( 0.000000000000000000, 110.4999999999999858, 23.00000000000000000 ) ) ;
#44888 = SURFACE_SIDE_STYLE ('',( #27939 ) ) ;
#44889 = CARTESIAN_POINT ( 'NONE',  ( -97.19292637653379074, -10.01517768586948698, 6.132527647946031529E-16 ) ) ;
#44890 = SHAPE_DEFINITION_REPRESENTATION ( #9725, #21747 ) ;
#44891 = STYLED_ITEM ( 'NONE', ( #16319 ), #19793 ) ;
#44892 = CARTESIAN_POINT ( 'NONE',  ( -162.9570736234661865, 9.058813317711329915, -2.943386871421373119 ) ) ;
#44893 = SURFACE_STYLE_FILL_AREA ( #28658 ) ;
#44894 = DIRECTION ( 'NONE',  ( 1.000000000000000000, -0.000000000000000000, 0.000000000000000000 ) ) ;
#44895 = CARTESIAN_POINT ( 'NONE',  ( -41.84210526315788314, 107.2928455055531600, 3.500000000000000444 ) ) ;
#44896 = CIRCLE ( 'NONE', #14524, 0.5000000000000004441 ) ;
#44897 =( LENGTH_UNIT ( ) NAMED_UNIT ( * ) SI_UNIT ( .MILLI., .METRE. ) );
#44898 = ORIENTED_EDGE ( 'NONE', *, *, #21949, .T. ) ;
#44899 = ADVANCED_FACE ( 'NONE', ( #24574 ), #56193, .T. ) ;
#44900 = CARTESIAN_POINT ( 'NONE',  ( -56.63152288741350304, -7.947250274547568161, -1.331476843523650588 ) ) ;
#44901 = ORIENTED_EDGE ( 'NONE', *, *, #218, .T. ) ;
#44902 = DIRECTION ( 'NONE',  ( -1.000000000000000000, -0.000000000000000000, -0.000000000000000000 ) ) ;
#44903 = CIRCLE ( 'NONE', #46051, 25.00000000000001421 ) ;
#44904 =( GEOMETRIC_REPRESENTATION_CONTEXT ( 3 ) GLOBAL_UNCERTAINTY_ASSIGNED_CONTEXT ( ( #16590 ) ) GLOBAL_UNIT_ASSIGNED_CONTEXT ( ( #4741, #26196, #25503 ) ) REPRESENTATION_CONTEXT ( 'NONE', 'WORKASPACE' ) );
#44905 = CARTESIAN_POINT ( 'NONE',  ( -7.632228543268608334, 121.9570736234661723, 2.479861379858952830 ) ) ;
#44906 = STYLED_ITEM ( 'NONE', ( #26805 ), #44129 ) ;
#44907 = SURFACE_STYLE_FILL_AREA ( #45936 ) ;
#44908 = CARTESIAN_POINT ( 'NONE',  ( 16.75000000000000711, 0.000000000000000000, 3.750000000000000000 ) ) ;
#44910 = EDGE_LOOP ( 'NONE', ( #10703, #60725, #53786, #18578 ) ) ;
#44909 =( GEOMETRIC_REPRESENTATION_CONTEXT ( 3 ) GLOBAL_UNCERTAINTY_ASSIGNED_CONTEXT ( ( #31281 ) ) GLOBAL_UNIT_ASSIGNED_CONTEXT ( ( #62710, #35665, #13853 ) ) REPRESENTATION_CONTEXT ( 'NONE', 'WORKASPACE' ) );
#44911 = DIRECTION ( 'NONE',  ( 0.000000000000000000, 0.000000000000000000, -1.000000000000000000 ) ) ;
#44912 = EDGE_CURVE ( 'NONE', #35108, #16524, #62926, .T. ) ;
#44913 = DIRECTION ( 'NONE',  ( -1.000000000000000000, -0.000000000000000000, 1.300977106640434644E-16 ) ) ;
#44914 = DIRECTION ( 'NONE',  ( 1.000000000000000000, 0.000000000000000000, 0.000000000000000000 ) ) ;
#44915 = CIRCLE ( 'NONE', #957, 0.5000000000000004441 ) ;
#44916 = AXIS2_PLACEMENT_3D ( 'NONE', #167, #6900, #23098 ) ;
#44917 = EDGE_CURVE ( 'NONE', #13814, #28936, #56801, .T. ) ;
#44918 = LINE ( 'NONE', #13912, #33958 ) ;
#44919 = CARTESIAN_POINT ( 'NONE',  ( -93.14499999999999602, -4.716976649647092401, 6.492361379858946790 ) ) ;
#44921 = ORIENTED_EDGE ( 'NONE', *, *, #53058, .T. ) ;
#44920 = VECTOR ( 'NONE', #34906, 1000.000000000000000 ) ;
#44922 = AXIS2_PLACEMENT_3D ( 'NONE', #25096, #46609, #57811 ) ;
#44923 = VECTOR ( 'NONE', #48718, 1000.000000000000000 ) ;
#44924 =( NAMED_UNIT ( * ) SI_UNIT ( $, .STERADIAN. ) SOLID_ANGLE_UNIT ( ) );
#44925 = EDGE_CURVE ( 'NONE', #40436, #24428, #53425, .T. ) ;
#44926 = CARTESIAN_POINT ( 'NONE',  ( 66.49999999999998579, 37.00000000000000000, 4.000000000000000000 ) ) ;
#44927 = VERTEX_POINT ( 'NONE', #15123 ) ;
#44928 = CYLINDRICAL_SURFACE ( 'NONE', #41525, 17.42000000000001236 ) ;
#44929 =( GEOMETRIC_REPRESENTATION_CONTEXT ( 3 ) GLOBAL_UNCERTAINTY_ASSIGNED_CONTEXT ( ( #42636 ) ) GLOBAL_UNIT_ASSIGNED_CONTEXT ( ( #14761, #61880, #36236 ) ) REPRESENTATION_CONTEXT ( 'NONE', 'WORKASPACE' ) );
#44930 = EDGE_CURVE ( 'NONE', #40311, #12077, #27754, .T. ) ;
#44931 = ORIENTED_EDGE ( 'NONE', *, *, #63526, .F. ) ;
#44932 = CARTESIAN_POINT ( 'NONE',  ( -15.98999599679679839, 118.4999999999999716, 9.500000000000000000 ) ) ;
#44933 = ORIENTED_EDGE ( 'NONE', *, *, #9635, .T. ) ;
#44934 = CARTESIAN_POINT ( 'NONE',  ( 60.00000000000000000, 110.4999999999999858, 9.500000000000000000 ) ) ;
#44935 = CARTESIAN_POINT ( 'NONE',  ( -13.75000000000000533, 30.74999999999999289, 3.750000000000000000 ) ) ;
#44937 = VECTOR ( 'NONE', #50295, 1000.000000000000000 ) ;
#44936 = CARTESIAN_POINT ( 'NONE',  ( -7.511572993685798115E-16, -2.500000000000000000, 6.999999999999997335 ) ) ;
#44938 = CARTESIAN_POINT ( 'NONE',  ( -176.1570736234662036, -9.058813317711329915, -2.943386871421370898 ) ) ;
#44939 = FACE_OUTER_BOUND ( 'NONE', #24987, .T. ) ;
#44940 = TOROIDAL_SURFACE ( 'NONE', #14576, 9.525000000000000355, 1.000000000000000888 ) ;
#44941 = CARTESIAN_POINT ( 'NONE',  ( -112.4070736234661894, 3.094860106618428031, -9.524999999999993250 ) ) ;
#44942 = CARTESIAN_POINT ( 'NONE',  ( 44.91886116991580735, 9.999999999999980460, 3.500000000000000000 ) ) ;
#44943 = DIRECTION ( 'NONE',  ( -0.000000000000000000, -1.000000000000000000, 0.000000000000000000 ) ) ;
#44944 = EDGE_LOOP ( 'NONE', ( #6699, #63335, #35465, #15226 ) ) ;
#44945 = CARTESIAN_POINT ( 'NONE',  ( 0.8561460859850872351, 43.00000000000000000, 45.61250543006184444 ) ) ;
#44946 = DIRECTION ( 'NONE',  ( -1.000000000000000000, 0.000000000000000000, 0.000000000000000000 ) ) ;
#44947 = EDGE_LOOP ( 'NONE', ( #6452, #36517, #2247, #34486 ) ) ;
#44948 = CARTESIAN_POINT ( 'NONE',  ( -162.2049999999999557, -2.607480562269071545, -8.024999999999991473 ) ) ;
#44949 = DIRECTION ( 'NONE',  ( -1.000000000000000000, 0.000000000000000000, -0.000000000000000000 ) ) ;
#44950 = DIRECTION ( 'NONE',  ( 0.000000000000000000, 0.000000000000000000, 1.000000000000000000 ) ) ;
#44951 = CARTESIAN_POINT ( 'NONE',  ( -166.9450000000000216, -9.827790563157499189E-16, -8.024999999999991473 ) ) ;
#44952 = CARTESIAN_POINT ( 'NONE',  ( -160.3449999999999989, 7.632228543268599452, -2.479861379858951942 ) ) ;
#44953 = AXIS2_PLACEMENT_3D ( 'NONE', #19455, #18433, #13476 ) ;
#44954 = VECTOR ( 'NONE', #51057, 1000.000000000000000 ) ;
#44955 = EDGE_LOOP ( 'NONE', ( #51294, #33723, #32652, #554 ) ) ;
#44956 = CARTESIAN_POINT ( 'NONE',  ( -9.568252947146934417, 1.427299755870875320, 0.6386920474458039898 ) ) ;
#44957 = STYLED_ITEM ( 'NONE', ( #59437 ), #44686 ) ;
#44958 = CARTESIAN_POINT ( 'NONE',  ( 8.920833891111493941, -2.231456886122029193, -2.548662454712524728 ) ) ;
#44959 = CARTESIAN_POINT ( 'NONE',  ( -76.25499999999999545, -4.716976649647092401, 6.492361379858946790 ) ) ;
#44960 = CARTESIAN_POINT ( 'NONE',  ( -36.08832455125276084, -11.72126376154535521, 1.574586324192390085 ) ) ;
#44961 = CARTESIAN_POINT ( 'NONE',  ( 24.21231517720798010, 112.9999999999999858, 10.00000000000000000 ) ) ;
#44962 = CARTESIAN_POINT ( 'NONE',  ( -71.39499999999998181, -6.826472737025113702, -4.959722759717900331 ) ) ;
#44963 = CARTESIAN_POINT ( 'NONE',  ( 8.102448949553183510, 146.1049999999999898, -5.886773742842746238 ) ) ;
#44964 = CARTESIAN_POINT ( 'NONE',  ( 21.75000000000001066, 22.24999999999998224, 3.750000000000000000 ) ) ;
#44965 =( GEOMETRIC_REPRESENTATION_CONTEXT ( 3 ) GLOBAL_UNCERTAINTY_ASSIGNED_CONTEXT ( ( #68771 ) ) GLOBAL_UNIT_ASSIGNED_CONTEXT ( ( #14219, #47311, #35682 ) ) REPRESENTATION_CONTEXT ( 'NONE', 'WORKASPACE' ) );
#44966 =( GEOMETRIC_REPRESENTATION_CONTEXT ( 3 ) GLOBAL_UNCERTAINTY_ASSIGNED_CONTEXT ( ( #36981 ) ) GLOBAL_UNIT_ASSIGNED_CONTEXT ( ( #11403, #32872, #58917 ) ) REPRESENTATION_CONTEXT ( 'NONE', 'WORKASPACE' ) );
#44967 =( GEOMETRIC_REPRESENTATION_CONTEXT ( 3 ) GLOBAL_UNCERTAINTY_ASSIGNED_CONTEXT ( ( #43397 ) ) GLOBAL_UNIT_ASSIGNED_CONTEXT ( ( #7052, #33105, #49286 ) ) REPRESENTATION_CONTEXT ( 'NONE', 'WORKASPACE' ) );
#44968 = CIRCLE ( 'NONE', #51675, 0.5000000000000004441 ) ;
#44969 = CARTESIAN_POINT ( 'NONE',  ( 3.851859888774471706E-31, -8.500000000000000000, 1.000000000000000888 ) ) ;
#44970 = CIRCLE ( 'NONE', #21379, 3.100000000000005418 ) ;
#44971 = CARTESIAN_POINT ( 'NONE',  ( 47.50000000000000000, 99.99999999999992895, 10.00000000000000000 ) ) ;
#44972 = EDGE_CURVE ( 'NONE', #330, #40347, #59034, .T. ) ;
#44973 = ORIENTED_EDGE ( 'NONE', *, *, #22101, .F. ) ;
#44974 = VECTOR ( 'NONE', #34449, 1000.000000000000000 ) ;
#44975 = ORIENTED_EDGE ( 'NONE', *, *, #52033, .F. ) ;
#44976 = FILL_AREA_STYLE ('',( #24856 ) ) ;
#44977 = PRESENTATION_LAYER_ASSIGNMENT (  '', '', ( #6732 ) ) ;
#44978 = CARTESIAN_POINT ( 'NONE',  ( -132.3570736234661922, 5.598654528085804216, 7.705886871421366635 ) ) ;
#44979 = EDGE_CURVE ( 'NONE', #20918, #49856, #46105, .T. ) ;
#44980 = STYLED_ITEM ( 'NONE', ( #49978 ), #11074 ) ;
#44981 = CARTESIAN_POINT ( 'NONE',  ( -45.00000000000001421, 8.163938725409353836, 6.987118804072284028 ) ) ;
#44982 = CARTESIAN_POINT ( 'NONE',  ( -195.0000000000000000, 0.000000000000000000, 9.524999999999991473 ) ) ;
#44983 = VECTOR ( 'NONE', #41064, 1000.000000000000000 ) ;
#44984 = DIRECTION ( 'NONE',  ( 0.000000000000000000, 0.000000000000000000, 1.000000000000000000 ) ) ;
#44985 = ADVANCED_FACE ( 'NONE', ( #20715 ), #5203, .T. ) ;
#44986 = DIRECTION ( 'NONE',  ( 0.000000000000000000, 0.000000000000000000, 1.000000000000000000 ) ) ;
#44987 = ORIENTED_EDGE ( 'NONE', *, *, #38094, .F. ) ;
#44988 = CARTESIAN_POINT ( 'NONE',  ( -98.60499999999997556, 6.826472737025113702, -4.959722759717902107 ) ) ;
#44989 = EDGE_LOOP ( 'NONE', ( #15412, #20092, #46831, #57796 ) ) ;
#44990 = CARTESIAN_POINT ( 'NONE',  ( 28.00000000000000000, 38.70020753820971748, -89.00000000000000000 ) ) ;
#44991 = PLANE ( 'NONE',  #51241 ) ;
#44992 = EDGE_CURVE ( 'NONE', #34254, #63927, #6336, .T. ) ;
#44993 = ORIENTED_EDGE ( 'NONE', *, *, #39186, .T. ) ;
#44994 = CARTESIAN_POINT ( 'NONE',  ( -66.44292637653380496, -1.166476076187852838E-15, -9.524999999999991473 ) ) ;
#44995 = CARTESIAN_POINT ( 'NONE',  ( 60.00000000000000000, 1.797044900979284448E-15, -12.00000000000000000 ) ) ;
#44996 = ORIENTED_EDGE ( 'NONE', *, *, #53533, .F. ) ;
#44997 = ADVANCED_FACE ( 'NONE', ( #26648 ), #55042, .F. ) ;
#44999 = CARTESIAN_POINT ( 'NONE',  ( -67.55707362346618083, -1.166476076187852838E-15, -9.524999999999991473 ) ) ;
#44998 = AXIS2_PLACEMENT_3D ( 'NONE', #26991, #11184, #26317 ) ;
#45000 = FILL_AREA_STYLE ('',( #33030 ) ) ;
#45001 = CARTESIAN_POINT ( 'NONE',  ( -121.7949999999999875, 2.607480562269068880, -8.024999999999993250 ) ) ;
#45002 = VERTEX_POINT ( 'NONE', #13106 ) ;
#45003 =( BOUNDED_CURVE ( )  B_SPLINE_CURVE ( 3, ( #17002, #26098, #4271, #42685 ),
 .UNSPECIFIED., .F., .F. ) 
 B_SPLINE_CURVE_WITH_KNOTS ( ( 4, 4 ),
 ( 4.712388980384689674, 5.505033981715339308 ),
 .UNSPECIFIED. ) 
 CURVE ( )  GEOMETRIC_REPRESENTATION_ITEM ( )  RATIONAL_B_SPLINE_CURVE ( ( 1.000000000000000000, 0.9483245655077793268, 0.9483245655077793268, 1.000000000000000000 ) ) 
 REPRESENTATION_ITEM ( '' )  );
#45004 = EDGE_LOOP ( 'NONE', ( #41040, #58688, #52656, #23073 ) ) ;
#45005 = FACE_OUTER_BOUND ( 'NONE', #18832, .T. ) ;
#45006 = CARTESIAN_POINT ( 'NONE',  ( -10.44927233264747102, -11.81971797664088442, -2.077929409079531720 ) ) ;
#45007 =( GEOMETRIC_REPRESENTATION_CONTEXT ( 3 ) GLOBAL_UNCERTAINTY_ASSIGNED_CONTEXT ( ( #6487 ) ) GLOBAL_UNIT_ASSIGNED_CONTEXT ( ( #51686, #3431, #52046 ) ) REPRESENTATION_CONTEXT ( 'NONE', 'WORKASPACE' ) );
#45008 = ADVANCED_FACE ( 'NONE', ( #30303 ), #42761, .F. ) ;
#45009 =( NAMED_UNIT ( * ) PLANE_ANGLE_UNIT ( ) SI_UNIT ( $, .RADIAN. ) );
#45010 = ORIENTED_EDGE ( 'NONE', *, *, #8836, .F. ) ;
#45011 = CARTESIAN_POINT ( 'NONE',  ( -4.716976649647098618, 139.1429263765338078, 6.492361379858953008 ) ) ;
#45012 = CARTESIAN_POINT ( 'NONE',  ( -13.50000000000000533, 30.74999999999999289, 3.750000000000000000 ) ) ;
#45013 = CARTESIAN_POINT ( 'NONE',  ( 68.50000000000000000, 1.797044900979284448E-15, 10.50000000000000000 ) ) ;
#45014 = DIRECTION ( 'NONE',  ( -1.000000000000000000, 0.000000000000000000, 0.000000000000000000 ) ) ;
#45015 = ORIENTED_EDGE ( 'NONE', *, *, #3976, .T. ) ;
#45016 = MECHANICAL_DESIGN_GEOMETRIC_PRESENTATION_REPRESENTATION (  '', ( #46118 ), #10143 ) ;
#45017 = SPHERICAL_SURFACE ( 'NONE', #57641, 0.2500000000000000000 ) ;
#45018 = EDGE_LOOP ( 'NONE', ( #49214, #16686, #38277, #41137 ) ) ;
#45019 = FILL_AREA_STYLE_COLOUR ( '', #4560 ) ;
#45020 = AXIS2_PLACEMENT_3D ( 'NONE', #64021, #47209, #32018 ) ;
#45021 = SURFACE_STYLE_USAGE ( .BOTH. , #39049 ) ;
#45022 = CARTESIAN_POINT ( 'NONE',  ( -83.99999999999997158, 50.00000000000000000, 12.00000000000000000 ) ) ;
#45023 = CARTESIAN_POINT ( 'NONE',  ( -137.6049999999999329, 6.826472737025113702, -4.959722759717902107 ) ) ;
#45024 = CARTESIAN_POINT ( 'NONE',  ( -34.99999999999999289, 99.99999999999998579, 9.500000000000000000 ) ) ;
#45025 = VECTOR ( 'NONE', #27356, 1000.000000000000000 ) ;
#45026 = DIRECTION ( 'NONE',  ( -0.000000000000000000, -0.000000000000000000, 1.000000000000000000 ) ) ;
#45027 = VERTEX_POINT ( 'NONE', #67273 ) ;
#45028 = CARTESIAN_POINT ( 'NONE',  ( 69.99999999999998579, 37.00000000000000000, 4.000000000000000000 ) ) ;
#45029 = AXIS2_PLACEMENT_3D ( 'NONE', #37563, #48445, #64910 ) ;
#45030 = DIRECTION ( 'NONE',  ( -0.000000000000000000, -0.000000000000000000, 1.000000000000000000 ) ) ;
#45031 = VERTEX_POINT ( 'NONE', #50759 ) ;
#45032 = ORIENTED_EDGE ( 'NONE', *, *, #20983, .F. ) ;
#45033 = CARTESIAN_POINT ( 'NONE',  ( -32.39845779402550363, -8.920930673357418073, -1.643626324569322117 ) ) ;
#45034 = CARTESIAN_POINT ( 'NONE',  ( -52.25707362346618368, 5.598654528085800663, -7.705886871421367523 ) ) ;
#45035 = CARTESIAN_POINT ( 'NONE',  ( 1.804495846578303864, 51.08602766979955589, 7.112547338523483198 ) ) ;
#45036 = ORIENTED_EDGE ( 'NONE', *, *, #23912, .T. ) ;
#45037 = CARTESIAN_POINT ( 'NONE',  ( -123.8070736234661666, 10.01517768586948698, -1.839758294383808966E-15 ) ) ;
#45038 = PRESENTATION_STYLE_ASSIGNMENT (( #44359 ) ) ;
#45039 = FACE_OUTER_BOUND ( 'NONE', #32146, .T. ) ;
#45040 =( GEOMETRIC_REPRESENTATION_CONTEXT ( 3 ) GLOBAL_UNCERTAINTY_ASSIGNED_CONTEXT ( ( #47512 ) ) GLOBAL_UNIT_ASSIGNED_CONTEXT ( ( #21397, #32639, #43272 ) ) REPRESENTATION_CONTEXT ( 'NONE', 'WORKASPACE' ) );
#45041 = AXIS2_PLACEMENT_3D ( 'NONE', #17529, #22785, #11872 ) ;
#45042 = CARTESIAN_POINT ( 'NONE',  ( -181.7949999999999875, 2.607480562269069324, -8.024999999999993250 ) ) ;
#45043 = DIRECTION ( 'NONE',  ( 0.000000000000000000, -1.000000000000000000, -0.000000000000000000 ) ) ;
#45044 = STYLED_ITEM ( 'NONE', ( #59037 ), #16578 ) ;
#45045 = ORIENTED_EDGE ( 'NONE', *, *, #38101, .F. ) ;
#45046 = ADVANCED_FACE ( 'NONE', ( #8198 ), #51807, .T. ) ;
#45047 = CARTESIAN_POINT ( 'NONE',  ( -74.88079918414226199, 35.74057955362109595, -9.832742485723521497 ) ) ;
#45048 = DIRECTION ( 'NONE',  ( 0.000000000000000000, -1.000000000000000000, 0.000000000000000000 ) ) ;
#45049 = CARTESIAN_POINT ( 'NONE',  ( -7.000000000000000888, 0.000000000000000000, 0.000000000000000000 ) ) ;
#45050 = CARTESIAN_POINT ( 'NONE',  ( 4.237300235311910690, 154.5000000000000568, -8.541910993906817851 ) ) ;
#45051 = DIRECTION ( 'NONE',  ( 0.000000000000000000, 0.000000000000000000, -1.000000000000000000 ) ) ;
#45052 = CARTESIAN_POINT ( 'NONE',  ( -98.24499999999999034, -4.716976649647093289, -6.492361379858945902 ) ) ;
#45053 = CARTESIAN_POINT ( 'NONE',  ( -9.058813317711338797, 114.4549999999999841, 2.943386871421373563 ) ) ;
#45054 = CARTESIAN_POINT ( 'NONE',  ( -75.89499999999998181, 6.826472737025116366, 4.959722759717898555 ) ) ;
#45055 = DIRECTION ( 'NONE',  ( 0.000000000000000000, 0.000000000000000000, -1.000000000000000000 ) ) ;
#45056 = LINE ( 'NONE', #55208, #6938 ) ;
#45057 = AXIS2_PLACEMENT_3D ( 'NONE', #45670, #29797, #2667 ) ;
#45058 = CARTESIAN_POINT ( 'NONE',  ( 0.000000000000000000, 0.000000000000000000, -12.50000000000000000 ) ) ;
#45059 = DIRECTION ( 'NONE',  ( 1.000000000000000000, -0.000000000000000000, 0.000000000000000000 ) ) ;
#45060 = CARTESIAN_POINT ( 'NONE',  ( 41.61282686761438043, 107.5028968421555930, -3.982829320873341850 ) ) ;
#45062 = EDGE_LOOP ( 'NONE', ( #8888, #46615, #38034, #52569, #29712, #28571, #57273, #37953 ) ) ;
#45061 = VECTOR ( 'NONE', #41797, 999.9999999999998863 ) ;
#45063 = CARTESIAN_POINT ( 'NONE',  ( -114.5929263765337822, -3.094860106618431139, -9.524999999999991473 ) ) ;
#45064 = MECHANICAL_DESIGN_GEOMETRIC_PRESENTATION_REPRESENTATION (  '', ( #36048 ), #57379 ) ;
#45065 =( NAMED_UNIT ( * ) SI_UNIT ( $, .STERADIAN. ) SOLID_ANGLE_UNIT ( ) );
#45066 = CARTESIAN_POINT ( 'NONE',  ( -137.0949999999999989, -2.607480562269071545, -8.024999999999991473 ) ) ;
#45067 = SURFACE_STYLE_FILL_AREA ( #7041 ) ;
#45068 = EDGE_CURVE ( 'NONE', #41524, #50329, #25059, .T. ) ;
#45069 =( LENGTH_UNIT ( ) NAMED_UNIT ( * ) SI_UNIT ( .MILLI., .METRE. ) );
#45070 = CIRCLE ( 'NONE', #57387, 0.2500000000000002220 ) ;
#45071 = DIRECTION ( 'NONE',  ( 0.000000000000000000, -0.000000000000000000, 1.000000000000000000 ) ) ;
#45072 = DIRECTION ( 'NONE',  ( -0.000000000000000000, -1.000000000000000000, -0.000000000000000000 ) ) ;
#45073 = ORIENTED_EDGE ( 'NONE', *, *, #12867, .T. ) ;
#45074 = ORIENTED_EDGE ( 'NONE', *, *, #6854, .T. ) ;
#45075 = STYLED_ITEM ( 'NONE', ( #20559 ), #34621 ) ;
#45076 = DIRECTION ( 'NONE',  ( 0.000000000000000000, 0.000000000000000000, 1.000000000000000000 ) ) ;
#45077 = CARTESIAN_POINT ( 'NONE',  ( -63.44292637653379785, -1.166476076187852838E-15, -9.524999999999991473 ) ) ;
#45078 = EDGE_CURVE ( 'NONE', #9427, #4257, #40926, .T. ) ;
#45079 = AXIS2_PLACEMENT_3D ( 'NONE', #24166, #45673, #7314 ) ;
#45080 = CARTESIAN_POINT ( 'NONE',  ( 0.000000000000000000, 0.000000000000000000, 0.000000000000000000 ) ) ;
#45081 = CARTESIAN_POINT ( 'NONE',  ( -131.3070736234661524, -10.01517768586948698, 6.132527647946031529E-16 ) ) ;
#45082 = COLOUR_RGB ( '', 0.40784314, 0.44705882, 0.49803922) ;
#45083 = CARTESIAN_POINT ( 'NONE',  ( 18.25000000000000711, 33.99999999999999289, -3.750000000000000000 ) ) ;
#45084 = CARTESIAN_POINT ( 'NONE',  ( -9.250000000000003553, 27.99999999999998934, 4.000000000000000000 ) ) ;
#45085 = ORIENTED_EDGE ( 'NONE', *, *, #69104, .F. ) ;
#45086 = CARTESIAN_POINT ( 'NONE',  ( -130.1049999999999898, -6.826472737025113702, 4.959722759717902107 ) ) ;
#45087 = ORIENTED_EDGE ( 'NONE', *, *, #9062, .T. ) ;
#45088 = ORIENTED_EDGE ( 'NONE', *, *, #15131, .F. ) ;
#45089 = DIRECTION ( 'NONE',  ( 0.000000000000000000, -1.000000000000000000, 0.000000000000000000 ) ) ;
#45090 = CYLINDRICAL_SURFACE ( 'NONE', #66922, 0.2500000000000002220 ) ;
#45091 = EDGE_LOOP ( 'NONE', ( #22190, #56385, #16205, #43708 ) ) ;
#45092 = ADVANCED_FACE ( 'NONE', ( #18738 ), #45167, .F. ) ;
#45093 = FILL_AREA_STYLE_COLOUR ( '', #56787 ) ;
#45094 = CARTESIAN_POINT ( 'NONE',  ( 5.598654528085809545, 139.1449999999999818, -7.705886871421373741 ) ) ;
#45095 = CARTESIAN_POINT ( 'NONE',  ( 0.000000000000000000, 154.9999999999999716, 0.000000000000000000 ) ) ;
#45096 = COLOUR_RGB ( '', 0.66274510, 0.83137255, 0.94901961) ;
#45097 = ORIENTED_EDGE ( 'NONE', *, *, #46583, .F. ) ;
#45098 = DIRECTION ( 'NONE',  ( 1.000000000000000000, 3.469446951953611033E-15, 0.000000000000000000 ) ) ;
#45099 = CARTESIAN_POINT ( 'NONE',  ( -9.058813317711337021, 144.1549999999999727, -2.943386871421374895 ) ) ;
#45100 = CARTESIAN_POINT ( 'NONE',  ( -56.60499999999998266, 6.826472737025113702, -4.959722759717902107 ) ) ;
#45101 = EDGE_CURVE ( 'NONE', #42646, #54470, #50647, .T. ) ;
#45102 =( LENGTH_UNIT ( ) NAMED_UNIT ( * ) SI_UNIT ( .MILLI., .METRE. ) );
#45103 = VERTEX_POINT ( 'NONE', #29277 ) ;
#45104 = CARTESIAN_POINT ( 'NONE',  ( 9.058813317711338797, 154.9549999999999841, -2.943386871421372675 ) ) ;
#45105 = LINE ( 'NONE', #59852, #21012 ) ;
#45106 = SURFACE_SIDE_STYLE ('',( #35198 ) ) ;
#45107 = DIRECTION ( 'NONE',  ( 1.000000000000000000, 0.000000000000000000, 0.000000000000000000 ) ) ;
#45108 = EDGE_LOOP ( 'NONE', ( #22054, #68321 ) ) ;
#45109 = ORIENTED_EDGE ( 'NONE', *, *, #48644, .T. ) ;
#45110 = CARTESIAN_POINT ( 'NONE',  ( 20.57648123223228254, 114.4999999999999574, 10.27659574468085069 ) ) ;
#45111 = DIRECTION ( 'NONE',  ( -0.8660254037844385966, 0.000000000000000000, -0.5000000000000003331 ) ) ;
#45113 = CARTESIAN_POINT ( 'NONE',  ( -160.8549999999999898, 4.716976649647094177, 6.492361379858945902 ) ) ;
#45112 = VECTOR ( 'NONE', #27853, 1000.000000000000000 ) ;
#45114 = ORIENTED_EDGE ( 'NONE', *, *, #64178, .T. ) ;
#45115 = MECHANICAL_DESIGN_GEOMETRIC_PRESENTATION_REPRESENTATION (  '', ( #55086 ), #17023 ) ;
#45116 =( GEOMETRIC_REPRESENTATION_CONTEXT ( 3 ) GLOBAL_UNCERTAINTY_ASSIGNED_CONTEXT ( ( #40514 ) ) GLOBAL_UNIT_ASSIGNED_CONTEXT ( ( #54079, #16830, #59703 ) ) REPRESENTATION_CONTEXT ( 'NONE', 'WORKASPACE' ) );
#45117 =( NAMED_UNIT ( * ) SI_UNIT ( $, .STERADIAN. ) SOLID_ANGLE_UNIT ( ) );
#45118 = SURFACE_STYLE_FILL_AREA ( #60892 ) ;
#45119 = ORIENTED_EDGE ( 'NONE', *, *, #27682, .T. ) ;
#45120 = VERTEX_POINT ( 'NONE', #50408 ) ;
#45121 = FACE_OUTER_BOUND ( 'NONE', #47466, .T. ) ;
#45122 =( GEOMETRIC_REPRESENTATION_CONTEXT ( 3 ) GLOBAL_UNCERTAINTY_ASSIGNED_CONTEXT ( ( #27732 ) ) GLOBAL_UNIT_ASSIGNED_CONTEXT ( ( #31237, #47133, #21386 ) ) REPRESENTATION_CONTEXT ( 'NONE', 'WORKASPACE' ) );
#45123 = CARTESIAN_POINT ( 'NONE',  ( -45.89905495956738690, 9.405628579031727554, -3.102072197697239631 ) ) ;
#45124 = CARTESIAN_POINT ( 'NONE',  ( -80.45499999999998408, 7.632228543268599452, -2.479861379858951942 ) ) ;
#45125 = EDGE_LOOP ( 'NONE', ( #25785, #39148, #62424, #25316 ) ) ;
#45126 = CARTESIAN_POINT ( 'NONE',  ( -52.00000000000000000, -1.926070501056209087E-14, -10.49999999999999822 ) ) ;
#45127 = AXIS2_PLACEMENT_3D ( 'NONE', #49285, #44043, #28123 ) ;
#45128 = LINE ( 'NONE', #1422, #2502 ) ;
#45129 = SURFACE_SIDE_STYLE ('',( #13771 ) ) ;
#45130 = EDGE_CURVE ( 'NONE', #50401, #60879, #20302, .T. ) ;
#45131 = CIRCLE ( 'NONE', #66412, 1.000000000000000888 ) ;
#45132 = VERTEX_POINT ( 'NONE', #39890 ) ;
#45133 = FILL_AREA_STYLE_COLOUR ( '', #28113 ) ;
#45134 = PRESENTATION_LAYER_ASSIGNMENT (  '', '', ( #42925 ) ) ;
#45135 = SURFACE_STYLE_FILL_AREA ( #45492 ) ;
#45136 = CARTESIAN_POINT ( 'NONE',  ( 9.058813317711338797, 141.8449999999999989, -2.943386871421372675 ) ) ;
#45137 = CARTESIAN_POINT ( 'NONE',  ( -110.0949999999999704, -2.607480562269071545, -8.024999999999991473 ) ) ;
#45138 = DIRECTION ( 'NONE',  ( -0.000000000000000000, -0.000000000000000000, 1.000000000000000000 ) ) ;
#45139 = PRODUCT_RELATED_PRODUCT_CATEGORY ( 'part', '', ( #37873 ) ) ;
#45141 = CARTESIAN_POINT ( 'NONE',  ( -71.49999999999998579, 64.07124727947029896, 9.500000000000000000 ) ) ;
#45140 = DIRECTION ( 'NONE',  ( 0.000000000000000000, 0.000000000000000000, 1.000000000000000000 ) ) ;
#45142 = ADVANCED_FACE ( 'NONE', ( #24017 ), #61295, .F. ) ;
#45143 = CARTESIAN_POINT ( 'NONE',  ( -149.8429263765337964, 9.058813317711329915, -2.943386871421373119 ) ) ;
#45144 = CARTESIAN_POINT ( 'NONE',  ( -168.4449999999999932, 0.000000000000000000, 8.024999999999991473 ) ) ;
#45145 = EDGE_CURVE ( 'NONE', #29357, #20853, #52171, .T. ) ;
#45146 = EDGE_CURVE ( 'NONE', #36170, #15405, #3, .T. ) ;
#45147 = CARTESIAN_POINT ( 'NONE',  ( 57.24999999999999289, 27.99999999999998934, -3.750000000000000000 ) ) ;
#45148 = SURFACE_STYLE_USAGE ( .BOTH. , #55999 ) ;
#45149 = EDGE_LOOP ( 'NONE', ( #8284, #48354, #21167, #47164, #42702 ) ) ;
#45150 = CARTESIAN_POINT ( 'NONE',  ( -9.827790563157511022E-16, 130.4429263765338192, 8.025000000000000355 ) ) ;
#45151 = ORIENTED_EDGE ( 'NONE', *, *, #36008, .T. ) ;
#45152 = DIRECTION ( 'NONE',  ( -0.7833176619561879050, 0.6216216216216192691, -2.156683240403591475E-15 ) ) ;
#45153 = AXIS2_PLACEMENT_3D ( 'NONE', #67366, #7928, #13194 ) ;
#45154 = EDGE_CURVE ( 'NONE', #60124, #22316, #6792, .T. ) ;
#45155 =( GEOMETRIC_REPRESENTATION_CONTEXT ( 3 ) GLOBAL_UNCERTAINTY_ASSIGNED_CONTEXT ( ( #26377 ) ) GLOBAL_UNIT_ASSIGNED_CONTEXT ( ( #55393, #2916, #12822 ) ) REPRESENTATION_CONTEXT ( 'NONE', 'WORKASPACE' ) );
#45156 = DIRECTION ( 'NONE',  ( 1.000000000000000000, 0.000000000000000000, -0.000000000000000000 ) ) ;
#45157 = CARTESIAN_POINT ( 'NONE',  ( 0.3542424171060606919, 42.77450929379337907, 74.52798306220823576 ) ) ;
#45158 = DIRECTION ( 'NONE',  ( 1.000000000000000000, 0.000000000000000000, -0.000000000000000000 ) ) ;
#45159 = EDGE_CURVE ( 'NONE', #63718, #20985, #10178, .T. ) ;
#45160 = ORIENTED_EDGE ( 'NONE', *, *, #43260, .F. ) ;
#45161 = CARTESIAN_POINT ( 'NONE',  ( -172.5549999999999784, 0.000000000000000000, 8.024999999999991473 ) ) ;
#45162 = ORIENTED_EDGE ( 'NONE', *, *, #60219, .T. ) ;
#45163 = FACE_OUTER_BOUND ( 'NONE', #54482, .T. ) ;
#45164 = AXIS2_PLACEMENT_3D ( 'NONE', #46376, #35081, #56175 ) ;
#45165 = DIRECTION ( 'NONE',  ( -0.000000000000000000, -1.000000000000000000, -0.000000000000000000 ) ) ;
#45166 = EDGE_CURVE ( 'NONE', #26540, #38142, #20106, .T. ) ;
#45167 = CYLINDRICAL_SURFACE ( 'NONE', #10239, 0.5000000000000004441 ) ;
#45168 = VECTOR ( 'NONE', #34566, 1000.000000000000000 ) ;
#45169 = DIRECTION ( 'NONE',  ( 0.000000000000000000, 1.000000000000000000, 0.000000000000000000 ) ) ;
#45170 = CARTESIAN_POINT ( 'NONE',  ( 6.826472737025121695, 153.6070736234661638, -4.959722759717905660 ) ) ;
#45171 = PRESENTATION_LAYER_ASSIGNMENT (  '', '', ( #32787 ) ) ;
#45172 = ORIENTED_EDGE ( 'NONE', *, *, #36989, .T. ) ;
#45173 = CARTESIAN_POINT ( 'NONE',  ( 69.74999999999998579, 37.00000000000000000, 4.000000000000000000 ) ) ;
#45174 = CARTESIAN_POINT ( 'NONE',  ( -88.10499999999998977, -6.826472737025113702, 4.959722759717902107 ) ) ;
#45175 = B_SPLINE_CURVE_WITH_KNOTS ( 'NONE', 3,
 ( #16126, #22404, #48490, #37603, #189, #43568, #53396, #59004, #43230, #44261, #64957, #59319, #21354, #10818, #54060, #38286, #27995, #26621, #59681, #1231, #33316, #11500, #69550, #32596, #32264, #32973, #53712, #5866, #54409, #38634, #27309, #6228, #27655, #16812, #22762, #42881, #60038, #65317, #22067, #11149, #49164, #17507, #6546, #65661 ),
 .UNSPECIFIED., .F., .F.,
 ( 4, 2, 2, 2, 2, 2, 2, 2, 2, 2, 2, 2, 2, 2, 2, 2, 2, 2, 2, 2, 2, 4 ),
 ( 0.008690707667102608169, 0.01030713786529175932, 0.01192356806348091047, 0.01353999826167006162, 0.01515642845985921278, 0.01596464355895379009, 0.01677285865804836393, 0.01838928885623751855, 0.01919750395533209586, 0.02000571905442666970, 0.02162214925261582432, 0.02323857945080497547, 0.02404679454989955278, 0.02485500964899412663, 0.02647143984718328125, 0.02727965494627785509, 0.02808787004537243240, 0.02970430024356158355, 0.03051251534265616433, 0.03132073044175073817, 0.03293716063993989973, 0.03455359083812905435 ),
 .UNSPECIFIED. ) ;
#45176 = CARTESIAN_POINT ( 'NONE',  ( 3.094860106618431583, 133.2049999999999841, 9.525000000000000355 ) ) ;
#45177 =( GEOMETRIC_REPRESENTATION_CONTEXT ( 3 ) GLOBAL_UNCERTAINTY_ASSIGNED_CONTEXT ( ( #63001 ) ) GLOBAL_UNIT_ASSIGNED_CONTEXT ( ( #38503, #54268, #49048 ) ) REPRESENTATION_CONTEXT ( 'NONE', 'WORKASPACE' ) );
#45178 = FACE_OUTER_BOUND ( 'NONE', #30217, .T. ) ;
#45179 = AXIS2_PLACEMENT_3D ( 'NONE', #6828, #68885, #5500 ) ;
#45180 = SURFACE_SIDE_STYLE ('',( #24702 ) ) ;
#45181 = DIRECTION ( 'NONE',  ( 0.000000000000000000, -1.000000000000000000, 0.000000000000000000 ) ) ;
#45182 = EDGE_LOOP ( 'NONE', ( #41457, #2603, #25111, #55946 ) ) ;
#45183 = FILL_AREA_STYLE_COLOUR ( '', #56421 ) ;
#45184 = EDGE_CURVE ( 'NONE', #62964, #10674, #14871, .T. ) ;
#45185 = CARTESIAN_POINT ( 'NONE',  ( -56.99499999999999034, -6.826472737025115478, 4.959722759717900331 ) ) ;
#45186 = ORIENTED_EDGE ( 'NONE', *, *, #59465, .T. ) ;
#45187 = CARTESIAN_POINT ( 'NONE',  ( 6.000000000000020428, 43.00000000000000711, 29.06445261836602256 ) ) ;
#45188 = COLOUR_RGB ( '', 0.66274510, 0.83137255, 0.94901961) ;
#45189 = CARTESIAN_POINT ( 'NONE',  ( -23.71231517720798010, 117.9999999999999716, -7.500000000000000000 ) ) ;
#45190 = CARTESIAN_POINT ( 'NONE',  ( -86.09292637653378222, 3.094860106618433360, 9.524999999999991473 ) ) ;
#45191 = SURFACE_STYLE_FILL_AREA ( #23691 ) ;
#45192 = ORIENTED_EDGE ( 'NONE', *, *, #44298, .T. ) ;
#45193 = CARTESIAN_POINT ( 'NONE',  ( -51.50115812098317036, -11.66198514980602674, 1.604287519264194550 ) ) ;
#45194 = CARTESIAN_POINT ( 'NONE',  ( -51.74499999999998323, 4.716976649647094177, 6.492361379858945902 ) ) ;
#45195 = SURFACE_STYLE_USAGE ( .BOTH. , #39566 ) ;
#45196 = ORIENTED_EDGE ( 'NONE', *, *, #50823, .F. ) ;
#45197 = COLOUR_RGB ( '', 0.08235294, 0.09019608, 0.10196078) ;
#45198 = CARTESIAN_POINT ( 'NONE',  ( -75.00000000000000000, 8.552062714373263930, 6.929199553059595118 ) ) ;
#45199 = CARTESIAN_POINT ( 'NONE',  ( -102.2049999999999983, -2.607480562269071545, -8.024999999999991473 ) ) ;
#45200 = VERTEX_POINT ( 'NONE', #47257 ) ;
#45201 = DIRECTION ( 'NONE',  ( 0.000000000000000000, 1.000000000000000000, 0.000000000000000000 ) ) ;
#45202 = FILL_AREA_STYLE_COLOUR ( '', #41551 ) ;
#45203 = DIRECTION ( 'NONE',  ( -1.000000000000000000, 0.000000000000000000, 0.000000000000000000 ) ) ;
#45204 = CARTESIAN_POINT ( 'NONE',  ( -151.1070736234661638, 8.102448949553171076, -5.886773742842744461 ) ) ;
#45205 = PRESENTATION_LAYER_ASSIGNMENT (  '', '', ( #26019 ) ) ;
#45206 = CARTESIAN_POINT ( 'NONE',  ( 4.750000000000002665, 24.99999999999998579, 4.000000000000000000 ) ) ;
#45207 = CARTESIAN_POINT ( 'NONE',  ( 3.094860106618431583, 147.0949999999999704, 9.525000000000000355 ) ) ;
#45208 = CARTESIAN_POINT ( 'NONE',  ( -82.70707362346617231, -3.094860106618431139, -9.524999999999991473 ) ) ;
#45209 = AXIS2_PLACEMENT_3D ( 'NONE', #54571, #6379, #27809 ) ;
#45210 = EDGE_LOOP ( 'NONE', ( #68142, #8866, #2854, #49062 ) ) ;
#45212 = DIRECTION ( 'NONE',  ( -1.000000000000000000, 0.000000000000000000, 0.000000000000000000 ) ) ;
#45211 = AXIS2_PLACEMENT_3D ( 'NONE', #58635, #21330, #15068 ) ;
#45213 = FILL_AREA_STYLE_COLOUR ( '', #60491 ) ;
#45214 = CARTESIAN_POINT ( 'NONE',  ( -125.1549999999999869, 7.632228543268600340, 2.479861379858949277 ) ) ;
#45215 = CARTESIAN_POINT ( 'NONE',  ( -74.75000000000000000, -4.000000000000000000, 7.000000000000001776 ) ) ;
#45216 = CARTESIAN_POINT ( 'NONE',  ( 8.102448949553181734, 114.3949999999999676, 5.886773742842750679 ) ) ;
#45217 = AXIS2_PLACEMENT_3D ( 'NONE', #38246, #1194, #11811 ) ;
#45218 = CARTESIAN_POINT ( 'NONE',  ( -131.8449999999999989, -7.632228543268599452, 2.479861379858951054 ) ) ;
#45219 = CARTESIAN_POINT ( 'NONE',  ( -131.0949999999999989, -2.607480562269071545, -8.024999999999991473 ) ) ;
#45220 = AXIS2_PLACEMENT_3D ( 'NONE', #8718, #47082, #25237 ) ;
#45221 = CARTESIAN_POINT ( 'NONE',  ( 7.750000000000000000, 33.74999999999998579, 3.750000000000000000 ) ) ;
#45222 = ORIENTED_EDGE ( 'NONE', *, *, #61964, .T. ) ;
#45223 = FACE_OUTER_BOUND ( 'NONE', #8832, .T. ) ;
#45224 = ADVANCED_FACE ( 'NONE', ( #15239 ), #69025, .T. ) ;
#45225 = CARTESIAN_POINT ( 'NONE',  ( 45.50000000000000000, 99.99999999999992895, 10.00000000000000000 ) ) ;
#45226 = CARTESIAN_POINT ( 'NONE',  ( -184.3429263765338249, -9.058813317711329915, 2.943386871421371787 ) ) ;
#45227 = CARTESIAN_POINT ( 'NONE',  ( -48.59499999999997755, 2.607480562269073321, 8.024999999999991473 ) ) ;
#45228 = EDGE_CURVE ( 'NONE', #62431, #23874, #42336, .T. ) ;
#45229 = CARTESIAN_POINT ( 'NONE',  ( 10.00000000000000533, 50.00000000000000000, -60.00000000000000000 ) ) ;
#45230 = DIRECTION ( 'NONE',  ( 0.000000000000000000, 0.000000000000000000, -1.000000000000000000 ) ) ;
#45231 = AXIS2_PLACEMENT_3D ( 'NONE', #37345, #26711, #47205 ) ;
#45232 = CARTESIAN_POINT ( 'NONE',  ( 7.440601873764706831, 1.112499515747338741, 0.4948905776603317874 ) ) ;
#45233 = CARTESIAN_POINT ( 'NONE',  ( -92.24292637653380211, 5.598654528085804216, 7.705886871421366635 ) ) ;
#45234 = APPLICATION_PROTOCOL_DEFINITION ( 'draft international standard', 'automotive_design', 1998, #51410 ) ;
#45235 = CARTESIAN_POINT ( 'NONE',  ( -15.98999599679679839, 117.9999999999999716, -9.500000000000000000 ) ) ;
#45236 = FACE_BOUND ( 'NONE', #22561, .T. ) ;
#45237 = STYLED_ITEM ( 'NONE', ( #28614 ), #25627 ) ;
#45238 = CARTESIAN_POINT ( 'NONE',  ( -9.250000000000003553, 27.99999999999998934, 3.750000000000000000 ) ) ;
#45239 =( NAMED_UNIT ( * ) PLANE_ANGLE_UNIT ( ) SI_UNIT ( $, .RADIAN. ) );
#45240 = VECTOR ( 'NONE', #55350, 1000.000000000000000 ) ;
#45241 = ADVANCED_FACE ( 'NONE', ( #57418 ), #30665, .T. ) ;
#45242 = CARTESIAN_POINT ( 'NONE',  ( 30.75000000000001066, 15.99999999999997691, 4.000000000000000000 ) ) ;
#45243 = ORIENTED_EDGE ( 'NONE', *, *, #17011, .F. ) ;
#45244 = PLANE ( 'NONE',  #64434 ) ;
#45245 = SURFACE_SIDE_STYLE ('',( #18134 ) ) ;
#45246 = CARTESIAN_POINT ( 'NONE',  ( -48.00000000000000000, 99.99999999999992895, 9.500000000000000000 ) ) ;
#45247 = VERTEX_POINT ( 'NONE', #54206 ) ;
#45248 = FILL_AREA_STYLE ('',( #18137 ) ) ;
#45249 = AXIS2_PLACEMENT_3D ( 'NONE', #46867, #20417, #5258 ) ;
#45250 = VECTOR ( 'NONE', #8698, 1000.000000000000000 ) ;
#45251 = CARTESIAN_POINT ( 'NONE',  ( 4.716976649647096842, 119.8570736234661638, 6.492361379858953896 ) ) ;
#45252 = VECTOR ( 'NONE', #26691, 1000.000000000000000 ) ;
#45253 = CARTESIAN_POINT ( 'NONE',  ( 0.000000000000000000, 0.000000000000000000, 0.000000000000000000 ) ) ;
#45254 = CARTESIAN_POINT ( 'NONE',  ( 75.00000000000000000, 19.30628705663858469, -6.500000000000000888 ) ) ;
#45255 = B_SPLINE_CURVE_WITH_KNOTS ( 'NONE', 3,
 ( #40796, #3069, #50289, #55901, #23534, #45047, #51673, #66452, #67491, #13320, #40437, #3424 ),
 .UNSPECIFIED., .F., .F.,
 ( 4, 2, 2, 2, 2, 4 ),
 ( 0.000000000000000000, 0.0001665198070560709623, 0.0003330396141121419245, 0.0006660792282242990279, 0.0009991188423364562397, 0.001332158456448613235 ),
 .UNSPECIFIED. ) ;
#45256 = AXIS2_PLACEMENT_3D ( 'NONE', #57152, #55779, #45944 ) ;
#45257 = DIRECTION ( 'NONE',  ( 5.782411586589351722E-16, -1.000000000000000000, -0.000000000000000000 ) ) ;
#45258 = ORIENTED_EDGE ( 'NONE', *, *, #35571, .T. ) ;
#45259 = FACE_OUTER_BOUND ( 'NONE', #16608, .T. ) ;
#45260 = CLOSED_SHELL ( 'NONE', ( #27916, #59678, #15523, #55549, #22970, #19005, #64881, #46620, #14785, #38719, #11369, #40379, #15173, #68155, #44129, #30884, #17106, #3359, #2318, #55422, #58288, #56958, #35029, #13616, #662, #7231, #30079, #45582, #31183, #56708, #1136, #62317, #29512 ) ) ;
#45261 = CARTESIAN_POINT ( 'NONE',  ( 20.71231517720798010, 115.4999999999999574, 10.00000000000000000 ) ) ;
#45262 = CARTESIAN_POINT ( 'NONE',  ( 2.607480562269030688, 149.7070736234661581, 8.025000000000034106 ) ) ;
#45263 = EDGE_CURVE ( 'NONE', #47020, #59162, #51829, .T. ) ;
#45264 = CARTESIAN_POINT ( 'NONE',  ( 6.330869393641158638, 43.00000000000000000, 28.38386403503541899 ) ) ;
#45265 = VECTOR ( 'NONE', #60208, 1000.000000000000000 ) ;
#45266 =( NAMED_UNIT ( * ) SI_UNIT ( $, .STERADIAN. ) SOLID_ANGLE_UNIT ( ) );
#45267 = ADVANCED_FACE ( 'NONE', ( #33118, #65096 ), #22208, .T. ) ;
#45268 = CARTESIAN_POINT ( 'NONE',  ( -81.59499999999997044, 2.607480562269073321, 8.024999999999991473 ) ) ;
#45269 = ORIENTED_EDGE ( 'NONE', *, *, #17635, .T. ) ;
#45270 =( GEOMETRIC_REPRESENTATION_CONTEXT ( 3 ) GLOBAL_UNCERTAINTY_ASSIGNED_CONTEXT ( ( #17285 ) ) GLOBAL_UNIT_ASSIGNED_CONTEXT ( ( #37060, #32778, #22226 ) ) REPRESENTATION_CONTEXT ( 'NONE', 'WORKASPACE' ) );
#45271 = FILL_AREA_STYLE ('',( #24117 ) ) ;
#45272 = CARTESIAN_POINT ( 'NONE',  ( 12.50000000000000355, 30.74999999999998579, -3.750000000000000000 ) ) ;
#45273 = UNCERTAINTY_MEASURE_WITH_UNIT (LENGTH_MEASURE( 1.000000000000000082E-05 ), #26609, 'distance_accuracy_value', 'NONE');
#45274 = ORIENTED_EDGE ( 'NONE', *, *, #66902, .T. ) ;
#45275 = SURFACE_SIDE_STYLE ('',( #23770 ) ) ;
#45276 = AXIS2_PLACEMENT_3D ( 'NONE', #66691, #29383, #51911 ) ;
#45277 = DIRECTION ( 'NONE',  ( 1.000000000000000000, 2.055968564120660634E-14, 0.000000000000000000 ) ) ;
#45278 = ORIENTED_EDGE ( 'NONE', *, *, #42603, .F. ) ;
#45279 = AXIS2_PLACEMENT_3D ( 'NONE', #33652, #27657, #49166 ) ;
#45280 = CARTESIAN_POINT ( 'NONE',  ( -74.49999999999998579, 119.9999999999997726, -9.500000000000000000 ) ) ;
#45281 = VERTEX_POINT ( 'NONE', #44057 ) ;
#45282 = SURFACE_STYLE_USAGE ( .BOTH. , #30690 ) ;
#45283 = DIRECTION ( 'NONE',  ( 0.000000000000000000, 0.000000000000000000, 1.000000000000000000 ) ) ;
#45284 = PLANE ( 'NONE',  #34190 ) ;
#45285 = DIRECTION ( 'NONE',  ( 0.000000000000000000, 1.000000000000000000, 0.000000000000000000 ) ) ;
#45286 = CARTESIAN_POINT ( 'NONE',  ( -174.9570736234661865, 9.058813317711329915, -2.943386871421373119 ) ) ;
#45287 = CARTESIAN_POINT ( 'NONE',  ( 7.794228634059952476, 4.500000000000003553, 0.000000000000000000 ) ) ;
#45288 = CARTESIAN_POINT ( 'NONE',  ( 9.058813317711338797, 111.8449999999999847, -2.943386871421372675 ) ) ;
#45289 = CARTESIAN_POINT ( 'NONE',  ( -109.5570736234661666, -1.166476076187852838E-15, -9.524999999999991473 ) ) ;
#45290 = CARTESIAN_POINT ( 'NONE',  ( -2.754976799258605169, 2.005084411322475280, 7.000000000000000000 ) ) ;
#45291 = LINE ( 'NONE', #40015, #43717 ) ;
#45292 = EDGE_LOOP ( 'NONE', ( #60762, #54536 ) ) ;
#45293 =( BOUNDED_CURVE ( )  B_SPLINE_CURVE ( 2, ( #66257, #61653, #1841, #46241, #50113, #30014, #66622, #12436, #23352, #39572, #44855 ),
 .UNSPECIFIED., .F., .F. ) 
 B_SPLINE_CURVE_WITH_KNOTS ( ( 3, 2, 2, 2, 2, 3 ),
 ( 0.1764705882352939903, 0.1823529411764704400, 0.1882352941176469174, 0.1941176470588234226, 0.1999999999999999001, 0.2058823529411763498 ),
 .UNSPECIFIED. ) 
 CURVE ( )  GEOMETRIC_REPRESENTATION_ITEM ( )  RATIONAL_B_SPLINE_CURVE ( ( 1.000000000000001110, 0.9510565162951523099, 1.000000000000000000, 0.9510565162951535312, 1.000000000000000000, 0.9510565162951535312, 1.000000000000000000, 0.9510565162951535312, 1.000000000000000000, 0.9510565162951544194, 0.9999999999999991118 ) ) 
 REPRESENTATION_ITEM ( '' )  );
#45294 = MECHANICAL_DESIGN_GEOMETRIC_PRESENTATION_REPRESENTATION (  '', ( #5914 ), #12656 ) ;
#45295 = CARTESIAN_POINT ( 'NONE',  ( 8.000000000000030198, 5.000000000000000000, -32.00402776293825013 ) ) ;
#45296 = DIRECTION ( 'NONE',  ( 0.000000000000000000, 0.000000000000000000, 1.000000000000000000 ) ) ;
#45297 = ORIENTED_EDGE ( 'NONE', *, *, #17603, .F. ) ;
#45298 = CARTESIAN_POINT ( 'NONE',  ( -161.4549999999999841, 7.632228543268599452, -2.479861379858951942 ) ) ;
#45299 = DIRECTION ( 'NONE',  ( -1.982541115402069054E-16, -0.000000000000000000, 1.000000000000000000 ) ) ;
#45300 = ADVANCED_FACE ( 'NONE', ( #11993 ), #16653, .T. ) ;
#45301 = CARTESIAN_POINT ( 'NONE',  ( -165.2949999999999591, -2.607480562269069768, 8.024999999999991473 ) ) ;
#45302 = COLOUR_RGB ( '', 0.09019608, 0.27058824, 0.51372549) ;
#45303 = CARTESIAN_POINT ( 'NONE',  ( -162.1449999999999818, -4.716976649647092401, 6.492361379858946790 ) ) ;
#45304 = ORIENTED_EDGE ( 'NONE', *, *, #28505, .T. ) ;
#45305 = CYLINDRICAL_SURFACE ( 'NONE', #3252, 0.2500000000000002220 ) ;
#45306 = CIRCLE ( 'NONE', #47595, 0.5000000000000004441 ) ;
#45307 = CARTESIAN_POINT ( 'NONE',  ( 72.50000000000000000, 35.92875272052971525, 10.00000000000000000 ) ) ;
#45308 = CARTESIAN_POINT ( 'NONE',  ( -123.2929263765345667, 3.094860106605588967, -9.525000000009322676 ) ) ;
#45309 = CARTESIAN_POINT ( 'NONE',  ( -71.60499999999997556, 6.826472737025113702, -4.959722759717902107 ) ) ;
#45310 = CARTESIAN_POINT ( 'NONE',  ( 31.00000000000000355, 43.00000000000000000, -45.61250543006184444 ) ) ;
#45311 = SURFACE_STYLE_USAGE ( .BOTH. , #29426 ) ;
#45312 = EDGE_CURVE ( 'NONE', #38501, #37491, #64428, .T. ) ;
#45313 = CARTESIAN_POINT ( 'NONE',  ( -70.94499999999997897, -9.827790563157499189E-16, -8.024999999999991473 ) ) ;
#45314 = CARTESIAN_POINT ( 'NONE',  ( 8.102448949553183510, 143.1049999999999329, -5.886773742842746238 ) ) ;
#45315 = COLOUR_RGB ( '', 0.40784314, 0.44705882, 0.49803922) ;
#45316 = SURFACE_STYLE_USAGE ( .BOTH. , #40358 ) ;
#45318 = EDGE_CURVE ( 'NONE', #1680, #29661, #27105, .T. ) ;
#45317 = VECTOR ( 'NONE', #40511, 1000.000000000000000 ) ;
#45319 = UNCERTAINTY_MEASURE_WITH_UNIT (LENGTH_MEASURE( 1.000000000000000082E-05 ), #61008, 'distance_accuracy_value', 'NONE');
#45320 =( BOUNDED_SURFACE ( )  B_SPLINE_SURFACE ( 3, 2, ( 
 ( #2001, #55889, #51311 ),
 ( #50278, #18618, #67137 ),
 ( #29127, #40095, #34766 ),
 ( #66442, #14023, #50965 ),
 ( #7690, #713, #56580 ),
 ( #45033, #8745, #35128 ),
 ( #45384, #62199, #8049 ),
 ( #13308, #18259, #35484 ) ),
 .UNSPECIFIED., .F., .F., .F. ) 
 B_SPLINE_SURFACE_WITH_KNOTS ( ( 4, 2, 2, 4 ),
 ( 3, 3 ),
 ( -1.357421119951851551E-16, 0.001805431820033041824, 0.002708147730049630716, 0.003610863640066219390 ),
 ( 0.000000000000000000, 1.000000000000000000 ),
 .UNSPECIFIED. ) 
 GEOMETRIC_REPRESENTATION_ITEM ( )  RATIONAL_B_SPLINE_SURFACE ( (
 ( 1.000000000000000000, 0.7942671885214119820, 1.000000000000000000),
 ( 1.000000000000000000, 0.8220809233579065012, 1.000000000000000000),
 ( 1.000000000000000000, 0.8510448064981840366, 1.000000000000000000),
 ( 1.000000000000000000, 0.8908666667640210424, 1.000000000000000000),
 ( 1.000000000000000000, 0.9035567410623921436, 1.000000000000000000),
 ( 1.000000000000000000, 0.9270715898449251036, 1.000000000000000000),
 ( 1.000000000000000000, 0.9379207207978137451, 1.000000000000000000),
 ( 1.000000000000000000, 0.9473232638932225225, 1.000000000000000000) ) ) 
 REPRESENTATION_ITEM ( '' )  SURFACE ( )  );
#45321 = AXIS2_PLACEMENT_3D ( 'NONE', #27387, #617, #1665 ) ;
#45322 = CARTESIAN_POINT ( 'NONE',  ( -159.5070736234661979, 8.102448949553176405, 5.886773742842740909 ) ) ;
#45323 = CARTESIAN_POINT ( 'NONE',  ( -19.89974874213239886, 114.9999999999999574, -10.00000000000001421 ) ) ;
#45324 =( GEOMETRIC_REPRESENTATION_CONTEXT ( 3 ) GLOBAL_UNCERTAINTY_ASSIGNED_CONTEXT ( ( #8210 ) ) GLOBAL_UNIT_ASSIGNED_CONTEXT ( ( #25308, #52422, #36252 ) ) REPRESENTATION_CONTEXT ( 'NONE', 'WORKASPACE' ) );
#45325 =( NAMED_UNIT ( * ) SI_UNIT ( $, .STERADIAN. ) SOLID_ANGLE_UNIT ( ) );
#45326 = CARTESIAN_POINT ( 'NONE',  ( 7.899999999999995914, 11.99999999999999289, 3.500000000000004885 ) ) ;
#45327 = AXIS2_PLACEMENT_3D ( 'NONE', #1395, #18336, #40155 ) ;
#45328 = EDGE_CURVE ( 'NONE', #17866, #64410, #36047, .T. ) ;
#45329 = AXIS2_PLACEMENT_3D ( 'NONE', #987, #53512, #28117 ) ;
#45330 = DIRECTION ( 'NONE',  ( 0.000000000000000000, 0.000000000000000000, -1.000000000000000000 ) ) ;
#45331 = LINE ( 'NONE', #1268, #42035 ) ;
#45332 = DIRECTION ( 'NONE',  ( 0.000000000000000000, 0.000000000000000000, -1.000000000000000000 ) ) ;
#45333 = EDGE_LOOP ( 'NONE', ( #11984, #65945, #4161 ) ) ;
#45334 = ORIENTED_EDGE ( 'NONE', *, *, #40538, .F. ) ;
#45335 = CARTESIAN_POINT ( 'NONE',  ( -74.50000000000001421, 1.735173206890468129E-14, -10.00000000000000000 ) ) ;
#45336 = CARTESIAN_POINT ( 'NONE',  ( -155.2429263765338021, 5.598654528085804216, 7.705886871421366635 ) ) ;
#45337 = COLOUR_RGB ( '', 0.09019608, 0.27058824, 0.51372549) ;
#45338 = CARTESIAN_POINT ( 'NONE',  ( -45.00000000000000000, 7.768687147774684831, 6.999999999999999112 ) ) ;
#45339 = CARTESIAN_POINT ( 'NONE',  ( 47.50000000000000000, 13.41640786499872462, -10.00000000000000000 ) ) ;
#45340 = LINE ( 'NONE', #55134, #27330 ) ;
#45341 = CARTESIAN_POINT ( 'NONE',  ( 75.83633811589984930, 14.00000000000000000, -66.72655454856717938 ) ) ;
#45342 = ORIENTED_EDGE ( 'NONE', *, *, #55183, .T. ) ;
#45343 = ORIENTED_EDGE ( 'NONE', *, *, #30020, .F. ) ;
#45344 = ORIENTED_EDGE ( 'NONE', *, *, #3357, .T. ) ;
#45345 = DIRECTION ( 'NONE',  ( -1.000000000000000000, -0.000000000000000000, 1.300977106640434891E-16 ) ) ;
#45346 = ORIENTED_EDGE ( 'NONE', *, *, #22241, .T. ) ;
#45347 = AXIS2_PLACEMENT_3D ( 'NONE', #2407, #29178, #61212 ) ;
#45348 = CARTESIAN_POINT ( 'NONE',  ( -84.05707362346618083, 0.000000000000000000, 9.524999999999991473 ) ) ;
#45349 = DIRECTION ( 'NONE',  ( -1.000000000000000000, -0.000000000000000000, -0.000000000000000000 ) ) ;
#45350 = CARTESIAN_POINT ( 'NONE',  ( -110.0949999999999704, -2.607480562269071545, -8.024999999999991473 ) ) ;
#45351 = ORIENTED_EDGE ( 'NONE', *, *, #40482, .F. ) ;
#45352 = ORIENTED_EDGE ( 'NONE', *, *, #47735, .F. ) ;
#45353 = AXIS2_PLACEMENT_3D ( 'NONE', #7178, #37931, #59306 ) ;
#45354 = DIRECTION ( 'NONE',  ( -1.000000000000000000, 0.000000000000000000, 0.000000000000000000 ) ) ;
#45355 = DIRECTION ( 'NONE',  ( 1.000000000000000000, 0.000000000000000000, 0.000000000000000000 ) ) ;
#45356 = CARTESIAN_POINT ( 'NONE',  ( -10.52052679316176587, -11.79239196812588553, -2.227343248702441159 ) ) ;
#45357 = CARTESIAN_POINT ( 'NONE',  ( -180.8929263765338078, -8.102448949553174629, -5.886773742842741797 ) ) ;
#45358 = ORIENTED_EDGE ( 'NONE', *, *, #6854, .F. ) ;
#45359 = CARTESIAN_POINT ( 'NONE',  ( 4.716976649647099507, 149.6429263765338078, -6.492361379858953008 ) ) ;
#45360 = DIRECTION ( 'NONE',  ( -0.000000000000000000, -0.000000000000000000, 1.000000000000000000 ) ) ;
#45361 = CARTESIAN_POINT ( 'NONE',  ( -195.0000000000000000, 0.000000000000000000, 0.000000000000000000 ) ) ;
#45362 = SURFACE_SIDE_STYLE ('',( #51291 ) ) ;
#45363 = CARTESIAN_POINT ( 'NONE',  ( -4.716976649647098618, 115.1429263765338078, 6.492361379858953008 ) ) ;
#45364 = MECHANICAL_DESIGN_GEOMETRIC_PRESENTATION_REPRESENTATION (  '', ( #18519 ), #42019 ) ;
#45365 = ORIENTED_EDGE ( 'NONE', *, *, #17116, .F. ) ;
#45366 = CARTESIAN_POINT ( 'NONE',  ( -69.99999999999998579, 50.00000000000000000, -6.999999999999988454 ) ) ;
#45367 = ORIENTED_EDGE ( 'NONE', *, *, #58931, .F. ) ;
#45368 = SURFACE_SIDE_STYLE ('',( #18602 ) ) ;
#45369 = CARTESIAN_POINT ( 'NONE',  ( -2.607480562269157254, 139.2070736234662149, -8.024999999999939959 ) ) ;
#45370 = CARTESIAN_POINT ( 'NONE',  ( -20.05205915161432628, 114.9999999999999574, 10.44837816993549318 ) ) ;
#45371 = DIRECTION ( 'NONE',  ( 0.000000000000000000, 0.000000000000000000, 1.000000000000000000 ) ) ;
#45372 = CARTESIAN_POINT ( 'NONE',  ( -129.9549999999999841, -7.632228543268599452, 2.479861379858951054 ) ) ;
#45373 = AXIS2_PLACEMENT_3D ( 'NONE', #31200, #67829, #4829 ) ;
#45374 = ORIENTED_EDGE ( 'NONE', *, *, #26606, .F. ) ;
#45375 = FACE_OUTER_BOUND ( 'NONE', #59478, .T. ) ;
#45376 = STYLED_ITEM ( 'NONE', ( #29755 ), #55842 ) ;
#45377 = FILL_AREA_STYLE ('',( #34081 ) ) ;
#45378 =( NAMED_UNIT ( * ) SI_UNIT ( $, .STERADIAN. ) SOLID_ANGLE_UNIT ( ) );
#45379 = CARTESIAN_POINT ( 'NONE',  ( -0.1770589935948743143, -2.499999999999996891, 7.000000000000002665 ) ) ;
#45380 = ORIENTED_EDGE ( 'NONE', *, *, #55004, .F. ) ;
#45381 = ORIENTED_EDGE ( 'NONE', *, *, #68381, .T. ) ;
#45382 = PRESENTATION_STYLE_ASSIGNMENT (( #12619 ) ) ;
#45383 = AXIS2_PLACEMENT_3D ( 'NONE', #55863, #6613, #44667 ) ;
#45384 = CARTESIAN_POINT ( 'NONE',  ( -32.58435833479455113, -9.007129948131591846, -1.827021129109788644 ) ) ;
#45385 = CARTESIAN_POINT ( 'NONE',  ( 16.75000000000000711, 27.74999999999998224, -3.750000000000000000 ) ) ;
#45386 = AXIS2_PLACEMENT_3D ( 'NONE', #42558, #69264, #10522 ) ;
#45387 = CARTESIAN_POINT ( 'NONE',  ( 44.99999999999998579, 119.9999999999999716, 9.500000000000000000 ) ) ;
#45388 = VERTEX_POINT ( 'NONE', #36161 ) ;
#45389 =( NAMED_UNIT ( * ) SI_UNIT ( $, .STERADIAN. ) SOLID_ANGLE_UNIT ( ) );
#45390 = FACE_OUTER_BOUND ( 'NONE', #4355, .T. ) ;
#45391 = EDGE_CURVE ( 'NONE', #41301, #16804, #1740, .T. ) ;
#45392 = CARTESIAN_POINT ( 'NONE',  ( -59.45707362346616520, -9.058813317711329915, 2.943386871421371787 ) ) ;
#45393 = CIRCLE ( 'NONE', #19522, 7.499999999999984901 ) ;
#45394 = CARTESIAN_POINT ( 'NONE',  ( 36.00000000000002132, 5.000000000000000000, -77.00402776293825013 ) ) ;
#45395 = CARTESIAN_POINT ( 'NONE',  ( 8.046771365092977746, 72.00000000000001421, -6.349999999999997868 ) ) ;
#45397 = EDGE_CURVE ( 'NONE', #52209, #18031, #13368, .T. ) ;
#45396 = ORIENTED_EDGE ( 'NONE', *, *, #66567, .T. ) ;
#45398 = VECTOR ( 'NONE', #1597, 1000.000000000000000 ) ;
#45399 = CARTESIAN_POINT ( 'NONE',  ( -161.7570736234661695, -5.598654528085801552, 7.705886871421367523 ) ) ;
#45400 = AXIS2_PLACEMENT_3D ( 'NONE', #44216, #6507, #27950 ) ;
#45401 = LINE ( 'NONE', #41151, #55132 ) ;
#45402 = CARTESIAN_POINT ( 'NONE',  ( -98.15499999999998693, 7.632228543268600340, 2.479861379858949277 ) ) ;
#45403 = CARTESIAN_POINT ( 'NONE',  ( -60.70461754965443646, -8.499999999999992895, 1.000000000000000000 ) ) ;
#45404 = FACE_OUTER_BOUND ( 'NONE', #26081, .T. ) ;
#45405 = ADVANCED_FACE ( 'NONE', ( #23580 ), #15814, .T. ) ;
#45406 = CIRCLE ( 'NONE', #31884, 3.499999999999999556 ) ;
#45407 = ADVANCED_FACE ( 'NONE', ( #28494 ), #68500, .F. ) ;
#45408 = CARTESIAN_POINT ( 'NONE',  ( -96.29499999999998749, -2.607480562269069768, 8.024999999999991473 ) ) ;
#45409 = CARTESIAN_POINT ( 'NONE',  ( -5.598654528085808657, 120.7549999999999812, 7.705886871421373741 ) ) ;
#45410 = CARTESIAN_POINT ( 'NONE',  ( -74.09499999999998465, -2.607480562269071545, -8.024999999999991473 ) ) ;
#45411 = ADVANCED_FACE ( 'NONE', ( #66865 ), #3436, .T. ) ;
#45412 = CIRCLE ( 'NONE', #21760, 17.00000000000000711 ) ;
#45413 = PRESENTATION_LAYER_ASSIGNMENT (  '', '', ( #19488 ) ) ;
#45414 = PLANE ( 'NONE',  #65193 ) ;
#45415 = EDGE_CURVE ( 'NONE', #67453, #43970, #32706, .T. ) ;
#45416 = UNCERTAINTY_MEASURE_WITH_UNIT (LENGTH_MEASURE( 1.000000000000000082E-05 ), #19173, 'distance_accuracy_value', 'NONE');
#45417 = CIRCLE ( 'NONE', #9429, 9.525000000000000355 ) ;
#45418 = CARTESIAN_POINT ( 'NONE',  ( 66.74999999999998579, 36.75000000000000000, -4.000000000000000000 ) ) ;
#45419 = ORIENTED_EDGE ( 'NONE', *, *, #55417, .T. ) ;
#45420 = ADVANCED_FACE ( 'NONE', ( #56282 ), #34144, .F. ) ;
#45421 = CARTESIAN_POINT ( 'NONE',  ( -111.4429263765338050, -1.166476076187852838E-15, -9.524999999999991473 ) ) ;
#45422 = CARTESIAN_POINT ( 'NONE',  ( -137.2450000000000045, -4.716976649647093289, -6.492361379858945902 ) ) ;
#45423 =( GEOMETRIC_REPRESENTATION_CONTEXT ( 3 ) GLOBAL_UNCERTAINTY_ASSIGNED_CONTEXT ( ( #34158 ) ) GLOBAL_UNIT_ASSIGNED_CONTEXT ( ( #46903, #66931, #34902 ) ) REPRESENTATION_CONTEXT ( 'NONE', 'WORKASPACE' ) );
#45424 =( LENGTH_UNIT ( ) NAMED_UNIT ( * ) SI_UNIT ( .MILLI., .METRE. ) );
#45425 = ORIENTED_EDGE ( 'NONE', *, *, #27221, .T. ) ;
#45426 = ORIENTED_EDGE ( 'NONE', *, *, #50690, .T. ) ;
#45427 = DIRECTION ( 'NONE',  ( 0.000000000000000000, 0.000000000000000000, 1.000000000000000000 ) ) ;
#45428 = DIRECTION ( 'NONE',  ( -0.000000000000000000, -0.000000000000000000, -1.000000000000000000 ) ) ;
#45429 =( GEOMETRIC_REPRESENTATION_CONTEXT ( 3 ) GLOBAL_UNCERTAINTY_ASSIGNED_CONTEXT ( ( #30547 ) ) GLOBAL_UNIT_ASSIGNED_CONTEXT ( ( #20589, #52956, #68432 ) ) REPRESENTATION_CONTEXT ( 'NONE', 'WORKASPACE' ) );
#45430 =( BOUNDED_CURVE ( )  B_SPLINE_CURVE ( 2, ( #41387, #57900, #30425, #30790, #31132, #3682, #41742, #47373, #19889, #25514, #47028 ),
 .UNSPECIFIED., .F., .F. ) 
 B_SPLINE_CURVE_WITH_KNOTS ( ( 3, 2, 2, 2, 2, 3 ),
 ( 0.02941176470588238029, 0.03529411764705885773, 0.04117647058823532824, 0.04705882352941180569, 0.05294117647058828313, 0.05882352941176476058 ),
 .UNSPECIFIED. ) 
 CURVE ( )  GEOMETRIC_REPRESENTATION_ITEM ( )  RATIONAL_B_SPLINE_CURVE ( ( 0.9999999999999997780, 0.9510565162951538642, 1.000000000000000000, 0.9510565162951535312, 1.000000000000000000, 0.9510565162951535312, 1.000000000000000000, 0.9510565162951535312, 1.000000000000000000, 0.9510565162951530871, 1.000000000000000444 ) ) 
 REPRESENTATION_ITEM ( '' )  );
#45431 = AXIS2_PLACEMENT_3D ( 'NONE', #4956, #9213, #47935 ) ;
#45432 = DIRECTION ( 'NONE',  ( 0.000000000000000000, 0.3420201433256694346, -0.9396926207859082059 ) ) ;
#45433 = DIRECTION ( 'NONE',  ( 0.000000000000000000, 0.000000000000000000, 1.000000000000000000 ) ) ;
#45434 = CARTESIAN_POINT ( 'NONE',  ( 4.041451884327379673, -7.000000000000002665, 1.082903768654758903 ) ) ;
#45435 = DIRECTION ( 'NONE',  ( -0.000000000000000000, 1.000000000000000000, -0.000000000000000000 ) ) ;
#45436 = EDGE_LOOP ( 'NONE', ( #26775, #21356, #46190, #2135 ) ) ;
#45437 = CARTESIAN_POINT ( 'NONE',  ( -133.2549999999999955, -4.716976649647092401, 6.492361379858946790 ) ) ;
#45438 = ORIENTED_EDGE ( 'NONE', *, *, #173, .T. ) ;
#45439 = VECTOR ( 'NONE', #32837, 1000.000000000000000 ) ;
#45440 = ORIENTED_EDGE ( 'NONE', *, *, #26904, .T. ) ;
#45441 = DIRECTION ( 'NONE',  ( 0.000000000000000000, 0.000000000000000000, -1.000000000000000000 ) ) ;
#45442 = CARTESIAN_POINT ( 'NONE',  ( -84.29292637653381348, 3.094860106618428031, -9.524999999999993250 ) ) ;
#45443 = EDGE_LOOP ( 'NONE', ( #18876, #50838, #40648, #61911 ) ) ;
#45444 = AXIS2_PLACEMENT_3D ( 'NONE', #51725, #24974, #46484 ) ;
#45445 = SURFACE_STYLE_FILL_AREA ( #38776 ) ;
#45446 = CARTESIAN_POINT ( 'NONE',  ( -9.058813317711338797, 140.3449999999999989, 2.943386871421373563 ) ) ;
#45447 =( LENGTH_UNIT ( ) NAMED_UNIT ( * ) SI_UNIT ( .MILLI., .METRE. ) );
#45448 = PRESENTATION_LAYER_ASSIGNMENT (  '', '', ( #38717 ) ) ;
#45449 = ORIENTED_EDGE ( 'NONE', *, *, #33894, .F. ) ;
#45450 = CARTESIAN_POINT ( 'NONE',  ( -60.49999999999998579, 50.00000000000000000, 6.999999999999999112 ) ) ;
#45451 = CARTESIAN_POINT ( 'NONE',  ( 8.102448949553179958, 142.5049999999999955, 5.886773742842750679 ) ) ;
#45452 = CARTESIAN_POINT ( 'NONE',  ( -49.25499999999999545, -4.716976649647092401, 6.492361379858946790 ) ) ;
#45453 = ORIENTED_EDGE ( 'NONE', *, *, #68284, .T. ) ;
#45454 = CARTESIAN_POINT ( 'NONE',  ( -7.632228543268607446, 117.5429263765338135, -2.479861379858953718 ) ) ;
#45455 = CARTESIAN_POINT ( 'NONE',  ( -25.00000000000000355, 37.00000000000000000, 4.000000000000000000 ) ) ;
#45456 = UNCERTAINTY_MEASURE_WITH_UNIT (LENGTH_MEASURE( 1.000000000000000082E-05 ), #56003, 'distance_accuracy_value', 'NONE');
#45457 = CARTESIAN_POINT ( 'NONE',  ( -88.04292637653379927, -9.058813317711329915, -2.943386871421370898 ) ) ;
#45458 = STYLED_ITEM ( 'NONE', ( #55978 ), #63145 ) ;
#45459 =( NAMED_UNIT ( * ) PLANE_ANGLE_UNIT ( ) SI_UNIT ( $, .RADIAN. ) );
#45460 = DIRECTION ( 'NONE',  ( 0.000000000000000000, 0.000000000000000000, 1.000000000000000000 ) ) ;
#45461 = ORIENTED_EDGE ( 'NONE', *, *, #23830, .T. ) ;
#45462 = CARTESIAN_POINT ( 'NONE',  ( 24.21231517720798010, 99.99999999999998579, 7.500000000000000000 ) ) ;
#45463 = ORIENTED_EDGE ( 'NONE', *, *, #69432, .T. ) ;
#45464 = CARTESIAN_POINT ( 'NONE',  ( -24.00000000000000000, 1.000000000000000000, 3.000000000000000000 ) ) ;
#45465 = CIRCLE ( 'NONE', #34170, 0.2500000000000002220 ) ;
#45466 = CARTESIAN_POINT ( 'NONE',  ( -122.9070736234668999, -3.094860106606060590, 9.525000000008979839 ) ) ;
#45467 = DIRECTION ( 'NONE',  ( -0.5000000000000002220, 0.000000000000000000, 0.8660254037844384856 ) ) ;
#45468 = CARTESIAN_POINT ( 'NONE',  ( -162.5049999999999386, -6.826472737025115478, -4.959722759717899443 ) ) ;
#45469 = ORIENTED_EDGE ( 'NONE', *, *, #69300, .F. ) ;
#45470 = DIRECTION ( 'NONE',  ( -2.478176394252580648E-16, 0.000000000000000000, -1.000000000000000000 ) ) ;
#45471 = UNCERTAINTY_MEASURE_WITH_UNIT (LENGTH_MEASURE( 1.000000000000000082E-05 ), #34102, 'distance_accuracy_value', 'NONE');
#45472 = LINE ( 'NONE', #65843, #22614 ) ;
#45473 = DIRECTION ( 'NONE',  ( -0.000000000000000000, -1.000000000000000000, -0.000000000000000000 ) ) ;
#45474 = EDGE_LOOP ( 'NONE', ( #11458, #59728, #2506, #33386 ) ) ;
#45475 = ORIENTED_EDGE ( 'NONE', *, *, #2394, .F. ) ;
#45476 = FACE_OUTER_BOUND ( 'NONE', #52338, .T. ) ;
#45477 = DIRECTION ( 'NONE',  ( -2.478176394252586564E-16, 0.000000000000000000, -1.000000000000000000 ) ) ;
#45478 = CARTESIAN_POINT ( 'NONE',  ( -76.10500000000000398, -6.826472737025115478, 4.959722759717900331 ) ) ;
#45480 = ORIENTED_EDGE ( 'NONE', *, *, #48504, .T. ) ;
#45479 = VECTOR ( 'NONE', #61889, 1000.000000000000000 ) ;
#45481 = EDGE_CURVE ( 'NONE', #20918, #52016, #66140, .T. ) ;
#45482 = DIRECTION ( 'NONE',  ( 1.000000000000000000, 0.000000000000000000, 0.000000000000000000 ) ) ;
#45483 = EDGE_CURVE ( 'NONE', #52933, #12157, #9130, .T. ) ;
#45484 = MECHANICAL_DESIGN_GEOMETRIC_PRESENTATION_REPRESENTATION (  '', ( #3880 ), #49969 ) ;
#45485 = CARTESIAN_POINT ( 'NONE',  ( 0.000000000000000000, -7.000000000000000888, 0.000000000000000000 ) ) ;
#45486 =( GEOMETRIC_REPRESENTATION_CONTEXT ( 3 ) GLOBAL_UNCERTAINTY_ASSIGNED_CONTEXT ( ( #67164 ) ) GLOBAL_UNIT_ASSIGNED_CONTEXT ( ( #35708, #751, #48038 ) ) REPRESENTATION_CONTEXT ( 'NONE', 'WORKASPACE' ) );
#45487 = EDGE_CURVE ( 'NONE', #32231, #34838, #2053, .T. ) ;
#45488 = CARTESIAN_POINT ( 'NONE',  ( -75.00000000000000000, 8.164117261306888196, -6.987107442241105026 ) ) ;
#45489 = CIRCLE ( 'NONE', #9503, 1.000000000000000888 ) ;
#45490 = ORIENTED_EDGE ( 'NONE', *, *, #48910, .T. ) ;
#45491 = SURFACE_SIDE_STYLE ('',( #29241 ) ) ;
#45493 = DIRECTION ( 'NONE',  ( 2.312964634635740689E-15, -1.000000000000000000, 0.000000000000000000 ) ) ;
#45492 = FILL_AREA_STYLE ('',( #7464 ) ) ;
#45494 = AXIS2_PLACEMENT_3D ( 'NONE', #55931, #23241, #18315 ) ;
#45495 = CARTESIAN_POINT ( 'NONE',  ( -5.598654528085808657, 143.6449999999999818, 7.705886871421373741 ) ) ;
#45496 = CARTESIAN_POINT ( 'NONE',  ( -108.2949999999999733, -2.607480562269069768, 8.024999999999991473 ) ) ;
#45497 = EDGE_CURVE ( 'NONE', #49292, #57697, #23804, .T. ) ;
#45498 = FACE_OUTER_BOUND ( 'NONE', #54705, .T. ) ;
#45499 = SURFACE_STYLE_USAGE ( .BOTH. , #44794 ) ;
#45500 = AXIS2_PLACEMENT_3D ( 'NONE', #12812, #63350, #42303 ) ;
#45502 = CARTESIAN_POINT ( 'NONE',  ( -19.48602968775583832, 11.79452023969822250, -2.232621730279843675 ) ) ;
#45501 = CARTESIAN_POINT ( 'NONE',  ( -96.05707362346618083, 0.000000000000000000, 9.524999999999991473 ) ) ;
#45503 = COLOUR_RGB ( '', 0.31764706, 0.68627451, 0.89019608) ;
#45504 = EDGE_CURVE ( 'NONE', #13063, #53683, #23725, .T. ) ;
#45505 = CARTESIAN_POINT ( 'NONE',  ( -138.7429263765338021, -5.598654528085803328, -7.705886871421366635 ) ) ;
#45506 = CARTESIAN_POINT ( 'NONE',  ( -167.0949999999999704, -2.607480562269071545, -8.024999999999991473 ) ) ;
#45507 = AXIS2_PLACEMENT_3D ( 'NONE', #34779, #45733, #50974 ) ;
#45508 = DIRECTION ( 'NONE',  ( 1.000000000000000000, -0.000000000000000000, -0.000000000000000000 ) ) ;
#45509 = VECTOR ( 'NONE', #64844, 1000.000000000000000 ) ;
#45511 = DIRECTION ( 'NONE',  ( 0.000000000000000000, 0.000000000000000000, 1.000000000000000000 ) ) ;
#45510 = VECTOR ( 'NONE', #25484, 1000.000000000000000 ) ;
#45512 = EDGE_LOOP ( 'NONE', ( #31247, #58362, #35127, #53549 ) ) ;
#45513 = CARTESIAN_POINT ( 'NONE',  ( -22.75000000000000711, 36.75000000000000000, -3.750000000000000000 ) ) ;
#45514 = VERTEX_POINT ( 'NONE', #32567 ) ;
#45515 = PRESENTATION_STYLE_ASSIGNMENT (( #62334 ) ) ;
#45516 = DIRECTION ( 'NONE',  ( 1.000000000000000000, -0.000000000000000000, 0.000000000000000000 ) ) ;
#45517 = CARTESIAN_POINT ( 'NONE',  ( -71.75000000000000000, -0.9999999999999995559, 19.00000000000000000 ) ) ;
#45518 = FACE_OUTER_BOUND ( 'NONE', #7455, .T. ) ;
#45519 = EDGE_LOOP ( 'NONE', ( #27743, #42432, #57971, #67907 ) ) ;
#45520 = CARTESIAN_POINT ( 'NONE',  ( -160.7049999999999841, 2.607480562269072433, 8.024999999999991473 ) ) ;
#45521 =( GEOMETRIC_REPRESENTATION_CONTEXT ( 3 ) GLOBAL_UNCERTAINTY_ASSIGNED_CONTEXT ( ( #61553 ) ) GLOBAL_UNIT_ASSIGNED_CONTEXT ( ( #11541, #16520, #18812 ) ) REPRESENTATION_CONTEXT ( 'NONE', 'WORKASPACE' ) );
#45522 = ORIENTED_EDGE ( 'NONE', *, *, #50131, .F. ) ;
#45523 = SURFACE_STYLE_USAGE ( .BOTH. , #29273 ) ;
#45524 = LINE ( 'NONE', #35270, #45569 ) ;
#45525 = ORIENTED_EDGE ( 'NONE', *, *, #36763, .F. ) ;
#45526 = CARTESIAN_POINT ( 'NONE',  ( 9.058813317711337021, 114.5449999999999733, 2.943386871421375783 ) ) ;
#45527 = CIRCLE ( 'NONE', #5053, 0.2500000000000002220 ) ;
#45528 = EDGE_CURVE ( 'NONE', #57523, #67106, #48117, .T. ) ;
#45529 = ORIENTED_EDGE ( 'NONE', *, *, #53483, .T. ) ;
#45530 = CARTESIAN_POINT ( 'NONE',  ( -9.058813317711338797, 114.4549999999999841, 2.943386871421373563 ) ) ;
#45531 = CARTESIAN_POINT ( 'NONE',  ( -73.10499999999997556, -6.826472737025113702, 4.959722759717902107 ) ) ;
#45532 = AXIS2_PLACEMENT_3D ( 'NONE', #57563, #20264, #41769 ) ;
#45533 = DIRECTION ( 'NONE',  ( -0.000000000000000000, -0.000000000000000000, 1.000000000000000000 ) ) ;
#45534 = CARTESIAN_POINT ( 'NONE',  ( 0.000000000000000000, 128.5549999999999784, -9.525000000000000355 ) ) ;
#45535 = UNCERTAINTY_MEASURE_WITH_UNIT (LENGTH_MEASURE( 1.000000000000000082E-05 ), #64110, 'distance_accuracy_value', 'NONE');
#45536 = CARTESIAN_POINT ( 'NONE',  ( 20.48276553341834827, 114.7646630323463057, 10.30680354032555712 ) ) ;
#45537 = DIRECTION ( 'NONE',  ( -1.000000000000000000, 0.000000000000000000, 0.000000000000000000 ) ) ;
#45538 = SURFACE_STYLE_USAGE ( .BOTH. , #44835 ) ;
#45539 = ORIENTED_EDGE ( 'NONE', *, *, #57344, .T. ) ;
#45540 = SURFACE_STYLE_USAGE ( .BOTH. , #55703 ) ;
#45541 = CARTESIAN_POINT ( 'NONE',  ( -52.94499999999999318, -9.827790563157499189E-16, -8.024999999999991473 ) ) ;
#45542 = ORIENTED_EDGE ( 'NONE', *, *, #46868, .F. ) ;
#45543 = DIRECTION ( 'NONE',  ( -0.000000000000000000, 0.000000000000000000, -1.000000000000000000 ) ) ;
#45544 =( GEOMETRIC_REPRESENTATION_CONTEXT ( 3 ) GLOBAL_UNCERTAINTY_ASSIGNED_CONTEXT ( ( #24997 ) ) GLOBAL_UNIT_ASSIGNED_CONTEXT ( ( #64629, #37599, #4833 ) ) REPRESENTATION_CONTEXT ( 'NONE', 'WORKASPACE' ) );
#45545 = FACE_OUTER_BOUND ( 'NONE', #43274, .T. ) ;
#45546 = DIRECTION ( 'NONE',  ( 1.224646799147353207E-16, 1.000000000000000000, -0.000000000000000000 ) ) ;
#45547 = ORIENTED_EDGE ( 'NONE', *, *, #10415, .F. ) ;
#45548 = CARTESIAN_POINT ( 'NONE',  ( -51.72259415970177798, -11.52611143915721037, 3.270167026231387997 ) ) ;
#45549 = CARTESIAN_POINT ( 'NONE',  ( -50.39499999999999602, -6.826472737025113702, -4.959722759717900331 ) ) ;
#45550 =( LENGTH_UNIT ( ) NAMED_UNIT ( * ) SI_UNIT ( .MILLI., .METRE. ) );
#45551 = ORIENTED_EDGE ( 'NONE', *, *, #32247, .T. ) ;
#45552 = EDGE_CURVE ( 'NONE', #34838, #26540, #38254, .T. ) ;
#45553 = MECHANICAL_DESIGN_GEOMETRIC_PRESENTATION_REPRESENTATION (  '', ( #17416 ), #69075 ) ;
#45554 = CARTESIAN_POINT ( 'NONE',  ( -75.00000000000000000, 8.443649368548715728, 5.542175914092815958 ) ) ;
#45555 = CARTESIAN_POINT ( 'NONE',  ( -107.0049999999999955, 6.826472737025116366, 4.959722759717898555 ) ) ;
#45556 = VERTEX_POINT ( 'NONE', #4437 ) ;
#45557 = EDGE_CURVE ( 'NONE', #10312, #56046, #50080, .T. ) ;
#45558 = CARTESIAN_POINT ( 'NONE',  ( -13.75000000000000533, 30.74999999999999289, 3.750000000000000000 ) ) ;
#45559 = FACE_OUTER_BOUND ( 'NONE', #53515, .T. ) ;
#45560 = AXIS2_PLACEMENT_3D ( 'NONE', #69604, #47522, #42255 ) ;
#45561 = CARTESIAN_POINT ( 'NONE',  ( -143.1570736234662036, -9.058813317711329915, -2.943386871421370898 ) ) ;
#45562 = CARTESIAN_POINT ( 'NONE',  ( 12.72792206135785698, 115.4999999999999574, -10.50000000000000000 ) ) ;
#45563 = CARTESIAN_POINT ( 'NONE',  ( -5.598654528085808657, 137.6449999999999818, 7.705886871421373741 ) ) ;
#45564 = CARTESIAN_POINT ( 'NONE',  ( -80.00707362346618368, -8.102448949553172852, -5.886773742842741797 ) ) ;
#45565 = ADVANCED_FACE ( 'NONE', ( #48813 ), #48460, .T. ) ;
#45566 =( LENGTH_UNIT ( ) NAMED_UNIT ( * ) SI_UNIT ( .MILLI., .METRE. ) );
#45567 = SURFACE_SIDE_STYLE ('',( #24062 ) ) ;
#45568 = ADVANCED_FACE ( 'NONE', ( #20996, #31535, #10105 ), #153, .F. ) ;
#45569 = VECTOR ( 'NONE', #19776, 1000.000000000000000 ) ;
#45570 = CARTESIAN_POINT ( 'NONE',  ( -120.8049999999999784, -8.437984349512085203, 5.166775262442717831E-16 ) ) ;
#45571 = CARTESIAN_POINT ( 'NONE',  ( 22.00000000000000711, 43.00000000000000000, -45.61250543006183733 ) ) ;
#45572 = CARTESIAN_POINT ( 'NONE',  ( 0.000000000000000000, 109.4449999999999932, -9.525000000000000355 ) ) ;
#45573 = CARTESIAN_POINT ( 'NONE',  ( -135.8949999999999818, 6.826472737025116366, 4.959722759717898555 ) ) ;
#45574 = TOROIDAL_SURFACE ( 'NONE', #10733, 1.000000000000000000, 0.5000000000000000000 ) ;
#45575 = EDGE_CURVE ( 'NONE', #39293, #36711, #16098, .T. ) ;
#45576 = CARTESIAN_POINT ( 'NONE',  ( -116.6949999999999790, -8.437984349512086979, 5.166775262442717831E-16 ) ) ;
#45577 = CARTESIAN_POINT ( 'NONE',  ( -36.00278222459130006, -10.17514555344026306, 4.251650545525158975 ) ) ;
#45578 = VERTEX_POINT ( 'NONE', #32237 ) ;
#45579 = DIRECTION ( 'NONE',  ( 0.000000000000000000, -0.000000000000000000, -1.000000000000000000 ) ) ;
#45580 = LINE ( 'NONE', #23377, #30532 ) ;
#45581 = VECTOR ( 'NONE', #34295, 1000.000000000000000 ) ;
#45582 = ADVANCED_FACE ( 'NONE', ( #5834 ), #27273, .T. ) ;
#45583 = CARTESIAN_POINT ( 'NONE',  ( -171.1429263765338078, 5.598654528085800663, -7.705886871421367523 ) ) ;
#45584 =( NAMED_UNIT ( * ) PLANE_ANGLE_UNIT ( ) SI_UNIT ( $, .RADIAN. ) );
#45585 = CARTESIAN_POINT ( 'NONE',  ( -50.39499999999999602, -6.826472737025115478, -4.959722759717899443 ) ) ;
#45586 = FILL_AREA_STYLE_COLOUR ( '', #30152 ) ;
#45587 = CARTESIAN_POINT ( 'NONE',  ( -195.0000000000000000, 1.166476076187852838E-15, -9.524999999999991473 ) ) ;
#45588 = SURFACE_SIDE_STYLE ('',( #61688 ) ) ;
#45589 = LINE ( 'NONE', #9309, #54062 ) ;
#45590 = ORIENTED_EDGE ( 'NONE', *, *, #20850, .T. ) ;
#45591 = CARTESIAN_POINT ( 'NONE',  ( -97.04292637653379927, -9.058813317711329915, -2.943386871421370898 ) ) ;
#45592 = SHAPE_DEFINITION_REPRESENTATION ( #58577, #15001 ) ;
#45593 = PLANE ( 'NONE',  #57683 ) ;
#45594 = COLOUR_RGB ( '', 0.40784314, 0.44705882, 0.49803922) ;
#45595 = CARTESIAN_POINT ( 'NONE',  ( 39.49999999999999289, 18.99999999999997868, 3.750000000000000000 ) ) ;
#45596 = APPLICATION_CONTEXT ( 'automotive_design' ) ;
#45597 = VECTOR ( 'NONE', #55096, 1000.000000000000000 ) ;
#45598 = PRESENTATION_STYLE_ASSIGNMENT (( #61695 ) ) ;
#45599 = LINE ( 'NONE', #51183, #51719 ) ;
#45600 = CARTESIAN_POINT ( 'NONE',  ( -78.80707362346618083, 10.01517768586948698, -1.839758294383808966E-15 ) ) ;
#45601 =( NAMED_UNIT ( * ) PLANE_ANGLE_UNIT ( ) SI_UNIT ( $, .RADIAN. ) );
#45602 = ORIENTED_EDGE ( 'NONE', *, *, #21374, .T. ) ;
#45603 = DIRECTION ( 'NONE',  ( 1.000000000000000000, 0.000000000000000000, -0.000000000000000000 ) ) ;
#45604 = CARTESIAN_POINT ( 'NONE',  ( 3.851859888774471706E-31, -8.500000000000000000, 1.000000000000000888 ) ) ;
#45606 = ORIENTED_EDGE ( 'NONE', *, *, #16849, .T. ) ;
#45605 = CIRCLE ( 'NONE', #61269, 4.999999999999997335 ) ;
#45607 = CARTESIAN_POINT ( 'NONE',  ( -64.49292637653380211, -8.102448949553174629, 5.886773742842742685 ) ) ;
#45608 = CARTESIAN_POINT ( 'NONE',  ( -4.716976649647098618, 137.2570736234661695, 6.492361379858953008 ) ) ;
#45609 = EDGE_CURVE ( 'NONE', #36166, #45027, #39280, .T. ) ;
#45610 = CARTESIAN_POINT ( 'NONE',  ( 75.00000000000000000, 19.30628705663858469, -7.000000000000000000 ) ) ;
#45611 = DIRECTION ( 'NONE',  ( 0.000000000000000000, 1.000000000000000000, 0.000000000000000000 ) ) ;
#45612 = ORIENTED_EDGE ( 'NONE', *, *, #60049, .F. ) ;
#45613 = CARTESIAN_POINT ( 'NONE',  ( -16.75000000000000000, -3.000000000000000000, 19.00000000000000000 ) ) ;
#45614 = VECTOR ( 'NONE', #20472, 1000.000000000000000 ) ;
#45615 = CARTESIAN_POINT ( 'NONE',  ( 6.826472737025121695, 150.6070736234661069, -4.959722759717905660 ) ) ;
#45616 = VECTOR ( 'NONE', #27724, 1000.000000000000000 ) ;
#45617 = CIRCLE ( 'NONE', #56831, 110.0000000000000142 ) ;
#45618 = CARTESIAN_POINT ( 'NONE',  ( -48.50000000000000000, 14.49137674618942562, -10.00000000000000000 ) ) ;
#45619 = CARTESIAN_POINT ( 'NONE',  ( -80.84499999999998465, -7.632228543268599452, 2.479861379858951054 ) ) ;
#45620 = ORIENTED_EDGE ( 'NONE', *, *, #3337, .T. ) ;
#45621 = VECTOR ( 'NONE', #53111, 1000.000000000000000 ) ;
#45622 =( BOUNDED_SURFACE ( )  B_SPLINE_SURFACE ( 3, 2, ( 
 ( #41575, #25698, #12546 ),
 ( #16827, #6934, #22780 ),
 ( #29055, #55815, #12192 ),
 ( #33665, #1605, #17181 ),
 ( #49521, #49179, #11518 ),
 ( #43582, #1249, #33331 ),
 ( #17846, #28359, #54752 ),
 ( #44277, #22421, #32987 ),
 ( #65678, #39669, #34011 ),
 ( #49867, #17524, #60727 ) ),
 .UNSPECIFIED., .F., .F., .F. ) 
 B_SPLINE_SURFACE_WITH_KNOTS ( ( 4, 2, 2, 2, 4 ),
 ( 3, 3 ),
 ( 3.141592653589793116, 3.666904475503235616, 4.192216297416678117, 4.717528119330120617, 5.242839941243563118 ),
 ( 0.000000000000000000, 1.000000000000000000 ),
 .UNSPECIFIED. ) 
 GEOMETRIC_REPRESENTATION_ITEM ( )  RATIONAL_B_SPLINE_SURFACE ( (
 ( 1.000000000000000000, 0.5847102846637711737, 1.000000000000000000),
 ( 1.000000000000000000, 0.5846320934540470970, 1.000000000000000000),
 ( 1.000000000000000000, 0.5911458751171370096, 1.000000000000000000),
 ( 1.000000000000000000, 0.6141839381259066588, 1.000000000000000000),
 ( 1.000000000000000000, 0.6306589281296752780, 1.000000000000000000),
 ( 1.000000000000000000, 0.6676671612970677128, 1.000000000000000000),
 ( 1.000000000000000000, 0.6881200523218607978, 1.000000000000000000),
 ( 1.000000000000000000, 0.7272421848983147141, 1.000000000000000000),
 ( 1.000000000000000000, 0.7459210345857979485, 1.000000000000000000),
 ( 1.000000000000000000, 0.7615729461579521242, 1.000000000000000000) ) ) 
 REPRESENTATION_ITEM ( '' )  SURFACE ( )  );
#45623 = DIRECTION ( 'NONE',  ( 0.9396926207859093161, 0.3420201433256664370, 0.000000000000000000 ) ) ;
#45624 = EDGE_CURVE ( 'NONE', #35471, #55787, #54374, .T. ) ;
#45625 = CARTESIAN_POINT ( 'NONE',  ( -32.38286428517920257, -8.500000000000000000, 6.664929171799900409 ) ) ;
#45626 =( GEOMETRIC_REPRESENTATION_CONTEXT ( 3 ) GLOBAL_UNCERTAINTY_ASSIGNED_CONTEXT ( ( #26447 ) ) GLOBAL_UNIT_ASSIGNED_CONTEXT ( ( #59536, #11356, #21213 ) ) REPRESENTATION_CONTEXT ( 'NONE', 'WORKASPACE' ) );
#45627 = ORIENTED_EDGE ( 'NONE', *, *, #18872, .T. ) ;
#45628 = CARTESIAN_POINT ( 'NONE',  ( -74.99999999999998579, 50.00000000000000000, 9.500000000000000000 ) ) ;
#45629 = EDGE_CURVE ( 'NONE', #56046, #4654, #12498, .T. ) ;
#45630 = DIRECTION ( 'NONE',  ( 0.000000000000000000, -0.000000000000000000, 1.000000000000000000 ) ) ;
#45631 = EDGE_LOOP ( 'NONE', ( #19588, #59669, #57451, #25566, #62092, #43963, #30529, #29124 ) ) ;
#45632 = EDGE_CURVE ( 'NONE', #47340, #34416, #6196, .T. ) ;
#45633 = FACE_OUTER_BOUND ( 'NONE', #22035, .T. ) ;
#45634 = ORIENTED_EDGE ( 'NONE', *, *, #2647, .F. ) ;
#45635 = FILL_AREA_STYLE_COLOUR ( '', #65608 ) ;
#45636 = SURFACE_SIDE_STYLE ('',( #40326 ) ) ;
#45637 = CARTESIAN_POINT ( 'NONE',  ( -166.5570736234661808, -1.166476076187852838E-15, -9.524999999999991473 ) ) ;
#45638 = SPHERICAL_SURFACE ( 'NONE', #43267, 0.2500000000000000000 ) ;
#45639 = CARTESIAN_POINT ( 'NONE',  ( 9.058813317711337021, 117.5449999999999875, 2.943386871421375783 ) ) ;
#45640 = CARTESIAN_POINT ( 'NONE',  ( -115.5570736234661808, -1.166476076187852838E-15, -9.524999999999991473 ) ) ;
#45641 = PRESENTATION_LAYER_ASSIGNMENT (  '', '', ( #19738 ) ) ;
#45642 = LINE ( 'NONE', #40692, #7108 ) ;
#45643 = ADVANCED_FACE ( 'NONE', ( #55424 ), #12152, .F. ) ;
#45644 = CARTESIAN_POINT ( 'NONE',  ( -84.65707362346616094, 9.058813317711329915, 2.943386871421369566 ) ) ;
#45645 = EDGE_LOOP ( 'NONE', ( #700, #23828, #60501, #45707, #24606, #54027, #63414, #38624 ) ) ;
#45646 = DIRECTION ( 'NONE',  ( 0.000000000000000000, 0.000000000000000000, -1.000000000000000000 ) ) ;
#45647 = EDGE_CURVE ( 'NONE', #57711, #24348, #19185, .T. ) ;
#45648 = DIRECTION ( 'NONE',  ( -0.000000000000000000, -0.000000000000000000, -1.000000000000000000 ) ) ;
#45649 = CARTESIAN_POINT ( 'NONE',  ( -150.8050000000000068, -8.437984349512085203, 5.166775262442717831E-16 ) ) ;
#45650 = CARTESIAN_POINT ( 'NONE',  ( -75.00000000000000000, 9.117000356772813063, 6.738247770644825607 ) ) ;
#45651 = CARTESIAN_POINT ( 'NONE',  ( -8.208819650266621082, 111.3781065788698896, -2.747382571411663754 ) ) ;
#45652 = CARTESIAN_POINT ( 'NONE',  ( -161.5449999999999875, -7.632228543268600340, -2.479861379858950166 ) ) ;
#45653 =( GEOMETRIC_REPRESENTATION_CONTEXT ( 3 ) GLOBAL_UNCERTAINTY_ASSIGNED_CONTEXT ( ( #33299 ) ) GLOBAL_UNIT_ASSIGNED_CONTEXT ( ( #65731, #18238, #11570 ) ) REPRESENTATION_CONTEXT ( 'NONE', 'WORKASPACE' ) );
#45654 = CARTESIAN_POINT ( 'NONE',  ( -151.9449999999999932, -9.827790563157499189E-16, -8.024999999999991473 ) ) ;
#45655 = VERTEX_POINT ( 'NONE', #27630 ) ;
#45656 = CARTESIAN_POINT ( 'NONE',  ( -66.74292637653380211, -5.598654528085803328, -7.705886871421366635 ) ) ;
#45657 = CARTESIAN_POINT ( 'NONE',  ( 96.10348817448824832, 0.000000000000000000, -27.38099488609876531 ) ) ;
#45658 = CARTESIAN_POINT ( 'NONE',  ( -65.60499999999997556, 6.826472737025113702, -4.959722759717902107 ) ) ;
#45659 = CARTESIAN_POINT ( 'NONE',  ( -37.68484432981706789, -12.63346336609729370, 1.177413386875751256 ) ) ;
#45660 = CARTESIAN_POINT ( 'NONE',  ( -154.4070736234665162, 3.094860106612512762, -9.525000000004292033 ) ) ;
#45661 = CARTESIAN_POINT ( 'NONE',  ( -67.34499999999998465, 7.632228543268599452, -2.479861379858951942 ) ) ;
#45662 = CARTESIAN_POINT ( 'NONE',  ( 3.094860106618435136, 149.4049999999999443, -9.525000000000000355 ) ) ;
#45663 = ADVANCED_FACE ( 'NONE', ( #49139 ), #18144, .T. ) ;
#45664 = DIRECTION ( 'NONE',  ( 0.000000000000000000, 0.000000000000000000, -1.000000000000000000 ) ) ;
#45665 = COLOUR_RGB ( '', 0.66274510, 0.83137255, 0.94901961) ;
#45666 = DIRECTION ( 'NONE',  ( 1.000000000000000000, 0.000000000000000000, 0.000000000000000000 ) ) ;
#45667 = ADVANCED_FACE ( 'NONE', ( #46665 ), #35374, .F. ) ;
#45668 = CIRCLE ( 'NONE', #17444, 0.2500000000000002220 ) ;
#45669 = DIRECTION ( 'NONE',  ( -1.000000000000000000, 0.000000000000000000, 0.000000000000000000 ) ) ;
#45670 = CARTESIAN_POINT ( 'NONE',  ( 92.41620014002536720, 0.000000000000000000, 24.00402776293825369 ) ) ;
#45671 = CARTESIAN_POINT ( 'NONE',  ( 33.00000000000000711, 14.00000000000000000, -35.50000000000000000 ) ) ;
#45672 = DIRECTION ( 'NONE',  ( -1.000000000000000000, 0.000000000000000000, 0.000000000000000000 ) ) ;
#45673 = DIRECTION ( 'NONE',  ( 0.000000000000000000, 0.000000000000000000, 1.000000000000000000 ) ) ;
#45674 = CARTESIAN_POINT ( 'NONE',  ( -118.9429263765338050, 0.000000000000000000, 9.524999999999991473 ) ) ;
#45675 = FILL_AREA_STYLE ('',( #28743 ) ) ;
#45676 = ORIENTED_EDGE ( 'NONE', *, *, #28891, .F. ) ;
#45677 = ORIENTED_EDGE ( 'NONE', *, *, #60357, .F. ) ;
#45678 = CARTESIAN_POINT ( 'NONE',  ( -156.4429263765338192, -1.166476076187852838E-15, -9.524999999999991473 ) ) ;
#45679 = CARTESIAN_POINT ( 'NONE',  ( 45.50000000000000000, 9.639620389971918613, -6.500000000000000000 ) ) ;
#45680 = SURFACE_SIDE_STYLE ('',( #23158 ) ) ;
#45681 = ORIENTED_EDGE ( 'NONE', *, *, #7630, .T. ) ;
#45682 = ORIENTED_EDGE ( 'NONE', *, *, #17123, .T. ) ;
#45683 = COLOUR_RGB ( '', 0.08235294, 0.09019608, 0.10196078) ;
#45684 = VERTEX_POINT ( 'NONE', #56827 ) ;
#45685 = CARTESIAN_POINT ( 'NONE',  ( -65.69292637653380496, 10.01517768586948698, -1.839758294383808966E-15 ) ) ;
#45686 = DIRECTION ( 'NONE',  ( 0.000000000000000000, 1.000000000000000000, 0.000000000000000000 ) ) ;
#45687 = VECTOR ( 'NONE', #3744, 1000.000000000000000 ) ;
#45688 = EDGE_LOOP ( 'NONE', ( #45627, #62038, #4061, #48084 ) ) ;
#45689 = EDGE_CURVE ( 'NONE', #1660, #37997, #8638, .T. ) ;
#45690 = CIRCLE ( 'NONE', #9739, 0.5000000000000004441 ) ;
#45691 = CARTESIAN_POINT ( 'NONE',  ( -83.30707362346619504, -10.01517768586948698, 6.132527647946031529E-16 ) ) ;
#45692 = SURFACE_STYLE_USAGE ( .BOTH. , #8714 ) ;
#45693 = CARTESIAN_POINT ( 'NONE',  ( -114.7449999999999903, 4.716976649647094177, 6.492361379858945902 ) ) ;
#45694 = ORIENTED_EDGE ( 'NONE', *, *, #19604, .F. ) ;
#45695 = CARTESIAN_POINT ( 'NONE',  ( -0.8808868071890268991, 110.4999999999999574, -9.494348005351133324 ) ) ;
#45696 = CARTESIAN_POINT ( 'NONE',  ( -183.2510368117331154, 0.000000000000000000, 8.774999999999991473 ) ) ;
#45697 = CARTESIAN_POINT ( 'NONE',  ( -13.68947831298332218, -10.98244867573161443, -4.836413723188878855 ) ) ;
#45698 = ADVANCED_FACE ( 'NONE', ( #24436 ), #2607, .T. ) ;
#45699 = CARTESIAN_POINT ( 'NONE',  ( -179.7570736234661979, -5.598654528085801552, 7.705886871421367523 ) ) ;
#45700 = EDGE_LOOP ( 'NONE', ( #13004, #50335, #10285, #10605 ) ) ;
#45701 = CARTESIAN_POINT ( 'NONE',  ( 0.000000000000000000, 146.9429263765338192, -8.025000000000000355 ) ) ;
#45702 = DIRECTION ( 'NONE',  ( -1.000000000000000000, 0.000000000000000000, 0.000000000000000000 ) ) ;
#45703 = CYLINDRICAL_SURFACE ( 'NONE', #34010, 13.00000000000000533 ) ;
#45704 = COLOUR_RGB ( '', 0.09019608, 0.27058824, 0.51372549) ;
#45705 = EDGE_CURVE ( 'NONE', #3488, #67189, #22678, .T. ) ;
#45706 =( NAMED_UNIT ( * ) SI_UNIT ( $, .STERADIAN. ) SOLID_ANGLE_UNIT ( ) );
#45707 = ORIENTED_EDGE ( 'NONE', *, *, #1626, .T. ) ;
#45708 = SURFACE_STYLE_FILL_AREA ( #41119 ) ;
#45709 = ORIENTED_EDGE ( 'NONE', *, *, #52669, .T. ) ;
#45710 = DIRECTION ( 'NONE',  ( -0.000000000000000000, -0.000000000000000000, -1.000000000000000000 ) ) ;
#45711 =( NAMED_UNIT ( * ) SI_UNIT ( $, .STERADIAN. ) SOLID_ANGLE_UNIT ( ) );
#45712 = LINE ( 'NONE', #7675, #55466 ) ;
#45713 = CARTESIAN_POINT ( 'NONE',  ( -9.985360875542992787, -0.7048476316490953630, 0.9853608755428877597 ) ) ;
#45714 = CARTESIAN_POINT ( 'NONE',  ( -134.0049999999999955, 6.826472737025116366, 4.959722759717898555 ) ) ;
#45715 = DIRECTION ( 'NONE',  ( -0.000000000000000000, 1.000000000000000000, 0.000000000000000000 ) ) ;
#45716 = ORIENTED_EDGE ( 'NONE', *, *, #52683, .T. ) ;
#45717 = CYLINDRICAL_SURFACE ( 'NONE', #59872, 0.2500000000000002220 ) ;
#45718 = DIRECTION ( 'NONE',  ( -1.000000000000000000, 0.000000000000000000, 0.000000000000000000 ) ) ;
#45719 = DIRECTION ( 'NONE',  ( 0.000000000000000000, 0.000000000000000000, -1.000000000000000000 ) ) ;
#45720 = ORIENTED_EDGE ( 'NONE', *, *, #35673, .F. ) ;
#45721 = VERTEX_POINT ( 'NONE', #51535 ) ;
#45722 = CYLINDRICAL_SURFACE ( 'NONE', #9262, 0.5000000000000004441 ) ;
#45723 = CARTESIAN_POINT ( 'NONE',  ( 0.000000000000000000, 0.000000000000000000, 0.000000000000000000 ) ) ;
#45724 = ADVANCED_FACE ( 'NONE', ( #51203 ), #14601, .T. ) ;
#45725 = CARTESIAN_POINT ( 'NONE',  ( 4.000000000000029310, 43.00000000000000000, 90.00000000000000000 ) ) ;
#45726 = CARTESIAN_POINT ( 'NONE',  ( 12.00000000000001776, 15.00000000000000000, -29.68999999999999417 ) ) ;
#45727 = ORIENTED_EDGE ( 'NONE', *, *, #50588, .F. ) ;
#45728 = SURFACE_STYLE_FILL_AREA ( #24222 ) ;
#45729 = CARTESIAN_POINT ( 'NONE',  ( -180.5049999999999670, -6.826472737025115478, -4.959722759717899443 ) ) ;
#45730 = DIRECTION ( 'NONE',  ( -0.000000000000000000, -0.000000000000000000, 1.000000000000000000 ) ) ;
#45731 =( LENGTH_UNIT ( ) NAMED_UNIT ( * ) SI_UNIT ( .MILLI., .METRE. ) );
#45732 = CARTESIAN_POINT ( 'NONE',  ( -59.60707362346616378, -8.102448949553172852, 5.886773742842742685 ) ) ;
#45733 = DIRECTION ( 'NONE',  ( 0.000000000000000000, 0.000000000000000000, 1.000000000000000000 ) ) ;
#45734 = ORIENTED_EDGE ( 'NONE', *, *, #69082, .F. ) ;
#45735 =( LENGTH_UNIT ( ) NAMED_UNIT ( * ) SI_UNIT ( .MILLI., .METRE. ) );
#45736 = FILL_AREA_STYLE ('',( #62896 ) ) ;
#45737 = CARTESIAN_POINT ( 'NONE',  ( 13.74999999999998757, -7.950815931560351124E-15, 4.000000000000000000 ) ) ;
#45738 = CARTESIAN_POINT ( 'NONE',  ( -104.7549999999999812, 4.716976649647091513, -6.492361379858946790 ) ) ;
#45739 = DIRECTION ( 'NONE',  ( -1.000000000000000000, -0.000000000000000000, -0.000000000000000000 ) ) ;
#45740 =( NAMED_UNIT ( * ) SI_UNIT ( $, .STERADIAN. ) SOLID_ANGLE_UNIT ( ) );
#45741 = AXIS2_PLACEMENT_3D ( 'NONE', #15356, #69471, #9006 ) ;
#45742 = CARTESIAN_POINT ( 'NONE',  ( -102.8949999999999818, 6.826472737025115478, 4.959722759717899443 ) ) ;
#45743 = CARTESIAN_POINT ( 'NONE',  ( -8.102448949553181734, 114.6049999999999756, 5.886773742842747126 ) ) ;
#45744 = VECTOR ( 'NONE', #47274, 1000.000000000000000 ) ;
#45745 = CARTESIAN_POINT ( 'NONE',  ( -67.94499999999999318, -9.827790563157499189E-16, -8.024999999999991473 ) ) ;
#45746 = CARTESIAN_POINT ( 'NONE',  ( 35.99999999999999289, 5.000000000000000000, 72.00402776293825013 ) ) ;
#45747 = FACE_OUTER_BOUND ( 'NONE', #41099, .T. ) ;
#45748 = CARTESIAN_POINT ( 'NONE',  ( 0.000000000000000000, 0.000000000000000000, 0.2500000000000011102 ) ) ;
#45749 = DIRECTION ( 'NONE',  ( 0.000000000000000000, 0.000000000000000000, 1.000000000000000000 ) ) ;
#45750 = VERTEX_POINT ( 'NONE', #14253 ) ;
#45751 = CARTESIAN_POINT ( 'NONE',  ( -113.8429263765337964, 9.058813317711329915, -2.943386871421373119 ) ) ;
#45752 = CARTESIAN_POINT ( 'NONE',  ( -137.8449999999999989, -7.632228543268599452, 2.479861379858951054 ) ) ;
#45753 = CIRCLE ( 'NONE', #46930, 0.2500000000000002220 ) ;
#45754 = CARTESIAN_POINT ( 'NONE',  ( 0.000000000000000000, 87.30187232391182306, 8.025000000000000355 ) ) ;
#45756 = FACE_OUTER_BOUND ( 'NONE', #8106, .T. ) ;
#45755 = FACE_OUTER_BOUND ( 'NONE', #54363, .T. ) ;
#45757 = FILL_AREA_STYLE_COLOUR ( '', #42958 ) ;
#45758 = ORIENTED_EDGE ( 'NONE', *, *, #63167, .F. ) ;
#45759 = ORIENTED_EDGE ( 'NONE', *, *, #22043, .T. ) ;
#45760 = LINE ( 'NONE', #24261, #1574 ) ;
#45761 = CARTESIAN_POINT ( 'NONE',  ( 1.400957079539663752, 2.390838073342431258, 7.000000000000000000 ) ) ;
#45762 = CARTESIAN_POINT ( 'NONE',  ( -195.0000000000000000, 0.000000000000000000, 0.000000000000000000 ) ) ;
#45763 = CARTESIAN_POINT ( 'NONE',  ( -127.2570736234661695, 5.598654528085800663, -7.705886871421367523 ) ) ;
#45764 = ORIENTED_EDGE ( 'NONE', *, *, #13245, .F. ) ;
#45765 = CARTESIAN_POINT ( 'NONE',  ( -127.8549999999999898, 4.716976649647094177, 6.492361379858945902 ) ) ;
#45766 = ORIENTED_EDGE ( 'NONE', *, *, #26275, .F. ) ;
#45767 = CARTESIAN_POINT ( 'NONE',  ( -127.1070736234661922, 8.102448949553171076, -5.886773742842744461 ) ) ;
#45768 = ORIENTED_EDGE ( 'NONE', *, *, #56948, .T. ) ;
#45769 = CARTESIAN_POINT ( 'NONE',  ( -171.8929263765338078, -8.102448949553174629, -5.886773742842741797 ) ) ;
#45770 = CARTESIAN_POINT ( 'NONE',  ( -84.14292637653379359, 5.598654528085800663, -7.705886871421367523 ) ) ;
#45771 = ORIENTED_EDGE ( 'NONE', *, *, #23212, .T. ) ;
#45772 = EDGE_CURVE ( 'NONE', #11926, #13586, #29379, .T. ) ;
#45773 = DIRECTION ( 'NONE',  ( 0.000000000000000000, 0.000000000000000000, 1.000000000000000000 ) ) ;
#45774 = CARTESIAN_POINT ( 'NONE',  ( 9.058813317711338797, 144.8449999999999989, -2.943386871421372675 ) ) ;
#45775 = SURFACE_STYLE_FILL_AREA ( #24278 ) ;
#45776 = VERTEX_POINT ( 'NONE', #3656 ) ;
#45777 = FILL_AREA_STYLE_COLOUR ( '', #57760 ) ;
#45778 = CARTESIAN_POINT ( 'NONE',  ( -5.598654528085808657, 144.7549999999999955, 7.705886871421373741 ) ) ;
#45779 = CYLINDRICAL_SURFACE ( 'NONE', #47441, 13.00000000000000178 ) ;
#45780 = ORIENTED_EDGE ( 'NONE', *, *, #67094, .F. ) ;
#45781 = CARTESIAN_POINT ( 'NONE',  ( 6.826472737025119919, 118.8929263765337936, 4.959722759717908325 ) ) ;
#45782 = FILL_AREA_STYLE ('',( #2796 ) ) ;
#45783 = COLOUR_RGB ( '', 0.72549020, 0.75294118, 0.79215686) ;
#45784 = STYLED_ITEM ( 'NONE', ( #58079 ), #65509 ) ;
#45785 = EDGE_CURVE ( 'NONE', #29677, #44784, #1261, .T. ) ;
#45786 = FACE_OUTER_BOUND ( 'NONE', #7489, .T. ) ;
#45787 = VECTOR ( 'NONE', #9182, 1000.000000000000000 ) ;
#45788 = ORIENTED_EDGE ( 'NONE', *, *, #6820, .T. ) ;
#45789 = EDGE_CURVE ( 'NONE', #29357, #7058, #23765, .T. ) ;
#45790 = CARTESIAN_POINT ( 'NONE',  ( -3.535366420403589061, -9.000000000000005329, 0.6617903051486780930 ) ) ;
#45791 = ORIENTED_EDGE ( 'NONE', *, *, #62862, .F. ) ;
#45792 =( LENGTH_UNIT ( ) NAMED_UNIT ( * ) SI_UNIT ( .MILLI., .METRE. ) );
#45793 = CARTESIAN_POINT ( 'NONE',  ( -30.86848549628973615, -7.933252306487679206, -1.326499884503476334 ) ) ;
#45794 = CYLINDRICAL_SURFACE ( 'NONE', #50903, 0.2500000000000002220 ) ;
#45795 = CARTESIAN_POINT ( 'NONE',  ( -165.2050000000000125, -2.607480562269071545, -8.024999999999991473 ) ) ;
#45797 = ORIENTED_EDGE ( 'NONE', *, *, #27689, .F. ) ;
#45796 = EDGE_CURVE ( 'NONE', #55073, #41299, #66546, .T. ) ;
#45798 = ADVANCED_FACE ( 'NONE', ( #58205 ), #53287, .F. ) ;
#45799 = SURFACE_STYLE_USAGE ( .BOTH. , #62290 ) ;
#45800 = ORIENTED_EDGE ( 'NONE', *, *, #18026, .F. ) ;
#45801 = SURFACE_SIDE_STYLE ('',( #25003 ) ) ;
#45802 = ORIENTED_EDGE ( 'NONE', *, *, #20150, .T. ) ;
#45803 = FILL_AREA_STYLE ('',( #24309 ) ) ;
#45805 = EDGE_CURVE ( 'NONE', #45655, #49491, #67569, .T. ) ;
#45804 = TOROIDAL_SURFACE ( 'NONE', #31139, 14.49999999999999822, 0.5000000000000000000 ) ;
#45806 =( NAMED_UNIT ( * ) SI_UNIT ( $, .STERADIAN. ) SOLID_ANGLE_UNIT ( ) );
#45807 = DIRECTION ( 'NONE',  ( -0.000000000000000000, -0.000000000000000000, 1.000000000000000000 ) ) ;
#45808 = CARTESIAN_POINT ( 'NONE',  ( -74.75499999999998124, 4.716976649647091513, -6.492361379858946790 ) ) ;
#45809 = VERTEX_POINT ( 'NONE', #68776 ) ;
#45810 = CYLINDRICAL_SURFACE ( 'NONE', #38524, 0.5000000000000004441 ) ;
#45811 = DIRECTION ( 'NONE',  ( -0.000000000000000000, -1.000000000000000000, -0.000000000000000000 ) ) ;
#45812 = CARTESIAN_POINT ( 'NONE',  ( -75.00000000000000000, 8.062885798616331812, -5.903555993539113089 ) ) ;
#45813 = VERTEX_POINT ( 'NONE', #53614 ) ;
#45814 = CARTESIAN_POINT ( 'NONE',  ( -33.72126112590540004, -9.584527543374615988, -3.208686727472596978 ) ) ;
#45816 = DIRECTION ( 'NONE',  ( 0.000000000000000000, 0.000000000000000000, 1.000000000000000000 ) ) ;
#45815 = CARTESIAN_POINT ( 'NONE',  ( 26.25000000000001066, 18.99999999999997868, -3.750000000000000000 ) ) ;
#45817 = CARTESIAN_POINT ( 'NONE',  ( -9.058813317711338797, 137.3449999999999989, 2.943386871421373563 ) ) ;
#45818 = CARTESIAN_POINT ( 'NONE',  ( -107.0949999999999847, -2.607480562269071545, -8.024999999999991473 ) ) ;
#45819 = SURFACE_STYLE_FILL_AREA ( #19030 ) ;
#45820 = CARTESIAN_POINT ( 'NONE',  ( -24.00000000000000000, 1.000000000000000000, 4.000000000000000000 ) ) ;
#45822 = CARTESIAN_POINT ( 'NONE',  ( -71.84292637653381064, 9.058813317711329915, -2.943386871421373119 ) ) ;
#45821 = DIRECTION ( 'NONE',  ( 1.156482317317873451E-16, 1.000000000000000000, -0.000000000000000000 ) ) ;
#45823 = AXIS2_PLACEMENT_3D ( 'NONE', #55472, #1931, #54423 ) ;
#45824 = CARTESIAN_POINT ( 'NONE',  ( -146.6929263765337623, 10.01517768586948698, -1.839758294383808571E-15 ) ) ;
#45825 =( NAMED_UNIT ( * ) SI_UNIT ( $, .STERADIAN. ) SOLID_ANGLE_UNIT ( ) );
#45826 = CARTESIAN_POINT ( 'NONE',  ( -166.0449999999999875, 7.632228543268600340, 2.479861379858949277 ) ) ;
#45827 = AXIS2_PLACEMENT_3D ( 'NONE', #31666, #53143, #26386 ) ;
#45828 = CYLINDRICAL_SURFACE ( 'NONE', #53911, 0.5000000000000004441 ) ;
#45829 = ORIENTED_EDGE ( 'NONE', *, *, #66890, .T. ) ;
#45830 = CIRCLE ( 'NONE', #14364, 0.5000000000000004441 ) ;
#45831 = CARTESIAN_POINT ( 'NONE',  ( -4.716976649647097730, 129.2429263765338021, -6.492361379858953896 ) ) ;
#45832 = VERTEX_POINT ( 'NONE', #42085 ) ;
#45833 = CARTESIAN_POINT ( 'NONE',  ( 4.000000000000002665, 43.00000000000000000, -89.00000000000000000 ) ) ;
#45834 = CARTESIAN_POINT ( 'NONE',  ( -4.750000000000002665, 24.99999999999998579, 3.750000000000000000 ) ) ;
#45835 = CYLINDRICAL_SURFACE ( 'NONE', #37190, 9.524999999999991473 ) ;
#45836 = DIRECTION ( 'NONE',  ( 0.000000000000000000, -1.000000000000000000, -0.000000000000000000 ) ) ;
#45837 = AXIS2_PLACEMENT_3D ( 'NONE', #63182, #20616, #4774 ) ;
#45838 = CARTESIAN_POINT ( 'NONE',  ( -74.99999999999998579, 50.00000000000000000, -7.500000000000000000 ) ) ;
#45839 = ORIENTED_EDGE ( 'NONE', *, *, #16761, .F. ) ;
#45840 = CARTESIAN_POINT ( 'NONE',  ( -162.2049999999999557, -2.607480562269071545, -8.024999999999991473 ) ) ;
#45841 = ORIENTED_EDGE ( 'NONE', *, *, #33208, .F. ) ;
#45842 = VERTEX_POINT ( 'NONE', #16020 ) ;
#45843 = EDGE_CURVE ( 'NONE', #29016, #3957, #44062, .T. ) ;
#45844 = DIRECTION ( 'NONE',  ( 1.000000000000000000, -1.189524669241239115E-16, 0.000000000000000000 ) ) ;
#45845 = DIRECTION ( 'NONE',  ( 0.000000000000000000, 0.000000000000000000, -1.000000000000000000 ) ) ;
#45846 = CARTESIAN_POINT ( 'NONE',  ( 3.094860106618435136, 115.2949999999999733, -9.525000000000000355 ) ) ;
#45847 = EDGE_CURVE ( 'NONE', #46203, #27439, #34979, .T. ) ;
#45848 = ORIENTED_EDGE ( 'NONE', *, *, #34707, .T. ) ;
#45849 = FACE_BOUND ( 'NONE', #38251, .T. ) ;
#45850 = CARTESIAN_POINT ( 'NONE',  ( 0.000000000000000000, 113.5549999999999926, -9.525000000000000355 ) ) ;
#45851 = CARTESIAN_POINT ( 'NONE',  ( -77.30499999999996419, 8.437984349512086979, -1.550032578732815448E-15 ) ) ;
#45852 = FILL_AREA_STYLE ('',( #24025 ) ) ;
#45853 = EDGE_LOOP ( 'NONE', ( #38339, #60135, #19891 ) ) ;
#45854 = CARTESIAN_POINT ( 'NONE',  ( -5.598654528085808657, 135.7549999999999955, 7.705886871421373741 ) ) ;
#45855 = FILL_AREA_STYLE ('',( #51125 ) ) ;
#45856 = EDGE_CURVE ( 'NONE', #4579, #49504, #13680, .T. ) ;
#45857 = CARTESIAN_POINT ( 'NONE',  ( -48.00000000000000000, 13.41640786499872284, 7.500000000000000000 ) ) ;
#45858 = CARTESIAN_POINT ( 'NONE',  ( 0.000000000000000000, -3.500000000000000000, 0.000000000000000000 ) ) ;
#45859 = EDGE_CURVE ( 'NONE', #31646, #52813, #47423, .T. ) ;
#45860 = CARTESIAN_POINT ( 'NONE',  ( 0.000000000000000000, 2.299999999999999822, 0.000000000000000000 ) ) ;
#45861 = VERTEX_POINT ( 'NONE', #16367 ) ;
#45862 = DIRECTION ( 'NONE',  ( 1.000000000000000000, 0.000000000000000000, 0.000000000000000000 ) ) ;
#45863 = CARTESIAN_POINT ( 'NONE',  ( -49.19499999999999318, 8.437984349512085203, -1.550032578732815448E-15 ) ) ;
#45864 = ORIENTED_EDGE ( 'NONE', *, *, #47883, .T. ) ;
#45865 = PLANE ( 'NONE',  #12598 ) ;
#45866 = CARTESIAN_POINT ( 'NONE',  ( 7.441974819423174736, 2.003239292658530513, -1.110121504110836987 ) ) ;
#45867 = DIRECTION ( 'NONE',  ( -1.000000000000000000, 1.224646799147349509E-16, 0.000000000000000000 ) ) ;
#45868 = EDGE_CURVE ( 'NONE', #10026, #63373, #68738, .T. ) ;
#45869 =( LENGTH_UNIT ( ) NAMED_UNIT ( * ) SI_UNIT ( .MILLI., .METRE. ) );
#45870 = ORIENTED_EDGE ( 'NONE', *, *, #59099, .T. ) ;
#45871 = CARTESIAN_POINT ( 'NONE',  ( -55.94499999999999318, -9.827790563157499189E-16, -8.024999999999991473 ) ) ;
#45872 = CYLINDRICAL_SURFACE ( 'NONE', #14201, 0.5000000000000004441 ) ;
#45873 = ORIENTED_EDGE ( 'NONE', *, *, #25876, .F. ) ;
#45874 = VECTOR ( 'NONE', #55706, 1000.000000000000000 ) ;
#45875 = AXIS2_PLACEMENT_3D ( 'NONE', #15689, #15007, #4759 ) ;
#45876 = CYLINDRICAL_SURFACE ( 'NONE', #24672, 0.9999999999999995559 ) ;
#45877 = CARTESIAN_POINT ( 'NONE',  ( -104.9049999999999869, 2.607480562269068880, -8.024999999999993250 ) ) ;
#45878 = VERTEX_POINT ( 'NONE', #26178 ) ;
#45879 = LINE ( 'NONE', #62018, #10053 ) ;
#45880 = AXIS2_PLACEMENT_3D ( 'NONE', #9308, #30731, #25463 ) ;
#45881 = CARTESIAN_POINT ( 'NONE',  ( -141.9570736234661865, 9.058813317711329915, -2.943386871421373119 ) ) ;
#45882 = B_SPLINE_CURVE_WITH_KNOTS ( 'NONE', 3,
 ( #55487, #56163, #55829, #29068, #50566, #2291, #7992, #29437 ),
 .UNSPECIFIED., .F., .F.,
 ( 4, 2, 2, 4 ),
 ( 2.544313220892526165E-07, 0.002693395767724534023, 0.004039966435925755432, 0.005386537104126977275 ),
 .UNSPECIFIED. ) ;
#45883 = LINE ( 'NONE', #44858, #2457 ) ;
#45884 = CARTESIAN_POINT ( 'NONE',  ( 9.058813317711338797, 141.8449999999999989, -2.943386871421372675 ) ) ;
#45885 = CARTESIAN_POINT ( 'NONE',  ( -83.90707362346614673, -3.094860106618429807, 9.524999999999991473 ) ) ;
#45886 = CARTESIAN_POINT ( 'NONE',  ( -92.99292637653380211, 8.102448949553172852, -5.886773742842744461 ) ) ;
#45887 = FILL_AREA_STYLE_COLOUR ( '', #33856 ) ;
#45888 = CARTESIAN_POINT ( 'NONE',  ( 57.00000000000000000, 5.000000000000000000, 60.00402776293827145 ) ) ;
#45889 = AXIS2_PLACEMENT_3D ( 'NONE', #32444, #44114, #16667 ) ;
#45891 = CARTESIAN_POINT ( 'NONE',  ( -100.9429263765338050, 0.000000000000000000, 9.524999999999991473 ) ) ;
#45890 = CARTESIAN_POINT ( 'NONE',  ( -74.99999999999998579, 50.00000000000000000, -7.000000000000000000 ) ) ;
#45892 = CARTESIAN_POINT ( 'NONE',  ( -119.0049999999999955, 6.826472737025116366, 4.959722759717898555 ) ) ;
#45893 = CARTESIAN_POINT ( 'NONE',  ( -158.9929263765338021, 8.102448949553172852, -5.886773742842744461 ) ) ;
#45894 = CARTESIAN_POINT ( 'NONE',  ( -5.598654528085808657, 113.6449999999999818, 7.705886871421373741 ) ) ;
#45895 = CARTESIAN_POINT ( 'NONE',  ( -137.8449999999999989, -7.632228543268599452, 2.479861379858951054 ) ) ;
#45896 = CARTESIAN_POINT ( 'NONE',  ( -121.4949999999999761, 6.826472737025113702, -4.959722759717902107 ) ) ;
#45897 = DIRECTION ( 'NONE',  ( 0.7071067811865474617, 0.000000000000000000, 0.7071067811865474617 ) ) ;
#45898 = ORIENTED_EDGE ( 'NONE', *, *, #7252, .F. ) ;
#45899 = EDGE_CURVE ( 'NONE', #39384, #34141, #66453, .T. ) ;
#45900 = FACE_OUTER_BOUND ( 'NONE', #20058, .T. ) ;
#45901 = SPHERICAL_SURFACE ( 'NONE', #33468, 1.000000000000000000 ) ;
#45902 = SURFACE_SIDE_STYLE ('',( #2198 ) ) ;
#45903 = AXIS2_PLACEMENT_3D ( 'NONE', #58765, #32032, #5977 ) ;
#45904 = CARTESIAN_POINT ( 'NONE',  ( -174.5929263765337964, -3.094860106618431139, -9.524999999999991473 ) ) ;
#45905 = CARTESIAN_POINT ( 'NONE',  ( -48.29499999999997328, -2.607480562269069768, 8.024999999999991473 ) ) ;
#45906 = CIRCLE ( 'NONE', #58274, 1.000000000000000888 ) ;
#45907 = SURFACE_STYLE_FILL_AREA ( #68385 ) ;
#45908 = VECTOR ( 'NONE', #65810, 1000.000000000000114 ) ;
#45909 =( NAMED_UNIT ( * ) PLANE_ANGLE_UNIT ( ) SI_UNIT ( $, .RADIAN. ) );
#45910 = DIRECTION ( 'NONE',  ( -1.000000000000000000, 0.000000000000000000, 0.000000000000000000 ) ) ;
#45911 = VERTEX_POINT ( 'NONE', #42423 ) ;
#45912 = UNCERTAINTY_MEASURE_WITH_UNIT (LENGTH_MEASURE( 1.000000000000000082E-05 ), #48097, 'distance_accuracy_value', 'NONE');
#45913 = CARTESIAN_POINT ( 'NONE',  ( -86.69292637653380496, 10.01517768586948698, -1.839758294383808571E-15 ) ) ;
#45914 = PRODUCT_CONTEXT ( 'NONE', #62165, 'mechanical' ) ;
#45915 = CARTESIAN_POINT ( 'NONE',  ( -53.56480923418825313, -9.954352215710184026, -2.522777614992231410 ) ) ;
#45916 = DIRECTION ( 'NONE',  ( -0.000000000000000000, 1.000000000000000000, -0.000000000000000000 ) ) ;
#45917 = SURFACE_STYLE_FILL_AREA ( #40288 ) ;
#45918 = PRESENTATION_STYLE_ASSIGNMENT (( #56442 ) ) ;
#45919 = DIRECTION ( 'NONE',  ( 0.000000000000000000, 0.000000000000000000, 1.000000000000000000 ) ) ;
#45920 = PRESENTATION_LAYER_ASSIGNMENT (  '', '', ( #31253 ) ) ;
#45921 = AXIS2_PLACEMENT_3D ( 'NONE', #15284, #14545, #19824 ) ;
#45922 = EDGE_CURVE ( 'NONE', #30865, #62777, #64268, .T. ) ;
#45923 = LINE ( 'NONE', #35700, #49617 ) ;
#45924 = EDGE_CURVE ( 'NONE', #3912, #51799, #22647, .T. ) ;
#45925 = ORIENTED_EDGE ( 'NONE', *, *, #61507, .F. ) ;
#45926 = CARTESIAN_POINT ( 'NONE',  ( -106.9429263765337907, 0.000000000000000000, 9.524999999999991473 ) ) ;
#45927 = CARTESIAN_POINT ( 'NONE',  ( 34.99999999999999289, 99.99999999999998579, 3.500000000000000000 ) ) ;
#45928 = DIRECTION ( 'NONE',  ( 1.000000000000000000, 0.000000000000000000, 0.000000000000000000 ) ) ;
#45929 = EDGE_LOOP ( 'NONE', ( #14516, #41539, #68855 ) ) ;
#45930 = DIRECTION ( 'NONE',  ( 0.000000000000000000, 0.000000000000000000, -1.000000000000000000 ) ) ;
#45931 = PRESENTATION_LAYER_ASSIGNMENT (  '', '', ( #37016 ) ) ;
#45932 = CARTESIAN_POINT ( 'NONE',  ( -7.632228543268608334, 133.9570736234661581, 2.479861379858952830 ) ) ;
#45933 = EDGE_CURVE ( 'NONE', #12077, #64678, #30993, .T. ) ;
#45934 = AXIS2_PLACEMENT_3D ( 'NONE', #16798, #22390, #65988 ) ;
#45935 = ORIENTED_EDGE ( 'NONE', *, *, #47130, .T. ) ;
#45936 = FILL_AREA_STYLE ('',( #50845 ) ) ;
#45937 =( GEOMETRIC_REPRESENTATION_CONTEXT ( 3 ) GLOBAL_UNCERTAINTY_ASSIGNED_CONTEXT ( ( #7307 ) ) GLOBAL_UNIT_ASSIGNED_CONTEXT ( ( #37353, #64728, #47924 ) ) REPRESENTATION_CONTEXT ( 'NONE', 'WORKASPACE' ) );
#45938 =( LENGTH_UNIT ( ) NAMED_UNIT ( * ) SI_UNIT ( .MILLI., .METRE. ) );
#45939 = ORIENTED_EDGE ( 'NONE', *, *, #55524, .T. ) ;
#45940 = DIRECTION ( 'NONE',  ( 1.000000000000000000, -0.000000000000000000, -1.300977106640434891E-16 ) ) ;
#45941 = CARTESIAN_POINT ( 'NONE',  ( -74.99999999999998579, 50.00000000000000000, 10.00000000000000000 ) ) ;
#45942 = DIRECTION ( 'NONE',  ( 0.000000000000000000, 1.000000000000000000, 0.000000000000000000 ) ) ;
#45943 = EDGE_CURVE ( 'NONE', #23561, #7596, #13521, .T. ) ;
#45944 = DIRECTION ( 'NONE',  ( 1.000000000000000000, 0.000000000000000000, 0.000000000000000000 ) ) ;
#45945 = CARTESIAN_POINT ( 'NONE',  ( -79.34499999999998465, 7.632228543268599452, -2.479861379858951942 ) ) ;
#45946 = ORIENTED_EDGE ( 'NONE', *, *, #34556, .F. ) ;
#45947 = PRESENTATION_STYLE_ASSIGNMENT (( #7940 ) ) ;
#45948 =( NAMED_UNIT ( * ) PLANE_ANGLE_UNIT ( ) SI_UNIT ( $, .RADIAN. ) );
#45949 = VECTOR ( 'NONE', #20344, 1000.000000000000000 ) ;
#45950 = ADVANCED_FACE ( 'NONE', ( #23004 ), #44154, .F. ) ;
#45951 = UNCERTAINTY_MEASURE_WITH_UNIT (LENGTH_MEASURE( 1.000000000000000082E-05 ), #61472, 'distance_accuracy_value', 'NONE');
#45952 = ORIENTED_EDGE ( 'NONE', *, *, #66218, .F. ) ;
#45953 = LINE ( 'NONE', #41725, #69581 ) ;
#45954 = CIRCLE ( 'NONE', #24505, 19.99999999999998934 ) ;
#45955 = CARTESIAN_POINT ( 'NONE',  ( -69.74999999999998579, -4.000000000000000000, 0.000000000000000000 ) ) ;
#45956 = DIRECTION ( 'NONE',  ( 0.000000000000000000, 1.000000000000000000, 0.000000000000000000 ) ) ;
#45957 = ORIENTED_EDGE ( 'NONE', *, *, #24928, .T. ) ;
#45958 = SURFACE_STYLE_FILL_AREA ( #56122 ) ;
#45959 = ORIENTED_EDGE ( 'NONE', *, *, #41987, .F. ) ;
#45960 = DIRECTION ( 'NONE',  ( 0.000000000000000000, 0.000000000000000000, -1.000000000000000000 ) ) ;
#45961 = VECTOR ( 'NONE', #13029, 1000.000000000000000 ) ;
#45962 = CARTESIAN_POINT ( 'NONE',  ( -171.3570736234661922, 5.598654528085804216, 7.705886871421366635 ) ) ;
#45963 = FACE_OUTER_BOUND ( 'NONE', #32705, .T. ) ;
#45964 = CARTESIAN_POINT ( 'NONE',  ( 9.058813317711337021, 111.5449999999999875, 2.943386871421375783 ) ) ;
#45965 = MECHANICAL_DESIGN_GEOMETRIC_PRESENTATION_REPRESENTATION (  '', ( #61627 ), #39290 ) ;
#45966 = CARTESIAN_POINT ( 'NONE',  ( -113.4570736234661723, -9.058813317711329915, 2.943386871421371787 ) ) ;
#45967 = DIRECTION ( 'NONE',  ( 0.000000000000000000, 0.000000000000000000, -1.000000000000000000 ) ) ;
#45968 = FACE_OUTER_BOUND ( 'NONE', #16695, .T. ) ;
#45969 = ORIENTED_EDGE ( 'NONE', *, *, #22578, .F. ) ;
#45970 = COLOUR_RGB ( '', 0.72549020, 0.75294118, 0.79215686) ;
#45971 = CARTESIAN_POINT ( 'NONE',  ( 0.000000000000000000, 122.9429263765338192, -8.025000000000000355 ) ) ;
#45972 = COLOUR_RGB ( '', 0.08235294, 0.09019608, 0.10196078) ;
#45974 = DIRECTION ( 'NONE',  ( 9.376883653928687363E-17, -1.000000000000000000, 0.000000000000000000 ) ) ;
#45973 = DIRECTION ( 'NONE',  ( -0.9704308468600219006, -0.2413793103448194921, 0.000000000000000000 ) ) ;
#45975 = DIRECTION ( 'NONE',  ( -0.000000000000000000, -0.000000000000000000, 1.000000000000000000 ) ) ;
#45976 = CARTESIAN_POINT ( 'NONE',  ( -154.7049999999999841, 2.607480562269073321, 8.024999999999991473 ) ) ;
#45977 = CARTESIAN_POINT ( 'NONE',  ( -166.1949999999999932, 8.437984349512085203, -1.550032578732815448E-15 ) ) ;
#45978 = AXIS2_PLACEMENT_3D ( 'NONE', #39236, #34603, #66634 ) ;
#45979 = CARTESIAN_POINT ( 'NONE',  ( -144.1449999999999818, -4.716976649647092401, 6.492361379858946790 ) ) ;
#45980 = ORIENTED_EDGE ( 'NONE', *, *, #14623, .F. ) ;
#45981 = PRESENTATION_LAYER_ASSIGNMENT (  '', '', ( #44891 ) ) ;
#45982 = ADVANCED_FACE ( 'NONE', ( #6449 ), #35287, .T. ) ;
#45983 = CARTESIAN_POINT ( 'NONE',  ( -66.59292637653379643, -3.094860106618431139, -9.524999999999991473 ) ) ;
#45984 = DIRECTION ( 'NONE',  ( 1.000000000000000000, 4.336808689941999001E-16, 0.000000000000000000 ) ) ;
#45985 = SURFACE_SIDE_STYLE ('',( #51245 ) ) ;
#45986 = CARTESIAN_POINT ( 'NONE',  ( -65.75499999999998124, 4.716976649647091513, -6.492361379858946790 ) ) ;
#45987 = FACE_OUTER_BOUND ( 'NONE', #33628, .T. ) ;
#45988 = DIRECTION ( 'NONE',  ( 1.000000000000000000, -0.000000000000000000, 0.000000000000000000 ) ) ;
#45989 = CARTESIAN_POINT ( 'NONE',  ( -65.84499999999998465, -7.632228543268599452, 2.479861379858951054 ) ) ;
#45990 = CARTESIAN_POINT ( 'NONE',  ( 5.598654528085809545, 155.2549999999999670, -7.705886871421373741 ) ) ;
#45991 = CARTESIAN_POINT ( 'NONE',  ( -143.3070736234661524, -10.01517768586948698, 6.132527647946031529E-16 ) ) ;
#45992 = DIRECTION ( 'NONE',  ( 0.000000000000000000, -0.000000000000000000, 1.000000000000000000 ) ) ;
#45993 = UNCERTAINTY_MEASURE_WITH_UNIT (LENGTH_MEASURE( 1.000000000000000082E-05 ), #66920, 'distance_accuracy_value', 'NONE');
#45994 = DIRECTION ( 'NONE',  ( -0.000000000000000000, -0.000000000000000000, 1.000000000000000000 ) ) ;
#45995 = PRODUCT_DEFINITION ( 'UNKNOWN', '', #31526, #64216 ) ;
#45996 = CARTESIAN_POINT ( 'NONE',  ( 5.196152422706629359, 9.000000000000008882, 1.392304845413260272 ) ) ;
#45997 = ADVANCED_FACE ( 'NONE', ( #27883 ), #20734, .F. ) ;
#45998 = EDGE_CURVE ( 'NONE', #11115, #40876, #45003, .T. ) ;
#45999 = DIRECTION ( 'NONE',  ( 0.000000000000000000, 1.000000000000000000, 0.000000000000000000 ) ) ;
#46000 = DIRECTION ( 'NONE',  ( -0.000000000000000000, -0.000000000000000000, 1.000000000000000000 ) ) ;
#46001 = CIRCLE ( 'NONE', #33575, 4.999999999999997335 ) ;
#46002 = ADVANCED_FACE ( 'NONE', ( #68339 ), #20462, .F. ) ;
#46003 = LINE ( 'NONE', #3005, #25986 ) ;
#46004 = EDGE_CURVE ( 'NONE', #7942, #49243, #21171, .T. ) ;
#46005 = AXIS2_PLACEMENT_3D ( 'NONE', #49781, #2565, #66997 ) ;
#46006 = DIRECTION ( 'NONE',  ( -1.000000000000000000, 0.000000000000000000, 0.000000000000000000 ) ) ;
#46007 = CARTESIAN_POINT ( 'NONE',  ( -4.390521455347699664, -1.510510638266201466, -9.000000000000003553 ) ) ;
#46008 = VERTEX_POINT ( 'NONE', #25416 ) ;
#46009 = MECHANICAL_DESIGN_GEOMETRIC_PRESENTATION_REPRESENTATION (  '', ( #49356 ), #63949 ) ;
#46010 = ORIENTED_EDGE ( 'NONE', *, *, #21284, .F. ) ;
#46011 = CARTESIAN_POINT ( 'NONE',  ( -53.60138881051016568, -9.947368421052624754, -2.000000000000000000 ) ) ;
#46012 = VECTOR ( 'NONE', #7140, 1000.000000000000000 ) ;
#46014 = AXIS2_PLACEMENT_3D ( 'NONE', #31055, #2895, #14911 ) ;
#46013 = DIRECTION ( 'NONE',  ( 0.000000000000000000, 0.000000000000000000, -1.000000000000000000 ) ) ;
#46015 = SHAPE_REPRESENTATION ( '13. Bolt M6x45', ( #42840 ), #2196 ) ;
#46016 = EDGE_CURVE ( 'NONE', #55848, #408, #21527, .T. ) ;
#46017 = CARTESIAN_POINT ( 'NONE',  ( 48.50000000000000000, 14.49137674618942562, -7.500000000000000000 ) ) ;
#46018 = DIRECTION ( 'NONE',  ( -1.000000000000000000, 0.000000000000000000, 0.000000000000000000 ) ) ;
#46019 = PRESENTATION_LAYER_ASSIGNMENT (  '', '', ( #6660 ) ) ;
#46020 = FACE_BOUND ( 'NONE', #23409, .T. ) ;
#46021 = EDGE_CURVE ( 'NONE', #58067, #4438, #14887, .T. ) ;
#46022 = ORIENTED_EDGE ( 'NONE', *, *, #40438, .F. ) ;
#46023 = ORIENTED_EDGE ( 'NONE', *, *, #24005, .F. ) ;
#46024 = DIRECTION ( 'NONE',  ( 0.000000000000000000, 0.000000000000000000, -1.000000000000000000 ) ) ;
#46025 =( LENGTH_UNIT ( ) NAMED_UNIT ( * ) SI_UNIT ( .MILLI., .METRE. ) );
#46026 = VERTEX_POINT ( 'NONE', #20119 ) ;
#46027 = CARTESIAN_POINT ( 'NONE',  ( -65.99292637653378790, 8.102448949553172852, -5.886773742842744461 ) ) ;
#46028 = CARTESIAN_POINT ( 'NONE',  ( -144.7429263765338021, -5.598654528085803328, -7.705886871421366635 ) ) ;
#46029 = ORIENTED_EDGE ( 'NONE', *, *, #44675, .T. ) ;
#46030 =( GEOMETRIC_REPRESENTATION_CONTEXT ( 3 ) GLOBAL_UNCERTAINTY_ASSIGNED_CONTEXT ( ( #22146 ) ) GLOBAL_UNIT_ASSIGNED_CONTEXT ( ( #24735, #56414, #30707 ) ) REPRESENTATION_CONTEXT ( 'NONE', 'WORKASPACE' ) );
#46031 = LINE ( 'NONE', #24184, #27477 ) ;
#46032 = DIRECTION ( 'NONE',  ( 0.000000000000000000, 0.000000000000000000, 1.000000000000000000 ) ) ;
#46033 = CARTESIAN_POINT ( 'NONE',  ( -112.4949999999999761, 6.826472737025113702, -4.959722759717902107 ) ) ;
#46034 = ORIENTED_EDGE ( 'NONE', *, *, #27629, .F. ) ;
#46035 = AXIS2_PLACEMENT_3D ( 'NONE', #14141, #19035, #61959 ) ;
#46036 = DIRECTION ( 'NONE',  ( -1.156482317317873451E-16, 1.000000000000000000, 0.000000000000000000 ) ) ;
#46037 = CARTESIAN_POINT ( 'NONE',  ( -10.51797786690659109, -11.79336193633089636, 2.222196116146513134 ) ) ;
#46038 = ORIENTED_EDGE ( 'NONE', *, *, #30799, .T. ) ;
#46039 = CARTESIAN_POINT ( 'NONE',  ( -9.827790563157511022E-16, 148.4429263765338476, 8.025000000000000355 ) ) ;
#46040 = CARTESIAN_POINT ( 'NONE',  ( -54.69521332591794760, -9.106085870126005233, -2.687031549327465907 ) ) ;
#46041 = CYLINDRICAL_SURFACE ( 'NONE', #46768, 9.524999999999991473 ) ;
#46042 = AXIS2_PLACEMENT_3D ( 'NONE', #17440, #1514, #49108 ) ;
#46043 = CARTESIAN_POINT ( 'NONE',  ( 0.000000000000000000, 2.299999999999999822, 0.000000000000000000 ) ) ;
#46044 = ORIENTED_EDGE ( 'NONE', *, *, #55680, .T. ) ;
#46045 = DIRECTION ( 'NONE',  ( 0.000000000000000000, -1.000000000000000000, 0.000000000000000000 ) ) ;
#46046 = VERTEX_POINT ( 'NONE', #15581 ) ;
#46047 =( LENGTH_UNIT ( ) NAMED_UNIT ( * ) SI_UNIT ( .MILLI., .METRE. ) );
#46048 = CYLINDRICAL_SURFACE ( 'NONE', #50370, 0.2500000000000002220 ) ;
#46049 = DIRECTION ( 'NONE',  ( 0.000000000000000000, 0.000000000000000000, 1.000000000000000000 ) ) ;
#46050 = CARTESIAN_POINT ( 'NONE',  ( -120.6549999999999869, -7.632228543268600340, -2.479861379858950166 ) ) ;
#46052 = ADVANCED_FACE ( 'NONE', ( #31032 ), #15253, .T. ) ;
#46051 = AXIS2_PLACEMENT_3D ( 'NONE', #26193, #20224, #68791 ) ;
#46053 = AXIS2_PLACEMENT_3D ( 'NONE', #63153, #69466, #37153 ) ;
#46054 = ORIENTED_EDGE ( 'NONE', *, *, #55351, .F. ) ;
#46055 = CARTESIAN_POINT ( 'NONE',  ( -17.75000000000000711, 30.99999999999999289, 3.750000000000000000 ) ) ;
#46056 = VECTOR ( 'NONE', #45138, 1000.000000000000000 ) ;
#46057 = DIRECTION ( 'NONE',  ( 0.000000000000000000, 0.000000000000000000, -1.000000000000000000 ) ) ;
#46058 = CARTESIAN_POINT ( 'NONE',  ( -7.632228543268607446, 120.5429263765338135, -2.479861379858953718 ) ) ;
#46059 = VERTEX_POINT ( 'NONE', #10634 ) ;
#46060 = VERTEX_POINT ( 'NONE', #47632 ) ;
#46061 = CARTESIAN_POINT ( 'NONE',  ( -4.041451884327381450, 7.000000000000006217, 7.500000000000000000 ) ) ;
#46062 = LINE ( 'NONE', #61838, #68030 ) ;
#46063 = CARTESIAN_POINT ( 'NONE',  ( 7.750000000000000000, 33.99999999999998579, 4.000000000000000000 ) ) ;
#46064 = CARTESIAN_POINT ( 'NONE',  ( -47.75499999999999545, 4.716976649647091513, -6.492361379858946790 ) ) ;
#46065 = ORIENTED_EDGE ( 'NONE', *, *, #42233, .T. ) ;
#46066 = CARTESIAN_POINT ( 'NONE',  ( -179.3049999999999784, 8.437984349512085203, -1.550032578732815448E-15 ) ) ;
#46067 = CARTESIAN_POINT ( 'NONE',  ( 44.99999999999998579, 119.9999999999999716, 9.500000000000000000 ) ) ;
#46068 =( GEOMETRIC_REPRESENTATION_CONTEXT ( 3 ) GLOBAL_UNCERTAINTY_ASSIGNED_CONTEXT ( ( #65899 ) ) GLOBAL_UNIT_ASSIGNED_CONTEXT ( ( #45792, #34169, #66884 ) ) REPRESENTATION_CONTEXT ( 'NONE', 'WORKASPACE' ) );
#46069 = CARTESIAN_POINT ( 'NONE',  ( -58.70707362346615810, -3.094860106618431139, -9.524999999999991473 ) ) ;
#46070 = COLOUR_RGB ( '', 0.09019608, 0.27058824, 0.51372549) ;
#46071 = CARTESIAN_POINT ( 'NONE',  ( -180.1450000000000102, -4.716976649647092401, 6.492361379858946790 ) ) ;
#46072 = DIRECTION ( 'NONE',  ( 1.000000000000000000, -1.387778780781444256E-14, -1.387778780781444256E-14 ) ) ;
#46073 = VERTEX_POINT ( 'NONE', #26450 ) ;
#46074 = PRESENTATION_LAYER_ASSIGNMENT (  '', '', ( #6714 ) ) ;
#46075 = SURFACE_STYLE_USAGE ( .BOTH. , #34786 ) ;
#46076 = CARTESIAN_POINT ( 'NONE',  ( -94.70499999999999829, 2.607480562269073321, 8.024999999999991473 ) ) ;
#46077 = CARTESIAN_POINT ( 'NONE',  ( 9.534962109133534369, 154.5000000000000284, -0.05439801238995608385 ) ) ;
#46078 = DIRECTION ( 'NONE',  ( 0.000000000000000000, 1.000000000000000000, 0.000000000000000000 ) ) ;
#46079 = AXIS2_PLACEMENT_3D ( 'NONE', #40043, #65350, #12558 ) ;
#46080 = DIRECTION ( 'NONE',  ( 1.000000000000000000, -0.000000000000000000, 0.000000000000000000 ) ) ;
#46081 = CARTESIAN_POINT ( 'NONE',  ( -93.59499999999997044, 2.607480562269072433, 8.024999999999991473 ) ) ;
#46082 = CARTESIAN_POINT ( 'NONE',  ( 9.058813317711337021, 121.6549999999999869, 2.943386871421375783 ) ) ;
#46083 = CARTESIAN_POINT ( 'NONE',  ( -72.44499999999997897, 0.000000000000000000, 8.024999999999991473 ) ) ;
#46084 = FACE_OUTER_BOUND ( 'NONE', #43921, .T. ) ;
#46085 = VECTOR ( 'NONE', #67958, 1000.000000000000000 ) ;
#46086 = PLANE ( 'NONE',  #35998 ) ;
#46087 = UNCERTAINTY_MEASURE_WITH_UNIT (LENGTH_MEASURE( 1.000000000000000082E-05 ), #61542, 'distance_accuracy_value', 'NONE');
#46088 = DIRECTION ( 'NONE',  ( 0.000000000000000000, -1.000000000000000000, 0.000000000000000000 ) ) ;
#46089 =( LENGTH_UNIT ( ) NAMED_UNIT ( * ) SI_UNIT ( .MILLI., .METRE. ) );
#46090 = ORIENTED_EDGE ( 'NONE', *, *, #51549, .T. ) ;
#46091 = EDGE_CURVE ( 'NONE', #1198, #35184, #50800, .T. ) ;
#46092 = CARTESIAN_POINT ( 'NONE',  ( -112.1929263765338050, -10.01517768586948698, 6.132527647946031529E-16 ) ) ;
#46093 = CARTESIAN_POINT ( 'NONE',  ( -129.4449999999999648, 0.000000000000000000, 8.024999999999991473 ) ) ;
#46094 = CARTESIAN_POINT ( 'NONE',  ( 39.24999999999999289, 15.74999999999997513, 4.000000000000000000 ) ) ;
#46095 = AXIS2_PLACEMENT_3D ( 'NONE', #18943, #40445, #13687 ) ;
#46096 = EDGE_CURVE ( 'NONE', #3748, #37645, #28976, .T. ) ;
#46097 = CARTESIAN_POINT ( 'NONE',  ( -23.21231517720797655, 113.4999999999999858, -9.500000000000000000 ) ) ;
#46099 = LINE ( 'NONE', #67520, #43883 ) ;
#46098 = CARTESIAN_POINT ( 'NONE',  ( -131.5429263765338135, 9.058813317711329915, 2.943386871421369566 ) ) ;
#46100 =( LENGTH_UNIT ( ) NAMED_UNIT ( * ) SI_UNIT ( .MILLI., .METRE. ) );
#46101 = VERTEX_POINT ( 'NONE', #32087 ) ;
#46102 = ORIENTED_EDGE ( 'NONE', *, *, #66552, .F. ) ;
#46103 = STYLED_ITEM ( 'NONE', ( #2451 ), #59098 ) ;
#46104 = DIRECTION ( 'NONE',  ( -0.000000000000000000, 1.000000000000000000, -0.000000000000000000 ) ) ;
#46105 = CIRCLE ( 'NONE', #32593, 113.0000000000030127 ) ;
#46106 = CARTESIAN_POINT ( 'NONE',  ( 9.000000000000003553, 25.24999999999998934, 4.000000000000000000 ) ) ;
#46107 = CARTESIAN_POINT ( 'NONE',  ( -72.49999999999998579, 119.9999999999997868, -9.500000000000000000 ) ) ;
#46108 = CARTESIAN_POINT ( 'NONE',  ( 3.499999999999999112, 33.99999999999998579, 4.000000000000000000 ) ) ;
#46109 = EDGE_CURVE ( 'NONE', #50108, #16746, #12556, .T. ) ;
#46110 = ORIENTED_EDGE ( 'NONE', *, *, #21047, .F. ) ;
#46111 = CARTESIAN_POINT ( 'NONE',  ( -127.5550000000000068, 0.000000000000000000, 8.024999999999991473 ) ) ;
#46112 = ORIENTED_EDGE ( 'NONE', *, *, #22167, .T. ) ;
#46113 = DIRECTION ( 'NONE',  ( -1.000000000000000000, 0.000000000000000000, 0.000000000000000000 ) ) ;
#46114 = CARTESIAN_POINT ( 'NONE',  ( -119.1570736234661751, -9.058813317711329915, -2.943386871421370898 ) ) ;
#46115 = ORIENTED_EDGE ( 'NONE', *, *, #18505, .F. ) ;
#46116 = CARTESIAN_POINT ( 'NONE',  ( -4.041451884327381450, -7.000000000000002665, 7.500000000000000000 ) ) ;
#46117 = ORIENTED_EDGE ( 'NONE', *, *, #68305, .T. ) ;
#46118 = STYLED_ITEM ( 'NONE', ( #26657 ), #21041 ) ;
#46119 = VECTOR ( 'NONE', #42974, 1000.000000000000000 ) ;
#46120 = CIRCLE ( 'NONE', #31506, 0.5000000000000004441 ) ;
#46121 = CARTESIAN_POINT ( 'NONE',  ( -5.598654528085806881, 142.7449999999999761, -7.705886871421374629 ) ) ;
#46122 = CARTESIAN_POINT ( 'NONE',  ( 7.999999999999992895, 5.000000000000000000, -24.00402776293826079 ) ) ;
#46123 = ORIENTED_EDGE ( 'NONE', *, *, #19914, .T. ) ;
#46124 = DIRECTION ( 'NONE',  ( 0.000000000000000000, 0.000000000000000000, 1.000000000000000000 ) ) ;
#46125 = CARTESIAN_POINT ( 'NONE',  ( 3.094860106618431583, 136.2049999999999557, 9.525000000000000355 ) ) ;
#46126 = CARTESIAN_POINT ( 'NONE',  ( 0.000000000000000000, 109.9999999999999858, -9.525000000000000355 ) ) ;
#46127 = TOROIDAL_SURFACE ( 'NONE', #7871, 17.50000000000000000, 0.5000000000000000000 ) ;
#46128 = DIRECTION ( 'NONE',  ( 0.6363636363636357984, 0.000000000000000000, 0.7713892158398705234 ) ) ;
#46129 = EDGE_LOOP ( 'NONE', ( #42788, #24306, #58365, #31663 ) ) ;
#46130 = CARTESIAN_POINT ( 'NONE',  ( 8.437984349512095861, 119.1929263765338050, 1.550032578732817026E-15 ) ) ;
#46131 = LINE ( 'NONE', #34840, #55907 ) ;
#46132 = UNCERTAINTY_MEASURE_WITH_UNIT (LENGTH_MEASURE( 1.000000000000000082E-05 ), #54284, 'distance_accuracy_value', 'NONE');
#46133 = DIRECTION ( 'NONE',  ( -1.000000000000000000, -0.000000000000000000, -0.000000000000000000 ) ) ;
#46134 = FILL_AREA_STYLE_COLOUR ( '', #8116 ) ;
#46135 = DIRECTION ( 'NONE',  ( 0.000000000000000000, 0.000000000000000000, -1.000000000000000000 ) ) ;
#46136 = ORIENTED_EDGE ( 'NONE', *, *, #56333, .F. ) ;
#46137 = CARTESIAN_POINT ( 'NONE',  ( -8.082903768654762899, 3.463586619550771876E-15, 1.082903768654759125 ) ) ;
#46138 = EDGE_LOOP ( 'NONE', ( #26417, #3410, #45461, #31446 ) ) ;
#46139 = STYLED_ITEM ( 'NONE', ( #52396 ), #15603 ) ;
#46140 = PLANE ( 'NONE',  #6422 ) ;
#46141 = DIRECTION ( 'NONE',  ( -1.000000000000000000, 0.000000000000000000, 0.000000000000000000 ) ) ;
#46142 = CARTESIAN_POINT ( 'NONE',  ( -164.0049999999999955, 6.826472737025116366, 4.959722759717898555 ) ) ;
#46143 = ORIENTED_EDGE ( 'NONE', *, *, #37788, .F. ) ;
#46144 = EDGE_CURVE ( 'NONE', #15724, #49424, #64229, .T. ) ;
#46145 = UNCERTAINTY_MEASURE_WITH_UNIT (LENGTH_MEASURE( 1.000000000000000082E-05 ), #5873, 'distance_accuracy_value', 'NONE');
#46146 = CIRCLE ( 'NONE', #20284, 0.5000000000000004441 ) ;
#46147 = AXIS2_PLACEMENT_3D ( 'NONE', #1712, #60837, #983 ) ;
#46148 = DIRECTION ( 'NONE',  ( 1.000000000000000000, 0.000000000000000000, 0.000000000000000000 ) ) ;
#46149 = CARTESIAN_POINT ( 'NONE',  ( -4.716976649647097730, 151.3570736234661638, -6.492361379858953896 ) ) ;
#46150 = DIRECTION ( 'NONE',  ( -0.000000000000000000, -1.000000000000000000, 0.000000000000000000 ) ) ;
#46151 = ORIENTED_EDGE ( 'NONE', *, *, #14663, .F. ) ;
#46152 = AXIS2_PLACEMENT_3D ( 'NONE', #31940, #37624, #54082 ) ;
#46153 = DIRECTION ( 'NONE',  ( -1.000000000000000000, 0.000000000000000000, 0.000000000000000000 ) ) ;
#46154 = ORIENTED_EDGE ( 'NONE', *, *, #11200, .F. ) ;
#46155 = CYLINDRICAL_SURFACE ( 'NONE', #38477, 1.000000000000000888 ) ;
#46156 = CARTESIAN_POINT ( 'NONE',  ( -78.50499999999996703, -6.826472737025115478, -4.959722759717899443 ) ) ;
#46157 = ORIENTED_EDGE ( 'NONE', *, *, #24338, .T. ) ;
#46158 = CARTESIAN_POINT ( 'NONE',  ( -9.250000000000003553, 27.74999999999998934, 3.750000000000000000 ) ) ;
#46159 = AXIS2_PLACEMENT_3D ( 'NONE', #62911, #67876, #14754 ) ;
#46160 = SURFACE_SIDE_STYLE ('',( #14451 ) ) ;
#46161 = CARTESIAN_POINT ( 'NONE',  ( -150.3570736234661638, 5.598654528085804216, 7.705886871421366635 ) ) ;
#46162 = VECTOR ( 'NONE', #29556, 1000.000000000000227 ) ;
#46163 =( GEOMETRIC_REPRESENTATION_CONTEXT ( 3 ) GLOBAL_UNCERTAINTY_ASSIGNED_CONTEXT ( ( #2448 ) ) GLOBAL_UNIT_ASSIGNED_CONTEXT ( ( #57735, #35233, #66908 ) ) REPRESENTATION_CONTEXT ( 'NONE', 'WORKASPACE' ) );
#46164 = CARTESIAN_POINT ( 'NONE',  ( -74.08599351457367277, 9.424643574460649376, -6.049632038801590284 ) ) ;
#46165 = DIRECTION ( 'NONE',  ( -0.000000000000000000, -0.000000000000000000, 1.000000000000000000 ) ) ;
#46166 = ORIENTED_EDGE ( 'NONE', *, *, #63915, .T. ) ;
#46167 = CARTESIAN_POINT ( 'NONE',  ( 22.49457430327976581, 26.84935569382991716, -27.39837423296133778 ) ) ;
#46168 = DIRECTION ( 'NONE',  ( -1.000000000000000000, 0.000000000000000000, 0.000000000000000000 ) ) ;
#46169 = CARTESIAN_POINT ( 'NONE',  ( 5.598654528085805993, 141.2449999999999761, 7.705886871421374629 ) ) ;
#46170 = CARTESIAN_POINT ( 'NONE',  ( -94.19499999999999318, 8.437984349512085203, -1.550032578732815448E-15 ) ) ;
#46171 = EDGE_CURVE ( 'NONE', #34584, #51653, #37387, .T. ) ;
#46172 = AXIS2_PLACEMENT_3D ( 'NONE', #67982, #40206, #61611 ) ;
#46173 = CARTESIAN_POINT ( 'NONE',  ( 57.00000000000000000, 0.9999999999999991118, 60.00402776293827145 ) ) ;
#46174 = PRESENTATION_LAYER_ASSIGNMENT (  '', '', ( #59628 ) ) ;
#46175 = UNCERTAINTY_MEASURE_WITH_UNIT (LENGTH_MEASURE( 1.000000000000000082E-05 ), #23556, 'distance_accuracy_value', 'NONE');
#46176 = AXIS2_PLACEMENT_3D ( 'NONE', #50913, #1947, #29070 ) ;
#46178 = CARTESIAN_POINT ( 'NONE',  ( -41.40606286463610530, 107.1009606408073580, -3.493716402184703806 ) ) ;
#46177 = CARTESIAN_POINT ( 'NONE',  ( -96.95707362346617231, 9.058813317711329915, -2.943386871421373119 ) ) ;
#46179 = CARTESIAN_POINT ( 'NONE',  ( -142.7929263765337851, -3.094860106618429807, 9.524999999999991473 ) ) ;
#46180 =( NAMED_UNIT ( * ) PLANE_ANGLE_UNIT ( ) SI_UNIT ( $, .RADIAN. ) );
#46181 = LINE ( 'NONE', #12471, #65792 ) ;
#46182 = CARTESIAN_POINT ( 'NONE',  ( -158.0949999999999704, -2.607480562269071545, -8.024999999999991473 ) ) ;
#46183 = CIRCLE ( 'NONE', #58502, 13.99999999999999822 ) ;
#46184 = EDGE_CURVE ( 'NONE', #18963, #9977, #22572, .T. ) ;
#46185 = SURFACE_SIDE_STYLE ('',( #13792 ) ) ;
#46186 = PRESENTATION_LAYER_ASSIGNMENT (  '', '', ( #19164 ) ) ;
#46187 = FILL_AREA_STYLE ('',( #8179 ) ) ;
#46188 = ORIENTED_EDGE ( 'NONE', *, *, #61964, .F. ) ;
#46189 = CARTESIAN_POINT ( 'NONE',  ( -2.607480562269073321, 127.2070736234661723, -8.025000000000000355 ) ) ;
#46190 = ORIENTED_EDGE ( 'NONE', *, *, #60513, .F. ) ;
#46191 = ADVANCED_FACE ( 'NONE', ( #23262 ), #56407, .T. ) ;
#46192 = COLOUR_RGB ( '', 0.66274510, 0.83137255, 0.94901961) ;
#46193 = CYLINDRICAL_SURFACE ( 'NONE', #30743, 0.5000000000000004441 ) ;
#46194 = AXIS2_PLACEMENT_3D ( 'NONE', #4785, #6175, #49126 ) ;
#46195 = ADVANCED_FACE ( 'NONE', ( #32775 ), #38787, .F. ) ;
#46196 = CARTESIAN_POINT ( 'NONE',  ( -44.99999999999999289, 8.340816515359847472, 6.279506003890324983 ) ) ;
#46197 = DIRECTION ( 'NONE',  ( 2.478176394252580648E-16, 0.000000000000000000, 1.000000000000000000 ) ) ;
#46198 = PRESENTATION_LAYER_ASSIGNMENT (  '', '', ( #57366 ) ) ;
#46199 = DIRECTION ( 'NONE',  ( -1.000000000000000000, 0.000000000000000000, 0.000000000000000000 ) ) ;
#46200 = ADVANCED_FACE ( 'NONE', ( #50015 ), #5673, .F. ) ;
#46201 = ORIENTED_EDGE ( 'NONE', *, *, #169, .F. ) ;
#46202 = CARTESIAN_POINT ( 'NONE',  ( -156.9549999999999841, -7.632228543268599452, 2.479861379858951054 ) ) ;
#46203 = VERTEX_POINT ( 'NONE', #49313 ) ;
#46204 = CARTESIAN_POINT ( 'NONE',  ( -46.25707362346617657, 5.598654528085800663, -7.705886871421367523 ) ) ;
#46205 = LINE ( 'NONE', #35969, #3922 ) ;
#46206 = ORIENTED_EDGE ( 'NONE', *, *, #24435, .F. ) ;
#46207 = CARTESIAN_POINT ( 'NONE',  ( -58.10707362346617799, 8.102448949553172852, -5.886773742842744461 ) ) ;
#46208 = CARTESIAN_POINT ( 'NONE',  ( -2.607480562269075097, 158.4070736234661751, 8.025000000000000355 ) ) ;
#46209 = ORIENTED_EDGE ( 'NONE', *, *, #35648, .F. ) ;
#46210 = MECHANICAL_DESIGN_GEOMETRIC_PRESENTATION_REPRESENTATION (  '', ( #42859 ), #60753 ) ;
#46211 = CARTESIAN_POINT ( 'NONE',  ( -10.11618306975752368, 54.14354156754873060, 6.790106699912857202 ) ) ;
#46212 = CARTESIAN_POINT ( 'NONE',  ( -5.598654528085808657, 111.7549999999999955, 7.705886871421373741 ) ) ;
#46213 = MECHANICAL_DESIGN_GEOMETRIC_PRESENTATION_REPRESENTATION (  '', ( #14701 ), #43949 ) ;
#46214 = CARTESIAN_POINT ( 'NONE',  ( -71.30499999999997840, 8.437984349512086979, -1.550032578732815448E-15 ) ) ;
#46215 = ORIENTED_EDGE ( 'NONE', *, *, #53670, .T. ) ;
#46216 = CARTESIAN_POINT ( 'NONE',  ( -3.094860106618432471, 134.7050000000000125, -9.525000000000000355 ) ) ;
#46217 = UNCERTAINTY_MEASURE_WITH_UNIT (LENGTH_MEASURE( 1.000000000000000082E-05 ), #8837, 'distance_accuracy_value', 'NONE');
#46218 = PRESENTATION_STYLE_ASSIGNMENT (( #61996 ) ) ;
#46219 = DIRECTION ( 'NONE',  ( 0.000000000000000000, -1.000000000000000000, 0.000000000000000000 ) ) ;
#46220 = AXIS2_PLACEMENT_3D ( 'NONE', #51339, #62226, #56249 ) ;
#46221 = CARTESIAN_POINT ( 'NONE',  ( -41.49999999999998579, 106.9282032302754999, 3.500000000000000000 ) ) ;
#46222 = AXIS2_PLACEMENT_3D ( 'NONE', #51011, #18313, #2773 ) ;
#46223 = CARTESIAN_POINT ( 'NONE',  ( 0.000000000000000000, 0.000000000000000000, 3.000000000000000000 ) ) ;
#46224 = EDGE_LOOP ( 'NONE', ( #27972, #18218, #41806, #37657 ) ) ;
#46225 = CARTESIAN_POINT ( 'NONE',  ( -184.0000000000000000, 0.000000000000000000, 0.000000000000000000 ) ) ;
#46226 = FILL_AREA_STYLE_COLOUR ( '', #3652 ) ;
#46227 = CARTESIAN_POINT ( 'NONE',  ( -56.69499999999998607, -8.437984349512085203, 5.166775262442717831E-16 ) ) ;
#46229 = ORIENTED_EDGE ( 'NONE', *, *, #6581, .F. ) ;
#46228 = MECHANICAL_DESIGN_GEOMETRIC_PRESENTATION_REPRESENTATION (  '', ( #5740 ), #50716 ) ;
#46230 = DIRECTION ( 'NONE',  ( -1.387778780781444413E-14, -1.000000000000000000, 0.000000000000000000 ) ) ;
#46231 = COLOUR_RGB ( '', 0.72549020, 0.75294118, 0.79215686) ;
#46232 = CARTESIAN_POINT ( 'NONE',  ( 7.766025168014159874, 1.733974831985843013, -0.5488498361408489234 ) ) ;
#46233 = LINE ( 'NONE', #7849, #39812 ) ;
#46234 = ORIENTED_EDGE ( 'NONE', *, *, #3774, .T. ) ;
#46235 = FACE_OUTER_BOUND ( 'NONE', #30060, .T. ) ;
#46236 = STYLED_ITEM ( 'NONE', ( #39882 ), #52528 ) ;
#46237 = VERTEX_POINT ( 'NONE', #1025 ) ;
#46238 = CARTESIAN_POINT ( 'NONE',  ( 0.000000000000000000, 0.000000000000000000, 0.7500000000000000000 ) ) ;
#46239 = CARTESIAN_POINT ( 'NONE',  ( -106.7049999999999983, 2.607480562269073321, 8.024999999999991473 ) ) ;
#46240 = EDGE_LOOP ( 'NONE', ( #22746, #42766, #42242, #47920 ) ) ;
#46241 = CARTESIAN_POINT ( 'NONE',  ( -6.826472737025120807, 118.5070736234661553, -4.959722759717907437 ) ) ;
#46242 = CARTESIAN_POINT ( 'NONE',  ( 30.75000000000001066, 15.74999999999997513, 3.750000000000000000 ) ) ;
#46243 = CARTESIAN_POINT ( 'NONE',  ( -142.4070736234661751, 3.094860106618428031, -9.524999999999993250 ) ) ;
#46244 = CARTESIAN_POINT ( 'NONE',  ( 21.25000000000001066, 24.74999999999998224, -4.000000000000000000 ) ) ;
#46245 = CARTESIAN_POINT ( 'NONE',  ( -1.166476076187854022E-15, 140.9449999999999932, 9.525000000000000355 ) ) ;
#46246 = CARTESIAN_POINT ( 'NONE',  ( -70.55707362346616662, -1.166476076187852838E-15, -9.524999999999991473 ) ) ;
#46247 = FACE_OUTER_BOUND ( 'NONE', #46913, .T. ) ;
#46248 =( NAMED_UNIT ( * ) SI_UNIT ( $, .STERADIAN. ) SOLID_ANGLE_UNIT ( ) );
#46249 = STYLED_ITEM ( 'NONE', ( #33505 ), #41398 ) ;
#46250 = PRESENTATION_LAYER_ASSIGNMENT (  '', '', ( #51854 ) ) ;
#46252 = CARTESIAN_POINT ( 'NONE',  ( -100.7929263765348509, -3.094860106600816341, 9.525000000012788348 ) ) ;
#46251 = FILL_AREA_STYLE_COLOUR ( '', #54862 ) ;
#46253 = CARTESIAN_POINT ( 'NONE',  ( -116.9050000000000011, 2.607480562269068880, -8.024999999999993250 ) ) ;
#46254 = CARTESIAN_POINT ( 'NONE',  ( 15.98999599679679839, 147.4999999999999716, 10.00000000000000000 ) ) ;
#46255 = CARTESIAN_POINT ( 'NONE',  ( -122.9950000000000045, -6.826472737025115478, 4.959722759717900331 ) ) ;
#46256 = ADVANCED_FACE ( 'NONE', ( #40504 ), #62275, .F. ) ;
#46257 = CARTESIAN_POINT ( 'NONE',  ( -116.3949999999999818, -6.826472737025113702, -4.959722759717900331 ) ) ;
#46258 = VECTOR ( 'NONE', #40553, 1000.000000000000000 ) ;
#46259 =( NAMED_UNIT ( * ) PLANE_ANGLE_UNIT ( ) SI_UNIT ( $, .RADIAN. ) );
#46260 = ORIENTED_EDGE ( 'NONE', *, *, #42993, .F. ) ;
#46261 = EDGE_CURVE ( 'NONE', #45002, #65761, #40857, .T. ) ;
#46262 = SURFACE_STYLE_USAGE ( .BOTH. , #19832 ) ;
#46264 = ADVANCED_FACE ( 'NONE', ( #24616 ), #67718, .T. ) ;
#46263 = FACE_OUTER_BOUND ( 'NONE', #11229, .T. ) ;
#46265 =( GEOMETRIC_REPRESENTATION_CONTEXT ( 3 ) GLOBAL_UNCERTAINTY_ASSIGNED_CONTEXT ( ( #62811 ) ) GLOBAL_UNIT_ASSIGNED_CONTEXT ( ( #51900, #35719, #62765 ) ) REPRESENTATION_CONTEXT ( 'NONE', 'WORKASPACE' ) );
#46266 = VECTOR ( 'NONE', #33332, 1000.000000000000000 ) ;
#46267 = CARTESIAN_POINT ( 'NONE',  ( -172.9429263765337907, 0.000000000000000000, 9.524999999999991473 ) ) ;
#46268 =( NAMED_UNIT ( * ) SI_UNIT ( $, .STERADIAN. ) SOLID_ANGLE_UNIT ( ) );
#46269 = CARTESIAN_POINT ( 'NONE',  ( -52.49499999999999034, 6.826472737025113702, -4.959722759717902107 ) ) ;
#46270 = EDGE_CURVE ( 'NONE', #60715, #11384, #24288, .T. ) ;
#46271 = AXIS2_PLACEMENT_3D ( 'NONE', #48499, #5511, #32601 ) ;
#46272 = EDGE_CURVE ( 'NONE', #59022, #47549, #13381, .T. ) ;
#46273 = DIRECTION ( 'NONE',  ( -0.000000000000000000, -0.000000000000000000, 1.000000000000000000 ) ) ;
#46274 = TOROIDAL_SURFACE ( 'NONE', #55206, 1.000000000000000000, 0.5000000000000000000 ) ;
#46275 = ADVANCED_FACE ( 'NONE', ( #24985, #51377 ), #56999, .F. ) ;
#46276 = DIRECTION ( 'NONE',  ( -1.000000000000000000, 0.000000000000000000, 0.000000000000000000 ) ) ;
#46277 = CYLINDRICAL_SURFACE ( 'NONE', #12530, 0.2500000000000002220 ) ;
#46278 = EDGE_LOOP ( 'NONE', ( #59298, #60956, #37435, #67590 ) ) ;
#46279 = EDGE_CURVE ( 'NONE', #56560, #60715, #52782, .T. ) ;
#46280 = CARTESIAN_POINT ( 'NONE',  ( -88.94292637653380496, 0.000000000000000000, 9.524999999999991473 ) ) ;
#46281 = SHAPE_DEFINITION_REPRESENTATION ( #36716, #6947 ) ;
#46282 = COLOUR_RGB ( '', 0.40784314, 0.44705882, 0.49803922) ;
#46283 = EDGE_CURVE ( 'NONE', #39066, #44845, #16029, .T. ) ;
#46284 = COLOUR_RGB ( '', 0.72549020, 0.75294118, 0.79215686) ;
#46285 = DIRECTION ( 'NONE',  ( -0.000000000000000000, -0.000000000000000000, -1.000000000000000000 ) ) ;
#46286 = CIRCLE ( 'NONE', #22702, 4.999999999999999112 ) ;
#46287 = VERTEX_POINT ( 'NONE', #9532 ) ;
#46288 = VECTOR ( 'NONE', #51061, 1000.000000000000000 ) ;
#46289 = CARTESIAN_POINT ( 'NONE',  ( 92.41620014002536720, 5.000000000000000000, -29.00402776293825724 ) ) ;
#46290 = DIRECTION ( 'NONE',  ( -1.000000000000000000, -0.000000000000000000, -4.516179008354028246E-16 ) ) ;
#46291 = ORIENTED_EDGE ( 'NONE', *, *, #7085, .F. ) ;
#46292 = FACE_OUTER_BOUND ( 'NONE', #11312, .T. ) ;
#46293 = SURFACE_STYLE_USAGE ( .BOTH. , #68074 ) ;
#46294 = CARTESIAN_POINT ( 'NONE',  ( 6.826472737025119919, 135.0070736234661126, 4.959722759717908325 ) ) ;
#46295 = VECTOR ( 'NONE', #62871, 1000.000000000000000 ) ;
#46296 = ORIENTED_EDGE ( 'NONE', *, *, #69358, .T. ) ;
#46297 = CARTESIAN_POINT ( 'NONE',  ( -102.9549999999999841, -7.632228543268599452, 2.479861379858951054 ) ) ;
#46298 = DIRECTION ( 'NONE',  ( -1.000000000000000000, 0.000000000000000000, 0.000000000000000000 ) ) ;
#46299 =( NAMED_UNIT ( * ) PLANE_ANGLE_UNIT ( ) SI_UNIT ( $, .RADIAN. ) );
#46300 = ORIENTED_EDGE ( 'NONE', *, *, #63113, .F. ) ;
#46301 = CARTESIAN_POINT ( 'NONE',  ( 5.249999999999991118, 6.429395695523593306E-16, 0.000000000000000000 ) ) ;
#46302 = DIRECTION ( 'NONE',  ( -1.000000000000000000, -0.000000000000000000, 0.000000000000000000 ) ) ;
#46303 = FACE_OUTER_BOUND ( 'NONE', #26953, .T. ) ;
#46304 = MECHANICAL_DESIGN_GEOMETRIC_PRESENTATION_REPRESENTATION (  '', ( #61970 ), #39575 ) ;
#46305 = SURFACE_STYLE_USAGE ( .BOTH. , #40309 ) ;
#46306 = CARTESIAN_POINT ( 'NONE',  ( -79.79500000000000171, 2.607480562269068880, -8.024999999999993250 ) ) ;
#46307 = VERTEX_POINT ( 'NONE', #20040 ) ;
#46308 = ADVANCED_FACE ( 'NONE', ( #63319 ), #68958, .F. ) ;
#46309 = STYLED_ITEM ( 'NONE', ( #67207 ), #46264 ) ;
#46310 = CARTESIAN_POINT ( 'NONE',  ( -13.25000000000000355, 27.74999999999998934, 4.000000000000000000 ) ) ;
#46311 = AXIS2_PLACEMENT_3D ( 'NONE', #59438, #9663, #57116 ) ;
#46312 = VERTEX_POINT ( 'NONE', #15845 ) ;
#46313 = DIRECTION ( 'NONE',  ( 1.000000000000000000, 0.000000000000000000, 0.000000000000000000 ) ) ;
#46314 =( LENGTH_UNIT ( ) NAMED_UNIT ( * ) SI_UNIT ( .MILLI., .METRE. ) );
#46315 = AXIS2_PLACEMENT_3D ( 'NONE', #49476, #49143, #11124 ) ;
#46316 = AXIS2_PLACEMENT_3D ( 'NONE', #61265, #16994, #2101 ) ;
#46317 = SPHERICAL_SURFACE ( 'NONE', #6688, 0.5000000000000000000 ) ;
#46318 =( LENGTH_UNIT ( ) NAMED_UNIT ( * ) SI_UNIT ( .MILLI., .METRE. ) );
#46319 = VERTEX_POINT ( 'NONE', #68606 ) ;
#46320 = COLOUR_RGB ( '', 0.09019608, 0.27058824, 0.51372549) ;
#46321 = CARTESIAN_POINT ( 'NONE',  ( -97.55707362346618083, -1.166476076187852838E-15, -9.524999999999991473 ) ) ;
#46322 = ORIENTED_EDGE ( 'NONE', *, *, #53258, .F. ) ;
#46323 = CARTESIAN_POINT ( 'NONE',  ( -11.74999999999999645, -0.9999999999999995559, 20.00000000000000000 ) ) ;
#46324 = CARTESIAN_POINT ( 'NONE',  ( 21.25000000000001066, 24.74999999999998224, 3.750000000000000000 ) ) ;
#46325 = CARTESIAN_POINT ( 'NONE',  ( -166.4070736234662036, 3.094860106618428031, -9.524999999999993250 ) ) ;
#46326 = CIRCLE ( 'NONE', #59792, 0.5000000000000004441 ) ;
#46327 = DIRECTION ( 'NONE',  ( -1.000000000000000000, 0.000000000000000000, 0.000000000000000000 ) ) ;
#46328 = CARTESIAN_POINT ( 'NONE',  ( 5.598654528085805993, 117.2449999999999903, 7.705886871421374629 ) ) ;
#46329 = CARTESIAN_POINT ( 'NONE',  ( -105.5070736234661695, 8.102448949553176405, 5.886773742842740909 ) ) ;
#46330 = AXIS2_PLACEMENT_3D ( 'NONE', #4184, #42266, #52440 ) ;
#46331 =( NAMED_UNIT ( * ) SI_UNIT ( $, .STERADIAN. ) SOLID_ANGLE_UNIT ( ) );
#46332 = FILL_AREA_STYLE_COLOUR ( '', #39237 ) ;
#46333 = ORIENTED_EDGE ( 'NONE', *, *, #29035, .F. ) ;
#46334 = CARTESIAN_POINT ( 'NONE',  ( -82.49292637653378790, -8.102448949553174629, 5.886773742842742685 ) ) ;
#46335 = CARTESIAN_POINT ( 'NONE',  ( -4.041451884327381450, -7.000000000000002665, 7.500000000000000000 ) ) ;
#46336 = VECTOR ( 'NONE', #36564, 1000.000000000000114 ) ;
#46337 = CARTESIAN_POINT ( 'NONE',  ( -147.6549999999999727, -7.632228543268600340, -2.479861379858950166 ) ) ;
#46338 = ADVANCED_FACE ( 'NONE', ( #37327 ), #47186, .T. ) ;
#46339 = FILL_AREA_STYLE_COLOUR ( '', #7197 ) ;
#46340 =( LENGTH_UNIT ( ) NAMED_UNIT ( * ) SI_UNIT ( .MILLI., .METRE. ) );
#46341 = PRESENTATION_LAYER_ASSIGNMENT (  '', '', ( #49687 ) ) ;
#46342 = CARTESIAN_POINT ( 'NONE',  ( -169.1949999999999932, 8.437984349512085203, -1.550032578732815448E-15 ) ) ;
#46343 = CARTESIAN_POINT ( 'NONE',  ( -144.2950000000000159, -2.607480562269069768, 8.024999999999991473 ) ) ;
#46344 =( BOUNDED_CURVE ( )  B_SPLINE_CURVE ( 2, ( #32326, #11566, #64347, #63991, #48209, #53117, #58728, #48911, #54124, #68949, #33037 ),
 .UNSPECIFIED., .F., .F. ) 
 B_SPLINE_CURVE_WITH_KNOTS ( ( 3, 2, 2, 2, 2, 3 ),
 ( 0.3913043478260775365, 0.3934782608695557293, 0.3956521739130339221, 0.3978260869565121705, 0.3999999999999904188, 0.4021739130434686116 ),
 .UNSPECIFIED. ) 
 CURVE ( )  GEOMETRIC_REPRESENTATION_ITEM ( )  RATIONAL_B_SPLINE_CURVE ( ( 1.000000000000212497, 0.9510565162949410345, 1.000000000000000000, 0.9510565162951535312, 1.000000000000000000, 0.9510565162951535312, 1.000000000000000000, 0.9510565162951535312, 1.000000000000000000, 0.9510565162953710239, 0.9999999999997825073 ) ) 
 REPRESENTATION_ITEM ( '' )  );
#46345 = ORIENTED_EDGE ( 'NONE', *, *, #37357, .T. ) ;
#46346 = EDGE_CURVE ( 'NONE', #5288, #11604, #43007, .T. ) ;
#46347 = CARTESIAN_POINT ( 'NONE',  ( 4.750000000000002665, 24.74999999999998579, 4.000000000000000000 ) ) ;
#46348 = PRESENTATION_LAYER_ASSIGNMENT (  '', '', ( #45237 ) ) ;
#46349 = CARTESIAN_POINT ( 'NONE',  ( -195.0000000000000000, 0.000000000000000000, 0.000000000000000000 ) ) ;
#46350 = CARTESIAN_POINT ( 'NONE',  ( -63.50499999999998124, -6.826472737025115478, -4.959722759717899443 ) ) ;
#46351 = DIRECTION ( 'NONE',  ( 0.000000000000000000, 0.000000000000000000, -1.000000000000000000 ) ) ;
#46352 =( GEOMETRIC_REPRESENTATION_CONTEXT ( 3 ) GLOBAL_UNCERTAINTY_ASSIGNED_CONTEXT ( ( #5398 ) ) GLOBAL_UNIT_ASSIGNED_CONTEXT ( ( #27204, #64535, #17060 ) ) REPRESENTATION_CONTEXT ( 'NONE', 'WORKASPACE' ) );
#46353 = CARTESIAN_POINT ( 'NONE',  ( -154.5570736234661808, -1.166476076187852838E-15, -9.524999999999991473 ) ) ;
#46354 = CARTESIAN_POINT ( 'NONE',  ( -65.69499999999999318, -8.437984349512086979, 5.166775262442717831E-16 ) ) ;
#46355 = CARTESIAN_POINT ( 'NONE',  ( -3.094860106618432471, 158.7049999999999557, -9.525000000000000355 ) ) ;
#46356 = CYLINDRICAL_SURFACE ( 'NONE', #11789, 4.999999999999997335 ) ;
#46357 = EDGE_CURVE ( 'NONE', #3932, #12107, #5248, .T. ) ;
#46358 = CARTESIAN_POINT ( 'NONE',  ( 57.00000000000000000, 16.00000000000000000, -60.00402776293825724 ) ) ;
#46359 = DIRECTION ( 'NONE',  ( -8.041998848429303274E-17, 1.110223024625156540E-16, -1.000000000000000222 ) ) ;
#46360 = LINE ( 'NONE', #9039, #2238 ) ;
#46361 = VECTOR ( 'NONE', #2435, 1000.000000000000000 ) ;
#46362 = EDGE_CURVE ( 'NONE', #50231, #65411, #48215, .T. ) ;
#46363 = DIRECTION ( 'NONE',  ( 0.000000000000000000, 1.000000000000000000, 0.000000000000000000 ) ) ;
#46364 = AXIS2_PLACEMENT_3D ( 'NONE', #24790, #47007, #57879 ) ;
#46365 = SURFACE_STYLE_FILL_AREA ( #51598 ) ;
#46366 = DIRECTION ( 'NONE',  ( 0.000000000000000000, 0.000000000000000000, 1.000000000000000000 ) ) ;
#46367 = CARTESIAN_POINT ( 'NONE',  ( -1.585182400056157181, -2.380245935246553035, -9.000000000000005329 ) ) ;
#46368 = ORIENTED_EDGE ( 'NONE', *, *, #8749, .F. ) ;
#46369 = VERTEX_POINT ( 'NONE', #68259 ) ;
#46370 = DIRECTION ( 'NONE',  ( 1.000000000000000000, 0.000000000000000000, 0.000000000000000000 ) ) ;
#46371 = COLOUR_RGB ( '', 0.72549020, 0.75294118, 0.79215686) ;
#46372 = FACE_OUTER_BOUND ( 'NONE', #28530, .T. ) ;
#46373 = COLOUR_RGB ( '', 0.66274510, 0.83137255, 0.94901961) ;
#46374 =( GEOMETRIC_REPRESENTATION_CONTEXT ( 3 ) GLOBAL_UNCERTAINTY_ASSIGNED_CONTEXT ( ( #10984 ) ) GLOBAL_UNIT_ASSIGNED_CONTEXT ( ( #41811, #57244, #3386 ) ) REPRESENTATION_CONTEXT ( 'NONE', 'WORKASPACE' ) );
#46375 =( NAMED_UNIT ( * ) PLANE_ANGLE_UNIT ( ) SI_UNIT ( $, .RADIAN. ) );
#46376 = CARTESIAN_POINT ( 'NONE',  ( -74.99999999999998579, 50.00000000000000000, -7.000000000000000000 ) ) ;
#46377 = ORIENTED_EDGE ( 'NONE', *, *, #14870, .T. ) ;
#46378 = ORIENTED_EDGE ( 'NONE', *, *, #45130, .T. ) ;
#46379 = DIRECTION ( 'NONE',  ( 0.7071067811865345831, 8.659560562354775086E-17, -0.7071067811865603403 ) ) ;
#46380 =( NAMED_UNIT ( * ) PLANE_ANGLE_UNIT ( ) SI_UNIT ( $, .RADIAN. ) );
#46381 = CIRCLE ( 'NONE', #9260, 5.499999999999976907 ) ;
#46382 = ORIENTED_EDGE ( 'NONE', *, *, #11112, .F. ) ;
#46383 = CARTESIAN_POINT ( 'NONE',  ( 10.01517768586949231, 112.8049999999999784, 1.839758294383810543E-15 ) ) ;
#46384 = DIRECTION ( 'NONE',  ( 1.000000000000000000, 0.000000000000000000, 0.000000000000000000 ) ) ;
#46385 = ORIENTED_EDGE ( 'NONE', *, *, #61687, .T. ) ;
#46386 = CARTESIAN_POINT ( 'NONE',  ( -107.5449999999999875, -7.632228543268600340, -2.479861379858950166 ) ) ;
#46387 = ORIENTED_EDGE ( 'NONE', *, *, #12073, .T. ) ;
#46388 = EDGE_CURVE ( 'NONE', #7642, #40384, #65879, .T. ) ;
#46389 = MECHANICAL_DESIGN_GEOMETRIC_PRESENTATION_REPRESENTATION (  '', ( #36310 ), #17161 ) ;
#46390 = LINE ( 'NONE', #35098, #16468 ) ;
#46391 = FILL_AREA_STYLE ('',( #51991 ) ) ;
#46392 = VECTOR ( 'NONE', #27277, 1000.000000000000000 ) ;
#46393 = CARTESIAN_POINT ( 'NONE',  ( -179.6070736234661638, -8.102448949553174629, 5.886773742842742685 ) ) ;
#46394 = ORIENTED_EDGE ( 'NONE', *, *, #58016, .F. ) ;
#46395 = CARTESIAN_POINT ( 'NONE',  ( 2.607480562269076430, 149.7929263765338135, -8.025000000000000355 ) ) ;
#46396 = FACE_OUTER_BOUND ( 'NONE', #27151, .T. ) ;
#46397 = CARTESIAN_POINT ( 'NONE',  ( -11.74999999999999645, -3.000000000000000000, 19.00000000000000000 ) ) ;
#46398 = MECHANICAL_DESIGN_GEOMETRIC_PRESENTATION_REPRESENTATION (  '', ( #39654 ), #27246 ) ;
#46399 = CARTESIAN_POINT ( 'NONE',  ( 7.794228634059945371, 2.500000000000000000, 4.500000000000000888 ) ) ;
#46400 = DIRECTION ( 'NONE',  ( 0.000000000000000000, 0.000000000000000000, 1.000000000000000000 ) ) ;
#46401 = VERTEX_POINT ( 'NONE', #929 ) ;
#46402 = EDGE_LOOP ( 'NONE', ( #50609, #38515, #9680, #17997 ) ) ;
#46403 = LINE ( 'NONE', #67827, #7986 ) ;
#46404 = FACE_OUTER_BOUND ( 'NONE', #6186, .T. ) ;
#46405 = AXIS2_PLACEMENT_3D ( 'NONE', #39740, #14017, #3048 ) ;
#46407 = CARTESIAN_POINT ( 'NONE',  ( -122.9049999999999727, 2.607480562269068880, -8.024999999999993250 ) ) ;
#46406 = PRESENTATION_LAYER_ASSIGNMENT (  '', '', ( #7048 ) ) ;
#46408 = CARTESIAN_POINT ( 'NONE',  ( -52.00000000000000000, -1.926070501056209087E-14, 11.50000000000000000 ) ) ;
#46409 = CARTESIAN_POINT ( 'NONE',  ( 0.000000000000000000, 27.74999999999998934, 3.750000000000000000 ) ) ;
#46410 = SURFACE_STYLE_FILL_AREA ( #14015 ) ;
#46411 =( GEOMETRIC_REPRESENTATION_CONTEXT ( 3 ) GLOBAL_UNCERTAINTY_ASSIGNED_CONTEXT ( ( #38217 ) ) GLOBAL_UNIT_ASSIGNED_CONTEXT ( ( #8485, #45459, #13742 ) ) REPRESENTATION_CONTEXT ( 'NONE', 'WORKASPACE' ) );
#46412 =( NAMED_UNIT ( * ) SI_UNIT ( $, .STERADIAN. ) SOLID_ANGLE_UNIT ( ) );
#46413 = DIRECTION ( 'NONE',  ( 0.000000000000000000, 1.000000000000000000, 0.000000000000000000 ) ) ;
#46414 = CARTESIAN_POINT ( 'NONE',  ( 24.00000000000000000, 1.000000000000000888, 4.000000000000000000 ) ) ;
#46415 = ORIENTED_EDGE ( 'NONE', *, *, #56725, .F. ) ;
#46416 = STYLED_ITEM ( 'NONE', ( #67646 ), #23814 ) ;
#46417 = ORIENTED_EDGE ( 'NONE', *, *, #11517, .F. ) ;
#46418 = CARTESIAN_POINT ( 'NONE',  ( -109.9429263765338050, 0.000000000000000000, 9.524999999999991473 ) ) ;
#46419 = LINE ( 'NONE', #13668, #40195 ) ;
#46420 = EDGE_CURVE ( 'NONE', #4040, #13709, #32868, .T. ) ;
#46421 = CARTESIAN_POINT ( 'NONE',  ( -71.49999999999998579, 119.9999999999997868, 7.500000000000000000 ) ) ;
#46422 = ORIENTED_EDGE ( 'NONE', *, *, #25841, .T. ) ;
#46423 = DIRECTION ( 'NONE',  ( 1.000000000000000000, 0.000000000000000000, 0.000000000000000000 ) ) ;
#46424 = CARTESIAN_POINT ( 'NONE',  ( -179.4550000000000125, 7.632228543268599452, -2.479861379858951942 ) ) ;
#46425 = EDGE_CURVE ( 'NONE', #2160, #68013, #66560, .T. ) ;
#46426 = CARTESIAN_POINT ( 'NONE',  ( -10.39230484541326938, 1.107695154586735509, -1.661048719744147042E-15 ) ) ;
#46427 = PRESENTATION_LAYER_ASSIGNMENT (  '', '', ( #55365 ) ) ;
#46428 = DIRECTION ( 'NONE',  ( -0.000000000000000000, -0.000000000000000000, -1.000000000000000000 ) ) ;
#46429 = CARTESIAN_POINT ( 'NONE',  ( -56.45707362346616520, -9.058813317711329915, 2.943386871421371787 ) ) ;
#46430 = AXIS2_PLACEMENT_3D ( 'NONE', #9620, #36724, #48305 ) ;
#46431 = CARTESIAN_POINT ( 'NONE',  ( -172.1949999999999648, 8.437984349512086979, -1.550032578732815448E-15 ) ) ;
#46432 = ORIENTED_EDGE ( 'NONE', *, *, #64319, .T. ) ;
#46433 = AXIS2_PLACEMENT_3D ( 'NONE', #65480, #18346, #39827 ) ;
#46434 = DIRECTION ( 'NONE',  ( 1.000000000000000000, -0.000000000000000000, -0.000000000000000000 ) ) ;
#46435 = EDGE_CURVE ( 'NONE', #19491, #4798, #12247, .T. ) ;
#46436 = SURFACE_SIDE_STYLE ('',( #56944 ) ) ;
#46437 = CARTESIAN_POINT ( 'NONE',  ( -93.05499999999997840, -9.827790563157499189E-16, -8.024999999999991473 ) ) ;
#46438 = PRESENTATION_STYLE_ASSIGNMENT (( #62899 ) ) ;
#46439 = EDGE_CURVE ( 'NONE', #44000, #33694, #1775, .T. ) ;
#46440 = STYLED_ITEM ( 'NONE', ( #23768 ), #7097 ) ;
#46441 = AXIS2_PLACEMENT_3D ( 'NONE', #39493, #45811, #18707 ) ;
#46442 = CARTESIAN_POINT ( 'NONE',  ( -87.89499999999996760, 6.826472737025115478, 4.959722759717899443 ) ) ;
#46443 = CARTESIAN_POINT ( 'NONE',  ( -5.598654528085808657, 123.7549999999999955, 7.705886871421373741 ) ) ;
#46444 = CARTESIAN_POINT ( 'NONE',  ( -65.39499999999998181, -6.826472737025115478, -4.959722759717899443 ) ) ;
#46445 = DIRECTION ( 'NONE',  ( 0.000000000000000000, 0.000000000000000000, -1.000000000000000000 ) ) ;
#46446 = EDGE_CURVE ( 'NONE', #61370, #65704, #59317, .T. ) ;
#46447 = DIRECTION ( 'NONE',  ( 0.000000000000000000, 0.000000000000000000, -1.000000000000000000 ) ) ;
#46448 = FILL_AREA_STYLE ('',( #61509 ) ) ;
#46449 =( BOUNDED_CURVE ( )  B_SPLINE_CURVE ( 2, ( #68273, #52462, #14816, #31300, #36296, #30965, #3866, #52799, #63332, #4571, #20055 ),
 .UNSPECIFIED., .F., .F. ) 
 B_SPLINE_CURVE_WITH_KNOTS ( ( 3, 2, 2, 2, 2, 3 ),
 ( 0.8260869565217391353, 0.8282608695652173836, 0.8304347826086956319, 0.8326086956521738802, 0.8347826086956521285, 0.8369565217391304879 ),
 .UNSPECIFIED. ) 
 CURVE ( )  GEOMETRIC_REPRESENTATION_ITEM ( )  RATIONAL_B_SPLINE_CURVE ( ( 1.000000000000000000, 0.9510565162951535312, 1.000000000000000000, 0.9510565162951535312, 1.000000000000000000, 0.9510565162951535312, 1.000000000000000000, 0.9510565162951535312, 1.000000000000000000, 0.9510565162951535312, 1.000000000000000000 ) ) 
 REPRESENTATION_ITEM ( '' )  );
#46450 = CIRCLE ( 'NONE', #53153, 0.5000000000000004441 ) ;
#46451 = SURFACE_STYLE_FILL_AREA ( #3435 ) ;
#46452 = ORIENTED_EDGE ( 'NONE', *, *, #2953, .F. ) ;
#46453 = CARTESIAN_POINT ( 'NONE',  ( -118.7929263765338135, -3.094860106618429807, 9.524999999999991473 ) ) ;
#46454 = EDGE_CURVE ( 'NONE', #4175, #4230, #9282, .T. ) ;
#46455 = CARTESIAN_POINT ( 'NONE',  ( -131.3949999999999818, -6.826472737025115478, -4.959722759717899443 ) ) ;
#46457 = DIRECTION ( 'NONE',  ( 0.000000000000000000, 0.000000000000000000, 1.000000000000000000 ) ) ;
#46456 = CARTESIAN_POINT ( 'NONE',  ( 25.75000000000001066, 19.24999999999997868, 3.750000000000000000 ) ) ;
#46458 = PRESENTATION_STYLE_ASSIGNMENT (( #20007 ) ) ;
#46459 = EDGE_LOOP ( 'NONE', ( #45802, #26532, #3834, #25656 ) ) ;
#46461 = ORIENTED_EDGE ( 'NONE', *, *, #1281, .F. ) ;
#46460 = CIRCLE ( 'NONE', #1421, 1.000000000000000888 ) ;
#46462 =( GEOMETRIC_REPRESENTATION_CONTEXT ( 3 ) GLOBAL_UNCERTAINTY_ASSIGNED_CONTEXT ( ( #64304 ) ) GLOBAL_UNIT_ASSIGNED_CONTEXT ( ( #68400, #52590, #67354 ) ) REPRESENTATION_CONTEXT ( 'NONE', 'WORKASPACE' ) );
#46463 = CARTESIAN_POINT ( 'NONE',  ( 22.00000000000001776, 43.00000000000000000, 45.61250543006183022 ) ) ;
#46464 = CARTESIAN_POINT ( 'NONE',  ( -23.21231517720797655, 118.4999999999999716, 7.500000000000000000 ) ) ;
#46465 =( LENGTH_UNIT ( ) NAMED_UNIT ( * ) SI_UNIT ( .MILLI., .METRE. ) );
#46466 = DIRECTION ( 'NONE',  ( 0.000000000000000000, 0.000000000000000000, 1.000000000000000000 ) ) ;
#46467 = DIRECTION ( 'NONE',  ( -1.000000000000000000, 0.000000000000000000, 0.000000000000000000 ) ) ;
#46468 = ORIENTED_EDGE ( 'NONE', *, *, #48042, .T. ) ;
#46469 = CARTESIAN_POINT ( 'NONE',  ( -134.0049999999999955, 6.826472737025115478, 4.959722759717899443 ) ) ;
#46470 = ORIENTED_EDGE ( 'NONE', *, *, #9661, .T. ) ;
#46471 = LINE ( 'NONE', #14778, #66816 ) ;
#46472 = CARTESIAN_POINT ( 'NONE',  ( -119.4570736234661723, -9.058813317711329915, 2.943386871421371787 ) ) ;
#46473 =( GEOMETRIC_REPRESENTATION_CONTEXT ( 3 ) GLOBAL_UNCERTAINTY_ASSIGNED_CONTEXT ( ( #1751 ) ) GLOBAL_UNIT_ASSIGNED_CONTEXT ( ( #36044, #30371, #3629 ) ) REPRESENTATION_CONTEXT ( 'NONE', 'WORKASPACE' ) );
#46474 = EDGE_LOOP ( 'NONE', ( #19863, #30263, #43983, #65244 ) ) ;
#46475 = CARTESIAN_POINT ( 'NONE',  ( 3.851859888774471706E-31, -8.500000000000000000, 24.00000000000000000 ) ) ;
#46476 = LINE ( 'NONE', #3833, #25334 ) ;
#46477 = ORIENTED_EDGE ( 'NONE', *, *, #25169, .F. ) ;
#46478 = AXIS2_PLACEMENT_3D ( 'NONE', #49930, #32339, #42957 ) ;
#46479 = CARTESIAN_POINT ( 'NONE',  ( -79.99999999999998579, 50.00000000000000000, -6.999999999999988454 ) ) ;
#46480 = CARTESIAN_POINT ( 'NONE',  ( -10.01517768586949231, 137.1949999999999363, -6.132527647946036459E-16 ) ) ;
#46481 = PRESENTATION_LAYER_ASSIGNMENT (  '', '', ( #28426 ) ) ;
#46482 = EDGE_CURVE ( 'NONE', #6975, #45132, #29493, .T. ) ;
#46483 = EDGE_LOOP ( 'NONE', ( #38737, #38797, #17494, #20997 ) ) ;
#46484 = DIRECTION ( 'NONE',  ( 0.000000000000000000, 0.000000000000000000, 1.000000000000000000 ) ) ;
#46485 = CARTESIAN_POINT ( 'NONE',  ( -5.598654528085806881, 149.8549999999999898, -7.705886871421374629 ) ) ;
#46486 = DIRECTION ( 'NONE',  ( -0.000000000000000000, -0.000000000000000000, -1.000000000000000000 ) ) ;
#46487 =( NAMED_UNIT ( * ) PLANE_ANGLE_UNIT ( ) SI_UNIT ( $, .RADIAN. ) );
#46488 = MECHANICAL_DESIGN_GEOMETRIC_PRESENTATION_REPRESENTATION (  '', ( #20630 ), #44279 ) ;
#46489 = ORIENTED_EDGE ( 'NONE', *, *, #7233, .T. ) ;
#46490 = CARTESIAN_POINT ( 'NONE',  ( -8.437984349512095861, 120.6929263765338050, -5.166775262442723748E-16 ) ) ;
#46491 = DIRECTION ( 'NONE',  ( 0.000000000000000000, 0.000000000000000000, -1.000000000000000000 ) ) ;
#46492 = CIRCLE ( 'NONE', #48699, 0.5000000000000004441 ) ;
#46493 =( GEOMETRIC_REPRESENTATION_CONTEXT ( 3 ) GLOBAL_UNCERTAINTY_ASSIGNED_CONTEXT ( ( #60949 ) ) GLOBAL_UNIT_ASSIGNED_CONTEXT ( ( #6648, #67146, #28803 ) ) REPRESENTATION_CONTEXT ( 'NONE', 'WORKASPACE' ) );
#46494 = FILL_AREA_STYLE_COLOUR ( '', #19402 ) ;
#46495 = DIRECTION ( 'NONE',  ( 0.6216216216216174928, -0.7833176619561892373, 0.000000000000000000 ) ) ;
#46496 = ORIENTED_EDGE ( 'NONE', *, *, #39961, .F. ) ;
#46497 = DIRECTION ( 'NONE',  ( -0.000000000000000000, -1.000000000000000000, -0.000000000000000000 ) ) ;
#46498 = ORIENTED_EDGE ( 'NONE', *, *, #54775, .T. ) ;
#46499 = CARTESIAN_POINT ( 'NONE',  ( -55.79292637653379217, -3.094860106618429807, 9.524999999999991473 ) ) ;
#46500 = CARTESIAN_POINT ( 'NONE',  ( 36.00000000000002842, 5.000000000000000000, 77.00402776293825013 ) ) ;
#46501 = CARTESIAN_POINT ( 'NONE',  ( 107.0858988931383777, 0.000000000000000000, -16.89933289725613363 ) ) ;
#46502 = CARTESIAN_POINT ( 'NONE',  ( -152.6050000000000182, 6.826472737025113702, -4.959722759717902107 ) ) ;
#46503 = ORIENTED_EDGE ( 'NONE', *, *, #46911, .T. ) ;
#46504 =( NAMED_UNIT ( * ) PLANE_ANGLE_UNIT ( ) SI_UNIT ( $, .RADIAN. ) );
#46505 = MECHANICAL_DESIGN_GEOMETRIC_PRESENTATION_REPRESENTATION (  '', ( #65531 ), #35214 ) ;
#46506 = VECTOR ( 'NONE', #32929, 1000.000000000000000 ) ;
#46507 = ADVANCED_FACE ( 'NONE', ( #55160 ), #59762, .F. ) ;
#46508 = CARTESIAN_POINT ( 'NONE',  ( -54.41715584325135069, -9.238994630453190027, 5.297413886133904626 ) ) ;
#46509 = CARTESIAN_POINT ( 'NONE',  ( 75.00000000000000000, 20.36037961002804053, 5.999999999999999112 ) ) ;
#46510 = DIRECTION ( 'NONE',  ( 1.000000000000000000, 0.000000000000000000, 0.000000000000000000 ) ) ;
#46511 = EDGE_LOOP ( 'NONE', ( #16818, #1883, #5637, #29130 ) ) ;
#46512 =( NAMED_UNIT ( * ) PLANE_ANGLE_UNIT ( ) SI_UNIT ( $, .RADIAN. ) );
#46513 = ADVANCED_FACE ( 'NONE', ( #23182 ), #45703, .T. ) ;
#46514 = ORIENTED_EDGE ( 'NONE', *, *, #58011, .F. ) ;
#46515 = DIRECTION ( 'NONE',  ( 0.000000000000000000, 0.000000000000000000, -1.000000000000000000 ) ) ;
#46516 = ADVANCED_FACE ( 'NONE', ( #56555 ), #18596, .F. ) ;
#46518 = CARTESIAN_POINT ( 'NONE',  ( -68.90499999999997272, 2.607480562269068880, -8.024999999999993250 ) ) ;
#46517 = AXIS2_PLACEMENT_3D ( 'NONE', #18749, #25071, #62359 ) ;
#46519 = EDGE_LOOP ( 'NONE', ( #68607, #55437, #59766, #48186 ) ) ;
#46520 = EDGE_CURVE ( 'NONE', #56343, #19343, #49796, .T. ) ;
#46521 = DIRECTION ( 'NONE',  ( 0.000000000000000000, -1.000000000000000000, 0.000000000000000000 ) ) ;
#46522 = STYLED_ITEM ( 'NONE', ( #40734 ), #48203 ) ;
#46523 = DIRECTION ( 'NONE',  ( 0.000000000000000000, 0.000000000000000000, -1.000000000000000000 ) ) ;
#46524 = DIRECTION ( 'NONE',  ( -1.000000000000000000, 0.000000000000000000, -0.000000000000000000 ) ) ;
#46525 = EDGE_LOOP ( 'NONE', ( #12680, #28237, #66846, #27023 ) ) ;
#46526 = COLOUR_RGB ( '', 0.40784314, 0.44705882, 0.49803922) ;
#46527 = AXIS2_PLACEMENT_3D ( 'NONE', #18047, #12402, #49722 ) ;
#46528 = CARTESIAN_POINT ( 'NONE',  ( -74.21272224914370952, 8.937790484661849888, -6.368793980437817304 ) ) ;
#46529 = DIRECTION ( 'NONE',  ( 1.000000000000000000, 0.000000000000000000, 0.000000000000000000 ) ) ;
#46531 = LINE ( 'NONE', #40537, #46085 ) ;
#46530 = CARTESIAN_POINT ( 'NONE',  ( -74.99999999999998579, 50.00000000000000000, 6.500000000000000000 ) ) ;
#46532 = EDGE_CURVE ( 'NONE', #13679, #42412, #53168, .T. ) ;
#46533 = AXIS2_PLACEMENT_3D ( 'NONE', #62657, #14481, #51792 ) ;
#46534 = CARTESIAN_POINT ( 'NONE',  ( 8.102448949553183510, 147.9949999999999761, -5.886773742842746238 ) ) ;
#46535 = CARTESIAN_POINT ( 'NONE',  ( -94.64499999999999602, 4.716976649647091513, -6.492361379858946790 ) ) ;
#46536 = AXIS2_PLACEMENT_3D ( 'NONE', #54053, #1225, #43565 ) ;
#46537 = CARTESIAN_POINT ( 'NONE',  ( 41.84210526315788314, 107.2928455055531600, -4.000000000000000000 ) ) ;
#46538 = AXIS2_PLACEMENT_3D ( 'NONE', #28334, #28693, #11837 ) ;
#46539 = CARTESIAN_POINT ( 'NONE',  ( -4.716976649647098618, 145.1429263765338078, 6.492361379858953008 ) ) ;
#46540 = VERTEX_POINT ( 'NONE', #7349 ) ;
#46541 = CARTESIAN_POINT ( 'NONE',  ( -148.1929263765337907, -10.01517768586948698, 6.132527647946031529E-16 ) ) ;
#46542 = TOROIDAL_SURFACE ( 'NONE', #21791, 1.000000000000000000, 0.5000000000000000000 ) ;
#46543 =( NAMED_UNIT ( * ) PLANE_ANGLE_UNIT ( ) SI_UNIT ( $, .RADIAN. ) );
#46544 = LINE ( 'NONE', #25035, #29789 ) ;
#46545 = CARTESIAN_POINT ( 'NONE',  ( -161.5449999999999875, -7.632228543268600340, -2.479861379858950166 ) ) ;
#46546 = STYLED_ITEM ( 'NONE', ( #39374 ), #6816 ) ;
#46547 = VECTOR ( 'NONE', #26997, 1000.000000000000000 ) ;
#46548 = EDGE_CURVE ( 'NONE', #26070, #23836, #18312, .T. ) ;
#46549 = CARTESIAN_POINT ( 'NONE',  ( 3.851859888774471706E-31, -8.500000000000000000, 1.000000000000000888 ) ) ;
#46550 = CARTESIAN_POINT ( 'NONE',  ( 0.000000000000000000, 87.30187232391182306, 0.000000000000000000 ) ) ;
#46551 = ORIENTED_EDGE ( 'NONE', *, *, #8191, .T. ) ;
#46552 = DIRECTION ( 'NONE',  ( 0.000000000000000000, 0.000000000000000000, -1.000000000000000000 ) ) ;
#46554 = ORIENTED_EDGE ( 'NONE', *, *, #45609, .F. ) ;
#46553 = AXIS2_PLACEMENT_3D ( 'NONE', #39464, #7073, #45098 ) ;
#46555 = EDGE_CURVE ( 'NONE', #46101, #12948, #67767, .T. ) ;
#46556 = FILL_AREA_STYLE ('',( #40203 ) ) ;
#46557 = CIRCLE ( 'NONE', #40914, 1.000000000000000000 ) ;
#46558 = COLOUR_RGB ( '', 0.40784314, 0.44705882, 0.49803922) ;
#46559 = CARTESIAN_POINT ( 'NONE',  ( -5.196152422706634688, 9.000000000000008882, 7.500000000000000000 ) ) ;
#46560 = FACE_OUTER_BOUND ( 'NONE', #9416, .T. ) ;
#46561 = CARTESIAN_POINT ( 'NONE',  ( -59.62135308701207492, -8.500000000000543565, 0.008598348328329818643 ) ) ;
#46562 = ORIENTED_EDGE ( 'NONE', *, *, #68867, .T. ) ;
#46563 = CARTESIAN_POINT ( 'NONE',  ( -160.1049999999999613, -6.826472737025113702, 4.959722759717902107 ) ) ;
#46564 = CIRCLE ( 'NONE', #11663, 1.000000000000000888 ) ;
#46565 = ORIENTED_EDGE ( 'NONE', *, *, #8979, .T. ) ;
#46566 = FACE_OUTER_BOUND ( 'NONE', #9911, .T. ) ;
#46567 = ORIENTED_EDGE ( 'NONE', *, *, #50534, .T. ) ;
#46568 = VECTOR ( 'NONE', #38943, 1000.000000000000000 ) ;
#46569 = SURFACE_STYLE_FILL_AREA ( #8879 ) ;
#46570 = DIRECTION ( 'NONE',  ( 0.000000000000000000, 0.000000000000000000, 1.000000000000000000 ) ) ;
#46571 = CARTESIAN_POINT ( 'NONE',  ( -6.826472737025120807, 157.5070736234661126, -4.959722759717907437 ) ) ;
#46572 = ORIENTED_EDGE ( 'NONE', *, *, #62638, .T. ) ;
#46573 = CARTESIAN_POINT ( 'NONE',  ( -34.99999999999992895, 112.9999999999999858, 7.000000000000000000 ) ) ;
#46574 = CARTESIAN_POINT ( 'NONE',  ( 10.57623092156539357, 58.31681314173471975, 12.50000000000000000 ) ) ;
#46575 = CARTESIAN_POINT ( 'NONE',  ( -78.05499999999997840, -9.827790563157499189E-16, -8.024999999999991473 ) ) ;
#46576 = SURFACE_STYLE_FILL_AREA ( #63401 ) ;
#46577 = ORIENTED_EDGE ( 'NONE', *, *, #55505, .T. ) ;
#46578 = CARTESIAN_POINT ( 'NONE',  ( -1.166476076187854022E-15, 142.0549999999999784, 9.525000000000000355 ) ) ;
#46579 = CYLINDRICAL_SURFACE ( 'NONE', #69266, 0.2500000000000002220 ) ;
#46580 = CARTESIAN_POINT ( 'NONE',  ( 20.07516809221520404, 115.0406803144924766, 9.999999999999998224 ) ) ;
#46581 = COLOUR_RGB ( '', 0.08235294, 0.09019608, 0.10196078) ;
#46582 = PRESENTATION_STYLE_ASSIGNMENT (( #30677 ) ) ;
#46583 = EDGE_CURVE ( 'NONE', #20391, #31566, #4836, .T. ) ;
#46584 = PRESENTATION_STYLE_ASSIGNMENT (( #41630 ) ) ;
#46585 = ORIENTED_EDGE ( 'NONE', *, *, #25336, .T. ) ;
#46587 = FACE_OUTER_BOUND ( 'NONE', #35222, .T. ) ;
#46586 = MECHANICAL_DESIGN_GEOMETRIC_PRESENTATION_REPRESENTATION (  '', ( #17350 ), #380 ) ;
#46588 = CARTESIAN_POINT ( 'NONE',  ( -159.4429263765338192, -1.166476076187852838E-15, -9.524999999999991473 ) ) ;
#46589 = CARTESIAN_POINT ( 'NONE',  ( -183.2050000000000125, -2.607480562269071545, -8.024999999999991473 ) ) ;
#46590 = ORIENTED_EDGE ( 'NONE', *, *, #30020, .T. ) ;
#46591 = LINE ( 'NONE', #67649, #11502 ) ;
#46592 = AXIS2_PLACEMENT_3D ( 'NONE', #45280, #66699, #40001 ) ;
#46593 = MECHANICAL_DESIGN_GEOMETRIC_PRESENTATION_REPRESENTATION (  '', ( #3820 ), #21842 ) ;
#46594 = CARTESIAN_POINT ( 'NONE',  ( -45.00000000000000000, 8.119648659858167861, -6.397056658262325612 ) ) ;
#46595 = EDGE_CURVE ( 'NONE', #46073, #15243, #57623, .T. ) ;
#46596 = PRESENTATION_LAYER_ASSIGNMENT (  '', '', ( #14001 ) ) ;
#46597 = SURFACE_STYLE_FILL_AREA ( #24375 ) ;
#46598 = ORIENTED_EDGE ( 'NONE', *, *, #27212, .F. ) ;
#46599 =( NAMED_UNIT ( * ) PLANE_ANGLE_UNIT ( ) SI_UNIT ( $, .RADIAN. ) );
#46600 = CARTESIAN_POINT ( 'NONE',  ( -4.250000000000001776, 21.74999999999998579, 4.000000000000000000 ) ) ;
#46601 = ORIENTED_EDGE ( 'NONE', *, *, #31533, .F. ) ;
#46602 = FACE_OUTER_BOUND ( 'NONE', #61557, .T. ) ;
#46603 = STYLED_ITEM ( 'NONE', ( #63200 ), #30079 ) ;
#46605 = ADVANCED_FACE ( 'NONE', ( #35805 ), #12662, .F. ) ;
#46604 = CARTESIAN_POINT ( 'NONE',  ( -74.99999999999998579, 50.00000000000000000, -10.00000000000000000 ) ) ;
#46606 = CARTESIAN_POINT ( 'NONE',  ( -107.7549999999999955, 4.716976649647091513, -6.492361379858946790 ) ) ;
#46607 = VERTEX_POINT ( 'NONE', #51636 ) ;
#46608 = PRESENTATION_STYLE_ASSIGNMENT (( #57095 ) ) ;
#46609 = DIRECTION ( 'NONE',  ( 0.000000000000000000, 0.000000000000000000, 1.000000000000000000 ) ) ;
#46610 = CARTESIAN_POINT ( 'NONE',  ( -142.8570736234661638, -5.598654528085803328, -7.705886871421366635 ) ) ;
#46611 = CARTESIAN_POINT ( 'NONE',  ( 9.058813317711338797, 147.8449999999999989, -2.943386871421372675 ) ) ;
#46612 = CARTESIAN_POINT ( 'NONE',  ( -75.05707362346616662, 0.000000000000000000, 9.524999999999991473 ) ) ;
#46613 = CIRCLE ( 'NONE', #17410, 5.000000000000004441 ) ;
#46614 = CARTESIAN_POINT ( 'NONE',  ( 60.00000000000000000, -2.024042244987997205E-14, 7.500000000000000000 ) ) ;
#46615 = ORIENTED_EDGE ( 'NONE', *, *, #60975, .T. ) ;
#46616 = DIRECTION ( 'NONE',  ( 0.000000000000000000, 0.000000000000000000, -1.000000000000000000 ) ) ;
#46617 = CARTESIAN_POINT ( 'NONE',  ( -17.22738557021654415, -11.12983653794787742, -4.488350797354065946 ) ) ;
#46619 = CARTESIAN_POINT ( 'NONE',  ( -6.938426666069064552, 2.291132984336068379, 1.982292489777641720 ) ) ;
#46618 = FILL_AREA_STYLE_COLOUR ( '', #4287 ) ;
#46620 = ADVANCED_FACE ( 'NONE', ( #9432 ), #3391, .F. ) ;
#46621 = VECTOR ( 'NONE', #24644, 1000.000000000000000 ) ;
#46622 = CARTESIAN_POINT ( 'NONE',  ( -124.5549999999999926, 0.000000000000000000, 8.024999999999991473 ) ) ;
#46623 = DIRECTION ( 'NONE',  ( 0.000000000000000000, 0.000000000000000000, -1.000000000000000000 ) ) ;
#46624 = CARTESIAN_POINT ( 'NONE',  ( -5.598654528085806881, 112.7449999999999903, -7.705886871421374629 ) ) ;
#46625 = CARTESIAN_POINT ( 'NONE',  ( -130.7950000000000159, 2.607480562269068880, -8.024999999999993250 ) ) ;
#46626 = AXIS2_PLACEMENT_3D ( 'NONE', #30573, #2780, #51019 ) ;
#46627 = AXIS2_PLACEMENT_3D ( 'NONE', #24107, #45611, #67029 ) ;
#46628 = VERTEX_POINT ( 'NONE', #31192 ) ;
#46629 = SURFACE_SIDE_STYLE ('',( #66649 ) ) ;
#46630 = CARTESIAN_POINT ( 'NONE',  ( -71.49999999999998579, 64.07124727947029896, -10.00000000000000000 ) ) ;
#46631 = CARTESIAN_POINT ( 'NONE',  ( -176.8429263765338249, 9.058813317711329915, -2.943386871421373119 ) ) ;
#46632 = CYLINDRICAL_SURFACE ( 'NONE', #64589, 1.000000000000000888 ) ;
#46633 = AXIS2_PLACEMENT_3D ( 'NONE', #53479, #26707, #49845 ) ;
#46634 = CARTESIAN_POINT ( 'NONE',  ( -7.632228543268607446, 124.6570736234661609, -2.479861379858953718 ) ) ;
#46635 = AXIS2_PLACEMENT_3D ( 'NONE', #12798, #12098, #50116 ) ;
#46636 = CARTESIAN_POINT ( 'NONE',  ( -80.49999999999998579, 50.00000000000000000, -6.500000000000000000 ) ) ;
#46637 = CARTESIAN_POINT ( 'NONE',  ( -4.041451884327381450, -7.000000000000002665, 1.082903768654759791 ) ) ;
#46638 = ORIENTED_EDGE ( 'NONE', *, *, #48162, .F. ) ;
#46639 = CARTESIAN_POINT ( 'NONE',  ( -82.49292637653378790, -8.102448949553172852, 5.886773742842742685 ) ) ;
#46640 = VECTOR ( 'NONE', #25824, 1000.000000000000000 ) ;
#46641 = SPHERICAL_SURFACE ( 'NONE', #44268, 0.2500000000000000000 ) ;
#46642 = CARTESIAN_POINT ( 'NONE',  ( 0.000000000000000000, 110.4999999999999858, 0.000000000000000000 ) ) ;
#46643 = AXIS2_PLACEMENT_3D ( 'NONE', #61426, #13596, #2284 ) ;
#46644 = DIRECTION ( 'NONE',  ( -1.000000000000000000, 0.000000000000000000, 6.938893903907222067E-15 ) ) ;
#46645 = CARTESIAN_POINT ( 'NONE',  ( 8.437984349512095861, 123.3070736234661524, 1.550032578732816828E-15 ) ) ;
#46646 = FILL_AREA_STYLE_COLOUR ( '', #29252 ) ;
#46647 = CARTESIAN_POINT ( 'NONE',  ( -156.6570736234661751, 9.058813317711329915, 2.943386871421369566 ) ) ;
#46648 = B_SPLINE_CURVE_WITH_KNOTS ( 'NONE', 3,
 ( #47452, #68874, #10806, #21013, #36878, #58296 ),
 .UNSPECIFIED., .F., .F.,
 ( 4, 2, 4 ),
 ( 0.000000000000000000, 0.0004110251708232767233, 0.0008220503416465534466 ),
 .UNSPECIFIED. ) ;
#46649 = ORIENTED_EDGE ( 'NONE', *, *, #29173, .T. ) ;
#46650 = DIRECTION ( 'NONE',  ( 0.000000000000000000, 0.000000000000000000, -1.000000000000000000 ) ) ;
#46651 = CARTESIAN_POINT ( 'NONE',  ( 61.99999999999998579, 30.99999999999999289, 3.750000000000000000 ) ) ;
#46652 = DIRECTION ( 'NONE',  ( 0.000000000000000000, -1.000000000000000000, 0.000000000000000000 ) ) ;
#46653 = VERTEX_POINT ( 'NONE', #15078 ) ;
#46654 = DIRECTION ( 'NONE',  ( 0.000000000000000000, 0.000000000000000000, -1.000000000000000000 ) ) ;
#46655 = SURFACE_STYLE_FILL_AREA ( #42072 ) ;
#46656 = CARTESIAN_POINT ( 'NONE',  ( 8.437984349512095861, 132.3070736234661524, 1.550032578732817026E-15 ) ) ;
#46657 = CIRCLE ( 'NONE', #26406, 4.000000000000000000 ) ;
#46658 = ORIENTED_EDGE ( 'NONE', *, *, #64017, .T. ) ;
#46659 = DIRECTION ( 'NONE',  ( 1.000000000000000000, 0.000000000000000000, -0.000000000000000000 ) ) ;
#46660 = CARTESIAN_POINT ( 'NONE',  ( -103.7049999999999983, 2.607480562269072433, 8.024999999999991473 ) ) ;
#46661 = CARTESIAN_POINT ( 'NONE',  ( 0.000000000000000000, 0.000000000000000000, 1.000000000000000000 ) ) ;
#46662 = ORIENTED_EDGE ( 'NONE', *, *, #35986, .T. ) ;
#46663 = FACE_OUTER_BOUND ( 'NONE', #29026, .T. ) ;
#46664 = CIRCLE ( 'NONE', #12907, 16.00000000000000000 ) ;
#46665 = FACE_OUTER_BOUND ( 'NONE', #10913, .T. ) ;
#46666 =( NAMED_UNIT ( * ) SI_UNIT ( $, .STERADIAN. ) SOLID_ANGLE_UNIT ( ) );
#46667 = EDGE_CURVE ( 'NONE', #38669, #46059, #27257, .T. ) ;
#46668 = COLOUR_RGB ( '', 0.40784314, 0.44705882, 0.49803922) ;
#46669 = ORIENTED_EDGE ( 'NONE', *, *, #40896, .T. ) ;
#46670 = CIRCLE ( 'NONE', #5039, 0.2500000000000002220 ) ;
#46671 = CARTESIAN_POINT ( 'NONE',  ( -80.54499999999998749, -7.632228543268600340, -2.479861379858950166 ) ) ;
#46672 = ORIENTED_EDGE ( 'NONE', *, *, #6896, .F. ) ;
#46673 = DIRECTION ( 'NONE',  ( -1.000000000000000000, 0.000000000000000000, 0.000000000000000000 ) ) ;
#46674 = FILL_AREA_STYLE_COLOUR ( '', #36765 ) ;
#46675 =( LENGTH_UNIT ( ) NAMED_UNIT ( * ) SI_UNIT ( .MILLI., .METRE. ) );
#46676 = UNCERTAINTY_MEASURE_WITH_UNIT (LENGTH_MEASURE( 1.000000000000000082E-05 ), #8, 'distance_accuracy_value', 'NONE');
#46677 = ORIENTED_EDGE ( 'NONE', *, *, #30971, .F. ) ;
#46678 = CARTESIAN_POINT ( 'NONE',  ( 22.75000000000000711, 37.00000000000000000, 4.000000000000000000 ) ) ;
#46679 = DIRECTION ( 'NONE',  ( 0.000000000000000000, 0.000000000000000000, -1.000000000000000000 ) ) ;
#46680 = DIRECTION ( 'NONE',  ( 0.000000000000000000, 0.000000000000000000, -1.000000000000000000 ) ) ;
#46682 = ADVANCED_FACE ( 'NONE', ( #69211 ), #36550, .T. ) ;
#46681 = CARTESIAN_POINT ( 'NONE',  ( 0.000000000000000000, 1.999999999999998668, 0.000000000000000000 ) ) ;
#46683 = EDGE_LOOP ( 'NONE', ( #21361, #44577, #31315, #54511 ) ) ;
#46684 = FACE_OUTER_BOUND ( 'NONE', #17665, .T. ) ;
#46685 = EDGE_CURVE ( 'NONE', #34272, #40596, #62522, .T. ) ;
#46686 = VECTOR ( 'NONE', #32411, 1000.000000000000000 ) ;
#46687 = VERTEX_POINT ( 'NONE', #36877 ) ;
#46688 = FACE_OUTER_BOUND ( 'NONE', #21250, .T. ) ;
#46689 = DIRECTION ( 'NONE',  ( -1.000000000000000000, -0.000000000000000000, 0.000000000000000000 ) ) ;
#46690 = PRESENTATION_STYLE_ASSIGNMENT (( #9716 ) ) ;
#46691 = CARTESIAN_POINT ( 'NONE',  ( -172.2570736234661695, 5.598654528085800663, -7.705886871421367523 ) ) ;
#46692 = EDGE_CURVE ( 'NONE', #4344, #28673, #8821, .T. ) ;
#46693 = CARTESIAN_POINT ( 'NONE',  ( -5.598654528085806881, 112.7449999999999903, -7.705886871421374629 ) ) ;
#46694 = CARTESIAN_POINT ( 'NONE',  ( -102.6570736234661751, 9.058813317711329915, 2.943386871421369566 ) ) ;
#46695 = FACE_OUTER_BOUND ( 'NONE', #66503, .T. ) ;
#46696 = ADVANCED_FACE ( 'NONE', ( #19618 ), #30499, .T. ) ;
#46697 = CARTESIAN_POINT ( 'NONE',  ( -74.99999999999998579, 50.00000000000000000, -10.49999999999999822 ) ) ;
#46698 = ORIENTED_EDGE ( 'NONE', *, *, #21912, .F. ) ;
#46699 = DIRECTION ( 'NONE',  ( 0.000000000000000000, 0.000000000000000000, -1.000000000000000000 ) ) ;
#46700 = CARTESIAN_POINT ( 'NONE',  ( -105.9570736234661865, 9.058813317711329915, -2.943386871421373119 ) ) ;
#46702 = CARTESIAN_POINT ( 'NONE',  ( -60.59292637653378932, -3.094860106618431139, -9.524999999999991473 ) ) ;
#46701 = CARTESIAN_POINT ( 'NONE',  ( -45.00000000000000000, -2.024042244987997205E-14, 9.500000000000000000 ) ) ;
#46703 = CARTESIAN_POINT ( 'NONE',  ( 4.250000000000001776, 22.24999999999998579, 3.750000000000000000 ) ) ;
#46704 = CARTESIAN_POINT ( 'NONE',  ( -154.2549999999999955, -4.716976649647092401, 6.492361379858946790 ) ) ;
#46705 = CYLINDRICAL_SURFACE ( 'NONE', #4923, 0.5000000000000004441 ) ;
#46706 = CARTESIAN_POINT ( 'NONE',  ( -7.896567696116268742, 111.7770433562488108, 2.415862565091794867 ) ) ;
#46707 = CARTESIAN_POINT ( 'NONE',  ( -155.8449999999999704, -7.632228543268599452, 2.479861379858951054 ) ) ;
#46708 = CARTESIAN_POINT ( 'NONE',  ( -151.3449999999999989, 7.632228543268599452, -2.479861379858951942 ) ) ;
#46709 = ORIENTED_EDGE ( 'NONE', *, *, #49830, .F. ) ;
#46710 = STYLED_ITEM ( 'NONE', ( #66170 ), #27846 ) ;
#46711 = CARTESIAN_POINT ( 'NONE',  ( 8.750000000000001776, 25.24999999999998934, 4.000000000000000000 ) ) ;
#46712 = FILL_AREA_STYLE ('',( #25196 ) ) ;
#46713 = CARTESIAN_POINT ( 'NONE',  ( 0.000000000000000000, 114.9999999999999574, -10.50000000000000000 ) ) ;
#46714 = UNCERTAINTY_MEASURE_WITH_UNIT (LENGTH_MEASURE( 1.000000000000000082E-05 ), #14101, 'distance_accuracy_value', 'NONE');
#46715 = CARTESIAN_POINT ( 'NONE',  ( -62.75499999999998835, 4.716976649647091513, -6.492361379858946790 ) ) ;
#46716 = CARTESIAN_POINT ( 'NONE',  ( -40.04190075645215785, -13.49999999999999467, 0.8979962945199019275 ) ) ;
#46717 = DIRECTION ( 'NONE',  ( -1.000000000000000000, 0.000000000000000000, 0.000000000000000000 ) ) ;
#46718 =( GEOMETRIC_REPRESENTATION_CONTEXT ( 3 ) GLOBAL_UNCERTAINTY_ASSIGNED_CONTEXT ( ( #32628 ) ) GLOBAL_UNIT_ASSIGNED_CONTEXT ( ( #1515, #12814, #43833 ) ) REPRESENTATION_CONTEXT ( 'NONE', 'WORKASPACE' ) );
#46719 = CARTESIAN_POINT ( 'NONE',  ( -61.04499999999998749, 7.632228543268600340, 2.479861379858949277 ) ) ;
#46720 = CARTESIAN_POINT ( 'NONE',  ( -9.058813317711338797, 159.4549999999999841, 2.943386871421373563 ) ) ;
#46721 = DIRECTION ( 'NONE',  ( -0.000000000000000000, -0.3420201433256629953, 0.9396926207859104263 ) ) ;
#46722 = VECTOR ( 'NONE', #31921, 1000.000000000000000 ) ;
#46723 = DIRECTION ( 'NONE',  ( 0.000000000000000000, 1.000000000000000000, 0.000000000000000000 ) ) ;
#46724 = UNCERTAINTY_MEASURE_WITH_UNIT (LENGTH_MEASURE( 1.000000000000000082E-05 ), #25445, 'distance_accuracy_value', 'NONE');
#46725 = CARTESIAN_POINT ( 'NONE',  ( 83.37126795232985899, 310.6078173946740435, -70.26655614460332799 ) ) ;
#46726 = LINE ( 'NONE', #68136, #64127 ) ;
#46727 = FILL_AREA_STYLE_COLOUR ( '', #48347 ) ;
#46728 =( NAMED_UNIT ( * ) SI_UNIT ( $, .STERADIAN. ) SOLID_ANGLE_UNIT ( ) );
#46729 = PRESENTATION_LAYER_ASSIGNMENT (  '', '', ( #1732 ) ) ;
#46730 =( NAMED_UNIT ( * ) SI_UNIT ( $, .STERADIAN. ) SOLID_ANGLE_UNIT ( ) );
#46731 = CARTESIAN_POINT ( 'NONE',  ( 3.249999999999999112, 34.24999999999998579, -3.750000000000000000 ) ) ;
#46732 = AXIS2_PLACEMENT_3D ( 'NONE', #31726, #27476, #64446 ) ;
#46733 = CARTESIAN_POINT ( 'NONE',  ( 30.50000000000000711, 18.74999999999997868, -3.750000000000000000 ) ) ;
#46734 = ORIENTED_EDGE ( 'NONE', *, *, #48426, .F. ) ;
#46735 = EDGE_LOOP ( 'NONE', ( #12449, #57081, #19929, #52194 ) ) ;
#46736 = DIRECTION ( 'NONE',  ( 0.000000000000000000, 0.000000000000000000, 1.000000000000000000 ) ) ;
#46738 = DIRECTION ( 'NONE',  ( 0.000000000000000000, 0.000000000000000000, 1.000000000000000000 ) ) ;
#46737 = TOROIDAL_SURFACE ( 'NONE', #1690, 8.499999999999994671, 0.5000000000000000000 ) ;
#46739 = PRESENTATION_LAYER_ASSIGNMENT (  '', '', ( #28687 ) ) ;
#46740 = CARTESIAN_POINT ( 'NONE',  ( -21.02379604162863558, 114.4999999999999574, 10.00000000000000000 ) ) ;
#46741 = CARTESIAN_POINT ( 'NONE',  ( -43.99999999999998579, 0.000000000000000000, 0.000000000000000000 ) ) ;
#46742 = VERTEX_POINT ( 'NONE', #3752 ) ;
#46743 = ORIENTED_EDGE ( 'NONE', *, *, #33304, .F. ) ;
#46744 = CARTESIAN_POINT ( 'NONE',  ( 47.50000000000000000, 99.99999999999992895, -9.500000000000000000 ) ) ;
#46745 = SURFACE_SIDE_STYLE ('',( #9061 ) ) ;
#46746 = ORIENTED_EDGE ( 'NONE', *, *, #57361, .F. ) ;
#46747 = CARTESIAN_POINT ( 'NONE',  ( -1.166476076187854022E-15, 118.0549999999999926, 9.525000000000000355 ) ) ;
#46748 = DIRECTION ( 'NONE',  ( 1.084202172485504434E-16, 0.000000000000000000, 1.000000000000000000 ) ) ;
#46749 = PRESENTATION_STYLE_ASSIGNMENT (( #68160 ) ) ;
#46750 = EDGE_CURVE ( 'NONE', #7249, #68346, #37490, .T. ) ;
#46751 = FILL_AREA_STYLE ('',( #8381 ) ) ;
#46752 = CARTESIAN_POINT ( 'NONE',  ( -108.2949999999999733, -2.607480562269069768, 8.024999999999991473 ) ) ;
#46753 = ORIENTED_EDGE ( 'NONE', *, *, #13114, .F. ) ;
#46754 = EDGE_CURVE ( 'NONE', #13202, #60808, #30635, .T. ) ;
#46755 = LINE ( 'NONE', #41445, #68119 ) ;
#46756 =( LENGTH_UNIT ( ) NAMED_UNIT ( * ) SI_UNIT ( .MILLI., .METRE. ) );
#46757 = SURFACE_SIDE_STYLE ('',( #15073 ) ) ;
#46758 = ORIENTED_EDGE ( 'NONE', *, *, #8825, .T. ) ;
#46759 = CARTESIAN_POINT ( 'NONE',  ( 7.632228543268608334, 146.3429263765338249, -2.479861379858951942 ) ) ;
#46760 = CARTESIAN_POINT ( 'NONE',  ( 10.00000000000001776, 42.00000000000000000, 28.38386403503541899 ) ) ;
#46761 = SURFACE_SIDE_STYLE ('',( #57608 ) ) ;
#46762 = CYLINDRICAL_SURFACE ( 'NONE', #16602, 14.00000000000000533 ) ;
#46763 = ORIENTED_EDGE ( 'NONE', *, *, #60947, .T. ) ;
#46764 = EDGE_CURVE ( 'NONE', #62297, #47153, #5487, .T. ) ;
#46765 = ORIENTED_EDGE ( 'NONE', *, *, #13301, .T. ) ;
#46766 = CARTESIAN_POINT ( 'NONE',  ( 29.00000000000002842, 42.58578643762690774, 80.00402776293826435 ) ) ;
#46767 = VECTOR ( 'NONE', #15332, 1000.000000000000000 ) ;
#46768 = AXIS2_PLACEMENT_3D ( 'NONE', #45361, #56554, #66780 ) ;
#46769 = FILL_AREA_STYLE_COLOUR ( '', #34631 ) ;
#46770 = FILL_AREA_STYLE_COLOUR ( '', #26236 ) ;
#46771 = CARTESIAN_POINT ( 'NONE',  ( -33.41658301726149460, -9.461864478049042404, 4.963675025617548364 ) ) ;
#46772 = COLOUR_RGB ( '', 0.08235294, 0.09019608, 0.10196078) ;
#46773 = CARTESIAN_POINT ( 'NONE',  ( -125.4549999999999841, 7.632228543268599452, -2.479861379858951942 ) ) ;
#46774 = CARTESIAN_POINT ( 'NONE',  ( -184.0000000000000000, 0.000000000000000000, 8.024999999999991473 ) ) ;
#46775 =( BOUNDED_CURVE ( )  B_SPLINE_CURVE ( 3, ( #22260, #41410, #54259, #48342 ),
 .UNSPECIFIED., .F., .F. ) 
 B_SPLINE_CURVE_WITH_KNOTS ( ( 4, 4 ),
 ( 4.712388980384689674, 6.283185307179586232 ),
 .UNSPECIFIED. ) 
 CURVE ( )  GEOMETRIC_REPRESENTATION_ITEM ( )  RATIONAL_B_SPLINE_CURVE ( ( 1.000000000000000000, 0.8047378541243649375, 0.8047378541243649375, 1.000000000000000000 ) ) 
 REPRESENTATION_ITEM ( '' )  );
#46776 = CARTESIAN_POINT ( 'NONE',  ( 10.00000000000001954, 42.00000000000000000, 28.38386403503541899 ) ) ;
#46777 = SURFACE_SIDE_STYLE ('',( #29492 ) ) ;
#46778 = CARTESIAN_POINT ( 'NONE',  ( -124.9429263765338192, 0.000000000000000000, 9.524999999999991473 ) ) ;
#46779 = EDGE_CURVE ( 'NONE', #1044, #49461, #9328, .T. ) ;
#46780 = DIRECTION ( 'NONE',  ( 0.000000000000000000, -1.000000000000000000, 0.000000000000000000 ) ) ;
#46781 = FILL_AREA_STYLE ('',( #8739 ) ) ;
#46782 = ORIENTED_EDGE ( 'NONE', *, *, #30727, .F. ) ;
#46783 = ORIENTED_EDGE ( 'NONE', *, *, #34901, .T. ) ;
#46784 = DIRECTION ( 'NONE',  ( -0.000000000000000000, -1.000000000000000000, -0.000000000000000000 ) ) ;
#46785 = SURFACE_SIDE_STYLE ('',( #25941 ) ) ;
#46786 =( LENGTH_UNIT ( ) NAMED_UNIT ( * ) SI_UNIT ( .MILLI., .METRE. ) );
#46787 = FACE_OUTER_BOUND ( 'NONE', #66423, .T. ) ;
#46789 = VERTEX_POINT ( 'NONE', #43556 ) ;
#46788 = COLOUR_RGB ( '', 0.31764706, 0.68627451, 0.89019608) ;
#46790 = CARTESIAN_POINT ( 'NONE',  ( -175.2549999999999955, -4.716976649647092401, 6.492361379858946790 ) ) ;
#46791 = FILL_AREA_STYLE ('',( #8416 ) ) ;
#46792 = FILL_AREA_STYLE_COLOUR ( '', #67251 ) ;
#46793 = CARTESIAN_POINT ( 'NONE',  ( -50.60707362346615668, -8.102448949553172852, 5.886773742842742685 ) ) ;
#46794 = COLOUR_RGB ( '', 0.09019608, 0.27058824, 0.51372549) ;
#46795 = CARTESIAN_POINT ( 'NONE',  ( -179.0949999999999704, -2.607480562269071545, -8.024999999999991473 ) ) ;
#46796 = CARTESIAN_POINT ( 'NONE',  ( 8.250000000000001776, 31.24999999999998579, 4.000000000000000000 ) ) ;
#46797 = AXIS2_PLACEMENT_3D ( 'NONE', #29464, #23843, #35458 ) ;
#46798 = ORIENTED_EDGE ( 'NONE', *, *, #49975, .T. ) ;
#46799 = DIRECTION ( 'NONE',  ( 0.000000000000000000, 0.000000000000000000, -1.000000000000000000 ) ) ;
#46800 = CARTESIAN_POINT ( 'NONE',  ( 45.65811388300841855, 10.21937129433612057, -6.500000000000000000 ) ) ;
#46801 = CARTESIAN_POINT ( 'NONE',  ( -95.30499999999997840, 8.437984349512085203, -1.550032578732815448E-15 ) ) ;
#46802 = LINE ( 'NONE', #19983, #47218 ) ;
#46804 = ADVANCED_FACE ( 'NONE', ( #26939 ), #16112, .T. ) ;
#46803 = DIRECTION ( 'NONE',  ( 0.000000000000000000, -0.9944852160011111719, -0.1048768571002353378 ) ) ;
#46805 = CARTESIAN_POINT ( 'NONE',  ( -92.84499999999998465, -7.632228543268599452, 2.479861379858951054 ) ) ;
#46806 = CARTESIAN_POINT ( 'NONE',  ( 5.598654528085805993, 127.3549999999999898, 7.705886871421374629 ) ) ;
#46807 = CARTESIAN_POINT ( 'NONE',  ( -71.24499999999999034, -4.716976649647093289, -6.492361379858945902 ) ) ;
#46808 = DIRECTION ( 'NONE',  ( -1.000000000000000000, 1.189524669241239115E-16, 0.000000000000000000 ) ) ;
#46809 = CARTESIAN_POINT ( 'NONE',  ( 31.00000000000000000, 14.00000000000000000, -79.00402776293826435 ) ) ;
#46810 = DIRECTION ( 'NONE',  ( -0.6163733505291654202, 0.000000000000000000, 0.7874540575534871856 ) ) ;
#46811 = UNCERTAINTY_MEASURE_WITH_UNIT (LENGTH_MEASURE( 1.000000000000000082E-05 ), #27617, 'distance_accuracy_value', 'NONE');
#46812 = ADVANCED_FACE ( 'NONE', ( #7516 ), #53699, .F. ) ;
#46813 = CARTESIAN_POINT ( 'NONE',  ( 0.000000000000000000, 110.4999999999999858, 0.000000000000000000 ) ) ;
#46814 = AXIS2_PLACEMENT_3D ( 'NONE', #46731, #34472, #52652 ) ;
#46815 = SURFACE_SIDE_STYLE ('',( #46451 ) ) ;
#46816 = VERTEX_POINT ( 'NONE', #55708 ) ;
#46817 = CARTESIAN_POINT ( 'NONE',  ( -108.2929263765337851, 3.094860106618428031, -9.524999999999993250 ) ) ;
#46818 = CARTESIAN_POINT ( 'NONE',  ( -132.1449999999999818, -4.716976649647092401, 6.492361379858946790 ) ) ;
#46819 = SURFACE_STYLE_USAGE ( .BOTH. , #1714 ) ;
#46820 = VECTOR ( 'NONE', #11577, 1000.000000000000000 ) ;
#46821 = AXIS2_PLACEMENT_3D ( 'NONE', #62516, #8717, #42176 ) ;
#46823 = DIRECTION ( 'NONE',  ( -0.000000000000000000, -0.000000000000000000, -1.000000000000000000 ) ) ;
#46822 = CARTESIAN_POINT ( 'NONE',  ( 0.000000000000000000, 2.299999999999999822, -3.000000000000000444 ) ) ;
#46824 =( GEOMETRIC_REPRESENTATION_CONTEXT ( 3 ) GLOBAL_UNCERTAINTY_ASSIGNED_CONTEXT ( ( #26405 ) ) GLOBAL_UNIT_ASSIGNED_CONTEXT ( ( #27549, #758, #38531 ) ) REPRESENTATION_CONTEXT ( 'NONE', 'WORKASPACE' ) );
#46825 = CARTESIAN_POINT ( 'NONE',  ( -12.72792206135785698, 115.4999999999999574, 10.50000000000000000 ) ) ;
#46826 = ORIENTED_EDGE ( 'NONE', *, *, #3878, .T. ) ;
#46827 = EDGE_LOOP ( 'NONE', ( #27203, #9334, #45952, #43109 ) ) ;
#46828 = CARTESIAN_POINT ( 'NONE',  ( 4.716976649647099507, 131.6429263765338362, -6.492361379858953008 ) ) ;
#46829 =( NAMED_UNIT ( * ) SI_UNIT ( $, .STERADIAN. ) SOLID_ANGLE_UNIT ( ) );
#46830 = DIRECTION ( 'NONE',  ( -1.000000000000000000, -0.000000000000000000, -0.000000000000000000 ) ) ;
#46831 = ORIENTED_EDGE ( 'NONE', *, *, #61051, .F. ) ;
#46832 = CARTESIAN_POINT ( 'NONE',  ( -118.7049999999999841, 2.607480562269072433, 8.024999999999991473 ) ) ;
#46834 = EDGE_CURVE ( 'NONE', #14756, #3256, #5931, .T. ) ;
#46833 = ORIENTED_EDGE ( 'NONE', *, *, #21596, .F. ) ;
#46835 = AXIS2_PLACEMENT_3D ( 'NONE', #62155, #45686, #67105 ) ;
#46836 = CARTESIAN_POINT ( 'NONE',  ( -127.4070736234661751, 3.094860106618428031, -9.524999999999993250 ) ) ;
#46837 = EDGE_CURVE ( 'NONE', #36852, #49243, #45306, .T. ) ;
#46838 = VERTEX_POINT ( 'NONE', #39915 ) ;
#46839 = CARTESIAN_POINT ( 'NONE',  ( -23.71231517720798365, 112.4999999999999858, -10.00000000000000000 ) ) ;
#46840 = ORIENTED_EDGE ( 'NONE', *, *, #50754, .T. ) ;
#46841 = CARTESIAN_POINT ( 'NONE',  ( -8.082903768654762899, 3.463586619550771876E-15, 1.082903768654759125 ) ) ;
#46842 = CARTESIAN_POINT ( 'NONE',  ( 5.598654528085809545, 145.1450000000000102, -7.705886871421373741 ) ) ;
#46843 = FILL_AREA_STYLE ('',( #67194 ) ) ;
#46844 = ORIENTED_EDGE ( 'NONE', *, *, #58146, .F. ) ;
#46845 = DIRECTION ( 'NONE',  ( 0.000000000000000000, -1.000000000000000000, 0.000000000000000000 ) ) ;
#46847 = EDGE_CURVE ( 'NONE', #40244, #47977, #41953, .T. ) ;
#46846 = CARTESIAN_POINT ( 'NONE',  ( -5.598654528085806881, 146.8549999999999898, -7.705886871421374629 ) ) ;
#46848 = CARTESIAN_POINT ( 'NONE',  ( 26.00000000000001776, 15.00000000000000000, 34.49999999999999289 ) ) ;
#46849 = ORIENTED_EDGE ( 'NONE', *, *, #13589, .T. ) ;
#46850 = CARTESIAN_POINT ( 'NONE',  ( 6.826472737025121695, 113.4929263765337879, -4.959722759717905660 ) ) ;
#46851 = CARTESIAN_POINT ( 'NONE',  ( 44.99999999999977973, 146.4999999999999716, 7.500000000000000000 ) ) ;
#46852 = UNCERTAINTY_MEASURE_WITH_UNIT (LENGTH_MEASURE( 1.000000000000000082E-05 ), #30764, 'distance_accuracy_value', 'NONE');
#46853 =( NAMED_UNIT ( * ) PLANE_ANGLE_UNIT ( ) SI_UNIT ( $, .RADIAN. ) );
#46854 = DIRECTION ( 'NONE',  ( 0.000000000000000000, -1.000000000000000000, 0.000000000000000000 ) ) ;
#46855 = CARTESIAN_POINT ( 'NONE',  ( 48.50000000000000000, 99.99999999999992895, 7.000000000000000000 ) ) ;
#46856 = ORIENTED_EDGE ( 'NONE', *, *, #722, .T. ) ;
#46857 = CARTESIAN_POINT ( 'NONE',  ( 29.00000000000002842, 35.42594141563417054, 80.00402776293826435 ) ) ;
#46858 = ADVANCED_FACE ( 'NONE', ( #53381 ), #16801, .T. ) ;
#46859 = ORIENTED_EDGE ( 'NONE', *, *, #59951, .T. ) ;
#46860 = CARTESIAN_POINT ( 'NONE',  ( -57.14292637653378648, 5.598654528085800663, -7.705886871421367523 ) ) ;
#46861 = SURFACE_STYLE_USAGE ( .BOTH. , #15179 ) ;
#46862 = FILL_AREA_STYLE ('',( #15180 ) ) ;
#46863 = CARTESIAN_POINT ( 'NONE',  ( -153.8049999999999784, -8.437984349512085203, 5.166775262442717831E-16 ) ) ;
#46864 = ORIENTED_EDGE ( 'NONE', *, *, #39346, .F. ) ;
#46865 = CARTESIAN_POINT ( 'NONE',  ( 12.72792206135785698, 149.9999999999999716, -10.00000000000000000 ) ) ;
#46866 = UNCERTAINTY_MEASURE_WITH_UNIT (LENGTH_MEASURE( 1.000000000000000082E-05 ), #43961, 'distance_accuracy_value', 'NONE');
#46867 = CARTESIAN_POINT ( 'NONE',  ( 22.00000000000002132, 50.00000000000000000, 60.00000000000000711 ) ) ;
#46868 = EDGE_CURVE ( 'NONE', #55641, #36029, #6319, .T. ) ;
#46869 = DIRECTION ( 'NONE',  ( 1.000000000000000000, 7.709882115452468306E-16, -0.000000000000000000 ) ) ;
#46870 = DIRECTION ( 'NONE',  ( 0.000000000000000000, -0.000000000000000000, -1.000000000000000000 ) ) ;
#46871 = DIRECTION ( 'NONE',  ( 0.000000000000000000, 1.000000000000000000, 0.000000000000000000 ) ) ;
#46872 = VERTEX_POINT ( 'NONE', #8909 ) ;
#46873 = ORIENTED_EDGE ( 'NONE', *, *, #11292, .T. ) ;
#46874 = CARTESIAN_POINT ( 'NONE',  ( 22.49933229817787605, 26.84000769619876436, 27.39862673134610205 ) ) ;
#46875 = CARTESIAN_POINT ( 'NONE',  ( 21.02379604162864268, 1.797044900979284448E-15, 10.00000000000000000 ) ) ;
#46876 = CARTESIAN_POINT ( 'NONE',  ( -62.15499999999998693, 7.632228543268600340, 2.479861379858949277 ) ) ;
#46877 = ORIENTED_EDGE ( 'NONE', *, *, #47317, .F. ) ;
#46878 = SURFACE_SIDE_STYLE ('',( #4215 ) ) ;
#46879 = CYLINDRICAL_SURFACE ( 'NONE', #52048, 0.5000000000000004441 ) ;
#46880 = AXIS2_PLACEMENT_3D ( 'NONE', #60200, #20343, #33133 ) ;
#46881 = DIRECTION ( 'NONE',  ( -1.000000000000000000, 0.000000000000000000, 0.000000000000000000 ) ) ;
#46882 = DIRECTION ( 'NONE',  ( 1.000000000000000000, 0.000000000000000000, -0.000000000000000000 ) ) ;
#46883 = ORIENTED_EDGE ( 'NONE', *, *, #38499, .F. ) ;
#46884 =( BOUNDED_CURVE ( )  B_SPLINE_CURVE ( 2, ( #27025, #58374, #48559, #52773, #58727, #31637, #26355, #47893, #15496, #4548, #20758 ),
 .UNSPECIFIED., .F., .F. ) 
 B_SPLINE_CURVE_WITH_KNOTS ( ( 3, 2, 2, 2, 2, 3 ),
 ( 0.3369565217391226053, 0.3391304347826007426, 0.3413043478260789354, 0.3434782608695571282, 0.3456521739130353210, 0.3478260869565134583 ),
 .UNSPECIFIED. ) 
 CURVE ( )  GEOMETRIC_REPRESENTATION_ITEM ( )  RATIONAL_B_SPLINE_CURVE ( ( 1.000000000000176303, 0.9510565162949773388, 1.000000000000000000, 0.9510565162951535312, 1.000000000000000000, 0.9510565162951535312, 1.000000000000000000, 0.9510565162951535312, 1.000000000000000000, 0.9510565162953397156, 0.9999999999998138156 ) ) 
 REPRESENTATION_ITEM ( '' )  );
#46885 = CARTESIAN_POINT ( 'NONE',  ( -75.00000000000000000, 8.701466902705684348, -5.869459488308679695 ) ) ;
#46886 = PRESENTATION_STYLE_ASSIGNMENT (( #41573 ) ) ;
#46887 = DIRECTION ( 'NONE',  ( 0.000000000000000000, 1.000000000000000000, 1.350863103983176297E-16 ) ) ;
#46888 = MECHANICAL_DESIGN_GEOMETRIC_PRESENTATION_REPRESENTATION (  '', ( #24324 ), #2932 ) ;
#46889 = CARTESIAN_POINT ( 'NONE',  ( 3.094860106618435136, 151.2949999999999875, -9.525000000000000355 ) ) ;
#46890 = CARTESIAN_POINT ( 'NONE',  ( -96.14499999999999602, -4.716976649647092401, 6.492361379858946790 ) ) ;
#46891 = LINE ( 'NONE', #68294, #17958 ) ;
#46892 = UNCERTAINTY_MEASURE_WITH_UNIT (LENGTH_MEASURE( 1.000000000000000082E-05 ), #57520, 'distance_accuracy_value', 'NONE');
#46893 = EDGE_CURVE ( 'NONE', #51117, #56449, #48726, .T. ) ;
#46894 = DIRECTION ( 'NONE',  ( 0.000000000000000000, 0.000000000000000000, -1.000000000000000000 ) ) ;
#46895 = ORIENTED_EDGE ( 'NONE', *, *, #38980, .F. ) ;
#46896 = CARTESIAN_POINT ( 'NONE',  ( -131.2429263765338021, 5.598654528085804216, 7.705886871421366635 ) ) ;
#46897 = CARTESIAN_POINT ( 'NONE',  ( -155.5449999999999875, -7.632228543268600340, -2.479861379858950166 ) ) ;
#46898 = DIRECTION ( 'NONE',  ( -0.7833176619561906806, -0.6216216216216158275, 0.000000000000000000 ) ) ;
#46899 = CARTESIAN_POINT ( 'NONE',  ( -133.3429263765337964, -9.058813317711329915, 2.943386871421371787 ) ) ;
#46900 = ORIENTED_EDGE ( 'NONE', *, *, #32634, .F. ) ;
#46901 = FACE_OUTER_BOUND ( 'NONE', #16382, .T. ) ;
#46902 = ORIENTED_EDGE ( 'NONE', *, *, #24363, .F. ) ;
#46903 =( LENGTH_UNIT ( ) NAMED_UNIT ( * ) SI_UNIT ( .MILLI., .METRE. ) );
#46904 = EDGE_CURVE ( 'NONE', #17887, #51828, #3700, .T. ) ;
#46905 = DIRECTION ( 'NONE',  ( 1.156482317317873451E-16, 1.000000000000000000, 0.000000000000000000 ) ) ;
#46906 = CARTESIAN_POINT ( 'NONE',  ( -61.49999999999998579, 50.00000000000000000, 10.00000000000000000 ) ) ;
#46907 = CARTESIAN_POINT ( 'NONE',  ( -173.0070736234661695, -8.102448949553174629, -5.886773742842741797 ) ) ;
#46908 = DIRECTION ( 'NONE',  ( 0.000000000000000000, -1.000000000000000000, 0.000000000000000000 ) ) ;
#46909 = ORIENTED_EDGE ( 'NONE', *, *, #39903, .F. ) ;
#46910 = CARTESIAN_POINT ( 'NONE',  ( -164.6049999999999613, 6.826472737025113702, -4.959722759717902107 ) ) ;
#46911 = EDGE_CURVE ( 'NONE', #62752, #28347, #38632, .T. ) ;
#46912 = ADVANCED_FACE ( 'NONE', ( #41296 ), #35301, .T. ) ;
#46913 = EDGE_LOOP ( 'NONE', ( #68963, #29575, #56865, #55330, #38336, #5394, #4626, #44996, #14066, #60385 ) ) ;
#46914 = CARTESIAN_POINT ( 'NONE',  ( 24.75000000000000355, 37.00000000000000000, -3.000000000000000000 ) ) ;
#46915 = ORIENTED_EDGE ( 'NONE', *, *, #66192, .T. ) ;
#46916 =( NAMED_UNIT ( * ) PLANE_ANGLE_UNIT ( ) SI_UNIT ( $, .RADIAN. ) );
#46917 = CARTESIAN_POINT ( 'NONE',  ( -58.55707362346616662, -1.166476076187852838E-15, -9.524999999999991473 ) ) ;
#46918 = CARTESIAN_POINT ( 'NONE',  ( 3.094860106618431583, 114.0949999999999704, 9.525000000000000355 ) ) ;
#46919 = ORIENTED_EDGE ( 'NONE', *, *, #60557, .T. ) ;
#46920 = CARTESIAN_POINT ( 'NONE',  ( 8.000000000000030198, 0.000000000000000000, 29.00402776293826079 ) ) ;
#46922 = ADVANCED_FACE ( 'NONE', ( #2883 ), #34944, .F. ) ;
#46921 = CARTESIAN_POINT ( 'NONE',  ( -3.094860106618432471, 116.7049999999999841, -9.525000000000000355 ) ) ;
#46923 = CARTESIAN_POINT ( 'NONE',  ( -69.80499999999997840, -8.437984349512086979, 5.166775262442717831E-16 ) ) ;
#46924 = CARTESIAN_POINT ( 'NONE',  ( 0.000000000000000000, -2.500000000000000000, 0.000000000000000000 ) ) ;
#46925 = ORIENTED_EDGE ( 'NONE', *, *, #18816, .F. ) ;
#46926 = CARTESIAN_POINT ( 'NONE',  ( 9.058813317711337021, 139.6550000000000011, 2.943386871421375783 ) ) ;
#46927 = UNCERTAINTY_MEASURE_WITH_UNIT (LENGTH_MEASURE( 1.000000000000000082E-05 ), #53646, 'distance_accuracy_value', 'NONE');
#46928 = CARTESIAN_POINT ( 'NONE',  ( -75.50000000000000000, -6.499999999999992006, 21.00000000000000000 ) ) ;
#46929 = EDGE_CURVE ( 'NONE', #68782, #25473, #61645, .T. ) ;
#46930 = AXIS2_PLACEMENT_3D ( 'NONE', #44425, #39469, #50688 ) ;
#46931 = DIRECTION ( 'NONE',  ( -0.000000000000000000, -0.6449798928094537809, 0.7641995406119435064 ) ) ;
#46932 = DIRECTION ( 'NONE',  ( -1.000000000000000000, 0.000000000000000000, 0.000000000000000000 ) ) ;
#46933 = ORIENTED_EDGE ( 'NONE', *, *, #66055, .F. ) ;
#46934 = CARTESIAN_POINT ( 'NONE',  ( -5.196152422706636465, 2.500000000000000000, 9.000000000000001776 ) ) ;
#46935 = CARTESIAN_POINT ( 'NONE',  ( -34.99999999999992895, 112.4999999999999858, -9.500000000000000000 ) ) ;
#46936 = CARTESIAN_POINT ( 'NONE',  ( -6.062177826491070398, -2.500000000000000000, -3.499999999999998224 ) ) ;
#46937 = CARTESIAN_POINT ( 'NONE',  ( -177.6550000000000011, -7.632228543268600340, -2.479861379858950166 ) ) ;
#46938 = ORIENTED_EDGE ( 'NONE', *, *, #14636, .T. ) ;
#46939 = CARTESIAN_POINT ( 'NONE',  ( 6.946753979098149401, 111.6727723711330071, -4.645043913640917843 ) ) ;
#46940 =( REPRESENTATION_RELATIONSHIP ('NONE','NONE', #5102, #21747 ) REPRESENTATION_RELATIONSHIP_WITH_TRANSFORMATION ( #31783 )SHAPE_REPRESENTATION_RELATIONSHIP( ) );
#46941 = CARTESIAN_POINT ( 'NONE',  ( 22.99999999999998934, 5.000000000000000000, 37.00402776293825724 ) ) ;
#46942 = ORIENTED_EDGE ( 'NONE', *, *, #16630, .F. ) ;
#46943 = SURFACE_STYLE_USAGE ( .BOTH. , #35652 ) ;
#46944 = LINE ( 'NONE', #68351, #34376 ) ;
#46945 = ORIENTED_EDGE ( 'NONE', *, *, #19217, .T. ) ;
#46946 = DIRECTION ( 'NONE',  ( -0.000000000000000000, 1.000000000000000000, 0.000000000000000000 ) ) ;
#46947 = CARTESIAN_POINT ( 'NONE',  ( -91.85499999999998977, 4.716976649647094177, 6.492361379858945902 ) ) ;
#46948 = ORIENTED_EDGE ( 'NONE', *, *, #60648, .F. ) ;
#46949 = FILL_AREA_STYLE_COLOUR ( '', #38196 ) ;
#46950 = CARTESIAN_POINT ( 'NONE',  ( -139.5570736234661808, -1.166476076187852838E-15, -9.524999999999991473 ) ) ;
#46951 = EDGE_CURVE ( 'NONE', #50261, #41081, #25130, .T. ) ;
#46952 = CARTESIAN_POINT ( 'NONE',  ( 74.50000000000000000, -2.220952357103124925E-14, 6.500000000000000000 ) ) ;
#46953 = PRESENTATION_STYLE_ASSIGNMENT (( #10658 ) ) ;
#46954 = CARTESIAN_POINT ( 'NONE',  ( -73.25707362346616947, 5.598654528085800663, -7.705886871421367523 ) ) ;
#46955 = DIRECTION ( 'NONE',  ( 0.000000000000000000, 0.000000000000000000, 1.000000000000000000 ) ) ;
#46956 = ORIENTED_EDGE ( 'NONE', *, *, #47963, .T. ) ;
#46957 = CARTESIAN_POINT ( 'NONE',  ( -69.99999999999998579, 50.00000000000000000, -12.00000000000000000 ) ) ;
#46958 = DIRECTION ( 'NONE',  ( 0.000000000000000000, 0.000000000000000000, -1.000000000000000000 ) ) ;
#46960 = CARTESIAN_POINT ( 'NONE',  ( -24.00000000000000355, 37.00000000000000000, 3.000000000000000000 ) ) ;
#46959 = SURFACE_SIDE_STYLE ('',( #30706 ) ) ;
#46961 = CARTESIAN_POINT ( 'NONE',  ( -107.7549999999999955, 4.716976649647091513, -6.492361379858946790 ) ) ;
#46962 = AXIS2_PLACEMENT_3D ( 'NONE', #21099, #42281, #15509 ) ;
#46963 = DIRECTION ( 'NONE',  ( -0.000000000000000000, -0.000000000000000000, 1.000000000000000000 ) ) ;
#46964 = CARTESIAN_POINT ( 'NONE',  ( 3.094860106618435136, 121.2949999999999733, -9.525000000000000355 ) ) ;
#46965 = CARTESIAN_POINT ( 'NONE',  ( -128.5449999999999875, -7.632228543268600340, -2.479861379858950166 ) ) ;
#46966 = SURFACE_STYLE_USAGE ( .BOTH. , #30034 ) ;
#46967 = DIRECTION ( 'NONE',  ( 0.000000000000000000, -1.000000000000000000, 0.000000000000000000 ) ) ;
#46968 = ORIENTED_EDGE ( 'NONE', *, *, #41810, .F. ) ;
#46969 = DIRECTION ( 'NONE',  ( 1.000000000000000000, 0.000000000000000000, 0.000000000000000000 ) ) ;
#46970 = CARTESIAN_POINT ( 'NONE',  ( -172.7929263765337851, -3.094860106618429807, 9.524999999999991473 ) ) ;
#46971 = FILL_AREA_STYLE_COLOUR ( '', #13556 ) ;
#46972 = SURFACE_STYLE_USAGE ( .BOTH. , #52572 ) ;
#46973 = MECHANICAL_DESIGN_GEOMETRIC_PRESENTATION_REPRESENTATION (  '', ( #53642 ), #13208 ) ;
#46974 = AXIS2_PLACEMENT_3D ( 'NONE', #22833, #49923, #61144 ) ;
#46975 = CARTESIAN_POINT ( 'NONE',  ( 57.00000000000000000, 13.00000000000000178, -60.00402776293827145 ) ) ;
#46976 = EDGE_CURVE ( 'NONE', #37991, #47273, #42010, .T. ) ;
#46977 = CYLINDRICAL_SURFACE ( 'NONE', #18129, 0.2500000000000002220 ) ;
#46978 = ORIENTED_EDGE ( 'NONE', *, *, #29613, .F. ) ;
#46979 = CARTESIAN_POINT ( 'NONE',  ( -81.44292637653380496, -1.166476076187852838E-15, -9.524999999999991473 ) ) ;
#46980 = CONTEXT_DEPENDENT_SHAPE_REPRESENTATION ( #34735, #58680 ) ;
#46981 = DIRECTION ( 'NONE',  ( -0.000000000000000000, -0.000000000000000000, -1.000000000000000000 ) ) ;
#46982 = CARTESIAN_POINT ( 'NONE',  ( -7.749999999999993783, 0.000000000000000000, 0.000000000000000000 ) ) ;
#46983 = EDGE_CURVE ( 'NONE', #50938, #39701, #15020, .T. ) ;
#46984 = FILL_AREA_STYLE ('',( #59193 ) ) ;
#46985 = CARTESIAN_POINT ( 'NONE',  ( -17.75000000000000355, -4.000000000000000000, 20.00000000000000000 ) ) ;
#46986 = EDGE_CURVE ( 'NONE', #2072, #17063, #65547, .T. ) ;
#46987 = EDGE_LOOP ( 'NONE', ( #8269, #25924, #11750, #9562 ) ) ;
#46988 = DIRECTION ( 'NONE',  ( 1.000000000000000000, 0.000000000000000000, -1.300977106640435137E-16 ) ) ;
#46989 = PLANE ( 'NONE',  #36532 ) ;
#46990 =( LENGTH_UNIT ( ) NAMED_UNIT ( * ) SI_UNIT ( .MILLI., .METRE. ) );
#46991 = VERTEX_POINT ( 'NONE', #58484 ) ;
#46992 = CARTESIAN_POINT ( 'NONE',  ( 7.794228634059945371, -2.500000000000000000, 4.500000000000000888 ) ) ;
#46993 = CARTESIAN_POINT ( 'NONE',  ( -2.607480562269073765, 136.2070736234661581, -8.025000000000000355 ) ) ;
#46994 = ORIENTED_EDGE ( 'NONE', *, *, #67500, .T. ) ;
#46995 = CIRCLE ( 'NONE', #36844, 16.00000000000000711 ) ;
#46996 = CARTESIAN_POINT ( 'NONE',  ( 4.750000000000002665, 24.74999999999998579, 3.750000000000000000 ) ) ;
#46997 = CARTESIAN_POINT ( 'NONE',  ( -105.0549999999999926, -9.827790563157499189E-16, -8.024999999999991473 ) ) ;
#46998 = UNCERTAINTY_MEASURE_WITH_UNIT (LENGTH_MEASURE( 1.000000000000000082E-05 ), #45069, 'distance_accuracy_value', 'NONE');
#46999 = VECTOR ( 'NONE', #1483, 1000.000000000000000 ) ;
#47000 = ORIENTED_EDGE ( 'NONE', *, *, #54927, .F. ) ;
#47001 =( GEOMETRIC_REPRESENTATION_CONTEXT ( 3 ) GLOBAL_UNCERTAINTY_ASSIGNED_CONTEXT ( ( #49532 ) ) GLOBAL_UNIT_ASSIGNED_CONTEXT ( ( #22071, #11155, #49508 ) ) REPRESENTATION_CONTEXT ( 'NONE', 'WORKASPACE' ) );
#47002 = CARTESIAN_POINT ( 'NONE',  ( -34.70658214735873059, -10.70299374098435052, 2.150780036138280060 ) ) ;
#47003 = ADVANCED_FACE ( 'NONE', ( #21180 ), #50939, .T. ) ;
#47004 = SURFACE_STYLE_USAGE ( .BOTH. , #62439 ) ;
#47005 = DIRECTION ( 'NONE',  ( 0.000000000000000000, 0.000000000000000000, 1.000000000000000000 ) ) ;
#47006 = EDGE_LOOP ( 'NONE', ( #18615, #8537, #53770, #7417 ) ) ;
#47007 = DIRECTION ( 'NONE',  ( 0.000000000000000000, 0.000000000000000000, -1.000000000000000000 ) ) ;
#47008 = CARTESIAN_POINT ( 'NONE',  ( -75.29500000000000171, -2.607480562269069768, 8.024999999999991473 ) ) ;
#47009 = ORIENTED_EDGE ( 'NONE', *, *, #25626, .T. ) ;
#47010 = FILL_AREA_STYLE_COLOUR ( '', #45197 ) ;
#47011 = CARTESIAN_POINT ( 'NONE',  ( 6.000000000000015099, 17.23130743308432855, -3.144186300207962859E-15 ) ) ;
#47012 = DIRECTION ( 'NONE',  ( 1.000000000000000000, -0.000000000000000000, -1.300977106640434891E-16 ) ) ;
#47013 = ORIENTED_EDGE ( 'NONE', *, *, #17873, .F. ) ;
#47014 = DIRECTION ( 'NONE',  ( -7.703719777548942317E-32, 1.000000000000000000, 0.000000000000000000 ) ) ;
#47015 = DIRECTION ( 'NONE',  ( 0.000000000000000000, 0.000000000000000000, 1.000000000000000000 ) ) ;
#47016 = AXIS2_PLACEMENT_3D ( 'NONE', #18382, #34534, #39867 ) ;
#47017 = AXIS2_PLACEMENT_3D ( 'NONE', #64544, #11407, #775 ) ;
#47018 = PRESENTATION_STYLE_ASSIGNMENT (( #47737 ) ) ;
#47019 = ORIENTED_EDGE ( 'NONE', *, *, #4417, .F. ) ;
#47020 = VERTEX_POINT ( 'NONE', #9960 ) ;
#47021 = SURFACE_STYLE_FILL_AREA ( #8656 ) ;
#47022 = CYLINDRICAL_SURFACE ( 'NONE', #55510, 0.5000000000000004441 ) ;
#47023 = CARTESIAN_POINT ( 'NONE',  ( -45.00000000000000000, 0.000000000000000000, 0.000000000000000000 ) ) ;
#47024 = CARTESIAN_POINT ( 'NONE',  ( -165.8070736234661524, 10.01517768586948698, -1.839758294383808571E-15 ) ) ;
#47025 = ADVANCED_FACE ( 'NONE', ( #10648 ), #48312, .T. ) ;
#47026 = CARTESIAN_POINT ( 'NONE',  ( 0.000000000000000000, 127.4449999999999790, -9.525000000000000355 ) ) ;
#47027 = CARTESIAN_POINT ( 'NONE',  ( -106.7070736234661865, -3.094860106618431139, -9.524999999999991473 ) ) ;
#47028 = CARTESIAN_POINT ( 'NONE',  ( 0.000000000000000000, 113.9429263765338192, -8.025000000000000355 ) ) ;
#47029 = DIRECTION ( 'NONE',  ( 1.000000000000000000, 0.000000000000000000, 0.000000000000000000 ) ) ;
#47030 = EDGE_LOOP ( 'NONE', ( #48206, #44863, #13516, #66529 ) ) ;
#47031 = CYLINDRICAL_SURFACE ( 'NONE', #67739, 0.2500000000000002220 ) ;
#47033 = CARTESIAN_POINT ( 'NONE',  ( -114.9570736234661723, 9.058813317711329915, -2.943386871421373119 ) ) ;
#47032 = DIRECTION ( 'NONE',  ( 0.000000000000000000, 0.000000000000000000, -1.000000000000000000 ) ) ;
#47034 = CARTESIAN_POINT ( 'NONE',  ( -47.50000000000000000, 99.99999999999992895, 10.00000000000000000 ) ) ;
#47035 = CARTESIAN_POINT ( 'NONE',  ( -148.4050000000000296, -2.607480562269069768, 8.024999999999991473 ) ) ;
#47036 = CARTESIAN_POINT ( 'NONE',  ( -3.869190034097910402, 110.8545876537711621, -8.353339643030292194 ) ) ;
#47037 = CARTESIAN_POINT ( 'NONE',  ( -155.5449999999999875, -7.632228543268600340, -2.479861379858950166 ) ) ;
#47038 = CONICAL_SURFACE ( 'NONE', #51503, 5.000000000000004441, 0.7853981633974587151 ) ;
#47039 = CARTESIAN_POINT ( 'NONE',  ( -149.6949999999999648, -8.437984349512086979, 5.166775262442717831E-16 ) ) ;
#47040 = EDGE_LOOP ( 'NONE', ( #60769, #61255, #47471, #32414 ) ) ;
#47041 = AXIS2_PLACEMENT_3D ( 'NONE', #18910, #40409, #61819 ) ;
#47042 = LINE ( 'NONE', #20966, #54939 ) ;
#47043 = CARTESIAN_POINT ( 'NONE',  ( 66.74999999999998579, 34.24999999999999289, -3.750000000000000000 ) ) ;
#47044 = CYLINDRICAL_SURFACE ( 'NONE', #32708, 7.499999999999985789 ) ;
#47045 = CARTESIAN_POINT ( 'NONE',  ( -59.00499999999998124, 6.826472737025116366, 4.959722759717898555 ) ) ;
#47046 = CARTESIAN_POINT ( 'NONE',  ( -59.24499999999999034, -4.716976649647093289, -6.492361379858945902 ) ) ;
#47047 = CARTESIAN_POINT ( 'NONE',  ( -8.102448949553181734, 156.0050000000000239, -5.886773742842749790 ) ) ;
#47048 = CARTESIAN_POINT ( 'NONE',  ( 48.50000000000000000, 14.49137674618942562, 7.500000000000000000 ) ) ;
#47049 = DIRECTION ( 'NONE',  ( 0.000000000000000000, 0.000000000000000000, 1.000000000000000000 ) ) ;
#47050 = EDGE_CURVE ( 'NONE', #35442, #5819, #13883, .T. ) ;
#47051 = MECHANICAL_DESIGN_GEOMETRIC_PRESENTATION_REPRESENTATION (  '', ( #38057 ), #15556 ) ;
#47052 = LINE ( 'NONE', #10431, #31222 ) ;
#47053 = AXIS2_PLACEMENT_3D ( 'NONE', #40758, #35803, #62173 ) ;
#47054 = CARTESIAN_POINT ( 'NONE',  ( -7.186760109405158303, 110.5296962873079707, 6.248938465618036453 ) ) ;
#47055 = CARTESIAN_POINT ( 'NONE',  ( 72.00000000000000000, 14.49137674618942917, 7.500000000000000000 ) ) ;
#47056 = CARTESIAN_POINT ( 'NONE',  ( 5.196152422706636465, -9.000000000000005329, 7.500000000000000000 ) ) ;
#47057 = ADVANCED_FACE ( 'NONE', ( #25765 ), #27136, .T. ) ;
#47058 = DIRECTION ( 'NONE',  ( 8.881784197001252323E-16, 0.000000000000000000, 1.000000000000000000 ) ) ;
#47059 = DIRECTION ( 'NONE',  ( 1.000000000000000000, 0.000000000000000000, 0.000000000000000000 ) ) ;
#47060 = VERTEX_POINT ( 'NONE', #34180 ) ;
#47061 = VERTEX_POINT ( 'NONE', #65131 ) ;
#47062 = SURFACE_STYLE_FILL_AREA ( #42482 ) ;
#47063 = EDGE_CURVE ( 'NONE', #37678, #41012, #22233, .T. ) ;
#47064 = CARTESIAN_POINT ( 'NONE',  ( 31.00000000000000711, 42.00000000000000000, -36.50000000000000000 ) ) ;
#47065 = EDGE_CURVE ( 'NONE', #60615, #43704, #22586, .T. ) ;
#47066 = DIRECTION ( 'NONE',  ( 0.000000000000000000, 1.000000000000000000, 0.000000000000000000 ) ) ;
#47067 = DIRECTION ( 'NONE',  ( -1.000000000000000000, -0.000000000000000000, -0.000000000000000000 ) ) ;
#47068 = ORIENTED_EDGE ( 'NONE', *, *, #24684, .F. ) ;
#47069 = ORIENTED_EDGE ( 'NONE', *, *, #5086, .F. ) ;
#47070 = DIRECTION ( 'NONE',  ( -1.000000000000000000, 0.000000000000000000, 0.000000000000000000 ) ) ;
#47071 = ADVANCED_FACE ( 'NONE', ( #50028 ), #59503, .T. ) ;
#47072 = CARTESIAN_POINT ( 'NONE',  ( 5.196152422706636465, -9.000000000000005329, 7.500000000000000000 ) ) ;
#47073 = ORIENTED_EDGE ( 'NONE', *, *, #7388, .T. ) ;
#47074 = CARTESIAN_POINT ( 'NONE',  ( -5.598654528085806881, 119.8549999999999898, -7.705886871421374629 ) ) ;
#47075 = LINE ( 'NONE', #36536, #9696 ) ;
#47076 = PRESENTATION_LAYER_ASSIGNMENT (  '', '', ( #23426 ) ) ;
#47077 = DIRECTION ( 'NONE',  ( 0.000000000000000000, 0.000000000000000000, 1.000000000000000000 ) ) ;
#47078 = CARTESIAN_POINT ( 'NONE',  ( -96.74499999999999034, 4.716976649647094177, 6.492361379858945902 ) ) ;
#47079 = EDGE_LOOP ( 'NONE', ( #672, #28536, #63427, #8643, #25905, #28409, #34168, #31387, #44122, #11806 ) ) ;
#47080 =( GEOMETRIC_REPRESENTATION_CONTEXT ( 3 ) GLOBAL_UNCERTAINTY_ASSIGNED_CONTEXT ( ( #36080 ) ) GLOBAL_UNIT_ASSIGNED_CONTEXT ( ( #61400, #49838, #7600 ) ) REPRESENTATION_CONTEXT ( 'NONE', 'WORKASPACE' ) );
#47081 = CARTESIAN_POINT ( 'NONE',  ( -8.175053251830410872, 110.5000000000000000, 4.967543156751275113 ) ) ;
#47082 = DIRECTION ( 'NONE',  ( 0.000000000000000000, 1.000000000000000000, 0.000000000000000000 ) ) ;
#47083 = DIRECTION ( 'NONE',  ( 0.3403530053317450621, -0.9351121967924954648, -0.09861547125863368013 ) ) ;
#47084 = ORIENTED_EDGE ( 'NONE', *, *, #9816, .T. ) ;
#47085 = CARTESIAN_POINT ( 'NONE',  ( -7.632228543268607446, 156.5429263765338419, -2.479861379858953718 ) ) ;
#47086 = AXIS2_PLACEMENT_3D ( 'NONE', #34294, #40276, #7556 ) ;
#47087 =( GEOMETRIC_REPRESENTATION_CONTEXT ( 3 ) GLOBAL_UNCERTAINTY_ASSIGNED_CONTEXT ( ( #67778 ) ) GLOBAL_UNIT_ASSIGNED_CONTEXT ( ( #21918, #27836, #38486 ) ) REPRESENTATION_CONTEXT ( 'NONE', 'WORKASPACE' ) );
#47088 =( NAMED_UNIT ( * ) PLANE_ANGLE_UNIT ( ) SI_UNIT ( $, .RADIAN. ) );
#47089 =( LENGTH_UNIT ( ) NAMED_UNIT ( * ) SI_UNIT ( .MILLI., .METRE. ) );
#47090 = EDGE_LOOP ( 'NONE', ( #18256, #34900, #9100, #15901 ) ) ;
#47091 = CARTESIAN_POINT ( 'NONE',  ( -62.00707362346617657, -8.102448949553174629, -5.886773742842741797 ) ) ;
#47092 = ORIENTED_EDGE ( 'NONE', *, *, #1954, .F. ) ;
#47093 = CARTESIAN_POINT ( 'NONE',  ( 20.86636340060661610, 115.0297054428233707, 10.00000000000000000 ) ) ;
#47094 = SURFACE_STYLE_FILL_AREA ( #4459 ) ;
#47096 = VECTOR ( 'NONE', #11013, 1000.000000000000000 ) ;
#47095 = DIRECTION ( 'NONE',  ( -1.000000000000000000, -0.000000000000000000, -0.000000000000000000 ) ) ;
#47097 = CARTESIAN_POINT ( 'NONE',  ( -121.2549999999999812, -4.716976649647092401, 6.492361379858946790 ) ) ;
#47098 = CARTESIAN_POINT ( 'NONE',  ( -184.0000000000000284, -7.203081035975417379, 3.559358198943581630 ) ) ;
#47099 = LINE ( 'NONE', #36193, #46295 ) ;
#47100 = AXIS2_PLACEMENT_3D ( 'NONE', #33744, #42719, #64117 ) ;
#47101 = CARTESIAN_POINT ( 'NONE',  ( -7.499999999999999112, 0.000000000000000000, 0.000000000000000000 ) ) ;
#47102 =( LENGTH_UNIT ( ) NAMED_UNIT ( * ) SI_UNIT ( .MILLI., .METRE. ) );
#47103 = FACE_OUTER_BOUND ( 'NONE', #24370, .T. ) ;
#47104 = LINE ( 'NONE', #14722, #12163 ) ;
#47105 = EDGE_LOOP ( 'NONE', ( #47013, #16168, #13350, #8728 ) ) ;
#47106 = CIRCLE ( 'NONE', #14474, 0.2500000000000002220 ) ;
#47107 = ORIENTED_EDGE ( 'NONE', *, *, #11100, .T. ) ;
#47108 = SURFACE_SIDE_STYLE ('',( #14726 ) ) ;
#47109 = CARTESIAN_POINT ( 'NONE',  ( -75.50000000000000000, 64.49137674618943095, 10.00000000000000000 ) ) ;
#47110 = CARTESIAN_POINT ( 'NONE',  ( -182.6929263765338192, 10.01517768586948698, -1.839758294383808966E-15 ) ) ;
#47111 = CARTESIAN_POINT ( 'NONE',  ( 6.826472737025121695, 114.6070736234661496, -4.959722759717905660 ) ) ;
#47112 = EDGE_LOOP ( 'NONE', ( #14917, #43777, #11977 ) ) ;
#47113 = DIRECTION ( 'NONE',  ( 1.000000000000000000, -0.000000000000000000, 0.000000000000000000 ) ) ;
#47114 = CARTESIAN_POINT ( 'NONE',  ( -181.1049999999999898, -6.826472737025115478, 4.959722759717900331 ) ) ;
#47115 = DIRECTION ( 'NONE',  ( 1.000000000000000000, -0.000000000000000000, -0.000000000000000000 ) ) ;
#47116 =( NAMED_UNIT ( * ) SI_UNIT ( $, .STERADIAN. ) SOLID_ANGLE_UNIT ( ) );
#47117 = CARTESIAN_POINT ( 'NONE',  ( -46.40707362346616094, 3.094860106618428031, -9.524999999999993250 ) ) ;
#47118 = CARTESIAN_POINT ( 'NONE',  ( -173.9949999999999761, -6.826472737025113702, 4.959722759717902107 ) ) ;
#47119 = EDGE_LOOP ( 'NONE', ( #42421, #62674, #29009, #42782 ) ) ;
#47120 = DIRECTION ( 'NONE',  ( 1.000000000000000000, 0.000000000000000000, 0.000000000000000000 ) ) ;
#47121 = CARTESIAN_POINT ( 'NONE',  ( -14.33318179684024862, 10.92439180899981999, 4.966154840202036347 ) ) ;
#47122 = CARTESIAN_POINT ( 'NONE',  ( -94.55499999999999261, 0.000000000000000000, 8.024999999999991473 ) ) ;
#47123 =( NAMED_UNIT ( * ) SI_UNIT ( $, .STERADIAN. ) SOLID_ANGLE_UNIT ( ) );
#47124 = SURFACE_STYLE_USAGE ( .BOTH. , #36919 ) ;
#47125 = COLOUR_RGB ( '', 0.08235294, 0.09019608, 0.10196078) ;
#47126 = CARTESIAN_POINT ( 'NONE',  ( -87.44499999999999318, 0.000000000000000000, 8.024999999999991473 ) ) ;
#47127 = CARTESIAN_POINT ( 'NONE',  ( 3.094860106618431583, 130.2049999999999841, 9.525000000000000355 ) ) ;
#47128 = CARTESIAN_POINT ( 'NONE',  ( -73.19499999999999318, 8.437984349512085203, -1.550032578732815448E-15 ) ) ;
#47129 = CARTESIAN_POINT ( 'NONE',  ( 20.57648123223228254, 114.5810881445910070, -10.27659574468084891 ) ) ;
#47130 = EDGE_CURVE ( 'NONE', #66131, #32455, #68988, .T. ) ;
#47131 = STYLED_ITEM ( 'NONE', ( #16061 ), #20490 ) ;
#47132 = DIRECTION ( 'NONE',  ( -0.000000000000000000, 1.000000000000000000, 0.000000000000000000 ) ) ;
#47133 =( NAMED_UNIT ( * ) PLANE_ANGLE_UNIT ( ) SI_UNIT ( $, .RADIAN. ) );
#47134 = AXIS2_PLACEMENT_3D ( 'NONE', #13177, #55046, #45919 ) ;
#47135 = AXIS2_PLACEMENT_3D ( 'NONE', #59511, #10319, #5349 ) ;
#47136 = ADVANCED_FACE ( 'NONE', ( #38107 ), #2085, .F. ) ;
#47137 = LINE ( 'NONE', #69254, #7936 ) ;
#47138 = CARTESIAN_POINT ( 'NONE',  ( -48.14292637653380780, 5.598654528085800663, -7.705886871421367523 ) ) ;
#47139 = EDGE_CURVE ( 'NONE', #40144, #24888, #66626, .T. ) ;
#47140 = ORIENTED_EDGE ( 'NONE', *, *, #63480, .T. ) ;
#47141 = CARTESIAN_POINT ( 'NONE',  ( -103.0429263765337993, -9.058813317711329915, -2.943386871421370898 ) ) ;
#47142 =( BOUNDED_CURVE ( )  B_SPLINE_CURVE ( 2, ( #18265, #61171, #34439, #2732, #41140, #42208, #68196, #47474, #20696, #19281, #40787 ),
 .UNSPECIFIED., .F., .F. ) 
 B_SPLINE_CURVE_WITH_KNOTS ( ( 3, 2, 2, 2, 2, 3 ),
 ( 0.6739130434782448775, 0.6760869565217263455, 0.6782608695652078135, 0.6804347826086891704, 0.6826086956521706384, 0.6847826086956522174 ),
 .UNSPECIFIED. ) 
 CURVE ( )  GEOMETRIC_REPRESENTATION_ITEM ( )  RATIONAL_B_SPLINE_CURVE ( ( 1.000000000000359934, 0.9510565162947935969, 1.000000000000000000, 0.9510565162951535312, 1.000000000000000000, 0.9510565162951535312, 1.000000000000000000, 0.9510565162951535312, 1.000000000000000000, 0.9510565162951535312, 1.000000000000000000 ) ) 
 REPRESENTATION_ITEM ( '' )  );
#47143 = CARTESIAN_POINT ( 'NONE',  ( -130.7950000000000159, 2.607480562269068880, -8.024999999999993250 ) ) ;
#47144 = CIRCLE ( 'NONE', #33636, 14.49999999999999822 ) ;
#47145 = ADVANCED_FACE ( 'NONE', ( #6052 ), #17675, .F. ) ;
#47146 = EDGE_CURVE ( 'NONE', #5542, #56654, #3139, .T. ) ;
#47147 = FILL_AREA_STYLE ('',( #9493 ) ) ;
#47148 = ADVANCED_FACE ( 'NONE', ( #51753 ), #29649, .T. ) ;
#47150 = SPHERICAL_SURFACE ( 'NONE', #31470, 7.499999999999992895 ) ;
#47149 = CARTESIAN_POINT ( 'NONE',  ( -43.99999999999999289, 1.166476076187854022E-15, -9.525000000000000355 ) ) ;
#47151 = ORIENTED_EDGE ( 'NONE', *, *, #4023, .F. ) ;
#47152 = COLOUR_RGB ( '', 0.08235294, 0.09019608, 0.10196078) ;
#47153 = VERTEX_POINT ( 'NONE', #23959 ) ;
#47154 = CARTESIAN_POINT ( 'NONE',  ( 2.607480562269034241, 131.7929263765337851, -8.025000000000032330 ) ) ;
#47155 = CIRCLE ( 'NONE', #16809, 0.2500000000000002220 ) ;
#47156 = EDGE_CURVE ( 'NONE', #34517, #38501, #51392, .T. ) ;
#47157 = CARTESIAN_POINT ( 'NONE',  ( -6.826472737025120807, 147.9929263765338305, 4.959722759717906548 ) ) ;
#47158 = DIRECTION ( 'NONE',  ( -1.000000000000000000, -0.000000000000000000, -0.000000000000000000 ) ) ;
#47159 = STYLED_ITEM ( 'NONE', ( #49775 ), #68785 ) ;
#47160 = FILL_AREA_STYLE_COLOUR ( '', #42133 ) ;
#47161 = FACE_OUTER_BOUND ( 'NONE', #30805, .T. ) ;
#47162 = ORIENTED_EDGE ( 'NONE', *, *, #19838, .T. ) ;
#47163 = CARTESIAN_POINT ( 'NONE',  ( -123.0549999999999926, -9.827790563157499189E-16, -8.024999999999991473 ) ) ;
#47164 = ORIENTED_EDGE ( 'NONE', *, *, #29335, .F. ) ;
#47165 = SURFACE_STYLE_USAGE ( .BOTH. , #63642 ) ;
#47166 = CARTESIAN_POINT ( 'NONE',  ( -122.9070736234661609, -3.094860106618429807, 9.524999999999991473 ) ) ;
#47167 = EDGE_LOOP ( 'NONE', ( #27104, #51178, #48402, #28403 ) ) ;
#47168 = SURFACE_SIDE_STYLE ('',( #26344 ) ) ;
#47169 = CARTESIAN_POINT ( 'NONE',  ( 22.25000000000000711, 33.74999999999999289, -3.750000000000000000 ) ) ;
#47170 = ORIENTED_EDGE ( 'NONE', *, *, #39579, .T. ) ;
#47172 = DIRECTION ( 'NONE',  ( 0.000000000000000000, 0.000000000000000000, -1.000000000000000000 ) ) ;
#47171 = COLOUR_RGB ( '', 0.66274510, 0.83137255, 0.94901961) ;
#47173 = CARTESIAN_POINT ( 'NONE',  ( 5.598654528085805993, 153.2450000000000045, 7.705886871421374629 ) ) ;
#47174 = PRESENTATION_STYLE_ASSIGNMENT (( #9520 ) ) ;
#47175 = ORIENTED_EDGE ( 'NONE', *, *, #6042, .F. ) ;
#47176 = CARTESIAN_POINT ( 'NONE',  ( 5.598654528085805993, 151.3549999999999898, 7.705886871421374629 ) ) ;
#47177 = CARTESIAN_POINT ( 'NONE',  ( 31.00000000000000000, 43.00000000000000000, -75.00000000000001421 ) ) ;
#47178 = AXIS2_PLACEMENT_3D ( 'NONE', #44873, #30714, #57113 ) ;
#47179 = CARTESIAN_POINT ( 'NONE',  ( 21.25000000000001066, 24.74999999999998224, -3.750000000000000000 ) ) ;
#47180 = VERTEX_POINT ( 'NONE', #67571 ) ;
#47181 = CARTESIAN_POINT ( 'NONE',  ( -9.827790563157511022E-16, 127.4429263765338192, 8.025000000000000355 ) ) ;
#47182 = DIRECTION ( 'NONE',  ( -1.000000000000000000, 0.000000000000000000, 0.000000000000000000 ) ) ;
#47183 = CARTESIAN_POINT ( 'NONE',  ( -47.30707362346616662, -10.01517768586948698, 6.132527647946031529E-16 ) ) ;
#47184 = DIRECTION ( 'NONE',  ( -0.000000000000000000, 0.000000000000000000, -1.000000000000000000 ) ) ;
#47185 = AXIS2_PLACEMENT_3D ( 'NONE', #60904, #66184, #60230 ) ;
#47186 = CYLINDRICAL_SURFACE ( 'NONE', #54192, 0.2500000000000002220 ) ;
#47187 = ORIENTED_EDGE ( 'NONE', *, *, #53824, .F. ) ;
#47188 = DIRECTION ( 'NONE',  ( 0.000000000000000000, 0.000000000000000000, 1.000000000000000000 ) ) ;
#47189 = ORIENTED_EDGE ( 'NONE', *, *, #1638, .T. ) ;
#47190 = CARTESIAN_POINT ( 'NONE',  ( -60.44292637653379785, -1.166476076187852838E-15, -9.524999999999991473 ) ) ;
#47191 = CIRCLE ( 'NONE', #59470, 0.5000000000000004441 ) ;
#47192 = DIRECTION ( 'NONE',  ( 0.000000000000000000, 0.000000000000000000, 1.000000000000000000 ) ) ;
#47193 = CARTESIAN_POINT ( 'NONE',  ( 8.000000000000030198, 5.000000000000000000, -29.00402776293826079 ) ) ;
#47194 = CARTESIAN_POINT ( 'NONE',  ( -152.9049999999999727, 2.607480562269068880, -8.024999999999993250 ) ) ;
#47195 = ORIENTED_EDGE ( 'NONE', *, *, #26508, .T. ) ;
#47196 = CIRCLE ( 'NONE', #66915, 1.000000000000000888 ) ;
#47197 = EDGE_CURVE ( 'NONE', #2776, #4654, #47694, .T. ) ;
#47198 = MECHANICAL_DESIGN_GEOMETRIC_PRESENTATION_REPRESENTATION (  '', ( #42671 ), #44782 ) ;
#47199 = CARTESIAN_POINT ( 'NONE',  ( -56.46916883648585639, -8.499999999999998224, 7.024140319044985148 ) ) ;
#47200 = FACE_OUTER_BOUND ( 'NONE', #9357, .T. ) ;
#47201 = DIRECTION ( 'NONE',  ( 0.000000000000000000, 0.000000000000000000, 1.000000000000000000 ) ) ;
#47202 = ORIENTED_EDGE ( 'NONE', *, *, #32971, .F. ) ;
#47203 = AXIS2_PLACEMENT_3D ( 'NONE', #61107, #55828, #41076 ) ;
#47204 = ORIENTED_EDGE ( 'NONE', *, *, #44364, .T. ) ;
#47205 = DIRECTION ( 'NONE',  ( 1.000000000000000000, 0.000000000000000000, 0.000000000000000000 ) ) ;
#47206 =( NAMED_UNIT ( * ) SI_UNIT ( $, .STERADIAN. ) SOLID_ANGLE_UNIT ( ) );
#47207 = CARTESIAN_POINT ( 'NONE',  ( -65.90499999999998693, 2.607480562269068880, -8.024999999999993250 ) ) ;
#47208 = ORIENTED_EDGE ( 'NONE', *, *, #6646, .T. ) ;
#47209 = DIRECTION ( 'NONE',  ( 0.000000000000000000, 1.000000000000000000, 0.000000000000000000 ) ) ;
#47210 = CARTESIAN_POINT ( 'NONE',  ( 34.99999999999992895, 113.4999999999999858, 7.000000000000000000 ) ) ;
#47211 = AXIS2_PLACEMENT_3D ( 'NONE', #18375, #11695, #33832 ) ;
#47212 = CARTESIAN_POINT ( 'NONE',  ( -124.1929263765338192, -10.01517768586948698, 6.132527647946031529E-16 ) ) ;
#47213 = DIRECTION ( 'NONE',  ( -1.000000000000000000, 0.000000000000000000, 0.000000000000000000 ) ) ;
#47214 = ORIENTED_EDGE ( 'NONE', *, *, #69423, .T. ) ;
#47215 = CARTESIAN_POINT ( 'NONE',  ( -74.09163092349538715, 9.403269179647930187, -6.097839204891418063 ) ) ;
#47216 = LINE ( 'NONE', #64032, #18055 ) ;
#47217 = DIRECTION ( 'NONE',  ( 0.7071067811865426878, 8.659560562354873694E-17, -0.7071067811865524577 ) ) ;
#47218 = VECTOR ( 'NONE', #57645, 1000.000000000000000 ) ;
#47219 = DIRECTION ( 'NONE',  ( 0.000000000000000000, -0.000000000000000000, -1.000000000000000000 ) ) ;
#47220 = ADVANCED_FACE ( 'NONE', ( #61567 ), #35572, .F. ) ;
#47221 = CARTESIAN_POINT ( 'NONE',  ( 3.094860106618435136, 145.2949999999999875, -9.525000000000000355 ) ) ;
#47222 = CARTESIAN_POINT ( 'NONE',  ( -95.39499999999999602, -6.826472737025115478, -4.959722759717899443 ) ) ;
#47223 = FILL_AREA_STYLE ('',( #25702 ) ) ;
#47224 = DIRECTION ( 'NONE',  ( 0.000000000000000000, 0.000000000000000000, -1.000000000000000000 ) ) ;
#47225 = PRESENTATION_LAYER_ASSIGNMENT (  '', '', ( #16869 ) ) ;
#47226 = EDGE_CURVE ( 'NONE', #2089, #29559, #52128, .T. ) ;
#47227 = CARTESIAN_POINT ( 'NONE',  ( 0.000000000000000000, 0.000000000000000000, -2.000000000000000000 ) ) ;
#47229 = EDGE_LOOP ( 'NONE', ( #1850, #13477, #60429, #1412 ) ) ;
#47228 = VECTOR ( 'NONE', #36680, 1000.000000000000114 ) ;
#47230 = CARTESIAN_POINT ( 'NONE',  ( -130.6429263765338078, -5.598654528085801552, 7.705886871421367523 ) ) ;
#47231 = PRESENTATION_STYLE_ASSIGNMENT (( #10258 ) ) ;
#47232 = DIRECTION ( 'NONE',  ( 0.000000000000000000, 1.000000000000000000, 0.000000000000000000 ) ) ;
#47233 = CARTESIAN_POINT ( 'NONE',  ( -161.2450000000000045, -4.716976649647093289, -6.492361379858945902 ) ) ;
#47234 = DIRECTION ( 'NONE',  ( 1.000000000000000000, 0.000000000000000000, 0.000000000000000000 ) ) ;
#47235 = CARTESIAN_POINT ( 'NONE',  ( -51.14292637653380780, 5.598654528085800663, -7.705886871421367523 ) ) ;
#47236 = EDGE_CURVE ( 'NONE', #64181, #35564, #61068, .T. ) ;
#47237 = CARTESIAN_POINT ( 'NONE',  ( 179.4361977533490347, 13.00000000000000178, -103.7004518695263044 ) ) ;
#47238 = STYLED_ITEM ( 'NONE', ( #15526 ), #11186 ) ;
#47239 = EDGE_LOOP ( 'NONE', ( #6791, #45829, #12684, #44138 ) ) ;
#47240 = PRESENTATION_STYLE_ASSIGNMENT (( #42914 ) ) ;
#47241 = VERTEX_POINT ( 'NONE', #15515 ) ;
#47242 = CARTESIAN_POINT ( 'NONE',  ( -70.94292637653380496, 0.000000000000000000, 9.524999999999991473 ) ) ;
#47244 = ADVANCED_FACE ( 'NONE', ( #20053 ), #48226, .F. ) ;
#47243 = AXIS2_PLACEMENT_3D ( 'NONE', #13606, #67085, #35070 ) ;
#47245 = CARTESIAN_POINT ( 'NONE',  ( 0.000000000000000000, 30.74999999999998579, 3.750000000000000000 ) ) ;
#47246 = CARTESIAN_POINT ( 'NONE',  ( -45.00000000000000000, 9.657020704707438341, 6.241538579429709799 ) ) ;
#47247 = CARTESIAN_POINT ( 'NONE',  ( -9.250000000000003553, 27.74999999999998934, -3.750000000000000000 ) ) ;
#47248 = CIRCLE ( 'NONE', #32562, 13.99999999999999822 ) ;
#47249 = SURFACE_STYLE_FILL_AREA ( #42655 ) ;
#47250 = ORIENTED_EDGE ( 'NONE', *, *, #40763, .T. ) ;
#47251 = CARTESIAN_POINT ( 'NONE',  ( -150.6549999999999727, -7.632228543268600340, -2.479861379858950166 ) ) ;
#47252 = EDGE_LOOP ( 'NONE', ( #48398, #44662, #40852, #12351, #20100, #46296, #27523, #24146, #43326, #6014, #38088, #440, #39188 ) ) ;
#47253 = CARTESIAN_POINT ( 'NONE',  ( -4.750000000000002665, 24.74999999999998579, -4.000000000000000000 ) ) ;
#47254 = ORIENTED_EDGE ( 'NONE', *, *, #64121, .T. ) ;
#47255 = MECHANICAL_DESIGN_GEOMETRIC_PRESENTATION_REPRESENTATION (  '', ( #22511 ), #21383 ) ;
#47256 =( GEOMETRIC_REPRESENTATION_CONTEXT ( 3 ) GLOBAL_UNCERTAINTY_ASSIGNED_CONTEXT ( ( #54491 ) ) GLOBAL_UNIT_ASSIGNED_CONTEXT ( ( #15115, #47487, #4494 ) ) REPRESENTATION_CONTEXT ( 'NONE', 'WORKASPACE' ) );
#47257 = CARTESIAN_POINT ( 'NONE',  ( 26.00000000000001066, 19.24999999999997868, 3.750000000000000000 ) ) ;
#47258 = DIRECTION ( 'NONE',  ( -0.000000000000000000, -1.000000000000000000, -0.000000000000000000 ) ) ;
#47259 = CARTESIAN_POINT ( 'NONE',  ( 0.000000000000000000, 121.4449999999999790, -9.525000000000000355 ) ) ;
#47260 =( GEOMETRIC_REPRESENTATION_CONTEXT ( 3 ) GLOBAL_UNCERTAINTY_ASSIGNED_CONTEXT ( ( #44556 ) ) GLOBAL_UNIT_ASSIGNED_CONTEXT ( ( #27433, #28470, #6679 ) ) REPRESENTATION_CONTEXT ( 'NONE', 'WORKASPACE' ) );
#47261 = VERTEX_POINT ( 'NONE', #42286 ) ;
#47262 = CARTESIAN_POINT ( 'NONE',  ( 0.000000000000000000, 122.5549999999999784, -9.525000000000000355 ) ) ;
#47263 = CARTESIAN_POINT ( 'NONE',  ( -67.40499999999997272, -2.607480562269069768, 8.024999999999991473 ) ) ;
#47264 = DIRECTION ( 'NONE',  ( 0.9704308468600219006, -0.2413793103448194366, 0.000000000000000000 ) ) ;
#47265 = EDGE_LOOP ( 'NONE', ( #59078, #41321, #68426, #35977 ) ) ;
#47266 = CARTESIAN_POINT ( 'NONE',  ( 10.01517768586949231, 148.8050000000000068, 1.839758294383810543E-15 ) ) ;
#47267 = CIRCLE ( 'NONE', #58469, 9.499999999999998224 ) ;
#47268 = LINE ( 'NONE', #46928, #32203 ) ;
#47269 = CARTESIAN_POINT ( 'NONE',  ( 9.250000000000003553, 27.74999999999998934, 3.750000000000000000 ) ) ;
#47270 = SURFACE_STYLE_USAGE ( .BOTH. , #41629 ) ;
#47271 = ADVANCED_BREP_SHAPE_REPRESENTATION ( '', ( #50161, #42840 ), #24690 ) ;
#47272 = DIRECTION ( 'NONE',  ( 0.000000000000000000, -1.000000000000000000, 0.000000000000000000 ) ) ;
#47273 = VERTEX_POINT ( 'NONE', #57715 ) ;
#47274 = DIRECTION ( 'NONE',  ( -0.000000000000000000, -0.000000000000000000, -1.000000000000000000 ) ) ;
#47275 = DIRECTION ( 'NONE',  ( -1.000000000000000000, 0.000000000000000000, 0.000000000000000000 ) ) ;
#47276 = CARTESIAN_POINT ( 'NONE',  ( -180.2049999999999841, -2.607480562269071545, -8.024999999999991473 ) ) ;
#47277 = ORIENTED_EDGE ( 'NONE', *, *, #39354, .T. ) ;
#47278 = CARTESIAN_POINT ( 'NONE',  ( 4.559337023122163046, 111.8214503647300688, -6.825287955804331119 ) ) ;
#47279 =( BOUNDED_CURVE ( )  B_SPLINE_CURVE ( 2, ( #40074, #61462, #24191, #61805, #35099, #29819, #52682, #24880, #41109, #20667, #57962 ),
 .UNSPECIFIED., .F., .F. ) 
 B_SPLINE_CURVE_WITH_KNOTS ( ( 3, 2, 2, 2, 2, 3 ),
 ( 0.9456521739130434590, 0.9478260869565217073, 0.9499999999999999556, 0.9521739130434783149, 0.9543478260869565633, 0.9565217391304348116 ),
 .UNSPECIFIED. ) 
 CURVE ( )  GEOMETRIC_REPRESENTATION_ITEM ( )  RATIONAL_B_SPLINE_CURVE ( ( 1.000000000000000000, 0.9510565162951535312, 1.000000000000000000, 0.9510565162951535312, 1.000000000000000000, 0.9510565162951535312, 1.000000000000000000, 0.9510565162951535312, 1.000000000000000000, 0.9510565162951535312, 1.000000000000000000 ) ) 
 REPRESENTATION_ITEM ( '' )  );
#47280 = EDGE_CURVE ( 'NONE', #12316, #9058, #36651, .T. ) ;
#47281 = SURFACE_STYLE_FILL_AREA ( #37433 ) ;
#47282 = VERTEX_POINT ( 'NONE', #37689 ) ;
#47283 = DIRECTION ( 'NONE',  ( 0.000000000000000000, 0.000000000000000000, -1.000000000000000000 ) ) ;
#47284 = VERTEX_POINT ( 'NONE', #68619 ) ;
#47285 = CARTESIAN_POINT ( 'NONE',  ( -94.70499999999999829, 2.607480562269073321, 8.024999999999991473 ) ) ;
#47286 = ORIENTED_EDGE ( 'NONE', *, *, #45847, .F. ) ;
#47287 = FACE_OUTER_BOUND ( 'NONE', #7512, .T. ) ;
#47288 = CIRCLE ( 'NONE', #49514, 0.5000000000000003331 ) ;
#47289 = CARTESIAN_POINT ( 'NONE',  ( -129.0570736234661808, 0.000000000000000000, 9.524999999999991473 ) ) ;
#47290 = STYLED_ITEM ( 'NONE', ( #4887 ), #34548 ) ;
#47291 = CARTESIAN_POINT ( 'NONE',  ( 7.999999999999989342, 5.000000000000000000, 37.00402776293825724 ) ) ;
#47292 = CARTESIAN_POINT ( 'NONE',  ( -9.058813317711338797, 152.3449999999999704, 2.943386871421373563 ) ) ;
#47293 = CARTESIAN_POINT ( 'NONE',  ( -74.75707362346616947, -5.598654528085801552, 7.705886871421367523 ) ) ;
#47294 = EDGE_CURVE ( 'NONE', #52329, #62435, #45417, .T. ) ;
#47295 = CIRCLE ( 'NONE', #13393, 0.2500000000000002220 ) ;
#47296 = CARTESIAN_POINT ( 'NONE',  ( -92.24292637653380211, 5.598654528085804216, 7.705886871421366635 ) ) ;
#47297 = ORIENTED_EDGE ( 'NONE', *, *, #4270, .F. ) ;
#47298 = DIRECTION ( 'NONE',  ( -1.000000000000000000, 0.000000000000000000, 0.000000000000000000 ) ) ;
#47299 =( GEOMETRIC_REPRESENTATION_CONTEXT ( 3 ) GLOBAL_UNCERTAINTY_ASSIGNED_CONTEXT ( ( #58777 ) ) GLOBAL_UNIT_ASSIGNED_CONTEXT ( ( #24762, #7907, #56806 ) ) REPRESENTATION_CONTEXT ( 'NONE', 'WORKASPACE' ) );
#47300 = CARTESIAN_POINT ( 'NONE',  ( -19.74219527431328203, -11.89431361296820988, -1.618896920497846059 ) ) ;
#47301 = SURFACE_STYLE_USAGE ( .BOTH. , #51488 ) ;
#47302 = EDGE_CURVE ( 'NONE', #63225, #21587, #21388, .T. ) ;
#47303 = CARTESIAN_POINT ( 'NONE',  ( -108.9549999999999983, -7.632228543268599452, 2.479861379858951054 ) ) ;
#47304 = EDGE_CURVE ( 'NONE', #42967, #12357, #31298, .T. ) ;
#47305 =( LENGTH_UNIT ( ) NAMED_UNIT ( * ) SI_UNIT ( .MILLI., .METRE. ) );
#47306 = CARTESIAN_POINT ( 'NONE',  ( 3.094860106618435136, 118.2949999999999875, -9.525000000000000355 ) ) ;
#47307 = CARTESIAN_POINT ( 'NONE',  ( -125.5449999999999875, -7.632228543268600340, -2.479861379858950166 ) ) ;
#47308 = AXIS2_PLACEMENT_3D ( 'NONE', #18244, #35112, #19260 ) ;
#47309 = CARTESIAN_POINT ( 'NONE',  ( 15.98999599679679839, 146.4999999999999716, -7.000000000000000000 ) ) ;
#47310 = MECHANICAL_DESIGN_GEOMETRIC_PRESENTATION_REPRESENTATION (  '', ( #13503 ), #25859 ) ;
#47311 =( NAMED_UNIT ( * ) PLANE_ANGLE_UNIT ( ) SI_UNIT ( $, .RADIAN. ) );
#47312 = AXIS2_PLACEMENT_3D ( 'NONE', #43523, #48442, #64908 ) ;
#47313 = EDGE_CURVE ( 'NONE', #35681, #44244, #63330, .T. ) ;
#47314 = ORIENTED_EDGE ( 'NONE', *, *, #8626, .F. ) ;
#47315 = CARTESIAN_POINT ( 'NONE',  ( -165.1429263765338078, 5.598654528085800663, -7.705886871421367523 ) ) ;
#47316 = CARTESIAN_POINT ( 'NONE',  ( 33.00000000000000000, 15.00000000000000000, -80.00402776293826435 ) ) ;
#47317 = EDGE_CURVE ( 'NONE', #2677, #10181, #32862, .T. ) ;
#47318 = B_SPLINE_CURVE_WITH_KNOTS ( 'NONE', 3,
 ( #47414, #31162, #25543, #61205, #25894, #50317, #57939, #28835 ),
 .UNSPECIFIED., .F., .F.,
 ( 4, 2, 2, 4 ),
 ( 3.510295945092028624E-18, 0.001616916654929161177, 0.002425374982393735043, 0.003233833309858308910 ),
 .UNSPECIFIED. ) ;
#47319 = EDGE_CURVE ( 'NONE', #26109, #50403, #5879, .T. ) ;
#47320 = CARTESIAN_POINT ( 'NONE',  ( -159.0570736234661808, 0.000000000000000000, 9.524999999999991473 ) ) ;
#47321 = EDGE_LOOP ( 'NONE', ( #33352, #37040, #40429, #34853 ) ) ;
#47322 = AXIS2_PLACEMENT_3D ( 'NONE', #58876, #18868, #35067 ) ;
#47323 = CARTESIAN_POINT ( 'NONE',  ( -90.44292637653379074, -1.166476076187852838E-15, -9.524999999999991473 ) ) ;
#47324 = CYLINDRICAL_SURFACE ( 'NONE', #3708, 9.524999999999991473 ) ;
#47325 = DIRECTION ( 'NONE',  ( -1.000000000000000000, 0.000000000000000000, 0.000000000000000000 ) ) ;
#47326 = VECTOR ( 'NONE', #21040, 1000.000000000000000 ) ;
#47327 = EDGE_CURVE ( 'NONE', #69071, #24587, #2473, .T. ) ;
#47328 = CYLINDRICAL_SURFACE ( 'NONE', #8938, 110.0000000000000142 ) ;
#47329 = TOROIDAL_SURFACE ( 'NONE', #19191, 4.000000000000000000, 1.000000000000000000 ) ;
#47330 = CARTESIAN_POINT ( 'NONE',  ( -183.9772050269406236, -7.512949680700584665, 2.846963971517519010 ) ) ;
#47331 = ORIENTED_EDGE ( 'NONE', *, *, #2402, .F. ) ;
#47332 = PRESENTATION_STYLE_ASSIGNMENT (( #51519 ) ) ;
#47333 = CIRCLE ( 'NONE', #56260, 0.2500000000000002220 ) ;
#47334 = DIRECTION ( 'NONE',  ( 1.000000000000000000, -0.000000000000000000, 0.000000000000000000 ) ) ;
#47335 = EDGE_LOOP ( 'NONE', ( #12958, #49394, #46496, #21818 ) ) ;
#47336 = CARTESIAN_POINT ( 'NONE',  ( -110.3929263765337936, 8.102448949553176405, 5.886773742842740909 ) ) ;
#47337 = CARTESIAN_POINT ( 'NONE',  ( -4.716976649647098618, 143.2570736234661410, 6.492361379858953008 ) ) ;
#47338 = FACE_OUTER_BOUND ( 'NONE', #25247, .T. ) ;
#47339 = AXIS2_PLACEMENT_3D ( 'NONE', #57759, #5904, #22102 ) ;
#47340 = VERTEX_POINT ( 'NONE', #69310 ) ;
#47341 = CARTESIAN_POINT ( 'NONE',  ( 82.09357085539578236, 5.000000000000000000, 32.00402776293825724 ) ) ;
#47342 = CARTESIAN_POINT ( 'NONE',  ( -104.3049999999999784, 8.437984349512086979, -1.550032578732815448E-15 ) ) ;
#47343 =( GEOMETRIC_REPRESENTATION_CONTEXT ( 3 ) GLOBAL_UNCERTAINTY_ASSIGNED_CONTEXT ( ( #25029 ) ) GLOBAL_UNIT_ASSIGNED_CONTEXT ( ( #51102, #66576, #24006 ) ) REPRESENTATION_CONTEXT ( 'NONE', 'WORKASPACE' ) );
#47344 = PRESENTATION_STYLE_ASSIGNMENT (( #25831 ) ) ;
#47345 = ORIENTED_EDGE ( 'NONE', *, *, #26438, .F. ) ;
#47346 = CARTESIAN_POINT ( 'NONE',  ( -38.85043651514852314, -13.12913046416487539, 1.005512611032779891 ) ) ;
#47347 = FACE_OUTER_BOUND ( 'NONE', #1796, .T. ) ;
#47348 = STYLED_ITEM ( 'NONE', ( #34748 ), #17817 ) ;
#47349 = ORIENTED_EDGE ( 'NONE', *, *, #22959, .F. ) ;
#47350 = DIRECTION ( 'NONE',  ( 0.000000000000000000, 0.000000000000000000, -1.000000000000000000 ) ) ;
#47351 = CARTESIAN_POINT ( 'NONE',  ( -71.54499999999998749, -7.632228543268600340, -2.479861379858950166 ) ) ;
#47352 = ORIENTED_EDGE ( 'NONE', *, *, #12836, .T. ) ;
#47353 = B_SPLINE_CURVE_WITH_KNOTS ( 'NONE', 3,
 ( #21401, #58030, #37293, #41512, #47510, #47870, #63965, #4883, #62921, #68928, #5217, #9837 ),
 .UNSPECIFIED., .F., .F.,
 ( 4, 2, 2, 2, 2, 4 ),
 ( 0.000000000000000000, 0.0009390420820170817780, 0.001408563123025622721, 0.001643323643529895524, 0.001760703903782034853, 0.001878084164034174398 ),
 .UNSPECIFIED. ) ;
#47354 = DIRECTION ( 'NONE',  ( 0.000000000000000000, 0.000000000000000000, -1.000000000000000000 ) ) ;
#47355 = CARTESIAN_POINT ( 'NONE',  ( -120.5070736234661553, 8.102448949553176405, 5.886773742842740909 ) ) ;
#47356 = CARTESIAN_POINT ( 'NONE',  ( -125.7570736234661695, -5.598654528085801552, 7.705886871421367523 ) ) ;
#47357 = ORIENTED_EDGE ( 'NONE', *, *, #43792, .T. ) ;
#47358 = DIRECTION ( 'NONE',  ( 0.000000000000000000, 0.000000000000000000, -1.000000000000000000 ) ) ;
#47359 = CARTESIAN_POINT ( 'NONE',  ( -175.9429263765337907, 0.000000000000000000, 9.524999999999991473 ) ) ;
#47360 =( GEOMETRIC_REPRESENTATION_CONTEXT ( 3 ) GLOBAL_UNCERTAINTY_ASSIGNED_CONTEXT ( ( #67081 ) ) GLOBAL_UNIT_ASSIGNED_CONTEXT ( ( #48697, #53582, #43084 ) ) REPRESENTATION_CONTEXT ( 'NONE', 'WORKASPACE' ) );
#47361 = FILL_AREA_STYLE_COLOUR ( '', #12303 ) ;
#47362 = ORIENTED_EDGE ( 'NONE', *, *, #14068, .T. ) ;
#47363 = DIRECTION ( 'NONE',  ( 0.000000000000000000, 0.000000000000000000, -1.000000000000000000 ) ) ;
#47364 = EDGE_LOOP ( 'NONE', ( #47362, #30636, #26278, #40406 ) ) ;
#47365 = DIRECTION ( 'NONE',  ( 0.000000000000000000, 0.000000000000000000, -1.000000000000000000 ) ) ;
#47366 = LINE ( 'NONE', #51558, #11686 ) ;
#47367 = DIRECTION ( 'NONE',  ( 0.000000000000000000, 0.000000000000000000, -1.000000000000000000 ) ) ;
#47368 = CARTESIAN_POINT ( 'NONE',  ( -158.7570736234661979, -5.598654528085801552, 7.705886871421367523 ) ) ;
#47369 = CARTESIAN_POINT ( 'NONE',  ( 8.102448949553181734, 120.9949999999999761, -5.886773742842746238 ) ) ;
#47370 = CARTESIAN_POINT ( 'NONE',  ( -99.80707362346616662, 10.01517768586948698, -1.839758294383808571E-15 ) ) ;
#47371 = AXIS2_PLACEMENT_3D ( 'NONE', #60006, #7248, #11815 ) ;
#47372 = EDGE_CURVE ( 'NONE', #373, #20601, #59819, .T. ) ;
#47373 = CARTESIAN_POINT ( 'NONE',  ( 6.826472737025121695, 113.4929263765338021, -4.959722759717905660 ) ) ;
#47374 = DIRECTION ( 'NONE',  ( -1.156482317317873451E-16, -1.000000000000000000, 0.000000000000000000 ) ) ;
#47375 = PRODUCT ( '2. Support', '2. Support', '', ( #62049 ) ) ;
#47376 = ORIENTED_EDGE ( 'NONE', *, *, #42705, .F. ) ;
#47377 = CYLINDRICAL_SURFACE ( 'NONE', #3622, 9.524999999999991473 ) ;
#47378 = EDGE_CURVE ( 'NONE', #68529, #29481, #21655, .T. ) ;
#47381 =( GEOMETRIC_REPRESENTATION_CONTEXT ( 3 ) GLOBAL_UNCERTAINTY_ASSIGNED_CONTEXT ( ( #46145 ) ) GLOBAL_UNIT_ASSIGNED_CONTEXT ( ( #5873, #870, #24061 ) ) REPRESENTATION_CONTEXT ( 'NONE', 'WORKASPACE' ) );
#47380 = SURFACE_SIDE_STYLE ('',( #36106 ) ) ;
#47379 = DIRECTION ( 'NONE',  ( 0.000000000000000000, -1.000000000000000000, 0.000000000000000000 ) ) ;
#47382 = CARTESIAN_POINT ( 'NONE',  ( -60.00000000000000000, -2.024042244987997205E-14, 6.500000000000000000 ) ) ;
#47383 = ADVANCED_FACE ( 'NONE', ( #42605 ), #36294, .F. ) ;
#47384 = CARTESIAN_POINT ( 'NONE',  ( -144.2050000000000125, -2.607480562269071545, -8.024999999999991473 ) ) ;
#47385 = CARTESIAN_POINT ( 'NONE',  ( 71.99999999999998579, 119.9999999999997868, -7.000000000000000000 ) ) ;
#47386 = SPHERICAL_SURFACE ( 'NONE', #33651, 0.2500000000000000000 ) ;
#47387 = MECHANICAL_DESIGN_GEOMETRIC_PRESENTATION_REPRESENTATION (  '', ( #24872 ), #15940 ) ;
#47388 = CARTESIAN_POINT ( 'NONE',  ( -151.1950000000000216, 8.437984349512085203, -1.550032578732815448E-15 ) ) ;
#47389 = CARTESIAN_POINT ( 'NONE',  ( -135.7450000000000045, 4.716976649647094177, 6.492361379858945902 ) ) ;
#47390 = CONICAL_SURFACE ( 'NONE', #2320, 5.000000000000004441, 0.7853981633974587151 ) ;
#47391 = ORIENTED_EDGE ( 'NONE', *, *, #19114, .T. ) ;
#47392 = MECHANICAL_DESIGN_GEOMETRIC_PRESENTATION_REPRESENTATION (  '', ( #50718 ), #17043 ) ;
#47393 = DIRECTION ( 'NONE',  ( -0.000000000000000000, -0.000000000000000000, 1.000000000000000000 ) ) ;
#47394 = CARTESIAN_POINT ( 'NONE',  ( 57.74999999999998579, 30.74999999999999289, 3.750000000000000000 ) ) ;
#47395 = UNCERTAINTY_MEASURE_WITH_UNIT (LENGTH_MEASURE( 1.000000000000000082E-05 ), #51445, 'distance_accuracy_value', 'NONE');
#47396 = CARTESIAN_POINT ( 'NONE',  ( -50.60499999999996845, 6.826472737025113702, -4.959722759717902107 ) ) ;
#47397 = CARTESIAN_POINT ( 'NONE',  ( -39.43665073983763136, -13.33375354601735552, 0.9443502740340453672 ) ) ;
#47398 = EDGE_CURVE ( 'NONE', #9325, #61370, #4062, .T. ) ;
#47399 = CARTESIAN_POINT ( 'NONE',  ( -1.166476076187854022E-15, 157.0550000000000068, 9.525000000000000355 ) ) ;
#47400 = CARTESIAN_POINT ( 'NONE',  ( -195.0000000000000000, 0.000000000000000000, 0.000000000000000000 ) ) ;
#47401 = CARTESIAN_POINT ( 'NONE',  ( 0.000000000000000000, -3.000000000000000000, 18.00000000000000000 ) ) ;
#47402 = COLOUR_RGB ( '', 0.08235294, 0.09019608, 0.10196078) ;
#47403 = B_SPLINE_CURVE_WITH_KNOTS ( 'NONE', 3,
 ( #55897, #12627, #1331, #50624, #34094, #39071, #7372, #2007 ),
 .UNSPECIFIED., .F., .F.,
 ( 4, 2, 2, 4 ),
 ( 0.01132179082380021552, 0.01341090848792873130, 0.01445546731999298833, 0.01550002615205724535 ),
 .UNSPECIFIED. ) ;
#47404 =( NAMED_UNIT ( * ) PLANE_ANGLE_UNIT ( ) SI_UNIT ( $, .RADIAN. ) );
#47405 = UNCERTAINTY_MEASURE_WITH_UNIT (LENGTH_MEASURE( 1.000000000000000082E-05 ), #61763, 'distance_accuracy_value', 'NONE');
#47406 = AXIS2_PLACEMENT_3D ( 'NONE', #15312, #4707, #47325 ) ;
#47407 = SURFACE_SIDE_STYLE ('',( #25887 ) ) ;
#47408 = PRESENTATION_LAYER_ASSIGNMENT (  '', '', ( #44042 ) ) ;
#47409 = CARTESIAN_POINT ( 'NONE',  ( -89.60707362346616378, -8.102448949553174629, 5.886773742842742685 ) ) ;
#47410 = DIRECTION ( 'NONE',  ( 0.000000000000000000, 0.000000000000000000, -1.000000000000000000 ) ) ;
#47411 = STYLED_ITEM ( 'NONE', ( #5599 ), #28116 ) ;
#47412 = FACE_OUTER_BOUND ( 'NONE', #2149, .T. ) ;
#47413 = EDGE_CURVE ( 'NONE', #33018, #20128, #66081, .T. ) ;
#47414 = CARTESIAN_POINT ( 'NONE',  ( -26.79538245034556354, -7.499999999999999112, 0.000000000000000000 ) ) ;
#47415 = DIRECTION ( 'NONE',  ( 1.000000000000000000, 0.000000000000000000, 0.000000000000000000 ) ) ;
#47416 = CYLINDRICAL_SURFACE ( 'NONE', #39664, 4.000000000000000000 ) ;
#47417 = ORIENTED_EDGE ( 'NONE', *, *, #29359, .F. ) ;
#47418 = VERTEX_POINT ( 'NONE', #7006 ) ;
#47419 = DIRECTION ( 'NONE',  ( -0.000000000000000000, 1.000000000000000000, 0.000000000000000000 ) ) ;
#47420 = AXIS2_PLACEMENT_3D ( 'NONE', #68923, #30558, #41175 ) ;
#47421 = ADVANCED_FACE ( 'NONE', ( #22148 ), #22851, .T. ) ;
#47422 = CARTESIAN_POINT ( 'NONE',  ( 2.607480562269076430, 114.9070736234661325, -8.025000000000000355 ) ) ;
#47423 = CIRCLE ( 'NONE', #28255, 0.5000000000000006661 ) ;
#47424 = CIRCLE ( 'NONE', #14813, 0.2500000000000002220 ) ;
#47425 = CARTESIAN_POINT ( 'NONE',  ( -20.44134218812435932, 115.3860596766049440, 10.00000000000000000 ) ) ;
#47426 = CARTESIAN_POINT ( 'NONE',  ( -77.75707362346618368, -5.598654528085801552, 7.705886871421367523 ) ) ;
#47427 = ORIENTED_EDGE ( 'NONE', *, *, #2216, .T. ) ;
#47428 = MECHANICAL_DESIGN_GEOMETRIC_PRESENTATION_REPRESENTATION (  '', ( #65353 ), #28263 ) ;
#47429 = ORIENTED_EDGE ( 'NONE', *, *, #18682, .F. ) ;
#47430 = DIRECTION ( 'NONE',  ( -1.000000000000000000, 0.000000000000000000, 0.000000000000000000 ) ) ;
#47431 = CARTESIAN_POINT ( 'NONE',  ( 57.00000000000000000, 14.00000000000000000, -60.00402776293827145 ) ) ;
#47432 = DIRECTION ( 'NONE',  ( 1.000000000000000000, -1.189524669241239115E-16, 0.000000000000000000 ) ) ;
#47433 = ORIENTED_EDGE ( 'NONE', *, *, #7312, .T. ) ;
#47434 = CARTESIAN_POINT ( 'NONE',  ( -8.102448949553181734, 114.6049999999999756, 5.886773742842747126 ) ) ;
#47435 = CARTESIAN_POINT ( 'NONE',  ( -1.502314598737159031E-15, 2.500000000000000000, -9.000000000000000000 ) ) ;
#47436 = DIRECTION ( 'NONE',  ( 0.000000000000000000, 0.000000000000000000, -1.000000000000000000 ) ) ;
#47437 = COLOUR_RGB ( '', 0.09019608, 0.27058824, 0.51372549) ;
#47438 = FACE_OUTER_BOUND ( 'NONE', #25756, .T. ) ;
#47439 = CARTESIAN_POINT ( 'NONE',  ( -105.2949999999999875, -2.607480562269069768, 8.024999999999991473 ) ) ;
#47440 = EDGE_LOOP ( 'NONE', ( #67801, #6696 ) ) ;
#47441 = AXIS2_PLACEMENT_3D ( 'NONE', #24976, #46486, #19705 ) ;
#47442 = PLANE ( 'NONE',  #46821 ) ;
#47443 = CARTESIAN_POINT ( 'NONE',  ( -164.0070736234661695, -8.102448949553174629, -5.886773742842741797 ) ) ;
#47444 = FILL_AREA_STYLE_COLOUR ( '', #25050 ) ;
#47445 = UNCERTAINTY_MEASURE_WITH_UNIT (LENGTH_MEASURE( 1.000000000000000082E-05 ), #46314, 'distance_accuracy_value', 'NONE');
#47446 = EDGE_LOOP ( 'NONE', ( #4219, #852, #14561, #24908 ) ) ;
#47447 = CARTESIAN_POINT ( 'NONE',  ( 6.826472737025121695, 155.4929263765338305, -4.959722759717905660 ) ) ;
#47448 = CARTESIAN_POINT ( 'NONE',  ( 14.98999599679679662, 1.797044900979284448E-15, -9.500000000000000000 ) ) ;
#47449 = CONICAL_SURFACE ( 'NONE', #19155, 5.000000000000000000, 0.7853981633974415066 ) ;
#47450 = CARTESIAN_POINT ( 'NONE',  ( 31.00000000000000711, 14.00000000000000000, -36.50000000000000000 ) ) ;
#47451 = VECTOR ( 'NONE', #46780, 1000.000000000000000 ) ;
#47452 = CARTESIAN_POINT ( 'NONE',  ( -20.71231517720797655, 149.4999999999999716, -10.00000000000000000 ) ) ;
#47453 = VERTEX_POINT ( 'NONE', #16896 ) ;
#47454 = VECTOR ( 'NONE', #49594, 1000.000000000000000 ) ;
#47455 = EDGE_CURVE ( 'NONE', #40202, #56118, #12614, .T. ) ;
#47456 = CARTESIAN_POINT ( 'NONE',  ( 20.07572180596747913, 115.0406156812134952, -10.00000000000000000 ) ) ;
#47457 = ORIENTED_EDGE ( 'NONE', *, *, #55505, .F. ) ;
#47458 = CARTESIAN_POINT ( 'NONE',  ( 20.77867704735745136, 115.1383905251040716, 10.00000000000000000 ) ) ;
#47459 = DIRECTION ( 'NONE',  ( 1.000000000000000000, 0.000000000000000000, 0.000000000000000000 ) ) ;
#47460 = CARTESIAN_POINT ( 'NONE',  ( 1.400957079523476700, 2.390838073347306914, -7.000000000000002665 ) ) ;
#47461 = CYLINDRICAL_SURFACE ( 'NONE', #47683, 4.999999999999999112 ) ;
#47462 = FACE_OUTER_BOUND ( 'NONE', #37029, .T. ) ;
#47463 = CARTESIAN_POINT ( 'NONE',  ( -72.00000000000000000, 14.49137674618942562, 7.500000000000000000 ) ) ;
#47464 = CARTESIAN_POINT ( 'NONE',  ( -195.0000000000000000, 1.166476076187852838E-15, -9.524999999999991473 ) ) ;
#47465 = DIRECTION ( 'NONE',  ( -0.000000000000000000, 1.000000000000000000, -0.000000000000000000 ) ) ;
#47466 = EDGE_LOOP ( 'NONE', ( #64603, #62401, #17508, #15731 ) ) ;
#47467 = AXIS2_PLACEMENT_3D ( 'NONE', #63492, #63821, #19872 ) ;
#47468 = VERTEX_POINT ( 'NONE', #39393 ) ;
#47469 = LINE ( 'NONE', #52018, #11537 ) ;
#47470 = CARTESIAN_POINT ( 'NONE',  ( -195.0000000000000000, 0.000000000000000000, 0.000000000000000000 ) ) ;
#47471 = ORIENTED_EDGE ( 'NONE', *, *, #34306, .F. ) ;
#47472 = ADVANCED_FACE ( 'NONE', ( #11939 ), #27400, .T. ) ;
#47473 = CARTESIAN_POINT ( 'NONE',  ( -172.4050000000000296, -2.607480562269069768, 8.024999999999991473 ) ) ;
#47474 = CARTESIAN_POINT ( 'NONE',  ( -90.89292637653380780, -8.102448949553174629, -5.886773742842741797 ) ) ;
#47475 = DIRECTION ( 'NONE',  ( 0.000000000000000000, 0.000000000000000000, 1.000000000000000000 ) ) ;
#47476 = CARTESIAN_POINT ( 'NONE',  ( -182.2450000000000045, -4.716976649647093289, -6.492361379858945902 ) ) ;
#47477 = AXIS2_PLACEMENT_3D ( 'NONE', #28031, #23469, #66037 ) ;
#47478 = CARTESIAN_POINT ( 'NONE',  ( -177.2950000000000159, -2.607480562269069768, 8.024999999999991473 ) ) ;
#47479 = VERTEX_POINT ( 'NONE', #49939 ) ;
#47480 = AXIS2_PLACEMENT_3D ( 'NONE', #64445, #52867, #37058 ) ;
#47481 = AXIS2_PLACEMENT_3D ( 'NONE', #50644, #2023, #23548 ) ;
#47482 = CARTESIAN_POINT ( 'NONE',  ( 4.041451884327376121, 7.000000000000007105, 7.500000000000000000 ) ) ;
#47483 = CARTESIAN_POINT ( 'NONE',  ( -96.20499999999996987, -2.607480562269071545, -8.024999999999991473 ) ) ;
#47484 = CARTESIAN_POINT ( 'NONE',  ( 16.00000000000001776, 14.00000000000000000, 29.68999999999999417 ) ) ;
#47485 = CARTESIAN_POINT ( 'NONE',  ( 7.227466682572271317, 6.938893903907228378E-15, 12.50000000000000000 ) ) ;
#47486 = COLOUR_RGB ( '', 0.72549020, 0.75294118, 0.79215686) ;
#47487 =( NAMED_UNIT ( * ) PLANE_ANGLE_UNIT ( ) SI_UNIT ( $, .RADIAN. ) );
#47488 = EDGE_CURVE ( 'NONE', #50847, #29858, #20602, .T. ) ;
#47489 = CARTESIAN_POINT ( 'NONE',  ( -93.74499999999999034, 4.716976649647094177, 6.492361379858945902 ) ) ;
#47490 = CARTESIAN_POINT ( 'NONE',  ( 5.598654528085805993, 124.3549999999999898, 7.705886871421374629 ) ) ;
#47491 = CARTESIAN_POINT ( 'NONE',  ( -56.84499999999997755, -7.632228543268599452, 2.479861379858951054 ) ) ;
#47492 = VECTOR ( 'NONE', #504, 1000.000000000000000 ) ;
#47493 = CARTESIAN_POINT ( 'NONE',  ( -75.00000000000000000, 9.520518382567221494, -6.450733387540871000 ) ) ;
#47494 = CARTESIAN_POINT ( 'NONE',  ( -170.0929263765340238, 3.094860106621441176, 9.524999999997808331 ) ) ;
#47495 = PRODUCT_DEFINITION_SHAPE ( 'NONE', 'NONE',  #69707 ) ;
#47496 =( GEOMETRIC_REPRESENTATION_CONTEXT ( 3 ) GLOBAL_UNCERTAINTY_ASSIGNED_CONTEXT ( ( #38453 ) ) GLOBAL_UNIT_ASSIGNED_CONTEXT ( ( #57078, #19798, #9265 ) ) REPRESENTATION_CONTEXT ( 'NONE', 'WORKASPACE' ) );
#47497 = CARTESIAN_POINT ( 'NONE',  ( -195.0000000000000000, 0.000000000000000000, 0.000000000000000000 ) ) ;
#47498 = UNCERTAINTY_MEASURE_WITH_UNIT (LENGTH_MEASURE( 1.000000000000000082E-05 ), #59921, 'distance_accuracy_value', 'NONE');
#47499 = CARTESIAN_POINT ( 'NONE',  ( -0.1770589935874667675, -2.499999999999994671, -7.000000000000002665 ) ) ;
#47500 = VERTEX_POINT ( 'NONE', #44348 ) ;
#47501 = DIRECTION ( 'NONE',  ( -0.000000000000000000, -0.000000000000000000, -1.000000000000000000 ) ) ;
#47502 = STYLED_ITEM ( 'NONE', ( #33158 ), #28849 ) ;
#47503 = SURFACE_SIDE_STYLE ('',( #25297 ) ) ;
#47504 = PRESENTATION_LAYER_ASSIGNMENT (  '', '', ( #62044 ) ) ;
#47506 = CARTESIAN_POINT ( 'NONE',  ( -24.75000000000000355, 37.00000000000000000, 4.000000000000000000 ) ) ;
#47505 =( NAMED_UNIT ( * ) PLANE_ANGLE_UNIT ( ) SI_UNIT ( $, .RADIAN. ) );
#47507 = PLANE ( 'NONE',  #47420 ) ;
#47508 = ORIENTED_EDGE ( 'NONE', *, *, #55976, .T. ) ;
#47509 = ORIENTED_EDGE ( 'NONE', *, *, #23676, .F. ) ;
#47510 = CARTESIAN_POINT ( 'NONE',  ( -45.79646929189460280, 8.974048487541155694, -6.364280603494541388 ) ) ;
#47511 = DIRECTION ( 'NONE',  ( 0.000000000000000000, 0.000000000000000000, -1.000000000000000000 ) ) ;
#47512 = UNCERTAINTY_MEASURE_WITH_UNIT (LENGTH_MEASURE( 1.000000000000000082E-05 ), #21397, 'distance_accuracy_value', 'NONE');
#47513 = CIRCLE ( 'NONE', #55329, 15.00000000000000000 ) ;
#47514 = DIRECTION ( 'NONE',  ( 1.000000000000000000, -0.000000000000000000, -1.300977106640434891E-16 ) ) ;
#47515 = DIRECTION ( 'NONE',  ( 0.000000000000000000, 0.000000000000000000, 1.000000000000000000 ) ) ;
#47516 = STYLED_ITEM ( 'NONE', ( #35297 ), #24383 ) ;
#47517 = CARTESIAN_POINT ( 'NONE',  ( -75.75000000000000000, -3.000000000000000000, 19.00000000000000000 ) ) ;
#47518 = SURFACE_STYLE_FILL_AREA ( #52070 ) ;
#47519 = ORIENTED_EDGE ( 'NONE', *, *, #51801, .T. ) ;
#47520 = CARTESIAN_POINT ( 'NONE',  ( -117.5049999999999670, -6.826472737025113702, -4.959722759717900331 ) ) ;
#47521 = ORIENTED_EDGE ( 'NONE', *, *, #47372, .T. ) ;
#47522 = DIRECTION ( 'NONE',  ( 0.000000000000000000, -1.000000000000000000, 0.000000000000000000 ) ) ;
#47523 = CARTESIAN_POINT ( 'NONE',  ( 2.607480562269034241, 129.9070736234661467, -8.025000000000032330 ) ) ;
#47524 = EDGE_LOOP ( 'NONE', ( #46300, #13611, #64384, #59910 ) ) ;
#47525 = SURFACE_SIDE_STYLE ('',( #63304 ) ) ;
#47526 = ORIENTED_EDGE ( 'NONE', *, *, #57355, .T. ) ;
#47527 = AXIS2_PLACEMENT_3D ( 'NONE', #18354, #29222, #32342 ) ;
#47528 = AXIS2_PLACEMENT_3D ( 'NONE', #9756, #41080, #62494 ) ;
#47529 = CARTESIAN_POINT ( 'NONE',  ( -5.598654528085808657, 152.6449999999999818, 7.705886871421373741 ) ) ;
#47530 = CARTESIAN_POINT ( 'NONE',  ( 12.75000000000000533, 28.24999999999998224, 3.750000000000000000 ) ) ;
#47531 = VERTEX_POINT ( 'NONE', #55172 ) ;
#47532 = STYLED_ITEM ( 'NONE', ( #66782 ), #46513 ) ;
#47533 = CARTESIAN_POINT ( 'NONE',  ( 0.000000000000000000, 154.9999999999999716, 10.02499999999997904 ) ) ;
#47534 = CARTESIAN_POINT ( 'NONE',  ( 8.102448949553181734, 152.1049999999999613, -5.886773742842746238 ) ) ;
#47535 = CARTESIAN_POINT ( 'NONE',  ( 7.899999999999995914, 11.99999999999999289, -3.499999999999991118 ) ) ;
#47536 = FACE_OUTER_BOUND ( 'NONE', #43367, .T. ) ;
#47537 = ORIENTED_EDGE ( 'NONE', *, *, #67414, .T. ) ;
#47538 = CARTESIAN_POINT ( 'NONE',  ( 7.632228543268608334, 125.3429263765338249, -2.479861379858951942 ) ) ;
#47539 = DIRECTION ( 'NONE',  ( 0.000000000000000000, -0.000000000000000000, 1.000000000000000000 ) ) ;
#47540 = UNCERTAINTY_MEASURE_WITH_UNIT (LENGTH_MEASURE( 1.000000000000000082E-05 ), #52883, 'distance_accuracy_value', 'NONE');
#47541 = CYLINDRICAL_SURFACE ( 'NONE', #27605, 2.000000000000003553 ) ;
#47542 =( GEOMETRIC_REPRESENTATION_CONTEXT ( 3 ) GLOBAL_UNCERTAINTY_ASSIGNED_CONTEXT ( ( #32156 ) ) GLOBAL_UNIT_ASSIGNED_CONTEXT ( ( #29999, #67296, #29297 ) ) REPRESENTATION_CONTEXT ( 'NONE', 'WORKASPACE' ) );
#47543 = CARTESIAN_POINT ( 'NONE',  ( 45.65811388298785545, 10.21937129432926916, 6.131267346259030582 ) ) ;
#47544 = SURFACE_STYLE_FILL_AREA ( #41537 ) ;
#47545 = EDGE_LOOP ( 'NONE', ( #49401, #60481, #51692, #48749 ) ) ;
#47546 = AXIS2_PLACEMENT_3D ( 'NONE', #44417, #27796, #1388 ) ;
#47547 = EDGE_CURVE ( 'NONE', #59351, #681, #12912, .T. ) ;
#47548 = DIRECTION ( 'NONE',  ( 1.000000000000000000, 0.000000000000000000, 0.000000000000000000 ) ) ;
#47549 = VERTEX_POINT ( 'NONE', #19633 ) ;
#47550 = CARTESIAN_POINT ( 'NONE',  ( -56.69292637653379785, 10.01517768586948698, -1.839758294383808571E-15 ) ) ;
#47551 = PRESENTATION_STYLE_ASSIGNMENT (( #20046 ) ) ;
#47552 = CARTESIAN_POINT ( 'NONE',  ( -5.885195493260865440, -3.806542393196800766, 1.022368767335940312E-15 ) ) ;
#47553 = CARTESIAN_POINT ( 'NONE',  ( -153.9550000000000125, -7.632228543268599452, 2.479861379858951054 ) ) ;
#47555 = ORIENTED_EDGE ( 'NONE', *, *, #6833, .F. ) ;
#47554 = COLOUR_RGB ( '', 0.31764706, 0.68627451, 0.89019608) ;
#47556 = FILL_AREA_STYLE ('',( #52794 ) ) ;
#47557 = UNCERTAINTY_MEASURE_WITH_UNIT (LENGTH_MEASURE( 1.000000000000000082E-05 ), #60289, 'distance_accuracy_value', 'NONE');
#47558 = ADVANCED_FACE ( 'NONE', ( #61159 ), #45717, .T. ) ;
#47559 = CIRCLE ( 'NONE', #48642, 0.2500000000000000000 ) ;
#47560 = EDGE_CURVE ( 'NONE', #36332, #53365, #53164, .T. ) ;
#47561 =( LENGTH_UNIT ( ) NAMED_UNIT ( * ) SI_UNIT ( .MILLI., .METRE. ) );
#47562 = FACE_OUTER_BOUND ( 'NONE', #64328, .T. ) ;
#47563 = DIRECTION ( 'NONE',  ( 0.000000000000000000, 1.000000000000000000, 0.000000000000000000 ) ) ;
#47564 = CARTESIAN_POINT ( 'NONE',  ( -13.25000000000000355, 27.74999999999998934, -3.750000000000000000 ) ) ;
#47565 = EDGE_LOOP ( 'NONE', ( #13392, #13448, #14988, #61745 ) ) ;
#47566 = ADVANCED_FACE ( 'NONE', ( #23514 ), #12967, .F. ) ;
#47567 = ORIENTED_EDGE ( 'NONE', *, *, #44732, .F. ) ;
#47568 = CARTESIAN_POINT ( 'NONE',  ( 22.31821212674813637, 25.64654866474386807, 27.48625202223684383 ) ) ;
#47569 = DIRECTION ( 'NONE',  ( 0.000000000000000000, 1.000000000000000000, 0.000000000000000000 ) ) ;
#47570 = TOROIDAL_SURFACE ( 'NONE', #7083, 16.44999999999999574, 0.5000000000000000000 ) ;
#47571 = CARTESIAN_POINT ( 'NONE',  ( -63.35499999999998266, -4.716976649647093289, -6.492361379858945902 ) ) ;
#47572 = EDGE_LOOP ( 'NONE', ( #42751, #55970, #64498, #36403 ) ) ;
#47573 = CARTESIAN_POINT ( 'NONE',  ( 60.00000000000000000, 1.797044900979284448E-15, 6.999999999999988454 ) ) ;
#47574 = EDGE_CURVE ( 'NONE', #44314, #51526, #2524, .T. ) ;
#47575 = DIRECTION ( 'NONE',  ( 0.000000000000000000, 0.000000000000000000, -1.000000000000000000 ) ) ;
#47576 = ADVANCED_FACE ( 'NONE', ( #23870 ), #40777, .T. ) ;
#47577 = EDGE_CURVE ( 'NONE', #61826, #27592, #1365, .T. ) ;
#47578 = CARTESIAN_POINT ( 'NONE',  ( -90.65707362346617515, 9.058813317711329915, 2.943386871421369566 ) ) ;
#47579 = DIRECTION ( 'NONE',  ( 0.000000000000000000, 0.000000000000000000, -1.000000000000000000 ) ) ;
#47580 = ORIENTED_EDGE ( 'NONE', *, *, #7350, .F. ) ;
#47581 = ADVANCED_FACE ( 'NONE', ( #34760 ), #36317, .F. ) ;
#47582 =( LENGTH_UNIT ( ) NAMED_UNIT ( * ) SI_UNIT ( .MILLI., .METRE. ) );
#47584 =( BOUNDED_CURVE ( )  B_SPLINE_CURVE ( 2, ( #14716, #67470, #40774, #25582, #68522, #35477, #63241, #15088, #52009, #51648, #19629 ),
 .UNSPECIFIED., .F., .F. ) 
 B_SPLINE_CURVE_WITH_KNOTS ( ( 3, 2, 2, 2, 2, 3 ),
 ( 0.6176470588235291048, 0.6235294117647055545, 0.6294117647058820042, 0.6352941176470585649, 0.6411764705882351256, 0.6470588235294115753 ),
 .UNSPECIFIED. ) 
 CURVE ( )  GEOMETRIC_REPRESENTATION_ITEM ( )  RATIONAL_B_SPLINE_CURVE ( ( 1.000000000000002665, 0.9510565162951507556, 1.000000000000000000, 0.9510565162951535312, 1.000000000000000000, 0.9510565162951535312, 1.000000000000000000, 0.9510565162951535312, 1.000000000000000000, 0.9510565162951554186, 0.9999999999999981126 ) ) 
 REPRESENTATION_ITEM ( '' )  );
#47583 = CYLINDRICAL_SURFACE ( 'NONE', #2718, 9.524999999999991473 ) ;
#47585 = AXIS2_PLACEMENT_3D ( 'NONE', #50026, #60887, #41550 ) ;
#47586 = LINE ( 'NONE', #9905, #22247 ) ;
#47587 = CARTESIAN_POINT ( 'NONE',  ( -117.1449999999999818, -4.716976649647092401, 6.492361379858946790 ) ) ;
#47588 = CARTESIAN_POINT ( 'NONE',  ( -3.094860106618434248, 149.7949999999999875, 9.525000000000000355 ) ) ;
#47589 = CARTESIAN_POINT ( 'NONE',  ( -96.89499999999998181, 6.826472737025116366, 4.959722759717898555 ) ) ;
#47590 = DIRECTION ( 'NONE',  ( 1.000000000000000000, 0.000000000000000000, 0.000000000000000000 ) ) ;
#47591 = AXIS2_PLACEMENT_3D ( 'NONE', #52796, #30963, #14814 ) ;
#47592 = FACE_OUTER_BOUND ( 'NONE', #54119, .T. ) ;
#47593 = UNCERTAINTY_MEASURE_WITH_UNIT (LENGTH_MEASURE( 1.000000000000000082E-05 ), #41028, 'distance_accuracy_value', 'NONE');
#47594 = DIRECTION ( 'NONE',  ( 0.000000000000000000, -1.000000000000000000, 0.000000000000000000 ) ) ;
#47595 = AXIS2_PLACEMENT_3D ( 'NONE', #28940, #32958, #10804 ) ;
#47596 = ORIENTED_EDGE ( 'NONE', *, *, #51163, .F. ) ;
#47597 = CARTESIAN_POINT ( 'NONE',  ( -131.6929263765338192, 10.01517768586948698, -1.839758294383808571E-15 ) ) ;
#47598 = DIRECTION ( 'NONE',  ( -0.000000000000000000, -1.000000000000000000, -0.000000000000000000 ) ) ;
#47599 = CARTESIAN_POINT ( 'NONE',  ( -160.6449999999999818, 4.716976649647091513, -6.492361379858946790 ) ) ;
#47600 = DIRECTION ( 'NONE',  ( 1.000000000000000000, 0.000000000000000000, -1.300977106640434891E-16 ) ) ;
#47601 = COLOUR_RGB ( '', 0.09019608, 0.27058824, 0.51372549) ;
#47602 =( NAMED_UNIT ( * ) PLANE_ANGLE_UNIT ( ) SI_UNIT ( $, .RADIAN. ) );
#47603 = CARTESIAN_POINT ( 'NONE',  ( -58.75000000000000000, -4.000000000000000000, 15.00000000000000178 ) ) ;
#47604 = ORIENTED_EDGE ( 'NONE', *, *, #16575, .F. ) ;
#47605 = EDGE_LOOP ( 'NONE', ( #64769, #68934, #30648, #56577 ) ) ;
#47606 = DIRECTION ( 'NONE',  ( -0.000000000000000000, -0.000000000000000000, 1.000000000000000000 ) ) ;
#47607 = VECTOR ( 'NONE', #14801, 1000.000000000000000 ) ;
#47608 = CARTESIAN_POINT ( 'NONE',  ( -143.9929263765337737, 8.102448949553172852, -5.886773742842744461 ) ) ;
#47609 = DIRECTION ( 'NONE',  ( 1.000000000000000000, -0.000000000000000000, 0.000000000000000000 ) ) ;
#47610 = CARTESIAN_POINT ( 'NONE',  ( -129.0570736234661808, 0.000000000000000000, 9.524999999999991473 ) ) ;
#47611 = AXIS2_PLACEMENT_3D ( 'NONE', #68334, #15248, #42344 ) ;
#47612 = ORIENTED_EDGE ( 'NONE', *, *, #22642, .F. ) ;
#47613 = CARTESIAN_POINT ( 'NONE',  ( -150.2049999999999841, -2.607480562269071545, -8.024999999999991473 ) ) ;
#47614 = AXIS2_PLACEMENT_3D ( 'NONE', #17629, #34121, #2766 ) ;
#47615 = ORIENTED_EDGE ( 'NONE', *, *, #10269, .T. ) ;
#47616 = LINE ( 'NONE', #53192, #32364 ) ;
#47617 =( NAMED_UNIT ( * ) PLANE_ANGLE_UNIT ( ) SI_UNIT ( $, .RADIAN. ) );
#47618 = EDGE_LOOP ( 'NONE', ( #47277, #28834, #53442, #67800 ) ) ;
#47619 = DIRECTION ( 'NONE',  ( 0.000000000000000000, -0.000000000000000000, 1.000000000000000000 ) ) ;
#47620 = CARTESIAN_POINT ( 'NONE',  ( 5.598654528085809545, 118.1449999999999818, -7.705886871421373741 ) ) ;
#47621 = PRESENTATION_STYLE_ASSIGNMENT (( #32395 ) ) ;
#47622 = AXIS2_PLACEMENT_3D ( 'NONE', #5875, #27318, #16820 ) ;
#47623 = VERTEX_POINT ( 'NONE', #55882 ) ;
#47624 = LINE ( 'NONE', #4636, #17360 ) ;
#47625 = CARTESIAN_POINT ( 'NONE',  ( 3.094860106618431583, 121.2049999999999841, 9.525000000000000355 ) ) ;
#47626 = CARTESIAN_POINT ( 'NONE',  ( -62.60499999999998266, 6.826472737025113702, -4.959722759717902107 ) ) ;
#47627 = DIRECTION ( 'NONE',  ( -1.156482317317873451E-16, -1.000000000000000000, 0.000000000000000000 ) ) ;
#47628 = EDGE_LOOP ( 'NONE', ( #46978, #39272, #43879, #68229 ) ) ;
#47629 = CARTESIAN_POINT ( 'NONE',  ( -9.058813317711338797, 150.4550000000000125, 2.943386871421373563 ) ) ;
#47630 = UNCERTAINTY_MEASURE_WITH_UNIT (LENGTH_MEASURE( 1.000000000000000082E-05 ), #7221, 'distance_accuracy_value', 'NONE');
#47631 = LINE ( 'NONE', #31368, #65892 ) ;
#47632 = CARTESIAN_POINT ( 'NONE',  ( -15.98999599679679839, 117.9999999999999716, 9.500000000000000000 ) ) ;
#47633 = CARTESIAN_POINT ( 'NONE',  ( -41.03154609328242941, 107.7014457728230781, 3.191672614837958388 ) ) ;
#47634 = EDGE_CURVE ( 'NONE', #37913, #14152, #2720, .T. ) ;
#47635 = DIRECTION ( 'NONE',  ( 0.000000000000000000, 1.000000000000000000, 0.000000000000000000 ) ) ;
#47636 = VERTEX_POINT ( 'NONE', #29120 ) ;
#47637 = CIRCLE ( 'NONE', #31844, 0.2500000000000002220 ) ;
#47638 = CARTESIAN_POINT ( 'NONE',  ( -74.49999999999998579, 119.9999999999997726, -10.00000000000000000 ) ) ;
#47639 = CARTESIAN_POINT ( 'NONE',  ( -47.54499999999997328, -7.632228543268600340, -2.479861379858950166 ) ) ;
#47640 = ORIENTED_EDGE ( 'NONE', *, *, #31735, .F. ) ;
#47641 = CARTESIAN_POINT ( 'NONE',  ( 8.234833373661283318, 111.3243718155183899, 2.821501943811244750 ) ) ;
#47642 = EDGE_CURVE ( 'NONE', #13821, #18031, #24211, .T. ) ;
#47643 = AXIS2_PLACEMENT_3D ( 'NONE', #62371, #30686, #57447 ) ;
#47644 = CARTESIAN_POINT ( 'NONE',  ( -72.00000000000000000, 36.32520566882265456, -9.500000000000000000 ) ) ;
#47645 = AXIS2_PLACEMENT_3D ( 'NONE', #7835, #67632, #19069 ) ;
#47646 = DIRECTION ( 'NONE',  ( -1.156482317317873451E-16, -1.000000000000000000, 0.000000000000000000 ) ) ;
#47647 = VERTEX_POINT ( 'NONE', #30167 ) ;
#47648 = DIRECTION ( 'NONE',  ( 0.000000000000000000, 0.000000000000000000, -1.000000000000000000 ) ) ;
#47649 = CARTESIAN_POINT ( 'NONE',  ( -132.0570736234661808, 0.000000000000000000, 9.524999999999991473 ) ) ;
#47650 = ORIENTED_EDGE ( 'NONE', *, *, #13920, .T. ) ;
#47651 = SURFACE_STYLE_USAGE ( .BOTH. , #63423 ) ;
#47652 = CARTESIAN_POINT ( 'NONE',  ( -92.15499999999998693, 7.632228543268600340, 2.479861379858949277 ) ) ;
#47654 = ORIENTED_EDGE ( 'NONE', *, *, #5529, .T. ) ;
#47653 = AXIS2_PLACEMENT_3D ( 'NONE', #43092, #64501, #15993 ) ;
#47655 = FACE_BOUND ( 'NONE', #66439, .T. ) ;
#47656 = EDGE_CURVE ( 'NONE', #62435, #56584, #41129, .T. ) ;
#47657 = DIRECTION ( 'NONE',  ( -0.000000000000000000, -0.000000000000000000, -1.000000000000000000 ) ) ;
#47658 = CARTESIAN_POINT ( 'NONE',  ( -132.9570736234661865, 9.058813317711329915, -2.943386871421373119 ) ) ;
#47659 = CIRCLE ( 'NONE', #39735, 1.000000000000000888 ) ;
#47660 =( LENGTH_UNIT ( ) NAMED_UNIT ( * ) SI_UNIT ( .MILLI., .METRE. ) );
#47661 = CARTESIAN_POINT ( 'NONE',  ( 8.102448949553181734, 150.9950000000000045, -5.886773742842746238 ) ) ;
#47662 = CARTESIAN_POINT ( 'NONE',  ( -68.75707362346616947, -5.598654528085801552, 7.705886871421367523 ) ) ;
#47663 = EDGE_CURVE ( 'NONE', #7643, #41467, #29535, .T. ) ;
#47664 = CARTESIAN_POINT ( 'NONE',  ( 45.00000000000000000, -1.469576158976824618E-14, -9.500000000000000000 ) ) ;
#47665 = PRESENTATION_LAYER_ASSIGNMENT (  '', '', ( #18386 ) ) ;
#47666 = VERTEX_POINT ( 'NONE', #68525 ) ;
#47668 =( NAMED_UNIT ( * ) SI_UNIT ( $, .STERADIAN. ) SOLID_ANGLE_UNIT ( ) );
#47667 =( NAMED_UNIT ( * ) SI_UNIT ( $, .STERADIAN. ) SOLID_ANGLE_UNIT ( ) );
#47669 = AXIS2_PLACEMENT_3D ( 'NONE', #22475, #50594, #1297 ) ;
#47670 = PRESENTATION_LAYER_ASSIGNMENT (  '', '', ( #16200 ) ) ;
#47671 = CARTESIAN_POINT ( 'NONE',  ( -110.7549999999999955, 4.716976649647091513, -6.492361379858946790 ) ) ;
#47672 = B_SPLINE_CURVE_WITH_KNOTS ( 'NONE', 3,
 ( #62959, #36283, #57705, #9535, #30953, #56662, #3128, #52452, #18997, #18686, #13385, #13745 ),
 .UNSPECIFIED., .F., .F.,
 ( 4, 2, 2, 2, 2, 4 ),
 ( 0.000000000000000000, 0.0001470450322352820696, 0.0002940900644705641393, 0.0005881801289411533237, 0.0008822701934117425622, 0.001176360257882331801 ),
 .UNSPECIFIED. ) ;
#47673 = CARTESIAN_POINT ( 'NONE',  ( 0.000000000000000000, 118.4449999999999932, -9.525000000000000355 ) ) ;
#47674 = CARTESIAN_POINT ( 'NONE',  ( -129.7450000000000045, 4.716976649647094177, 6.492361379858945902 ) ) ;
#47675 = CIRCLE ( 'NONE', #56590, 7.000000000000001776 ) ;
#47676 = SURFACE_STYLE_USAGE ( .BOTH. , #3255 ) ;
#47677 = SURFACE_STYLE_FILL_AREA ( #26142 ) ;
#47678 = COLOUR_RGB ( '', 0.08235294, 0.09019608, 0.10196078) ;
#47679 = ORIENTED_EDGE ( 'NONE', *, *, #9722, .T. ) ;
#47680 = CARTESIAN_POINT ( 'NONE',  ( -163.4929263765338305, -8.102448949553172852, 5.886773742842742685 ) ) ;
#47681 = PRESENTATION_STYLE_ASSIGNMENT (( #5044 ) ) ;
#47682 = B_SPLINE_CURVE_WITH_KNOTS ( 'NONE', 3,
 ( #57846, #68055, #31080, #37112, #58180, #48022 ),
 .UNSPECIFIED., .F., .F.,
 ( 4, 2, 4 ),
 ( 0.000000000000000000, 0.001170983007612366256, 0.002341966015224732512 ),
 .UNSPECIFIED. ) ;
#47683 = AXIS2_PLACEMENT_3D ( 'NONE', #47101, #68523, #58306 ) ;
#47684 = PRESENTATION_STYLE_ASSIGNMENT (( #53916 ) ) ;
#47685 = CARTESIAN_POINT ( 'NONE',  ( -22.50000000000000711, 36.75000000000000000, 4.000000000000000000 ) ) ;
#47686 = CARTESIAN_POINT ( 'NONE',  ( 48.74999999999999289, 24.74999999999998579, -3.750000000000000000 ) ) ;
#47687 = PRESENTATION_STYLE_ASSIGNMENT (( #43089 ) ) ;
#47688 = ORIENTED_EDGE ( 'NONE', *, *, #56549, .T. ) ;
#47689 = CARTESIAN_POINT ( 'NONE',  ( -73.49292637653380211, -8.102448949553172852, 5.886773742842742685 ) ) ;
#47690 = CONTEXT_DEPENDENT_SHAPE_REPRESENTATION ( #65364, #66028 ) ;
#47691 = CYLINDRICAL_SURFACE ( 'NONE', #9559, 0.2500000000000002220 ) ;
#47692 = SURFACE_STYLE_FILL_AREA ( #52915 ) ;
#47693 = ADVANCED_FACE ( 'NONE', ( #4467 ), #53109, .T. ) ;
#47694 = CIRCLE ( 'NONE', #48777, 0.5000000000000004441 ) ;
#47695 = CARTESIAN_POINT ( 'NONE',  ( 7.632228543268608334, 147.4570736234661581, -2.479861379858951942 ) ) ;
#47696 = SURFACE_STYLE_FILL_AREA ( #41692 ) ;
#47697 = CARTESIAN_POINT ( 'NONE',  ( -174.9550000000000125, -7.632228543268599452, 2.479861379858951054 ) ) ;
#47698 = CONICAL_SURFACE ( 'NONE', #66718, 4.499999999999976019, 0.7853981633974412846 ) ;
#47699 = VERTEX_POINT ( 'NONE', #69547 ) ;
#47700 = FILL_AREA_STYLE ('',( #26162 ) ) ;
#47701 = SURFACE_STYLE_FILL_AREA ( #56 ) ;
#47702 = CARTESIAN_POINT ( 'NONE',  ( -23.71231517720798010, 113.4999999999999858, -7.000000000000000000 ) ) ;
#47703 = ORIENTED_EDGE ( 'NONE', *, *, #54325, .T. ) ;
#47704 = AXIS2_PLACEMENT_3D ( 'NONE', #44935, #61735, #45960 ) ;
#47705 = PRESENTATION_STYLE_ASSIGNMENT (( #40654 ) ) ;
#47706 = CARTESIAN_POINT ( 'NONE',  ( -6.826472737025120807, 140.1070736234661354, 4.959722759717906548 ) ) ;
#47707 = AXIS2_PLACEMENT_3D ( 'NONE', #17421, #64874, #12437 ) ;
#47708 =( BOUNDED_SURFACE ( )  B_SPLINE_SURFACE ( 3, 2, ( 
 ( #46740, #68147, #19933 ),
 ( #62840, #14681, #36151 ),
 ( #57583, #9413, #30835 ),
 ( #25550, #21675, #42158 ),
 ( #53358, #32558, #69188 ),
 ( #58621, #52662, #47786 ),
 ( #47425, #63880, #37910 ),
 ( #31528, #41790, #57947 ),
 ( #68492, #43195, #21317 ),
 ( #27266, #59280, #64231 ) ),
 .UNSPECIFIED., .F., .F., .F. ) 
 B_SPLINE_SURFACE_WITH_KNOTS ( ( 4, 2, 2, 2, 4 ),
 ( 3, 3 ),
 ( 0.0006185862396527136518, 0.001034390655347180218, 0.001450195071041647001, 0.001865999486736113783, 0.002281803902430580566 ),
 ( 0.000000000000000000, 1.000000000000000000 ),
 .UNSPECIFIED. ) 
 GEOMETRIC_REPRESENTATION_ITEM ( )  RATIONAL_B_SPLINE_SURFACE ( (
 ( 1.000000000000000000, 0.8505317485662434729, 1.000000000000000000),
 ( 1.000000000000000000, 0.8505807179912472371, 1.000000000000000000),
 ( 1.000000000000000000, 0.8467906168084839980, 1.000000000000000000),
 ( 1.000000000000000000, 0.8327126069847174961, 1.000000000000000000),
 ( 1.000000000000000000, 0.8223235278808177506, 1.000000000000000000),
 ( 1.000000000000000000, 0.7965633808504525293, 1.000000000000000000),
 ( 1.000000000000000000, 0.7811310880225481590, 1.000000000000000000),
 ( 1.000000000000000000, 0.7464785550193693275, 1.000000000000000000),
 ( 1.000000000000000000, 0.7273804381889640291, 1.000000000000000000),
 ( 1.000000000000000000, 0.7071067811865585639, 1.000000000000000000) ) ) 
 REPRESENTATION_ITEM ( '' )  SURFACE ( )  );
#47709 = VERTEX_POINT ( 'NONE', #42877 ) ;
#47710 = DIRECTION ( 'NONE',  ( -0.000000000000000000, -0.000000000000000000, -1.000000000000000000 ) ) ;
#47711 = CARTESIAN_POINT ( 'NONE',  ( -89.75499999999998124, 4.716976649647091513, -6.492361379858946790 ) ) ;
#47712 = UNCERTAINTY_MEASURE_WITH_UNIT (LENGTH_MEASURE( 1.000000000000000082E-05 ), #1639, 'distance_accuracy_value', 'NONE');
#47713 = LINE ( 'NONE', #64852, #16277 ) ;
#47714 = ORIENTED_EDGE ( 'NONE', *, *, #63261, .T. ) ;
#47715 = CARTESIAN_POINT ( 'NONE',  ( -33.89861118948982721, -9.947368421052626530, 2.722470280083843619 ) ) ;
#47716 = ADVANCED_FACE ( 'NONE', ( #47462 ), #3765, .F. ) ;
#47717 = VECTOR ( 'NONE', #12397, 1000.000000000000000 ) ;
#47718 = CARTESIAN_POINT ( 'NONE',  ( -9.827790563157511022E-16, 142.4429263765338192, 8.025000000000000355 ) ) ;
#47719 = EDGE_CURVE ( 'NONE', #4438, #58900, #4831, .T. ) ;
#47720 = CYLINDRICAL_SURFACE ( 'NONE', #57842, 0.5000000000000004441 ) ;
#47721 =( LENGTH_UNIT ( ) NAMED_UNIT ( * ) SI_UNIT ( .MILLI., .METRE. ) );
#47722 = ORIENTED_EDGE ( 'NONE', *, *, #62361, .T. ) ;
#47723 = AXIS2_PLACEMENT_3D ( 'NONE', #35632, #20840, #9607 ) ;
#47724 = CARTESIAN_POINT ( 'NONE',  ( -74.99999999999998579, 50.00000000000000000, -6.500000000000000000 ) ) ;
#47725 = CARTESIAN_POINT ( 'NONE',  ( -70.49499999999996191, 6.826472737025113702, -4.959722759717902107 ) ) ;
#47726 = VERTEX_POINT ( 'NONE', #63244 ) ;
#47727 = CONICAL_SURFACE ( 'NONE', #45500, 7.000000000000000888, 0.7853981633974500554 ) ;
#47728 = AXIS2_PLACEMENT_3D ( 'NONE', #37852, #69461, #63147 ) ;
#47729 = CARTESIAN_POINT ( 'NONE',  ( 71.99999999999998579, 64.07124727947029896, 10.00000000000000000 ) ) ;
#47730 = EDGE_CURVE ( 'NONE', #5568, #26425, #31562, .T. ) ;
#47731 = CARTESIAN_POINT ( 'NONE',  ( 4.500000000000002665, 24.74999999999998579, -3.750000000000000000 ) ) ;
#47732 = ORIENTED_EDGE ( 'NONE', *, *, #38801, .T. ) ;
#47733 = CARTESIAN_POINT ( 'NONE',  ( -10.74999999999999645, 4.336808689942018722E-16, 20.00000000000000000 ) ) ;
#47734 = DIRECTION ( 'NONE',  ( 0.000000000000000000, 0.000000000000000000, -1.000000000000000000 ) ) ;
#47735 = EDGE_CURVE ( 'NONE', #62777, #64020, #27874, .T. ) ;
#47737 = SURFACE_STYLE_USAGE ( .BOTH. , #9708 ) ;
#47736 = CIRCLE ( 'NONE', #12858, 0.2500000000000002220 ) ;
#47738 = DIRECTION ( 'NONE',  ( -1.000000000000000000, -0.000000000000000000, 1.300977106640435137E-16 ) ) ;
#47739 = ORIENTED_EDGE ( 'NONE', *, *, #25110, .F. ) ;
#47740 = CARTESIAN_POINT ( 'NONE',  ( -8.246138225238285102, 2.499999999999994671, -3.717269627651451191 ) ) ;
#47741 = ORIENTED_EDGE ( 'NONE', *, *, #5230, .T. ) ;
#47742 = EDGE_CURVE ( 'NONE', #52352, #69681, #39006, .T. ) ;
#47743 = FACE_OUTER_BOUND ( 'NONE', #20572, .T. ) ;
#47744 = CARTESIAN_POINT ( 'NONE',  ( 1.000000000000000000, 1.000000000000000222, 4.000000000000000000 ) ) ;
#47745 = FILL_AREA_STYLE ('',( #48067 ) ) ;
#47746 = VECTOR ( 'NONE', #6187, 1000.000000000000000 ) ;
#47747 = CARTESIAN_POINT ( 'NONE',  ( -156.6570736234661751, 9.058813317711329915, 2.943386871421369566 ) ) ;
#47748 = CARTESIAN_POINT ( 'NONE',  ( 9.058813317711337021, 123.5449999999999875, 2.943386871421375783 ) ) ;
#47749 = CARTESIAN_POINT ( 'NONE',  ( -101.6070736234661780, -8.102448949553172852, 5.886773742842742685 ) ) ;
#47750 = EDGE_CURVE ( 'NONE', #40082, #36469, #53043, .T. ) ;
#47751 = SPHERICAL_SURFACE ( 'NONE', #24567, 0.5000000000000000000 ) ;
#47752 = EDGE_LOOP ( 'NONE', ( #14127, #40223, #61087, #37180 ) ) ;
#47754 = CYLINDRICAL_SURFACE ( 'NONE', #4340, 12.00000000000000178 ) ;
#47753 = DIRECTION ( 'NONE',  ( 1.156482317317870344E-15, 1.000000000000000000, 0.000000000000000000 ) ) ;
#47755 =( LENGTH_UNIT ( ) NAMED_UNIT ( * ) SI_UNIT ( .MILLI., .METRE. ) );
#47756 = AXIS2_PLACEMENT_3D ( 'NONE', #35531, #61525, #62243 ) ;
#47757 = CARTESIAN_POINT ( 'NONE',  ( -140.0049999999999386, 6.826472737025116366, 4.959722759717898555 ) ) ;
#47758 = CARTESIAN_POINT ( 'NONE',  ( -86.75707362346616947, -5.598654528085801552, 7.705886871421367523 ) ) ;
#47759 = CARTESIAN_POINT ( 'NONE',  ( -13.75000000000000533, 30.74999999999999289, -3.750000000000000000 ) ) ;
#47760 = CARTESIAN_POINT ( 'NONE',  ( -150.1450000000000102, -4.716976649647092401, 6.492361379858946790 ) ) ;
#47761 = CARTESIAN_POINT ( 'NONE',  ( -142.1949999999999932, 8.437984349512086979, -1.550032578732815448E-15 ) ) ;
#47762 = ORIENTED_EDGE ( 'NONE', *, *, #31656, .F. ) ;
#47763 = STYLED_ITEM ( 'NONE', ( #27541 ), #56306 ) ;
#47764 = CARTESIAN_POINT ( 'NONE',  ( 44.32257855570050253, 10.24209864716914531, -3.524404701560114539 ) ) ;
#47765 = FACE_OUTER_BOUND ( 'NONE', #20867, .T. ) ;
#47766 = DIRECTION ( 'NONE',  ( 1.224646799147353207E-16, 1.000000000000000000, -0.000000000000000000 ) ) ;
#47767 = CARTESIAN_POINT ( 'NONE',  ( -57.65499999999998693, -7.632228543268600340, -2.479861379858950166 ) ) ;
#47768 = DIRECTION ( 'NONE',  ( 1.068252564556022042E-16, -0.9944852160011111719, 0.1048768571002353378 ) ) ;
#47769 = SPHERICAL_SURFACE ( 'NONE', #64999, 0.5000000000000000000 ) ;
#47770 = DIRECTION ( 'NONE',  ( 5.551115123125782702E-17, -0.2829836251474256437, 0.9591247405308765961 ) ) ;
#47771 = PRESENTATION_LAYER_ASSIGNMENT (  '', '', ( #37619 ) ) ;
#47772 = EDGE_CURVE ( 'NONE', #23615, #34825, #54407, .T. ) ;
#47773 = CARTESIAN_POINT ( 'NONE',  ( 3.999798566743338668, 58.31681314173471975, -6.349999999999996092 ) ) ;
#47774 = LINE ( 'NONE', #8692, #68598 ) ;
#47775 = CIRCLE ( 'NONE', #66859, 0.2500000000000002220 ) ;
#47776 = CARTESIAN_POINT ( 'NONE',  ( -76.75000000000000000, -0.9999999999999995559, 6.000000000000001776 ) ) ;
#47777 = CARTESIAN_POINT ( 'NONE',  ( 13.25000000000000355, 28.24999999999998934, -4.000000000000000000 ) ) ;
#47778 = FACE_OUTER_BOUND ( 'NONE', #59660, .T. ) ;
#47779 = LINE ( 'NONE', #37202, #63238 ) ;
#47780 = ORIENTED_EDGE ( 'NONE', *, *, #55004, .T. ) ;
#47781 = STYLED_ITEM ( 'NONE', ( #34459 ), #62618 ) ;
#47782 = SURFACE_STYLE_FILL_AREA ( #10092 ) ;
#47783 = CIRCLE ( 'NONE', #19650, 0.2500000000000002220 ) ;
#47784 = CARTESIAN_POINT ( 'NONE',  ( 0.000000000000000000, 112.0570736234661666, -8.025000000000000355 ) ) ;
#47785 = EDGE_CURVE ( 'NONE', #48506, #15864, #33648, .T. ) ;
#47786 = CARTESIAN_POINT ( 'NONE',  ( -20.30219483484659548, 114.9087424184428130, 10.36565267485733877 ) ) ;
#47787 = CARTESIAN_POINT ( 'NONE',  ( 22.29422224269976027, 25.82156383787605236, -27.50000000000000711 ) ) ;
#47788 = AXIS2_PLACEMENT_3D ( 'NONE', #51756, #47201, #62621 ) ;
#47789 = DIRECTION ( 'NONE',  ( 0.000000000000000000, 0.000000000000000000, -1.000000000000000000 ) ) ;
#47790 = EDGE_LOOP ( 'NONE', ( #9596, #28079, #61163, #21412 ) ) ;
#47791 = ORIENTED_EDGE ( 'NONE', *, *, #11228, .F. ) ;
#47792 = CARTESIAN_POINT ( 'NONE',  ( 29.00000000000000000, 42.58578643762690774, -89.58578643762690774 ) ) ;
#47793 = CARTESIAN_POINT ( 'NONE',  ( -40.70406133565712992, -11.89285714285713880, 3.265330863013266693 ) ) ;
#47794 = ADVANCED_FACE ( 'NONE', ( #17162 ), #53709, .T. ) ;
#47795 = VECTOR ( 'NONE', #57497, 1000.000000000000000 ) ;
#47796 = SURFACE_SIDE_STYLE ('',( #26261 ) ) ;
#47797 = VERTEX_POINT ( 'NONE', #6917 ) ;
#47798 = EDGE_CURVE ( 'NONE', #28130, #37986, #64126, .T. ) ;
#47799 = CARTESIAN_POINT ( 'NONE',  ( 0.000000000000000000, 122.5549999999999784, -9.525000000000000355 ) ) ;
#47800 = DIRECTION ( 'NONE',  ( -1.000000000000000000, 0.000000000000000000, 0.000000000000000000 ) ) ;
#47801 = CARTESIAN_POINT ( 'NONE',  ( 98.00000000000000000, 0.000000000000000000, 0.000000000000000000 ) ) ;
#47802 = CARTESIAN_POINT ( 'NONE',  ( -103.3449999999999989, 7.632228543268599452, -2.479861379858951942 ) ) ;
#47803 = ORIENTED_EDGE ( 'NONE', *, *, #25563, .T. ) ;
#47804 = AXIS2_PLACEMENT_3D ( 'NONE', #50760, #34563, #56364 ) ;
#47805 =( LENGTH_UNIT ( ) NAMED_UNIT ( * ) SI_UNIT ( .MILLI., .METRE. ) );
#47806 = PRESENTATION_STYLE_ASSIGNMENT (( #31545 ) ) ;
#47807 = EDGE_CURVE ( 'NONE', #67697, #43704, #16124, .T. ) ;
#47808 =( LENGTH_UNIT ( ) NAMED_UNIT ( * ) SI_UNIT ( .MILLI., .METRE. ) );
#47809 = ORIENTED_EDGE ( 'NONE', *, *, #33683, .F. ) ;
#47810 = CARTESIAN_POINT ( 'NONE',  ( 2.607480562269076430, 158.7929263765338135, -8.025000000000000355 ) ) ;
#47811 =( NAMED_UNIT ( * ) SI_UNIT ( $, .STERADIAN. ) SOLID_ANGLE_UNIT ( ) );
#47812 = ADVANCED_FACE ( 'NONE', ( #59002 ), #40823, .F. ) ;
#47813 = CARTESIAN_POINT ( 'NONE',  ( 5.603568002170370654, 1.515110734050476804, 8.294335516573690725 ) ) ;
#47814 = DIRECTION ( 'NONE',  ( 0.000000000000000000, 0.000000000000000000, 1.000000000000000000 ) ) ;
#47815 = CARTESIAN_POINT ( 'NONE',  ( 20.71462254620879762, 114.5909367637873402, -9.999999999998797406 ) ) ;
#47816 = EDGE_LOOP ( 'NONE', ( #65449, #19688, #69276, #10148 ) ) ;
#47817 = CARTESIAN_POINT ( 'NONE',  ( 8.437984349512095861, 128.1929263765338192, 1.550032578732816828E-15 ) ) ;
#47818 = DIRECTION ( 'NONE',  ( -1.000000000000000000, -0.000000000000000000, -0.000000000000000000 ) ) ;
#47819 = DIRECTION ( 'NONE',  ( 0.000000000000000000, -1.000000000000000000, 0.000000000000000000 ) ) ;
#47820 = SURFACE_STYLE_USAGE ( .BOTH. , #27304 ) ;
#47821 = DIRECTION ( 'NONE',  ( 0.000000000000000000, 0.000000000000000000, -1.000000000000000000 ) ) ;
#47822 = CIRCLE ( 'NONE', #56757, 5.000000000000004441 ) ;
#47823 = CIRCLE ( 'NONE', #14070, 1.000000000000000888 ) ;
#47824 = PRESENTATION_STYLE_ASSIGNMENT (( #10478 ) ) ;
#47825 = LINE ( 'NONE', #28252, #38473 ) ;
#47826 = DIRECTION ( 'NONE',  ( 0.000000000000000000, 1.000000000000000000, 0.000000000000000000 ) ) ;
#47827 = DIRECTION ( 'NONE',  ( 0.000000000000000000, 1.000000000000000000, -0.000000000000000000 ) ) ;
#47828 = ORIENTED_EDGE ( 'NONE', *, *, #38298, .F. ) ;
#47829 = ORIENTED_EDGE ( 'NONE', *, *, #48423, .T. ) ;
#47830 = DIRECTION ( 'NONE',  ( -1.000000000000000000, 0.000000000000000000, 0.000000000000000000 ) ) ;
#47831 =( NAMED_UNIT ( * ) PLANE_ANGLE_UNIT ( ) SI_UNIT ( $, .RADIAN. ) );
#47832 = CARTESIAN_POINT ( 'NONE',  ( -170.3070736234661524, -10.01517768586948698, 6.132527647946031529E-16 ) ) ;
#47834 = PLANE ( 'NONE',  #26408 ) ;
#47833 = MECHANICAL_DESIGN_GEOMETRIC_PRESENTATION_REPRESENTATION (  '', ( #544 ), #5073 ) ;
#47835 = ORIENTED_EDGE ( 'NONE', *, *, #10422, .F. ) ;
#47836 =( NAMED_UNIT ( * ) PLANE_ANGLE_UNIT ( ) SI_UNIT ( $, .RADIAN. ) );
#47837 = CARTESIAN_POINT ( 'NONE',  ( -170.9049999999999727, 2.607480562269068880, -8.024999999999993250 ) ) ;
#47838 = FILL_AREA_STYLE_COLOUR ( '', #34098 ) ;
#47839 = EDGE_CURVE ( 'NONE', #56906, #58710, #38230, .T. ) ;
#47840 = CARTESIAN_POINT ( 'NONE',  ( -60.00000000000000000, -2.024042244987997205E-14, -10.00000000000000000 ) ) ;
#47841 = CARTESIAN_POINT ( 'NONE',  ( -47.30707362346615952, -10.01517768586948698, 6.132527647946031529E-16 ) ) ;
#47842 = COLOUR_RGB ( '', 0.72549020, 0.75294118, 0.79215686) ;
#47843 = COLOUR_RGB ( '', 0.08235294, 0.09019608, 0.10196078) ;
#47844 = CARTESIAN_POINT ( 'NONE',  ( -171.5949999999999704, 2.607480562269072433, 8.024999999999991473 ) ) ;
#47845 = ADVANCED_FACE ( 'NONE', ( #23787 ), #61743, .T. ) ;
#47846 = ORIENTED_EDGE ( 'NONE', *, *, #41997, .F. ) ;
#47847 = DIRECTION ( 'NONE',  ( 0.000000000000000000, -1.000000000000000000, 0.000000000000000000 ) ) ;
#47848 = CARTESIAN_POINT ( 'NONE',  ( -12.77386173820650583, 11.13265356232346903, -4.480059943853192728 ) ) ;
#47849 = CARTESIAN_POINT ( 'NONE',  ( -81.35499999999998977, -4.716976649647093289, -6.492361379858945902 ) ) ;
#47850 = DIRECTION ( 'NONE',  ( 0.000000000000000000, 1.000000000000000000, 0.000000000000000000 ) ) ;
#47851 = DIRECTION ( 'NONE',  ( 0.000000000000000000, -1.000000000000000000, 0.000000000000000000 ) ) ;
#47852 = CARTESIAN_POINT ( 'NONE',  ( -74.49999999999998579, 36.50926243676796190, -10.00000000000000000 ) ) ;
#47853 = AXIS2_PLACEMENT_3D ( 'NONE', #11298, #48636, #37397 ) ;
#47854 = CARTESIAN_POINT ( 'NONE',  ( -82.34499999999998465, 7.632228543268599452, -2.479861379858951942 ) ) ;
#47855 = CARTESIAN_POINT ( 'NONE',  ( 8.102448949553183510, 131.1049999999999898, -5.886773742842746238 ) ) ;
#47856 = CARTESIAN_POINT ( 'NONE',  ( -75.00000000000000000, 9.680295737756338781, -6.198572516085027573 ) ) ;
#47857 =( GEOMETRIC_REPRESENTATION_CONTEXT ( 3 ) GLOBAL_UNCERTAINTY_ASSIGNED_CONTEXT ( ( #23549 ) ) GLOBAL_UNIT_ASSIGNED_CONTEXT ( ( #10636, #43041, #5674 ) ) REPRESENTATION_CONTEXT ( 'NONE', 'WORKASPACE' ) );
#47858 = DIRECTION ( 'NONE',  ( -1.000000000000000000, 0.000000000000000000, 0.000000000000000000 ) ) ;
#47859 = CARTESIAN_POINT ( 'NONE',  ( 16.00000000000001776, 15.00000000000000000, -29.68999999999999417 ) ) ;
#47860 =( GEOMETRIC_REPRESENTATION_CONTEXT ( 3 ) GLOBAL_UNCERTAINTY_ASSIGNED_CONTEXT ( ( #65784 ) ) GLOBAL_UNIT_ASSIGNED_CONTEXT ( ( #43026, #27106, #32072 ) ) REPRESENTATION_CONTEXT ( 'NONE', 'WORKASPACE' ) );
#47861 = VERTEX_POINT ( 'NONE', #35401 ) ;
#47862 = AXIS2_PLACEMENT_3D ( 'NONE', #13166, #34623, #45230 ) ;
#47863 = LINE ( 'NONE', #69258, #49425 ) ;
#47864 = DIRECTION ( 'NONE',  ( -0.000000000000000000, -0.000000000000000000, -1.000000000000000000 ) ) ;
#47865 = EDGE_CURVE ( 'NONE', #51506, #63907, #35612, .T. ) ;
#47866 = DIRECTION ( 'NONE',  ( -1.000000000000000000, -0.000000000000000000, -4.516179008354028246E-16 ) ) ;
#47867 = CARTESIAN_POINT ( 'NONE',  ( 0.000000000000000000, 136.0570736234661808, -8.025000000000000355 ) ) ;
#47868 = EDGE_LOOP ( 'NONE', ( #48917, #33458, #64539, #31041 ) ) ;
#47869 = ORIENTED_EDGE ( 'NONE', *, *, #51896, .F. ) ;
#47870 = CARTESIAN_POINT ( 'NONE',  ( -45.85105955898281138, 9.184648417642959473, -6.276141209865980564 ) ) ;
#47871 =( NAMED_UNIT ( * ) PLANE_ANGLE_UNIT ( ) SI_UNIT ( $, .RADIAN. ) );
#47872 = APPLICATION_CONTEXT ( 'automotive_design' ) ;
#47873 =( GEOMETRIC_REPRESENTATION_CONTEXT ( 3 ) GLOBAL_UNCERTAINTY_ASSIGNED_CONTEXT ( ( #8141 ) ) GLOBAL_UNIT_ASSIGNED_CONTEXT ( ( #54065, #48847, #6552 ) ) REPRESENTATION_CONTEXT ( 'NONE', 'WORKASPACE' ) );
#47874 = EDGE_CURVE ( 'NONE', #54371, #65805, #3324, .T. ) ;
#47875 = SURFACE_SIDE_STYLE ('',( #64321 ) ) ;
#47876 = DIRECTION ( 'NONE',  ( -0.000000000000000000, -1.000000000000000000, 0.000000000000000000 ) ) ;
#47877 = CARTESIAN_POINT ( 'NONE',  ( 9.827790563157511022E-16, 87.30187232391182306, -8.025000000000000355 ) ) ;
#47878 = ORIENTED_EDGE ( 'NONE', *, *, #65011, .T. ) ;
#47879 = CARTESIAN_POINT ( 'NONE',  ( -125.1549999999999869, 7.632228543268600340, 2.479861379858949277 ) ) ;
#47880 = ORIENTED_EDGE ( 'NONE', *, *, #12073, .F. ) ;
#47881 = AXIS2_PLACEMENT_3D ( 'NONE', #12253, #65742, #60787 ) ;
#47882 = CARTESIAN_POINT ( 'NONE',  ( -137.4570736234661865, -9.058813317711329915, 2.943386871421371787 ) ) ;
#47883 = EDGE_CURVE ( 'NONE', #40174, #33741, #28399, .T. ) ;
#47884 = EDGE_LOOP ( 'NONE', ( #37131, #67979, #27668, #21078 ) ) ;
#47885 = FILL_AREA_STYLE_COLOUR ( '', #17578 ) ;
#47886 = VERTEX_POINT ( 'NONE', #56851 ) ;
#47887 = DIRECTION ( 'NONE',  ( 0.000000000000000000, 0.000000000000000000, 1.000000000000000000 ) ) ;
#47888 = CARTESIAN_POINT ( 'NONE',  ( 5.598654528085809545, 154.1449999999999818, -7.705886871421373741 ) ) ;
#47889 = CARTESIAN_POINT ( 'NONE',  ( 22.99999999999999645, 5.000000000000000000, 24.00402776293825013 ) ) ;
#47890 = ORIENTED_EDGE ( 'NONE', *, *, #18006, .F. ) ;
#47891 = CARTESIAN_POINT ( 'NONE',  ( 22.50000000000000711, 37.00000000000000000, 4.000000000000000000 ) ) ;
#47892 = CARTESIAN_POINT ( 'NONE',  ( -10.01517768586949408, 150.3050000000000068, -6.132527647946036459E-16 ) ) ;
#47893 = CARTESIAN_POINT ( 'NONE',  ( -135.5070736234661695, 8.102448949553176405, 5.886773742842740909 ) ) ;
#47894 = CARTESIAN_POINT ( 'NONE',  ( -181.6429263765338078, -5.598654528085801552, 7.705886871421367523 ) ) ;
#47895 = ORIENTED_EDGE ( 'NONE', *, *, #20983, .T. ) ;
#47896 = CARTESIAN_POINT ( 'NONE',  ( -2.607480562269075097, 121.2929263765337993, 8.025000000000000355 ) ) ;
#47897 = CARTESIAN_POINT ( 'NONE',  ( 20.71231517720798010, 149.9999999999999716, 10.00000000000000000 ) ) ;
#47898 = EDGE_CURVE ( 'NONE', #64306, #3150, #66346, .T. ) ;
#47899 =( LENGTH_UNIT ( ) NAMED_UNIT ( * ) SI_UNIT ( .MILLI., .METRE. ) );
#47900 = CIRCLE ( 'NONE', #15286, 5.999999999999998224 ) ;
#47901 = LINE ( 'NONE', #38008, #57940 ) ;
#47902 = ORIENTED_EDGE ( 'NONE', *, *, #51958, .T. ) ;
#47903 = MECHANICAL_DESIGN_GEOMETRIC_PRESENTATION_REPRESENTATION (  '', ( #33229 ), #27574 ) ;
#47904 = CARTESIAN_POINT ( 'NONE',  ( -41.06069799967657730, 107.9552192246431730, -3.682425535826299612 ) ) ;
#47905 = ORIENTED_EDGE ( 'NONE', *, *, #52517, .F. ) ;
#47906 = CARTESIAN_POINT ( 'NONE',  ( -53.69292637653380496, 10.01517768586948698, -1.839758294383808571E-15 ) ) ;
#47907 = TOROIDAL_SURFACE ( 'NONE', #1739, 1.000000000000000000, 0.5000000000000000000 ) ;
#47908 = CARTESIAN_POINT ( 'NONE',  ( -150.5049999999999955, -6.826472737025115478, -4.959722759717899443 ) ) ;
#47909 = CARTESIAN_POINT ( 'NONE',  ( -176.4570736234661865, -9.058813317711329915, 2.943386871421371787 ) ) ;
#47910 = CIRCLE ( 'NONE', #20884, 0.5000000000000000000 ) ;
#47911 = AXIS2_PLACEMENT_3D ( 'NONE', #38137, #31776, #43760 ) ;
#47912 = DIRECTION ( 'NONE',  ( 0.000000000000000000, -0.6691306063588591257, 0.7431448254773933559 ) ) ;
#47913 = CYLINDRICAL_SURFACE ( 'NONE', #24706, 16.00000000000000711 ) ;
#47914 = PRESENTATION_STYLE_ASSIGNMENT (( #28341 ) ) ;
#47915 = ORIENTED_EDGE ( 'NONE', *, *, #8979, .F. ) ;
#47916 = ORIENTED_EDGE ( 'NONE', *, *, #1203, .T. ) ;
#47917 = CARTESIAN_POINT ( 'NONE',  ( 66.24999999999998579, 34.24999999999999289, 3.750000000000000000 ) ) ;
#47918 = CARTESIAN_POINT ( 'NONE',  ( 57.74999999999998579, 30.74999999999999289, 3.750000000000000000 ) ) ;
#47919 = CARTESIAN_POINT ( 'NONE',  ( -65.00499999999998124, 6.826472737025116366, 4.959722759717898555 ) ) ;
#47920 = ORIENTED_EDGE ( 'NONE', *, *, #56795, .F. ) ;
#47921 = CARTESIAN_POINT ( 'NONE',  ( 4.750000000000002665, 0.000000000000000000, 3.750000000000000000 ) ) ;
#47922 = CARTESIAN_POINT ( 'NONE',  ( -7.000000000000002665, 0.000000000000000000, 0.000000000000000000 ) ) ;
#47923 = SURFACE_STYLE_USAGE ( .BOTH. , #16572 ) ;
#47924 =( NAMED_UNIT ( * ) SI_UNIT ( $, .STERADIAN. ) SOLID_ANGLE_UNIT ( ) );
#47925 = CARTESIAN_POINT ( 'NONE',  ( 1.000000000000000000, 1.000000000000000222, 3.000000000000000000 ) ) ;
#47926 = VERTEX_POINT ( 'NONE', #18167 ) ;
#47927 = AXIS2_PLACEMENT_3D ( 'NONE', #54334, #64888, #33241 ) ;
#47928 = CARTESIAN_POINT ( 'NONE',  ( -20.57648123223228254, 110.4999999999999858, 10.27659574468085069 ) ) ;
#47929 = FILL_AREA_STYLE_COLOUR ( '', #35318 ) ;
#47930 = CARTESIAN_POINT ( 'NONE',  ( 2.607480562269071989, 125.7070736234661723, 8.025000000000002132 ) ) ;
#47931 = AXIS2_PLACEMENT_3D ( 'NONE', #3041, #24205, #34751 ) ;
#47932 = CARTESIAN_POINT ( 'NONE',  ( -122.0949999999999847, -2.607480562269071545, -8.024999999999991473 ) ) ;
#47933 = CARTESIAN_POINT ( 'NONE',  ( -9.058813317711338797, 152.3449999999999704, 2.943386871421373563 ) ) ;
#47934 = CARTESIAN_POINT ( 'NONE',  ( -88.64499999999998181, 4.716976649647091513, -6.492361379858946790 ) ) ;
#47935 = DIRECTION ( 'NONE',  ( 0.000000000000000000, 0.000000000000000000, 1.000000000000000000 ) ) ;
#47936 = AXIS2_PLACEMENT_3D ( 'NONE', #31030, #25752, #63734 ) ;
#47937 = VECTOR ( 'NONE', #17239, 1000.000000000000000 ) ;
#47938 = MECHANICAL_DESIGN_GEOMETRIC_PRESENTATION_REPRESENTATION (  '', ( #29892 ), #65856 ) ;
#47939 = DIRECTION ( 'NONE',  ( -0.000000000000000000, 1.000000000000000000, 0.000000000000000000 ) ) ;
#47940 = FACE_OUTER_BOUND ( 'NONE', #55740, .T. ) ;
#47941 = ORIENTED_EDGE ( 'NONE', *, *, #56530, .F. ) ;
#47942 = CARTESIAN_POINT ( 'NONE',  ( -130.0429263765338135, -9.058813317711329915, -2.943386871421370898 ) ) ;
#47943 =( NAMED_UNIT ( * ) SI_UNIT ( $, .STERADIAN. ) SOLID_ANGLE_UNIT ( ) );
#47944 = CARTESIAN_POINT ( 'NONE',  ( 0.000000000000000000, 114.9999999999999574, 16.00000000000000000 ) ) ;
#47945 = CARTESIAN_POINT ( 'NONE',  ( -150.4449999999999932, 0.000000000000000000, 8.024999999999991473 ) ) ;
#47946 = CARTESIAN_POINT ( 'NONE',  ( -60.00000000000000000, -2.024042244987997205E-14, 10.00000000000000000 ) ) ;
#47947 = AXIS2_PLACEMENT_3D ( 'NONE', #43616, #28047, #1965 ) ;
#47948 = EDGE_CURVE ( 'NONE', #63631, #3382, #5985, .T. ) ;
#47949 = CARTESIAN_POINT ( 'NONE',  ( 3.499999999999998668, 36.99999999999999289, 4.000000000000000000 ) ) ;
#47950 = ORIENTED_EDGE ( 'NONE', *, *, #29370, .F. ) ;
#47951 = EDGE_LOOP ( 'NONE', ( #24704, #17134 ) ) ;
#47952 = STYLED_ITEM ( 'NONE', ( #40232 ), #57571 ) ;
#47953 = FILL_AREA_STYLE ('',( #31339 ) ) ;
#47954 = CARTESIAN_POINT ( 'NONE',  ( -7.632228543268608334, 117.8429263765338249, 2.479861379858952830 ) ) ;
#47955 = DIRECTION ( 'NONE',  ( 0.000000000000000000, 0.000000000000000000, -1.000000000000000000 ) ) ;
#47956 = CARTESIAN_POINT ( 'NONE',  ( -130.5570736234661808, -1.166476076187852838E-15, -9.524999999999991473 ) ) ;
#47957 = ORIENTED_EDGE ( 'NONE', *, *, #31696, .F. ) ;
#47958 = CARTESIAN_POINT ( 'NONE',  ( -153.2049999999999841, -2.607480562269071545, -8.024999999999991473 ) ) ;
#47959 = EDGE_CURVE ( 'NONE', #7763, #37266, #46460, .T. ) ;
#47960 = ORIENTED_EDGE ( 'NONE', *, *, #35897, .T. ) ;
#47961 = SURFACE_STYLE_FILL_AREA ( #53854 ) ;
#47962 = CARTESIAN_POINT ( 'NONE',  ( -141.5070736234661410, 8.102448949553176405, 5.886773742842740909 ) ) ;
#47964 = ORIENTED_EDGE ( 'NONE', *, *, #7469, .F. ) ;
#47963 = EDGE_CURVE ( 'NONE', #20128, #3527, #45642, .T. ) ;
#47965 =( LENGTH_UNIT ( ) NAMED_UNIT ( * ) SI_UNIT ( .MILLI., .METRE. ) );
#47966 = EDGE_CURVE ( 'NONE', #62912, #50010, #60739, .T. ) ;
#47967 = LINE ( 'NONE', #65097, #63460 ) ;
#47968 = CARTESIAN_POINT ( 'NONE',  ( -1.166476076187854022E-15, 116.9449999999999932, 9.525000000000000355 ) ) ;
#47969 = DIRECTION ( 'NONE',  ( 0.000000000000000000, 0.000000000000000000, 1.000000000000000000 ) ) ;
#47970 = ORIENTED_EDGE ( 'NONE', *, *, #44370, .F. ) ;
#47971 = CARTESIAN_POINT ( 'NONE',  ( -74.75000000000000000, -4.000000000000000000, 18.00000000000000000 ) ) ;
#47973 = EDGE_CURVE ( 'NONE', #16642, #6607, #25179, .T. ) ;
#47972 = CARTESIAN_POINT ( 'NONE',  ( 3.094860106618435136, 125.4049999999999869, -9.525000000000000355 ) ) ;
#47974 = CARTESIAN_POINT ( 'NONE',  ( -61.55499999999998550, 0.000000000000000000, 8.024999999999991473 ) ) ;
#47975 = CARTESIAN_POINT ( 'NONE',  ( -117.5949999999999989, 2.607480562269073321, 8.024999999999991473 ) ) ;
#47976 = LINE ( 'NONE', #64783, #58796 ) ;
#47977 = VERTEX_POINT ( 'NONE', #36098 ) ;
#47978 = CARTESIAN_POINT ( 'NONE',  ( -3.094860106618434248, 150.9050000000000011, 9.525000000000000355 ) ) ;
#47979 = CARTESIAN_POINT ( 'NONE',  ( 35.99999999999999289, 0.000000000000000000, 32.00402776293825724 ) ) ;
#47980 = EDGE_CURVE ( 'NONE', #10058, #7106, #25077, .T. ) ;
#47981 = DIRECTION ( 'NONE',  ( 0.000000000000000000, 0.000000000000000000, -1.000000000000000000 ) ) ;
#47982 = COLOUR_RGB ( '', 0.72549020, 0.75294118, 0.79215686) ;
#47983 = CARTESIAN_POINT ( 'NONE',  ( -17.75000000000000355, -3.000000000000000000, 0.000000000000000000 ) ) ;
#47984 = ORIENTED_EDGE ( 'NONE', *, *, #27021, .T. ) ;
#47985 = CARTESIAN_POINT ( 'NONE',  ( -46.25707362346617657, 5.598654528085800663, -7.705886871421367523 ) ) ;
#47986 = CARTESIAN_POINT ( 'NONE',  ( -182.0049999999999670, 6.826472737025116366, 4.959722759717898555 ) ) ;
#47987 = ORIENTED_EDGE ( 'NONE', *, *, #1452, .T. ) ;
#47988 = CARTESIAN_POINT ( 'NONE',  ( 21.00000000000001776, -3.148064030671221758, 29.68999999999999417 ) ) ;
#47989 = SURFACE_STYLE_USAGE ( .BOTH. , #26463 ) ;
#47990 = VERTEX_POINT ( 'NONE', #57177 ) ;
#47991 =( NAMED_UNIT ( * ) PLANE_ANGLE_UNIT ( ) SI_UNIT ( $, .RADIAN. ) );
#47992 =( BOUNDED_CURVE ( )  B_SPLINE_CURVE ( 3, ( #17258, #28075, #61160, #2350 ),
 .UNSPECIFIED., .F., .F. ) 
 B_SPLINE_CURVE_WITH_KNOTS ( ( 4, 4 ),
 ( 1.570796326794891451, 3.141592653589793116 ),
 .UNSPECIFIED. ) 
 CURVE ( )  GEOMETRIC_REPRESENTATION_ITEM ( )  RATIONAL_B_SPLINE_CURVE ( ( 1.000000000000000000, 0.8047378541243637162, 0.8047378541243637162, 1.000000000000000000 ) ) 
 REPRESENTATION_ITEM ( '' )  );
#47993 = ORIENTED_EDGE ( 'NONE', *, *, #24615, .F. ) ;
#47994 = FACE_OUTER_BOUND ( 'NONE', #13533, .T. ) ;
#47995 = MECHANICAL_DESIGN_GEOMETRIC_PRESENTATION_REPRESENTATION (  '', ( #26569 ), #1819 ) ;
#47996 = FILL_AREA_STYLE ('',( #26116 ) ) ;
#47997 = CARTESIAN_POINT ( 'NONE',  ( -90.65499999999998693, -7.632228543268600340, -2.479861379858950166 ) ) ;
#47998 = ORIENTED_EDGE ( 'NONE', *, *, #50645, .T. ) ;
#47999 = SURFACE_SIDE_STYLE ('',( #52201 ) ) ;
#48000 = CARTESIAN_POINT ( 'NONE',  ( -133.1070736234661922, 8.102448949553171076, -5.886773742842744461 ) ) ;
#48001 = CARTESIAN_POINT ( 'NONE',  ( -0.5586952923285121164, 154.4720785402125500, -9.525000000000002132 ) ) ;
#48002 = CARTESIAN_POINT ( 'NONE',  ( -67.40707362346614673, 3.094860106618428031, -9.524999999999993250 ) ) ;
#48003 = DIRECTION ( 'NONE',  ( -0.000000000000000000, -0.000000000000000000, 1.000000000000000000 ) ) ;
#48004 = ORIENTED_EDGE ( 'NONE', *, *, #19634, .T. ) ;
#48005 = CARTESIAN_POINT ( 'NONE',  ( 0.000000000000000000, 36.99999999999999289, 3.750000000000000000 ) ) ;
#48006 =( NAMED_UNIT ( * ) PLANE_ANGLE_UNIT ( ) SI_UNIT ( $, .RADIAN. ) );
#48007 = AXIS2_PLACEMENT_3D ( 'NONE', #59924, #16369, #54973 ) ;
#48008 = DIRECTION ( 'NONE',  ( 1.000000000000000000, 0.000000000000000000, 0.000000000000000000 ) ) ;
#48009 = CARTESIAN_POINT ( 'NONE',  ( -108.6549999999999869, -7.632228543268600340, -2.479861379858950166 ) ) ;
#48010 = CARTESIAN_POINT ( 'NONE',  ( -10.01517768586949231, 122.1949999999999648, -6.132527647946036459E-16 ) ) ;
#48011 = CARTESIAN_POINT ( 'NONE',  ( -116.3949999999999960, -6.826472737025115478, -4.959722759717899443 ) ) ;
#48012 =( BOUNDED_CURVE ( )  B_SPLINE_CURVE ( 2, ( #1205, #44235, #65637, #38949, #28317, #60349, #44579, #33621, #1563, #59295, #12500 ),
 .UNSPECIFIED., .F., .F. ) 
 B_SPLINE_CURVE_WITH_KNOTS ( ( 3, 2, 2, 2, 2, 3 ),
 ( 0.6413043478260719299, 0.6434782608695501782, 0.6456521739130284265, 0.6478260869565066749, 0.6499999999999848121, 0.6521739130434630605 ),
 .UNSPECIFIED. ) 
 CURVE ( )  GEOMETRIC_REPRESENTATION_ITEM ( )  RATIONAL_B_SPLINE_CURVE ( ( 1.000000000000337508, 0.9510565162948161344, 1.000000000000000000, 0.9510565162951535312, 1.000000000000000000, 0.9510565162951535312, 1.000000000000000000, 0.9510565162951535312, 1.000000000000000000, 0.9510565162954959240, 0.9999999999996576072 ) ) 
 REPRESENTATION_ITEM ( '' )  );
#48013 = CARTESIAN_POINT ( 'NONE',  ( 10.00000000000000178, 60.69879356856722552, -69.02971849933236115 ) ) ;
#48014 = ORIENTED_EDGE ( 'NONE', *, *, #39836, .T. ) ;
#48015 = CARTESIAN_POINT ( 'NONE',  ( -165.7429263765338305, -5.598654528085803328, -7.705886871421366635 ) ) ;
#48016 = CARTESIAN_POINT ( 'NONE',  ( -14.95322863490702225, 69.00000000000000000, 12.50000000000000000 ) ) ;
#48017 = AXIS2_PLACEMENT_3D ( 'NONE', #14121, #51761, #14444 ) ;
#48018 = CIRCLE ( 'NONE', #49107, 0.5000000000000004441 ) ;
#48019 = EDGE_CURVE ( 'NONE', #15417, #28999, #45430, .T. ) ;
#48020 =( GEOMETRIC_REPRESENTATION_CONTEXT ( 3 ) GLOBAL_UNCERTAINTY_ASSIGNED_CONTEXT ( ( #10931 ) ) GLOBAL_UNIT_ASSIGNED_CONTEXT ( ( #6528, #22743, #28324 ) ) REPRESENTATION_CONTEXT ( 'NONE', 'WORKASPACE' ) );
#48021 = FACE_OUTER_BOUND ( 'NONE', #67228, .T. ) ;
#48022 = CARTESIAN_POINT ( 'NONE',  ( -53.18756747357285519, -10.02680648607945102, -3.500000000000002220 ) ) ;
#48023 = ORIENTED_EDGE ( 'NONE', *, *, #56594, .F. ) ;
#48024 = CARTESIAN_POINT ( 'NONE',  ( -72.59292637653379643, -3.094860106618431139, -9.524999999999991473 ) ) ;
#48025 = CONTEXT_DEPENDENT_SHAPE_REPRESENTATION ( #10116, #21626 ) ;
#48027 = ADVANCED_FACE ( 'NONE', ( #46695 ), #68807, .T. ) ;
#48026 = DIRECTION ( 'NONE',  ( -0.2413793103448194644, 0.9704308468600220117, 0.000000000000000000 ) ) ;
#48028 = CARTESIAN_POINT ( 'NONE',  ( -7.335726704534229370, -5.294148637306920868, 0.03572125916566790127 ) ) ;
#48029 = ADVANCED_FACE ( 'NONE', ( #68443 ), #31612, .T. ) ;
#48030 = PRESENTATION_LAYER_ASSIGNMENT (  '', '', ( #52485 ) ) ;
#48031 = CARTESIAN_POINT ( 'NONE',  ( -179.3049999999999784, 8.437984349512086979, -1.550032578732815448E-15 ) ) ;
#48032 = ORIENTED_EDGE ( 'NONE', *, *, #38574, .F. ) ;
#48033 = FACE_OUTER_BOUND ( 'NONE', #1378, .T. ) ;
#48034 = FILL_AREA_STYLE_COLOUR ( '', #56728 ) ;
#48035 = EDGE_CURVE ( 'NONE', #55705, #15297, #52063, .T. ) ;
#48036 = DIRECTION ( 'NONE',  ( -5.782411586589351722E-16, -1.000000000000000000, 0.000000000000000000 ) ) ;
#48037 = CARTESIAN_POINT ( 'NONE',  ( 34.99999999999999289, 99.99999999999998579, 7.500000000000000000 ) ) ;
#48038 =( NAMED_UNIT ( * ) SI_UNIT ( $, .STERADIAN. ) SOLID_ANGLE_UNIT ( ) );
#48039 = CARTESIAN_POINT ( 'NONE',  ( 2.607480562269071989, 143.7070736234661297, 8.025000000000002132 ) ) ;
#48040 = EDGE_LOOP ( 'NONE', ( #60443, #51219, #18434, #30959 ) ) ;
#48042 = EDGE_CURVE ( 'NONE', #58037, #5366, #58774, .T. ) ;
#48041 = CARTESIAN_POINT ( 'NONE',  ( -24.00000000000000355, 36.75000000000000000, 4.000000000000000000 ) ) ;
#48043 = CARTESIAN_POINT ( 'NONE',  ( -95.15499999999998693, 7.632228543268600340, 2.479861379858949277 ) ) ;
#48044 = CARTESIAN_POINT ( 'NONE',  ( -75.75000000000000000, 4.336808689942018722E-16, 20.00000000000000000 ) ) ;
#48045 = VERTEX_POINT ( 'NONE', #63633 ) ;
#48046 = DIRECTION ( 'NONE',  ( -1.000000000000000000, 0.000000000000000000, 0.000000000000000000 ) ) ;
#48047 = CARTESIAN_POINT ( 'NONE',  ( 23.50000000000001776, 15.00000000000000000, 26.18999999999999417 ) ) ;
#48048 = SURFACE_STYLE_USAGE ( .BOTH. , #11040 ) ;
#48049 = CARTESIAN_POINT ( 'NONE',  ( 27.00000000000001776, -3.148064030671221758, -34.49999999999999289 ) ) ;
#48050 = VERTEX_POINT ( 'NONE', #27002 ) ;
#48051 = CARTESIAN_POINT ( 'NONE',  ( 7.440601873764706831, 1.112499515747338741, 0.4948905776603317874 ) ) ;
#48052 = CARTESIAN_POINT ( 'NONE',  ( -73.34499999999999886, 7.632228543268599452, -2.479861379858951942 ) ) ;
#48053 = ORIENTED_EDGE ( 'NONE', *, *, #33909, .T. ) ;
#48054 = DIRECTION ( 'NONE',  ( 1.000000000000000000, 0.000000000000000000, 0.000000000000000000 ) ) ;
#48055 = CARTESIAN_POINT ( 'NONE',  ( -120.6570736234661751, 9.058813317711329915, 2.943386871421369566 ) ) ;
#48056 = ORIENTED_EDGE ( 'NONE', *, *, #651, .F. ) ;
#48057 = CARTESIAN_POINT ( 'NONE',  ( 12.72792206135785698, 149.9999999999999716, 10.50000000000000000 ) ) ;
#48058 = VECTOR ( 'NONE', #1219, 1000.000000000000000 ) ;
#48059 = AXIS2_PLACEMENT_3D ( 'NONE', #45385, #14024, #24548 ) ;
#48060 = SURFACE_STYLE_FILL_AREA ( #11055 ) ;
#48061 = CARTESIAN_POINT ( 'NONE',  ( 10.00000000000001954, 43.00000000000000000, 45.61250543006183733 ) ) ;
#48062 = ORIENTED_EDGE ( 'NONE', *, *, #52683, .F. ) ;
#48063 = DIRECTION ( 'NONE',  ( -0.000000000000000000, -0.000000000000000000, 1.000000000000000000 ) ) ;
#48064 = ORIENTED_EDGE ( 'NONE', *, *, #52479, .T. ) ;
#48065 = CARTESIAN_POINT ( 'NONE',  ( -17.41962728626436530, -0.1139526552317604857, -2.000000000000000000 ) ) ;
#48066 = SURFACE_SIDE_STYLE ('',( #11763 ) ) ;
#48067 = FILL_AREA_STYLE_COLOUR ( '', #690 ) ;
#48068 = CARTESIAN_POINT ( 'NONE',  ( -155.9070736234662036, -3.094860106618429807, 9.524999999999991473 ) ) ;
#48069 = PRODUCT_DEFINITION_SHAPE ( 'NONE', 'NONE',  #69720 ) ;
#48070 = CARTESIAN_POINT ( 'NONE',  ( 5.598654528085809545, 121.1449999999999818, -7.705886871421373741 ) ) ;
#48071 = CARTESIAN_POINT ( 'NONE',  ( -90.05707362346616662, 0.000000000000000000, 9.524999999999991473 ) ) ;
#48072 = ADVANCED_FACE ( 'NONE', ( #69270 ), #10862, .T. ) ;
#48073 = SURFACE_SIDE_STYLE ('',( #11419 ) ) ;
#48074 = VERTEX_POINT ( 'NONE', #53092 ) ;
#48075 = SURFACE_STYLE_FILL_AREA ( #54332 ) ;
#48077 = FILL_AREA_STYLE ('',( #64887 ) ) ;
#48076 = CYLINDRICAL_SURFACE ( 'NONE', #50324, 3.100000000000003642 ) ;
#48078 = CARTESIAN_POINT ( 'NONE',  ( -85.55707362346618083, -1.166476076187852838E-15, -9.524999999999991473 ) ) ;
#48079 = AXIS2_PLACEMENT_3D ( 'NONE', #56995, #30947, #3845 ) ;
#48080 = CARTESIAN_POINT ( 'NONE',  ( -143.7549999999999955, 4.716976649647091513, -6.492361379858946790 ) ) ;
#48081 = CARTESIAN_POINT ( 'NONE',  ( 75.00000000000000000, 19.30628705663858469, 6.999999999999999112 ) ) ;
#48082 = CARTESIAN_POINT ( 'NONE',  ( -154.1949999999999648, 8.437984349512085203, -1.550032578732815448E-15 ) ) ;
#48083 = CARTESIAN_POINT ( 'NONE',  ( -137.2450000000000045, -4.716976649647093289, -6.492361379858945902 ) ) ;
#48084 = ORIENTED_EDGE ( 'NONE', *, *, #55554, .T. ) ;
#48085 = CARTESIAN_POINT ( 'NONE',  ( 44.99999999999999289, 9.999999999999992895, -4.000000000000000888 ) ) ;
#48086 = DIRECTION ( 'NONE',  ( 0.000000000000000000, -1.000000000000000000, 0.000000000000000000 ) ) ;
#48087 = CARTESIAN_POINT ( 'NONE',  ( 20.88896767935282739, 150.0000000000000284, -9.626543325103073201 ) ) ;
#48088 = UNCERTAINTY_MEASURE_WITH_UNIT (LENGTH_MEASURE( 1.000000000000000082E-05 ), #1634, 'distance_accuracy_value', 'NONE');
#48089 = CARTESIAN_POINT ( 'NONE',  ( -54.50499999999998835, -6.826472737025115478, -4.959722759717899443 ) ) ;
#48090 = DIRECTION ( 'NONE',  ( 0.000000000000000000, 0.000000000000000000, -1.000000000000000000 ) ) ;
#48091 = ADVANCED_FACE ( 'NONE', ( #42564, #36244, #20730 ), #53758, .T. ) ;
#48092 = EDGE_CURVE ( 'NONE', #29444, #8875, #15475, .T. ) ;
#48093 = CARTESIAN_POINT ( 'NONE',  ( 24.00000000000000000, 1.000000000000000000, -3.000000000000000000 ) ) ;
#48094 = CYLINDRICAL_SURFACE ( 'NONE', #33540, 0.5000000000000004441 ) ;
#48095 = DIRECTION ( 'NONE',  ( -7.080503983578803083E-17, -1.000000000000000000, 0.000000000000000000 ) ) ;
#48096 = UNCERTAINTY_MEASURE_WITH_UNIT (LENGTH_MEASURE( 1.000000000000000082E-05 ), #3170, 'distance_accuracy_value', 'NONE');
#48097 =( LENGTH_UNIT ( ) NAMED_UNIT ( * ) SI_UNIT ( .MILLI., .METRE. ) );
#48098 = EDGE_CURVE ( 'NONE', #19597, #19879, #47353, .T. ) ;
#48099 = VECTOR ( 'NONE', #57383, 1000.000000000000000 ) ;
#48100 = DIRECTION ( 'NONE',  ( -1.000000000000000000, 0.000000000000000000, 0.000000000000000000 ) ) ;
#48101 = VECTOR ( 'NONE', #13836, 999.9999999999998863 ) ;
#48102 = AXIS2_PLACEMENT_3D ( 'NONE', #5428, #26554, #58579 ) ;
#48103 = DIRECTION ( 'NONE',  ( -0.000000000000000000, -0.000000000000000000, -1.000000000000000000 ) ) ;
#48104 = ADVANCED_FACE ( 'NONE', ( #14768 ), #50934, .F. ) ;
#48105 = ORIENTED_EDGE ( 'NONE', *, *, #58608, .T. ) ;
#48106 = SURFACE_STYLE_USAGE ( .BOTH. , #68843 ) ;
#48107 = VECTOR ( 'NONE', #8351, 1000.000000000000000 ) ;
#48108 = CARTESIAN_POINT ( 'NONE',  ( 4.716976649647099507, 111.7570736234661553, -6.492361379858953008 ) ) ;
#48109 = EDGE_CURVE ( 'NONE', #7659, #2804, #42920, .T. ) ;
#48110 = CARTESIAN_POINT ( 'NONE',  ( -83.49999999999998579, 4.336808689942018722E-16, -5.100000000000000533 ) ) ;
#48111 = CIRCLE ( 'NONE', #45889, 0.2500000000000002220 ) ;
#48112 = FILL_AREA_STYLE ('',( #16774 ) ) ;
#48113 = ORIENTED_EDGE ( 'NONE', *, *, #38412, .F. ) ;
#48114 = VERTEX_POINT ( 'NONE', #55494 ) ;
#48115 = CARTESIAN_POINT ( 'NONE',  ( -109.1070736234661780, 8.102448949553172852, -5.886773742842744461 ) ) ;
#48116 = MECHANICAL_DESIGN_GEOMETRIC_PRESENTATION_REPRESENTATION (  '', ( #3076 ), #51439 ) ;
#48117 = LINE ( 'NONE', #15735, #11368 ) ;
#48118 = EDGE_LOOP ( 'NONE', ( #64987, #47140, #67009 ) ) ;
#48119 = CARTESIAN_POINT ( 'NONE',  ( -5.598654528085808657, 123.7549999999999955, 7.705886871421373741 ) ) ;
#48120 = CARTESIAN_POINT ( 'NONE',  ( -85.49292637653380211, -8.102448949553174629, 5.886773742842742685 ) ) ;
#48121 = DIRECTION ( 'NONE',  ( 0.000000000000000000, -1.000000000000000000, 0.000000000000000000 ) ) ;
#48122 = DIRECTION ( 'NONE',  ( -0.000000000000000000, 1.000000000000000000, -0.000000000000000000 ) ) ;
#48123 = CARTESIAN_POINT ( 'NONE',  ( -98.39499999999999602, -6.826472737025115478, -4.959722759717899443 ) ) ;
#48124 = VERTEX_POINT ( 'NONE', #6959 ) ;
#48125 = CARTESIAN_POINT ( 'NONE',  ( 4.879427070620491413, 154.0600444928449804, -7.674131026540870870 ) ) ;
#48126 = DIRECTION ( 'NONE',  ( 0.000000000000000000, 1.000000000000000000, -0.000000000000000000 ) ) ;
#48127 = DIRECTION ( 'NONE',  ( 0.000000000000000000, 0.000000000000000000, 1.000000000000000000 ) ) ;
#48128 = ORIENTED_EDGE ( 'NONE', *, *, #66120, .F. ) ;
#48129 = CARTESIAN_POINT ( 'NONE',  ( -7.632228543268607446, 159.5429263765338419, -2.479861379858953718 ) ) ;
#48130 = DIRECTION ( 'NONE',  ( 0.000000000000000000, 0.000000000000000000, -1.000000000000000000 ) ) ;
#48131 = SURFACE_SIDE_STYLE ('',( #42506 ) ) ;
#48132 = CARTESIAN_POINT ( 'NONE',  ( 20.48327417467292832, 114.7638625681370002, -10.30663925914721268 ) ) ;
#48133 = ORIENTED_EDGE ( 'NONE', *, *, #63999, .T. ) ;
#48134 = CARTESIAN_POINT ( 'NONE',  ( 68.99999999999998579, 36.75000000000000000, -4.000000000000000000 ) ) ;
#48135 =( LENGTH_UNIT ( ) NAMED_UNIT ( * ) SI_UNIT ( .MILLI., .METRE. ) );
#48136 = DIRECTION ( 'NONE',  ( 0.000000000000000000, -0.000000000000000000, 1.000000000000000000 ) ) ;
#48137 = CARTESIAN_POINT ( 'NONE',  ( -34.11772421319633253, -9.152876382972609193, 5.508355886455341022 ) ) ;
#48138 = PRESENTATION_STYLE_ASSIGNMENT (( #47820 ) ) ;
#48139 = DIRECTION ( 'NONE',  ( -0.000000000000000000, -1.000000000000000000, 0.000000000000000000 ) ) ;
#48140 = EDGE_CURVE ( 'NONE', #12229, #53126, #59751, .T. ) ;
#48141 = FACE_OUTER_BOUND ( 'NONE', #40415, .T. ) ;
#48142 = DIRECTION ( 'NONE',  ( -1.156482317317870344E-15, 1.000000000000000000, 0.000000000000000000 ) ) ;
#48143 = CARTESIAN_POINT ( 'NONE',  ( 71.62068965517238439, 63.58603185604027885, 7.500000000000000000 ) ) ;
#48144 = EDGE_LOOP ( 'NONE', ( #21332, #28888, #13283, #48197 ) ) ;
#48145 =( GEOMETRIC_REPRESENTATION_CONTEXT ( 3 ) GLOBAL_UNCERTAINTY_ASSIGNED_CONTEXT ( ( #28278 ) ) GLOBAL_UNIT_ASSIGNED_CONTEXT ( ( #61316, #39560, #2881 ) ) REPRESENTATION_CONTEXT ( 'NONE', 'WORKASPACE' ) );
#48146 = VERTEX_POINT ( 'NONE', #17547 ) ;
#48147 = CARTESIAN_POINT ( 'NONE',  ( 0.000000000000000000, 0.000000000000000000, 7.500000000000000000 ) ) ;
#48148 = CARTESIAN_POINT ( 'NONE',  ( -22.25000000000000711, 34.24999999999999289, 3.750000000000000000 ) ) ;
#48149 = DIRECTION ( 'NONE',  ( -0.000000000000000000, -0.000000000000000000, -1.000000000000000000 ) ) ;
#48150 =( LENGTH_UNIT ( ) NAMED_UNIT ( * ) SI_UNIT ( .MILLI., .METRE. ) );
#48151 = ORIENTED_EDGE ( 'NONE', *, *, #22717, .F. ) ;
#48152 = CARTESIAN_POINT ( 'NONE',  ( -164.7549999999999955, 4.716976649647091513, -6.492361379858946790 ) ) ;
#48153 = SURFACE_SIDE_STYLE ('',( #5186 ) ) ;
#48154 = DIRECTION ( 'NONE',  ( 0.000000000000000000, 0.000000000000000000, 1.000000000000000000 ) ) ;
#48155 = CARTESIAN_POINT ( 'NONE',  ( -179.6949999999999932, -8.437984349512085203, 5.166775262442717831E-16 ) ) ;
#48156 = CARTESIAN_POINT ( 'NONE',  ( -164.8449999999999989, -7.632228543268599452, 2.479861379858951054 ) ) ;
#48157 = ORIENTED_EDGE ( 'NONE', *, *, #52356, .F. ) ;
#48158 = PRODUCT_DEFINITION ( 'UNKNOWN', '', #6777, #17784 ) ;
#48159 = CYLINDRICAL_SURFACE ( 'NONE', #16743, 1.000000000000000888 ) ;
#48160 = EDGE_CURVE ( 'NONE', #62390, #58089, #18366, .T. ) ;
#48161 = FACE_OUTER_BOUND ( 'NONE', #62148, .T. ) ;
#48162 = EDGE_CURVE ( 'NONE', #55582, #36075, #38323, .T. ) ;
#48163 = CARTESIAN_POINT ( 'NONE',  ( -85.10499999999997556, -6.826472737025115478, 4.959722759717900331 ) ) ;
#48164 = DIRECTION ( 'NONE',  ( -1.000000000000000000, -0.000000000000000000, -0.000000000000000000 ) ) ;
#48165 = CARTESIAN_POINT ( 'NONE',  ( 23.85059380760285563, 27.39840537729088510, 27.20962804606061880 ) ) ;
#48166 = CARTESIAN_POINT ( 'NONE',  ( -75.00479156420786353, 35.98735966460310465, -9.505900230725330857 ) ) ;
#48167 = EDGE_CURVE ( 'NONE', #48050, #8636, #66965, .T. ) ;
#48168 = CARTESIAN_POINT ( 'NONE',  ( -80.09499999999998465, -2.607480562269071545, -8.024999999999991473 ) ) ;
#48169 = EDGE_CURVE ( 'NONE', #3561, #68782, #33354, .T. ) ;
#48170 = CARTESIAN_POINT ( 'NONE',  ( -8.102448949553181734, 138.0049999999999670, -5.886773742842749790 ) ) ;
#48171 = SURFACE_SIDE_STYLE ('',( #32996 ) ) ;
#48172 = CARTESIAN_POINT ( 'NONE',  ( -170.9929263765338021, 8.102448949553172852, -5.886773742842744461 ) ) ;
#48173 = DIRECTION ( 'NONE',  ( -0.000000000000000000, -1.000000000000000000, 0.000000000000000000 ) ) ;
#48174 = UNCERTAINTY_MEASURE_WITH_UNIT (LENGTH_MEASURE( 1.000000000000000082E-05 ), #55580, 'distance_accuracy_value', 'NONE');
#48175 = CARTESIAN_POINT ( 'NONE',  ( -75.14292637653380780, 5.598654528085800663, -7.705886871421367523 ) ) ;
#48176 = EDGE_LOOP ( 'NONE', ( #3576, #21632, #32053, #41227 ) ) ;
#48177 = ADVANCED_FACE ( 'NONE', ( #37987 ), #1463, .T. ) ;
#48178 = VECTOR ( 'NONE', #52478, 1000.000000000000000 ) ;
#48179 = CARTESIAN_POINT ( 'NONE',  ( -6.826472737025120807, 132.3929263765338362, -4.959722759717907437 ) ) ;
#48180 = ADVANCED_FACE ( 'NONE', ( #43276 ), #901, .F. ) ;
#48181 = VECTOR ( 'NONE', #7104, 1000.000000000000000 ) ;
#48182 = CARTESIAN_POINT ( 'NONE',  ( 22.00000000000000711, 50.00000000000000000, -60.00000000000000711 ) ) ;
#48184 = FILL_AREA_STYLE_COLOUR ( '', #28089 ) ;
#48183 = DIRECTION ( 'NONE',  ( 0.000000000000000000, 1.000000000000000000, 0.000000000000000000 ) ) ;
#48185 = ORIENTED_EDGE ( 'NONE', *, *, #34768, .F. ) ;
#48186 = ORIENTED_EDGE ( 'NONE', *, *, #6342, .T. ) ;
#48187 = CARTESIAN_POINT ( 'NONE',  ( -134.8429263765337964, 9.058813317711329915, -2.943386871421373119 ) ) ;
#48189 = AXIS2_PLACEMENT_3D ( 'NONE', #43901, #65310, #17155 ) ;
#48188 = UNCERTAINTY_MEASURE_WITH_UNIT (LENGTH_MEASURE( 1.000000000000000082E-05 ), #52735, 'distance_accuracy_value', 'NONE');
#48190 = CARTESIAN_POINT ( 'NONE',  ( -45.00000000000000000, 7.768687147774684831, -6.999999999999999112 ) ) ;
#48191 = CIRCLE ( 'NONE', #24525, 0.5000000000000004441 ) ;
#48192 = CYLINDRICAL_SURFACE ( 'NONE', #48745, 2.000000000000003553 ) ;
#48194 = CARTESIAN_POINT ( 'NONE',  ( 4.716976649647096842, 139.7429263765338305, 6.492361379858953896 ) ) ;
#48193 = CONICAL_SURFACE ( 'NONE', #6549, 6.999999999999997335, 0.7853981633974500554 ) ;
#48195 = VERTEX_POINT ( 'NONE', #60079 ) ;
#48196 = CARTESIAN_POINT ( 'NONE',  ( -119.6049999999999756, 6.826472737025113702, -4.959722759717902107 ) ) ;
#48197 = ORIENTED_EDGE ( 'NONE', *, *, #7661, .T. ) ;
#48198 = CARTESIAN_POINT ( 'NONE',  ( -136.8570736234661638, -5.598654528085803328, -7.705886871421366635 ) ) ;
#48199 = CARTESIAN_POINT ( 'NONE',  ( 19.89974874213240597, 115.4999999999999574, -10.00000000000000000 ) ) ;
#48200 = VERTEX_POINT ( 'NONE', #54780 ) ;
#48201 = ORIENTED_EDGE ( 'NONE', *, *, #61937, .F. ) ;
#48202 = AXIS2_PLACEMENT_3D ( 'NONE', #48704, #6426, #49047 ) ;
#48203 = ADVANCED_FACE ( 'NONE', ( #44308 ), #37539, .T. ) ;
#48204 = CARTESIAN_POINT ( 'NONE',  ( 3.094860106618431583, 153.0949999999999989, 9.525000000000000355 ) ) ;
#48205 = FILL_AREA_STYLE_COLOUR ( '', #45315 ) ;
#48206 = ORIENTED_EDGE ( 'NONE', *, *, #45843, .T. ) ;
#48207 = CARTESIAN_POINT ( 'NONE',  ( -22.75000000000000711, 37.00000000000000000, 3.750000000000000000 ) ) ;
#48208 = DIRECTION ( 'NONE',  ( 0.000000000000000000, -1.000000000000000000, 0.000000000000000000 ) ) ;
#48209 = CARTESIAN_POINT ( 'NONE',  ( -130.3429263765337964, -9.058813317711329915, 2.943386871421371787 ) ) ;
#48210 = ORIENTED_EDGE ( 'NONE', *, *, #60971, .F. ) ;
#48211 = CARTESIAN_POINT ( 'NONE',  ( -2.607480562269073765, 123.0929263765338106, -8.025000000000000355 ) ) ;
#48212 = CARTESIAN_POINT ( 'NONE',  ( -9.827790563157511022E-16, 139.4429263765338192, 8.025000000000000355 ) ) ;
#48213 = UNCERTAINTY_MEASURE_WITH_UNIT (LENGTH_MEASURE( 1.000000000000000082E-05 ), #86, 'distance_accuracy_value', 'NONE');
#48214 = AXIS2_PLACEMENT_3D ( 'NONE', #15105, #56937, #4133 ) ;
#48215 = LINE ( 'NONE', #57343, #55301 ) ;
#48216 = DIRECTION ( 'NONE',  ( -0.000000000000000000, -0.000000000000000000, 1.000000000000000000 ) ) ;
#48217 = ORIENTED_EDGE ( 'NONE', *, *, #56710, .T. ) ;
#48218 = DIRECTION ( 'NONE',  ( 1.000000000000000000, 0.000000000000000000, 0.000000000000000000 ) ) ;
#48219 = EDGE_LOOP ( 'NONE', ( #57632, #10106, #21082, #14055 ) ) ;
#48220 =( NAMED_UNIT ( * ) SI_UNIT ( $, .STERADIAN. ) SOLID_ANGLE_UNIT ( ) );
#48221 = CARTESIAN_POINT ( 'NONE',  ( -142.2549999999999955, -4.716976649647092401, 6.492361379858946790 ) ) ;
#48222 = CARTESIAN_POINT ( 'NONE',  ( -7.335726704534230258, -2.464278740834323411, -5.294148637306920868 ) ) ;
#48223 = DIRECTION ( 'NONE',  ( -1.000000000000000000, 0.000000000000000000, 0.000000000000000000 ) ) ;
#48224 = UNCERTAINTY_MEASURE_WITH_UNIT (LENGTH_MEASURE( 1.000000000000000082E-05 ), #19992, 'distance_accuracy_value', 'NONE');
#48225 = CIRCLE ( 'NONE', #63879, 0.5000000000000004441 ) ;
#48226 = PLANE ( 'NONE',  #63190 ) ;
#48227 = CARTESIAN_POINT ( 'NONE',  ( 41.84210526315787604, 107.2928455055531458, 3.500000000000011102 ) ) ;
#48228 =( NAMED_UNIT ( * ) SI_UNIT ( $, .STERADIAN. ) SOLID_ANGLE_UNIT ( ) );
#48229 = VERTEX_POINT ( 'NONE', #46011 ) ;
#48230 = ORIENTED_EDGE ( 'NONE', *, *, #18379, .F. ) ;
#48231 = DIRECTION ( 'NONE',  ( -1.000000000000000000, -1.387778780781444256E-14, 0.000000000000000000 ) ) ;
#48232 = CARTESIAN_POINT ( 'NONE',  ( 39.74999999999999289, 18.74999999999997868, 4.000000000000000000 ) ) ;
#48233 = CARTESIAN_POINT ( 'NONE',  ( -57.50499999999997414, -6.826472737025115478, -4.959722759717899443 ) ) ;
#48234 = ORIENTED_EDGE ( 'NONE', *, *, #31777, .T. ) ;
#48235 = CARTESIAN_POINT ( 'NONE',  ( 31.00000000000002132, 43.00000000000000000, 75.00000000000000000 ) ) ;
#48236 = DIRECTION ( 'NONE',  ( 0.000000000000000000, -1.000000000000000000, 0.000000000000000000 ) ) ;
#48237 = MECHANICAL_DESIGN_GEOMETRIC_PRESENTATION_REPRESENTATION (  '', ( #32412 ), #9995 ) ;
#48238 = CARTESIAN_POINT ( 'NONE',  ( -15.98999599679679839, 117.9999999999999716, -7.000000000000000000 ) ) ;
#48239 = STYLED_ITEM ( 'NONE', ( #2251 ), #4435 ) ;
#48240 = EDGE_LOOP ( 'NONE', ( #12238, #29675, #48315, #58850 ) ) ;
#48241 = EDGE_CURVE ( 'NONE', #15321, #61387, #67430, .T. ) ;
#48242 = CARTESIAN_POINT ( 'NONE',  ( -34.99999999999999289, 99.99999999999998579, 10.00000000000000000 ) ) ;
#48243 = DIRECTION ( 'NONE',  ( 1.000000000000000000, 0.000000000000000000, -0.000000000000000000 ) ) ;
#48244 = AXIS2_PLACEMENT_3D ( 'NONE', #66844, #55219, #29163 ) ;
#48245 = AXIS2_PLACEMENT_3D ( 'NONE', #55648, #19391, #67593 ) ;
#48246 = EDGE_CURVE ( 'NONE', #8864, #51444, #45412, .T. ) ;
#48247 = CARTESIAN_POINT ( 'NONE',  ( -110.8449999999999847, -7.632228543268599452, 2.479861379858951054 ) ) ;
#48248 = CARTESIAN_POINT ( 'NONE',  ( 9.058813317711338797, 156.8449999999999704, -2.943386871421372675 ) ) ;
#48249 = CARTESIAN_POINT ( 'NONE',  ( -88.34499999999999886, 7.632228543268599452, -2.479861379858951942 ) ) ;
#48250 = LINE ( 'NONE', #59434, #62307 ) ;
#48251 = CIRCLE ( 'NONE', #5494, 5.000000000000004441 ) ;
#48252 = LINE ( 'NONE', #10251, #58375 ) ;
#48253 = DIRECTION ( 'NONE',  ( 1.000000000000000000, 0.000000000000000000, 0.000000000000000000 ) ) ;
#48254 = UNCERTAINTY_MEASURE_WITH_UNIT (LENGTH_MEASURE( 1.000000000000000082E-05 ), #27628, 'distance_accuracy_value', 'NONE');
#48255 = AXIS2_PLACEMENT_3D ( 'NONE', #45888, #3244, #35322 ) ;
#48256 = DIRECTION ( 'NONE',  ( 0.000000000000000000, 0.000000000000000000, -1.000000000000000000 ) ) ;
#48257 = ORIENTED_EDGE ( 'NONE', *, *, #58856, .F. ) ;
#48258 = CARTESIAN_POINT ( 'NONE',  ( -138.5929263765338249, -3.094860106618431139, -9.524999999999991473 ) ) ;
#48259 = CARTESIAN_POINT ( 'NONE',  ( -145.7950000000000443, 2.607480562269068880, -8.024999999999993250 ) ) ;
#48260 = CARTESIAN_POINT ( 'NONE',  ( -72.49999999999998579, 119.9999999999997868, -10.00000000000000000 ) ) ;
#48261 = EDGE_CURVE ( 'NONE', #20470, #22693, #64449, .T. ) ;
#48262 = CARTESIAN_POINT ( 'NONE',  ( -66.05707362346618083, 0.000000000000000000, 9.524999999999991473 ) ) ;
#48263 = DIRECTION ( 'NONE',  ( -0.000000000000000000, -0.000000000000000000, 1.000000000000000000 ) ) ;
#48264 = ORIENTED_EDGE ( 'NONE', *, *, #52231, .T. ) ;
#48265 = ORIENTED_EDGE ( 'NONE', *, *, #41743, .T. ) ;
#48266 =( GEOMETRIC_REPRESENTATION_CONTEXT ( 3 ) GLOBAL_UNCERTAINTY_ASSIGNED_CONTEXT ( ( #13696 ) ) GLOBAL_UNIT_ASSIGNED_CONTEXT ( ( #38964, #44590, #60365 ) ) REPRESENTATION_CONTEXT ( 'NONE', 'WORKASPACE' ) );
#48267 = CYLINDRICAL_SURFACE ( 'NONE', #25135, 8.499999999999992895 ) ;
#48268 = CIRCLE ( 'NONE', #42651, 0.5000000000000004441 ) ;
#48269 = CARTESIAN_POINT ( 'NONE',  ( -45.88781401545035266, 9.325134922070681398, 6.185423913763131942 ) ) ;
#48270 = CARTESIAN_POINT ( 'NONE',  ( -130.4070736234668573, 3.094860106607471018, -9.525000000007956658 ) ) ;
#48271 = STYLED_ITEM ( 'NONE', ( #44452 ), #43186 ) ;
#48272 = EDGE_LOOP ( 'NONE', ( #61640, #24404 ) ) ;
#48273 = CARTESIAN_POINT ( 'NONE',  ( -147.9550000000000125, -7.632228543268599452, 2.479861379858951054 ) ) ;
#48274 = EDGE_CURVE ( 'NONE', #13649, #60291, #51266, .T. ) ;
#48275 = ORIENTED_EDGE ( 'NONE', *, *, #16402, .T. ) ;
#48276 = CARTESIAN_POINT ( 'NONE',  ( 0.000000000000000000, -2.500000000000000000, 0.000000000000000000 ) ) ;
#48277 = ORIENTED_EDGE ( 'NONE', *, *, #54620, .F. ) ;
#48278 = AXIS2_PLACEMENT_3D ( 'NONE', #29700, #66283, #44543 ) ;
#48279 = TOROIDAL_SURFACE ( 'NONE', #16786, 18.53939201416945082, 5.000000000000000000 ) ;
#48280 = CARTESIAN_POINT ( 'NONE',  ( -56.61586366453234831, -8.492381958573840706, -1.066368904513279592 ) ) ;
#48281 = EDGE_CURVE ( 'NONE', #26061, #68565, #39649, .T. ) ;
#48282 = DIRECTION ( 'NONE',  ( 1.000000000000000000, 0.000000000000000000, 0.000000000000000000 ) ) ;
#48283 = COLOUR_RGB ( '', 0.09019608, 0.27058824, 0.51372549) ;
#48284 = CARTESIAN_POINT ( 'NONE',  ( 5.598654528085809545, 124.1449999999999960, -7.705886871421373741 ) ) ;
#48285 = LINE ( 'NONE', #59475, #9292 ) ;
#48286 =( GEOMETRIC_REPRESENTATION_CONTEXT ( 3 ) GLOBAL_UNCERTAINTY_ASSIGNED_CONTEXT ( ( #67732 ) ) GLOBAL_UNIT_ASSIGNED_CONTEXT ( ( #9636, #62381, #25775 ) ) REPRESENTATION_CONTEXT ( 'NONE', 'WORKASPACE' ) );
#48287 =( BOUNDED_CURVE ( )  B_SPLINE_CURVE ( 2, ( #11897, #43953, #33358, #11546, #33017, #54786, #65369, #42927, #6597, #53763, #28039 ),
 .UNSPECIFIED., .F., .F. ) 
 B_SPLINE_CURVE_WITH_KNOTS ( ( 3, 2, 2, 2, 2, 3 ),
 ( 0.8152173913043477826, 0.8173913043478261420, 0.8195652173913043903, 0.8217391304347826386, 0.8239130434782608869, 0.8260869565217391353 ),
 .UNSPECIFIED. ) 
 CURVE ( )  GEOMETRIC_REPRESENTATION_ITEM ( )  RATIONAL_B_SPLINE_CURVE ( ( 1.000000000000000000, 0.9510565162951535312, 1.000000000000000000, 0.9510565162951535312, 1.000000000000000000, 0.9510565162951535312, 1.000000000000000000, 0.9510565162951535312, 1.000000000000000000, 0.9510565162951535312, 1.000000000000000000 ) ) 
 REPRESENTATION_ITEM ( '' )  );
#48288 = AXIS2_PLACEMENT_3D ( 'NONE', #2935, #51885, #46650 ) ;
#48289 = ORIENTED_EDGE ( 'NONE', *, *, #31423, .F. ) ;
#48290 = CARTESIAN_POINT ( 'NONE',  ( 9.058813317711337021, 118.6549999999999869, 2.943386871421375783 ) ) ;
#48291 = CARTESIAN_POINT ( 'NONE',  ( -63.65499999999998693, -7.632228543268600340, -2.479861379858950166 ) ) ;
#48292 = CARTESIAN_POINT ( 'NONE',  ( -117.1449999999999818, -4.716976649647092401, 6.492361379858946790 ) ) ;
#48293 = AXIS2_PLACEMENT_3D ( 'NONE', #3959, #20139, #62700 ) ;
#48294 = DIRECTION ( 'NONE',  ( -0.000000000000000000, 1.000000000000000000, -0.000000000000000000 ) ) ;
#48295 = ORIENTED_EDGE ( 'NONE', *, *, #4758, .T. ) ;
#48296 = CARTESIAN_POINT ( 'NONE',  ( 3.094860106618435136, 143.4049999999999443, -9.525000000000000355 ) ) ;
#48297 = SURFACE_SIDE_STYLE ('',( #30397 ) ) ;
#48298 = UNCERTAINTY_MEASURE_WITH_UNIT (LENGTH_MEASURE( 1.000000000000000082E-05 ), #9974, 'distance_accuracy_value', 'NONE');
#48299 = AXIS2_PLACEMENT_3D ( 'NONE', #23148, #12205, #66032 ) ;
#48300 = DIRECTION ( 'NONE',  ( -0.000000000000000000, -0.000000000000000000, 1.000000000000000000 ) ) ;
#48301 = CARTESIAN_POINT ( 'NONE',  ( 20.57648123223239622, 114.4999999999999574, 10.27659574468085246 ) ) ;
#48302 = FACE_OUTER_BOUND ( 'NONE', #53201, .T. ) ;
#48303 = EDGE_LOOP ( 'NONE', ( #36642, #14405, #2864, #54037 ) ) ;
#48304 = MECHANICAL_DESIGN_GEOMETRIC_PRESENTATION_REPRESENTATION (  '', ( #2096 ), #2131 ) ;
#48305 = DIRECTION ( 'NONE',  ( 0.000000000000000000, -0.000000000000000000, 1.000000000000000000 ) ) ;
#48306 = CARTESIAN_POINT ( 'NONE',  ( -169.4049999999999727, -2.607480562269069768, 8.024999999999991473 ) ) ;
#48307 = ORIENTED_EDGE ( 'NONE', *, *, #6051, .F. ) ;
#48308 = CARTESIAN_POINT ( 'NONE',  ( 62.24999999999998579, 33.99999999999999289, -3.750000000000000000 ) ) ;
#48309 = UNCERTAINTY_MEASURE_WITH_UNIT (LENGTH_MEASURE( 1.000000000000000082E-05 ), #47805, 'distance_accuracy_value', 'NONE');
#48310 = VECTOR ( 'NONE', #35060, 1000.000000000000000 ) ;
#48311 = FACE_OUTER_BOUND ( 'NONE', #25681, .T. ) ;
#48312 = CYLINDRICAL_SURFACE ( 'NONE', #44258, 0.5000000000000004441 ) ;
#48313 = CARTESIAN_POINT ( 'NONE',  ( 8.246138225238281549, -2.499999999999997780, 3.717269627651450303 ) ) ;
#48314 = FACE_OUTER_BOUND ( 'NONE', #47112, .T. ) ;
#48315 = ORIENTED_EDGE ( 'NONE', *, *, #58370, .T. ) ;
#48316 = CIRCLE ( 'NONE', #61746, 4.750000000000000000 ) ;
#48317 = PLANE ( 'NONE',  #2396 ) ;
#48318 = CARTESIAN_POINT ( 'NONE',  ( -95.60499999999998977, 6.826472737025113702, -4.959722759717902107 ) ) ;
#48319 = ORIENTED_EDGE ( 'NONE', *, *, #1085, .F. ) ;
#48320 = CARTESIAN_POINT ( 'NONE',  ( -46.64499999999998892, 4.716976649647091513, -6.492361379858946790 ) ) ;
#48321 = ADVANCED_FACE ( 'NONE', ( #23473 ), #13261, .F. ) ;
#48322 = CARTESIAN_POINT ( 'NONE',  ( -134.4570736234661865, -9.058813317711329915, 2.943386871421371787 ) ) ;
#48323 = AXIS2_PLACEMENT_3D ( 'NONE', #58217, #63150, #68428 ) ;
#48324 = MECHANICAL_DESIGN_GEOMETRIC_PRESENTATION_REPRESENTATION (  '', ( #39323 ), #50496 ) ;
#48325 = FACE_OUTER_BOUND ( 'NONE', #69093, .T. ) ;
#48326 = FACE_OUTER_BOUND ( 'NONE', #38011, .T. ) ;
#48327 = CARTESIAN_POINT ( 'NONE',  ( -68.45707362346617231, -9.058813317711329915, 2.943386871421371787 ) ) ;
#48328 = VECTOR ( 'NONE', #58098, 1000.000000000000000 ) ;
#48329 = EDGE_LOOP ( 'NONE', ( #5325, #63487, #58371, #10472 ) ) ;
#48330 = CARTESIAN_POINT ( 'NONE',  ( 0.000000000000000000, 2.500000000000000000, 0.000000000000000000 ) ) ;
#48331 = DIRECTION ( 'NONE',  ( 0.000000000000000000, 0.000000000000000000, -1.000000000000000000 ) ) ;
#48333 = DIRECTION ( 'NONE',  ( 0.000000000000000000, 0.000000000000000000, 1.000000000000000000 ) ) ;
#48332 = FILL_AREA_STYLE ('',( #11341 ) ) ;
#48334 = CARTESIAN_POINT ( 'NONE',  ( -108.2049999999999983, -2.607480562269071545, -8.024999999999991473 ) ) ;
#48335 = ADVANCED_FACE ( 'NONE', ( #25218 ), #51969, .F. ) ;
#48336 = CARTESIAN_POINT ( 'NONE',  ( -9.058813317711338797, 116.3449999999999847, 2.943386871421373563 ) ) ;
#48337 = CARTESIAN_POINT ( 'NONE',  ( -112.9449999999999932, -9.827790563157499189E-16, -8.024999999999991473 ) ) ;
#48338 = CIRCLE ( 'NONE', #6703, 0.2500000000000002220 ) ;
#48339 = AXIS2_PLACEMENT_3D ( 'NONE', #66126, #27094, #44395 ) ;
#48340 = ADVANCED_FACE ( 'NONE', ( #3726 ), #20641, .F. ) ;
#48341 = AXIS2_PLACEMENT_3D ( 'NONE', #17302, #39795, #39447 ) ;
#48342 = CARTESIAN_POINT ( 'NONE',  ( 28.00000000000002132, 43.00000000000000000, 90.00000000000000000 ) ) ;
#48343 = EDGE_CURVE ( 'NONE', #54480, #17044, #31522, .T. ) ;
#48344 = ORIENTED_EDGE ( 'NONE', *, *, #62077, .T. ) ;
#48345 = CARTESIAN_POINT ( 'NONE',  ( -164.9929263765338305, 8.102448949553171076, -5.886773742842744461 ) ) ;
#48346 = CARTESIAN_POINT ( 'NONE',  ( -181.0449999999999875, 7.632228543268600340, 2.479861379858949277 ) ) ;
#48347 = COLOUR_RGB ( '', 0.09019608, 0.27058824, 0.51372549) ;
#48348 = ADVANCED_FACE ( 'NONE', ( #53003 ), #26582, .T. ) ;
#48349 = CARTESIAN_POINT ( 'NONE',  ( 0.000000000000000000, 87.30187232391182306, 0.000000000000000000 ) ) ;
#48350 = PRESENTATION_LAYER_ASSIGNMENT (  '', '', ( #19115 ) ) ;
#48351 = DIRECTION ( 'NONE',  ( 0.000000000000000000, 0.000000000000000000, 1.000000000000000000 ) ) ;
#48352 = DIRECTION ( 'NONE',  ( -0.2413793103448194644, -0.9704308468600220117, 0.000000000000000000 ) ) ;
#48353 = CYLINDRICAL_SURFACE ( 'NONE', #49519, 0.5000000000000004441 ) ;
#48354 = ORIENTED_EDGE ( 'NONE', *, *, #54378, .T. ) ;
#48355 = CARTESIAN_POINT ( 'NONE',  ( -72.44292637653379074, -1.166476076187852838E-15, -9.524999999999991473 ) ) ;
#48356 = AXIS2_PLACEMENT_3D ( 'NONE', #63701, #32726, #10595 ) ;
#48357 = CARTESIAN_POINT ( 'NONE',  ( -75.00000000000000000, 67.00000000000000000, 6.500000000000000000 ) ) ;
#48358 = CARTESIAN_POINT ( 'NONE',  ( -25.00000000000000000, 1.000000000000000000, 3.000000000000000000 ) ) ;
#48359 = PRESENTATION_LAYER_ASSIGNMENT (  '', '', ( #28095 ) ) ;
#48360 =( LENGTH_UNIT ( ) NAMED_UNIT ( * ) SI_UNIT ( .MILLI., .METRE. ) );
#48361 =( LENGTH_UNIT ( ) NAMED_UNIT ( * ) SI_UNIT ( .MILLI., .METRE. ) );
#48362 = CARTESIAN_POINT ( 'NONE',  ( -44.99999999999977263, 147.4999999999999716, 9.500000000000000000 ) ) ;
#48363 = PRESENTATION_LAYER_ASSIGNMENT (  '', '', ( #1090 ) ) ;
#48364 = CARTESIAN_POINT ( 'NONE',  ( -182.3049999999999784, 8.437984349512086979, -1.550032578732815448E-15 ) ) ;
#48365 = VERTEX_POINT ( 'NONE', #827 ) ;
#48366 = CARTESIAN_POINT ( 'NONE',  ( -195.0000000000000000, 0.000000000000000000, 0.000000000000000000 ) ) ;
#48367 = CARTESIAN_POINT ( 'NONE',  ( 68.99999999999998579, 36.75000000000000000, -3.750000000000000000 ) ) ;
#48368 =( LENGTH_UNIT ( ) NAMED_UNIT ( * ) SI_UNIT ( .MILLI., .METRE. ) );
#48369 =( GEOMETRIC_REPRESENTATION_CONTEXT ( 3 ) GLOBAL_UNCERTAINTY_ASSIGNED_CONTEXT ( ( #56610 ) ) GLOBAL_UNIT_ASSIGNED_CONTEXT ( ( #54495, #37691, #48581 ) ) REPRESENTATION_CONTEXT ( 'NONE', 'WORKASPACE' ) );
#48370 =( NAMED_UNIT ( * ) SI_UNIT ( $, .STERADIAN. ) SOLID_ANGLE_UNIT ( ) );
#48371 = CARTESIAN_POINT ( 'NONE',  ( -7.632228543268608334, 142.9570736234661581, 2.479861379858952830 ) ) ;
#48372 = VERTEX_POINT ( 'NONE', #65273 ) ;
#48373 = AXIS2_PLACEMENT_3D ( 'NONE', #36226, #57654, #50990 ) ;
#48374 = CARTESIAN_POINT ( 'NONE',  ( 44.50000000000000000, 10.36037961002804408, -3.500000000000000000 ) ) ;
#48375 = CARTESIAN_POINT ( 'NONE',  ( -96.05499999999999261, -9.827790563157499189E-16, -8.024999999999991473 ) ) ;
#48376 = UNCERTAINTY_MEASURE_WITH_UNIT (LENGTH_MEASURE( 1.000000000000000082E-05 ), #64071, 'distance_accuracy_value', 'NONE');
#48377 = ORIENTED_EDGE ( 'NONE', *, *, #18285, .T. ) ;
#48378 = SURFACE_STYLE_FILL_AREA ( #1108 ) ;
#48379 = PRESENTATION_STYLE_ASSIGNMENT (( #53946 ) ) ;
#48380 = CARTESIAN_POINT ( 'NONE',  ( -34.07680040766327068, -9.981484022772619369, -3.029036331924419123 ) ) ;
#48381 = CARTESIAN_POINT ( 'NONE',  ( 21.24999999999998579, -2.457524924300472510E-14, 4.000000000000000000 ) ) ;
#48382 = MECHANICAL_DESIGN_GEOMETRIC_PRESENTATION_REPRESENTATION (  '', ( #14660 ), #36007 ) ;
#48384 = AXIS2_PLACEMENT_3D ( 'NONE', #23526, #56226, #29131 ) ;
#48383 = CARTESIAN_POINT ( 'NONE',  ( 23.85401998315348493, 27.39726515740571244, -27.21013614952132542 ) ) ;
#48385 = ORIENTED_EDGE ( 'NONE', *, *, #33742, .F. ) ;
#48386 = CARTESIAN_POINT ( 'NONE',  ( -75.89499999999998181, 6.826472737025116366, 4.959722759717898555 ) ) ;
#48388 = EDGE_LOOP ( 'NONE', ( #7183, #67382, #12153, #17150 ) ) ;
#48387 = VECTOR ( 'NONE', #62583, 1000.000000000000000 ) ;
#48389 = DIRECTION ( 'NONE',  ( -1.000000000000000000, 0.000000000000000000, -0.000000000000000000 ) ) ;
#48390 = DIRECTION ( 'NONE',  ( -1.000000000000000000, 0.000000000000000000, 0.000000000000000000 ) ) ;
#48391 = FACE_OUTER_BOUND ( 'NONE', #61993, .T. ) ;
#48392 = COLOUR_RGB ( '', 0.31764706, 0.68627451, 0.89019608) ;
#48393 = ORIENTED_EDGE ( 'NONE', *, *, #49336, .F. ) ;
#48394 = SURFACE_STYLE_FILL_AREA ( #39215 ) ;
#48395 = FILL_AREA_STYLE_COLOUR ( '', #47171 ) ;
#48396 =( NAMED_UNIT ( * ) PLANE_ANGLE_UNIT ( ) SI_UNIT ( $, .RADIAN. ) );
#48397 = CARTESIAN_POINT ( 'NONE',  ( -127.7049999999999699, 2.607480562269073321, 8.024999999999991473 ) ) ;
#48398 = ORIENTED_EDGE ( 'NONE', *, *, #5614, .F. ) ;
#48399 = CARTESIAN_POINT ( 'NONE',  ( 31.53557507391671066, 42.85561104658233944, -45.52242297229209811 ) ) ;
#48400 = CIRCLE ( 'NONE', #33735, 1.000000000000000888 ) ;
#48402 = ORIENTED_EDGE ( 'NONE', *, *, #53531, .T. ) ;
#48401 = EDGE_CURVE ( 'NONE', #17294, #46540, #53314, .T. ) ;
#48403 = CARTESIAN_POINT ( 'NONE',  ( -45.00000000000000000, -1.469576158976824302E-14, -9.500000000000000000 ) ) ;
#48404 = CARTESIAN_POINT ( 'NONE',  ( 4.041451884327379673, -7.000000000000002665, 7.500000000000000000 ) ) ;
#48405 = CARTESIAN_POINT ( 'NONE',  ( -162.8070736234661808, 10.01517768586948698, -1.839758294383808571E-15 ) ) ;
#48406 = AXIS2_PLACEMENT_3D ( 'NONE', #30908, #29525, #24939 ) ;
#48407 = CARTESIAN_POINT ( 'NONE',  ( -1.166476076187854022E-15, 125.9449999999999790, 9.525000000000000355 ) ) ;
#48408 = EDGE_CURVE ( 'NONE', #54091, #58809, #9480, .T. ) ;
#48409 = CARTESIAN_POINT ( 'NONE',  ( -91.10707362346619220, 8.102448949553171076, -5.886773742842744461 ) ) ;
#48410 = AXIS2_PLACEMENT_3D ( 'NONE', #5125, #58602, #53664 ) ;
#48411 = ADVANCED_FACE ( 'NONE', ( #26912 ), #36472, .T. ) ;
#48412 = ORIENTED_EDGE ( 'NONE', *, *, #4183, .F. ) ;
#48413 = MECHANICAL_DESIGN_GEOMETRIC_PRESENTATION_REPRESENTATION (  '', ( #57366 ), #15863 ) ;
#48414 = PRESENTATION_STYLE_ASSIGNMENT (( #5106 ) ) ;
#48415 = EDGE_CURVE ( 'NONE', #44000, #6894, #6510, .T. ) ;
#48417 = FILL_AREA_STYLE_COLOUR ( '', #40345 ) ;
#48416 = DIRECTION ( 'NONE',  ( 0.000000000000000000, 0.000000000000000000, -1.000000000000000000 ) ) ;
#48418 = CARTESIAN_POINT ( 'NONE',  ( -138.0549999999999784, -9.827790563157499189E-16, -8.024999999999991473 ) ) ;
#48419 = EDGE_CURVE ( 'NONE', #26152, #320, #13970, .T. ) ;
#48420 =( NAMED_UNIT ( * ) SI_UNIT ( $, .STERADIAN. ) SOLID_ANGLE_UNIT ( ) );
#48421 = FACE_OUTER_BOUND ( 'NONE', #33365, .T. ) ;
#48422 = CARTESIAN_POINT ( 'NONE',  ( -149.2449999999999761, -4.716976649647093289, -6.492361379858945902 ) ) ;
#48423 = EDGE_CURVE ( 'NONE', #8149, #26431, #24070, .T. ) ;
#48424 = CARTESIAN_POINT ( 'NONE',  ( -134.8449999999999989, -7.632228543268599452, 2.479861379858951054 ) ) ;
#48425 = STYLED_ITEM ( 'NONE', ( #9129 ), #59640 ) ;
#48426 = EDGE_CURVE ( 'NONE', #27627, #65906, #59643, .T. ) ;
#48427 = EDGE_LOOP ( 'NONE', ( #6958, #1644, #11402, #41372, #45788, #23552, #59135, #47714, #30094, #39044, #3807, #57251 ) ) ;
#48428 = CARTESIAN_POINT ( 'NONE',  ( 45.00050070149897152, 10.00016690049880630, -3.905286714425280969 ) ) ;
#48429 = DIRECTION ( 'NONE',  ( -0.000000000000000000, -1.000000000000000000, 0.000000000000000000 ) ) ;
#48430 =( GEOMETRIC_REPRESENTATION_CONTEXT ( 3 ) GLOBAL_UNCERTAINTY_ASSIGNED_CONTEXT ( ( #803 ) ) GLOBAL_UNIT_ASSIGNED_CONTEXT ( ( #47965, #9934, #52855 ) ) REPRESENTATION_CONTEXT ( 'NONE', 'WORKASPACE' ) );
#48431 = EDGE_CURVE ( 'NONE', #46789, #40883, #16769, .T. ) ;
#48433 = VECTOR ( 'NONE', #40799, 1000.000000000000000 ) ;
#48432 = DIRECTION ( 'NONE',  ( 0.000000000000000000, -1.000000000000000000, 0.000000000000000000 ) ) ;
#48434 = CARTESIAN_POINT ( 'NONE',  ( -55.70499999999998408, 2.607480562269073321, 8.024999999999991473 ) ) ;
#48435 =( LENGTH_UNIT ( ) NAMED_UNIT ( * ) SI_UNIT ( .MILLI., .METRE. ) );
#48436 = FILL_AREA_STYLE ('',( #41768 ) ) ;
#48437 = CARTESIAN_POINT ( 'NONE',  ( 5.696827471326748160, 152.9267479045095968, 5.780458086807691132 ) ) ;
#48438 = PRESENTATION_LAYER_ASSIGNMENT (  '', '', ( #29294 ) ) ;
#48439 = DIRECTION ( 'NONE',  ( 0.000000000000000000, 0.000000000000000000, 1.000000000000000000 ) ) ;
#48440 = STYLED_ITEM ( 'NONE', ( #44737 ), #34703 ) ;
#48441 = CARTESIAN_POINT ( 'NONE',  ( -103.6429263765337936, -5.598654528085801552, 7.705886871421367523 ) ) ;
#48442 = DIRECTION ( 'NONE',  ( -1.473213661637684089E-17, -1.473213661637684706E-17, 1.000000000000000000 ) ) ;
#48443 = PRESENTATION_LAYER_ASSIGNMENT (  '', '', ( #58539 ) ) ;
#48444 = CARTESIAN_POINT ( 'NONE',  ( -89.45707362346618652, -9.058813317711329915, 2.943386871421371787 ) ) ;
#48445 = DIRECTION ( 'NONE',  ( 0.000000000000000000, 0.000000000000000000, 1.000000000000000000 ) ) ;
#48446 = MECHANICAL_DESIGN_GEOMETRIC_PRESENTATION_REPRESENTATION (  '', ( #63009 ), #16995 ) ;
#48447 = FACE_OUTER_BOUND ( 'NONE', #20115, .T. ) ;
#48448 = CARTESIAN_POINT ( 'NONE',  ( -6.826472737025120807, 138.3929263765338078, -4.959722759717907437 ) ) ;
#48449 = CARTESIAN_POINT ( 'NONE',  ( 16.00000000000001776, 14.00000000000000000, -29.68999999999999417 ) ) ;
#48450 = ORIENTED_EDGE ( 'NONE', *, *, #41004, .T. ) ;
#48451 = AXIS2_PLACEMENT_3D ( 'NONE', #66740, #25208, #2287 ) ;
#48452 = CARTESIAN_POINT ( 'NONE',  ( -9.827790563157511022E-16, 113.5570736234661666, 8.025000000000000355 ) ) ;
#48453 = ADVANCED_FACE ( 'NONE', ( #54706, #54366, #5461, #44570 ), #54021, .F. ) ;
#48454 = CARTESIAN_POINT ( 'NONE',  ( 1.401671290772266598, -7.000000000000003553, 0.1093172352041265755 ) ) ;
#48455 = CARTESIAN_POINT ( 'NONE',  ( 74.99999999999998579, 19.99999999996227018, -6.081205180447406100 ) ) ;
#48456 = VERTEX_POINT ( 'NONE', #24426 ) ;
#48457 = ORIENTED_EDGE ( 'NONE', *, *, #45068, .F. ) ;
#48458 = CARTESIAN_POINT ( 'NONE',  ( -102.4429263765338050, -1.166476076187852838E-15, -9.524999999999991473 ) ) ;
#48459 = DIRECTION ( 'NONE',  ( -0.000000000000000000, 1.000000000000000000, -0.000000000000000000 ) ) ;
#48460 = CYLINDRICAL_SURFACE ( 'NONE', #28158, 1.000000000000000000 ) ;
#48461 = ORIENTED_EDGE ( 'NONE', *, *, #13711, .T. ) ;
#48462 = CARTESIAN_POINT ( 'NONE',  ( 8.102448949553181734, 127.5049999999999812, 5.886773742842750679 ) ) ;
#48463 = SURFACE_STYLE_FILL_AREA ( #60008 ) ;
#48464 = CARTESIAN_POINT ( 'NONE',  ( -18.25000000000000711, 33.74999999999999289, 3.750000000000000000 ) ) ;
#48465 = CARTESIAN_POINT ( 'NONE',  ( -96.59499999999998465, 2.607480562269073321, 8.024999999999991473 ) ) ;
#48466 = VERTEX_POINT ( 'NONE', #66673 ) ;
#48467 = CARTESIAN_POINT ( 'NONE',  ( 8.336895043469018773, 153.3467911821693690, 0.8633023660745396954 ) ) ;
#48468 = PRESENTATION_LAYER_ASSIGNMENT (  '', '', ( #55086 ) ) ;
#48469 = STYLED_ITEM ( 'NONE', ( #16580 ), #12139 ) ;
#48470 = CARTESIAN_POINT ( 'NONE',  ( 22.99999999999999645, 5.000000000000000000, 24.00402776293825013 ) ) ;
#48471 = ORIENTED_EDGE ( 'NONE', *, *, #27479, .T. ) ;
#48472 = DIRECTION ( 'NONE',  ( -1.596582957076307996E-15, -1.000000000000000000, -0.000000000000000000 ) ) ;
#48473 = CARTESIAN_POINT ( 'NONE',  ( 32.00000000000000000, 43.00000000000000000, -80.00402776293826435 ) ) ;
#48474 = COLOUR_RGB ( '', 0.66274510, 0.83137255, 0.94901961) ;
#48475 = DIRECTION ( 'NONE',  ( 0.000000000000000000, 0.000000000000000000, -1.000000000000000000 ) ) ;
#48476 = FILL_AREA_STYLE_COLOUR ( '', #45783 ) ;
#48477 = EDGE_CURVE ( 'NONE', #47180, #35681, #29696, .T. ) ;
#48478 = TOROIDAL_SURFACE ( 'NONE', #36112, 0.5000000000000000000, 0.2500000000000000000 ) ;
#48479 = ORIENTED_EDGE ( 'NONE', *, *, #43895, .T. ) ;
#48480 = DIRECTION ( 'NONE',  ( -1.000000000000000000, -0.000000000000000000, -0.000000000000000000 ) ) ;
#48481 = DIRECTION ( 'NONE',  ( 0.000000000000000000, 0.000000000000000000, 1.000000000000000000 ) ) ;
#48482 = SURFACE_STYLE_FILL_AREA ( #17501 ) ;
#48483 = FILL_AREA_STYLE_COLOUR ( '', #60098 ) ;
#48484 = AXIS2_PLACEMENT_3D ( 'NONE', #38526, #21961, #16696 ) ;
#48485 = EDGE_CURVE ( 'NONE', #62454, #45809, #42361, .T. ) ;
#48486 = CIRCLE ( 'NONE', #13634, 7.000000000000001776 ) ;
#48487 = CARTESIAN_POINT ( 'NONE',  ( 66.74999999999998579, 36.75000000000000000, 3.750000000000000000 ) ) ;
#48488 = CARTESIAN_POINT ( 'NONE',  ( 3.250000000000003553, 4.698209414103854191E-16, 3.750000000000000000 ) ) ;
#48489 = DIRECTION ( 'NONE',  ( 0.000000000000000000, 0.000000000000000000, 1.000000000000000000 ) ) ;
#48490 = CARTESIAN_POINT ( 'NONE',  ( -1.085428990800084259, 154.1022378970840236, 9.078527738363963095 ) ) ;
#48491 = ORIENTED_EDGE ( 'NONE', *, *, #2994, .F. ) ;
#48492 = VECTOR ( 'NONE', #40280, 1000.000000000000000 ) ;
#48493 = ORIENTED_EDGE ( 'NONE', *, *, #58829, .T. ) ;
#48494 =( LENGTH_UNIT ( ) NAMED_UNIT ( * ) SI_UNIT ( .MILLI., .METRE. ) );
#48495 = PLANE ( 'NONE',  #43368 ) ;
#48496 = CYLINDRICAL_SURFACE ( 'NONE', #5303, 1.000000000000000888 ) ;
#48497 = FILL_AREA_STYLE_COLOUR ( '', #56805 ) ;
#48498 = ORIENTED_EDGE ( 'NONE', *, *, #30092, .T. ) ;
#48499 = CARTESIAN_POINT ( 'NONE',  ( 8.250000000000001776, 31.24999999999998579, 3.750000000000000000 ) ) ;
#48500 = CARTESIAN_POINT ( 'NONE',  ( -169.2549999999999955, -4.716976649647092401, 6.492361379858946790 ) ) ;
#48501 = DIRECTION ( 'NONE',  ( 0.000000000000000000, -0.7071067811865647812, -0.7071067811865302533 ) ) ;
#48502 = CARTESIAN_POINT ( 'NONE',  ( -147.8070736234661524, 10.01517768586948698, -1.839758294383808966E-15 ) ) ;
#48503 = CARTESIAN_POINT ( 'NONE',  ( -173.9949999999999761, -6.826472737025115478, 4.959722759717900331 ) ) ;
#48504 = EDGE_CURVE ( 'NONE', #52155, #13744, #45465, .T. ) ;
#48505 = CARTESIAN_POINT ( 'NONE',  ( -163.0449999999999875, 7.632228543268600340, 2.479861379858949277 ) ) ;
#48506 = VERTEX_POINT ( 'NONE', #13185 ) ;
#48507 = FILL_AREA_STYLE ('',( #27326 ) ) ;
#48508 = EDGE_CURVE ( 'NONE', #20383, #12708, #63463, .T. ) ;
#48509 = CARTESIAN_POINT ( 'NONE',  ( -14.67070496082497577, 10.91243640479189025, -4.991899053143842302 ) ) ;
#48510 = CARTESIAN_POINT ( 'NONE',  ( -79.55499999999999261, 0.000000000000000000, 8.024999999999991473 ) ) ;
#48511 = DIRECTION ( 'NONE',  ( 0.000000000000000000, 0.000000000000000000, 1.000000000000000000 ) ) ;
#48512 = SURFACE_SIDE_STYLE ('',( #64655 ) ) ;
#48513 = CARTESIAN_POINT ( 'NONE',  ( -75.01967246898638564, 35.97479162478882131, -9.552766844405001123 ) ) ;
#48514 = CARTESIAN_POINT ( 'NONE',  ( -77.09499999999997044, -2.607480562269071545, -8.024999999999991473 ) ) ;
#48515 = CARTESIAN_POINT ( 'NONE',  ( -3.094860106618434248, 141.9050000000000011, 9.525000000000000355 ) ) ;
#48516 = B_SPLINE_CURVE_WITH_KNOTS ( 'NONE', 3,
 ( #64002, #41909, #21437, #15849, #15506, #47904, #31647, #31287, #63322, #58062 ),
 .UNSPECIFIED., .F., .F.,
 ( 4, 2, 2, 2, 4 ),
 ( 0.000000000000000000, 0.0004658606356703480804, 0.0009317212713406961607, 0.001397581907011044133, 0.001863442542681392321 ),
 .UNSPECIFIED. ) ;
#48517 = FILL_AREA_STYLE ('',( #42906 ) ) ;
#48518 = CARTESIAN_POINT ( 'NONE',  ( 3.409623619629276625, -7.000000000000002665, 0.7804846576204699238 ) ) ;
#48519 = MECHANICAL_DESIGN_GEOMETRIC_PRESENTATION_REPRESENTATION (  '', ( #9184 ), #49600 ) ;
#48520 = SURFACE_SIDE_STYLE ('',( #52733 ) ) ;
#48521 = CARTESIAN_POINT ( 'NONE',  ( -2.754976799268632703, -2.005084411318700077, -7.000000000000003553 ) ) ;
#48522 =( NAMED_UNIT ( * ) PLANE_ANGLE_UNIT ( ) SI_UNIT ( $, .RADIAN. ) );
#48523 = ORIENTED_EDGE ( 'NONE', *, *, #43566, .T. ) ;
#48524 = AXIS2_PLACEMENT_3D ( 'NONE', #11171, #1606, #32616 ) ;
#48525 = DIRECTION ( 'NONE',  ( 0.000000000000000000, 0.000000000000000000, -1.000000000000000000 ) ) ;
#48526 = CARTESIAN_POINT ( 'NONE',  ( -50.24292637653379501, 5.598654528085804216, 7.705886871421366635 ) ) ;
#48527 = AXIS2_PLACEMENT_3D ( 'NONE', #68036, #52210, #31060 ) ;
#48528 = MECHANICAL_DESIGN_GEOMETRIC_PRESENTATION_REPRESENTATION (  '', ( #39531 ), #5790 ) ;
#48529 = PRESENTATION_STYLE_ASSIGNMENT (( #17208 ) ) ;
#48530 = DIRECTION ( 'NONE',  ( -1.000000000000000000, 0.000000000000000000, 0.000000000000000000 ) ) ;
#48531 = ORIENTED_EDGE ( 'NONE', *, *, #36356, .F. ) ;
#48532 = ORIENTED_EDGE ( 'NONE', *, *, #59955, .T. ) ;
#48533 = DIRECTION ( 'NONE',  ( 0.000000000000000000, -0.000000000000000000, 1.000000000000000000 ) ) ;
#48534 = CYLINDRICAL_SURFACE ( 'NONE', #23038, 18.00000000000000355 ) ;
#48535 = ADVANCED_FACE ( 'NONE', ( #46292 ), #62063, .T. ) ;
#48536 =( GEOMETRIC_REPRESENTATION_CONTEXT ( 3 ) GLOBAL_UNCERTAINTY_ASSIGNED_CONTEXT ( ( #11622 ) ) GLOBAL_UNIT_ASSIGNED_CONTEXT ( ( #21426, #68948, #36963 ) ) REPRESENTATION_CONTEXT ( 'NONE', 'WORKASPACE' ) );
#48537 =( NAMED_UNIT ( * ) PLANE_ANGLE_UNIT ( ) SI_UNIT ( $, .RADIAN. ) );
#48538 = CYLINDRICAL_SURFACE ( 'NONE', #33721, 0.5000000000000004441 ) ;
#48539 = EDGE_CURVE ( 'NONE', #41467, #7942, #57777, .T. ) ;
#48540 =( NAMED_UNIT ( * ) SI_UNIT ( $, .STERADIAN. ) SOLID_ANGLE_UNIT ( ) );
#48541 = ADVANCED_FACE ( 'NONE', ( #56816 ), #30785, .F. ) ;
#48542 = DIRECTION ( 'NONE',  ( -0.000000000000000000, -1.000000000000000000, -0.000000000000000000 ) ) ;
#48543 = ORIENTED_EDGE ( 'NONE', *, *, #28729, .T. ) ;
#48544 = CARTESIAN_POINT ( 'NONE',  ( -109.4049999999999727, -2.607480562269069768, 8.024999999999991473 ) ) ;
#48545 = VERTEX_POINT ( 'NONE', #67712 ) ;
#48546 = CARTESIAN_POINT ( 'NONE',  ( -137.1570736234661751, -9.058813317711329915, -2.943386871421370898 ) ) ;
#48547 = CARTESIAN_POINT ( 'NONE',  ( 7.632228543268607446, 129.1570736234661467, 2.479861379858954606 ) ) ;
#48548 = ORIENTED_EDGE ( 'NONE', *, *, #39110, .T. ) ;
#48549 = PRESENTATION_STYLE_ASSIGNMENT (( #54793 ) ) ;
#48550 = DIRECTION ( 'NONE',  ( 1.000000000000000000, 0.000000000000000000, 0.000000000000000000 ) ) ;
#48551 = EDGE_LOOP ( 'NONE', ( #11328, #26669, #32205, #55223 ) ) ;
#48552 = CIRCLE ( 'NONE', #18177, 14.00000000000000533 ) ;
#48553 = DIRECTION ( 'NONE',  ( 0.000000000000000000, -0.000000000000000000, 1.000000000000000000 ) ) ;
#48554 = CARTESIAN_POINT ( 'NONE',  ( 3.094860106618435136, 160.2949999999999875, -9.525000000000000355 ) ) ;
#48555 = ORIENTED_EDGE ( 'NONE', *, *, #64162, .T. ) ;
#48556 = COLOUR_RGB ( '', 0.72549020, 0.75294118, 0.79215686) ;
#48557 = DIRECTION ( 'NONE',  ( -0.6363636363636377968, -0.000000000000000000, -0.7713892158398687471 ) ) ;
#48558 = CARTESIAN_POINT ( 'NONE',  ( -74.99999999999998579, 50.00000000000000000, 11.50000000000000000 ) ) ;
#48559 = CARTESIAN_POINT ( 'NONE',  ( -136.2570736234661695, 5.598654528085800663, -7.705886871421367523 ) ) ;
#48560 = CARTESIAN_POINT ( 'NONE',  ( -13.25000000000000355, 28.24999999999998934, -4.000000000000000000 ) ) ;
#48561 = ORIENTED_EDGE ( 'NONE', *, *, #21284, .T. ) ;
#48562 = CARTESIAN_POINT ( 'NONE',  ( 6.826472737025119919, 121.8929263765338220, 4.959722759717908325 ) ) ;
#48563 = CARTESIAN_POINT ( 'NONE',  ( -47.90707362346616094, -3.094860106618429807, 9.524999999999991473 ) ) ;
#48564 = VECTOR ( 'NONE', #48389, 1000.000000000000000 ) ;
#48565 = EDGE_CURVE ( 'NONE', #17133, #68588, #25174, .T. ) ;
#48566 = CARTESIAN_POINT ( 'NONE',  ( -65.00000000000000000, -1.962809905030629631E-14, -12.00000000000000000 ) ) ;
#48567 = ADVANCED_FACE ( 'NONE', ( #56450 ), #42108, .F. ) ;
#48568 = ORIENTED_EDGE ( 'NONE', *, *, #48578, .F. ) ;
#48569 = DIRECTION ( 'NONE',  ( 0.000000000000000000, 0.000000000000000000, -1.000000000000000000 ) ) ;
#48570 = VERTEX_POINT ( 'NONE', #19507 ) ;
#48571 = CARTESIAN_POINT ( 'NONE',  ( -51.74292637653380211, -5.598654528085803328, -7.705886871421366635 ) ) ;
#48572 = SURFACE_STYLE_FILL_AREA ( #33051 ) ;
#48573 = CARTESIAN_POINT ( 'NONE',  ( -117.0570736234661808, 0.000000000000000000, 9.524999999999991473 ) ) ;
#48575 = CARTESIAN_POINT ( 'NONE',  ( -142.7049999999999557, 2.607480562269073321, 8.024999999999991473 ) ) ;
#48574 =( GEOMETRIC_REPRESENTATION_CONTEXT ( 3 ) GLOBAL_UNCERTAINTY_ASSIGNED_CONTEXT ( ( #48174 ) ) GLOBAL_UNIT_ASSIGNED_CONTEXT ( ( #55580, #39788, #29167 ) ) REPRESENTATION_CONTEXT ( 'NONE', 'WORKASPACE' ) );
#48576 =( LENGTH_UNIT ( ) NAMED_UNIT ( * ) SI_UNIT ( .MILLI., .METRE. ) );
#48577 = CARTESIAN_POINT ( 'NONE',  ( -74.99999999999998579, 50.00000000000000000, -10.00000000000000000 ) ) ;
#48578 = EDGE_CURVE ( 'NONE', #28375, #15308, #20713, .T. ) ;
#48579 = CARTESIAN_POINT ( 'NONE',  ( -6.826472737025120807, 116.1070736234661496, 4.959722759717906548 ) ) ;
#48580 = SURFACE_SIDE_STYLE ('',( #43645 ) ) ;
#48581 =( NAMED_UNIT ( * ) SI_UNIT ( $, .STERADIAN. ) SOLID_ANGLE_UNIT ( ) );
#48582 = ORIENTED_EDGE ( 'NONE', *, *, #28707, .F. ) ;
#48583 = AXIS2_PLACEMENT_3D ( 'NONE', #13275, #40068, #62161 ) ;
#48585 = ADVANCED_FACE ( 'NONE', ( #4719 ), #68402, .F. ) ;
#48584 = ORIENTED_EDGE ( 'NONE', *, *, #36180, .T. ) ;
#48586 = DIRECTION ( 'NONE',  ( 1.000000000000000000, -0.000000000000000000, -0.000000000000000000 ) ) ;
#48587 = DIRECTION ( 'NONE',  ( 1.000000000000000000, 0.000000000000000000, 0.000000000000000000 ) ) ;
#48588 = CARTESIAN_POINT ( 'NONE',  ( -55.70499999999998408, 2.607480562269073321, 8.024999999999991473 ) ) ;
#48589 = VERTEX_POINT ( 'NONE', #69440 ) ;
#48590 = CARTESIAN_POINT ( 'NONE',  ( 12.72792206135785875, 1.797044900979284448E-15, 10.00000000000000000 ) ) ;
#48591 = FILL_AREA_STYLE_COLOUR ( '', #31786 ) ;
#48592 =( GEOMETRIC_REPRESENTATION_CONTEXT ( 3 ) GLOBAL_UNCERTAINTY_ASSIGNED_CONTEXT ( ( #4016 ) ) GLOBAL_UNIT_ASSIGNED_CONTEXT ( ( #42839, #57226, #53009 ) ) REPRESENTATION_CONTEXT ( 'NONE', 'WORKASPACE' ) );
#48593 = DIRECTION ( 'NONE',  ( -0.000000000000000000, -1.000000000000000000, -0.000000000000000000 ) ) ;
#48594 = EDGE_CURVE ( 'NONE', #16969, #24888, #22971, .T. ) ;
#48595 = COLOUR_RGB ( '', 0.08235294, 0.09019608, 0.10196078) ;
#48596 = CARTESIAN_POINT ( 'NONE',  ( -45.00000000000000000, -1.469576158976824302E-14, 6.999999999999999112 ) ) ;
#48597 = DIRECTION ( 'NONE',  ( 0.000000000000000000, 0.000000000000000000, 1.000000000000000000 ) ) ;
#48598 = EDGE_LOOP ( 'NONE', ( #64000, #8180, #20207, #42571 ) ) ;
#48599 = STYLED_ITEM ( 'NONE', ( #9263 ), #54849 ) ;
#48600 = DIRECTION ( 'NONE',  ( 1.000000000000000000, 0.000000000000000000, 0.000000000000000000 ) ) ;
#48601 = EDGE_CURVE ( 'NONE', #43339, #22316, #63985, .T. ) ;
#48602 = CARTESIAN_POINT ( 'NONE',  ( -34.99999999999992895, 112.4999999999999858, 9.500000000000000000 ) ) ;
#48603 = CARTESIAN_POINT ( 'NONE',  ( -94.55707362346616662, -1.166476076187852838E-15, -9.524999999999991473 ) ) ;
#48604 = CARTESIAN_POINT ( 'NONE',  ( 62.24999999999998579, 33.74999999999999289, -4.000000000000000000 ) ) ;
#48605 = CYLINDRICAL_SURFACE ( 'NONE', #37110, 2.500000000000002220 ) ;
#48606 = PRESENTATION_LAYER_ASSIGNMENT (  '', '', ( #30555 ) ) ;
#48607 = CARTESIAN_POINT ( 'NONE',  ( -112.3449999999999847, 7.632228543268599452, -2.479861379858951942 ) ) ;
#48608 = CARTESIAN_POINT ( 'NONE',  ( 3.094860106618431583, 112.2049999999999841, 9.525000000000000355 ) ) ;
#48609 = CARTESIAN_POINT ( 'NONE',  ( -83.39499999999998181, -6.826472737025115478, -4.959722759717899443 ) ) ;
#48610 = VECTOR ( 'NONE', #61164, 1000.000000000000000 ) ;
#48611 =( NAMED_UNIT ( * ) PLANE_ANGLE_UNIT ( ) SI_UNIT ( $, .RADIAN. ) );
#48612 = CARTESIAN_POINT ( 'NONE',  ( -23.21231517720797655, 117.9999999999999716, 9.500000000000000000 ) ) ;
#48613 =( BOUNDED_CURVE ( )  B_SPLINE_CURVE ( 2, ( #2369, #23888, #45399, #62213, #66819, #18630, #61854, #40108, #35141, #8060, #56596 ),
 .UNSPECIFIED., .F., .F. ) 
 B_SPLINE_CURVE_WITH_KNOTS ( ( 3, 2, 2, 2, 2, 3 ),
 ( 0.1521739130434746068, 0.1543478260869527996, 0.1565217391304310479, 0.1586956521739092407, 0.1608695652173874613, 0.1630434782608656819 ),
 .UNSPECIFIED. ) 
 CURVE ( )  GEOMETRIC_REPRESENTATION_ITEM ( )  RATIONAL_B_SPLINE_CURVE ( ( 1.000000000000082379, 0.9510565162950710416, 1.000000000000000000, 0.9510565162951535312, 1.000000000000000000, 0.9510565162951535312, 1.000000000000000000, 0.9510565162951535312, 1.000000000000000000, 0.9510565162952410168, 0.9999999999999125144 ) ) 
 REPRESENTATION_ITEM ( '' )  );
#48614 = CARTESIAN_POINT ( 'NONE',  ( -167.4570736234661865, -9.058813317711329915, 2.943386871421371787 ) ) ;
#48615 = DIRECTION ( 'NONE',  ( 1.000000000000000000, 0.000000000000000000, 0.000000000000000000 ) ) ;
#48616 = ORIENTED_EDGE ( 'NONE', *, *, #61722, .F. ) ;
#48617 = CARTESIAN_POINT ( 'NONE',  ( -128.2429263765338021, 5.598654528085804216, 7.705886871421366635 ) ) ;
#48618 = FILL_AREA_STYLE_COLOUR ( '', #65175 ) ;
#48619 = CARTESIAN_POINT ( 'NONE',  ( -152.2450000000000045, -4.716976649647093289, -6.492361379858945902 ) ) ;
#48620 =( NAMED_UNIT ( * ) SI_UNIT ( $, .STERADIAN. ) SOLID_ANGLE_UNIT ( ) );
#48621 = VECTOR ( 'NONE', #49321, 1000.000000000000000 ) ;
#48622 = CARTESIAN_POINT ( 'NONE',  ( -48.44499999999998607, 0.000000000000000000, 8.024999999999991473 ) ) ;
#48623 = CARTESIAN_POINT ( 'NONE',  ( 1.000000000000000000, 36.99999999999999289, -3.750000000000000000 ) ) ;
#48624 = ORIENTED_EDGE ( 'NONE', *, *, #56526, .F. ) ;
#48625 = ORIENTED_EDGE ( 'NONE', *, *, #65434, .F. ) ;
#48626 = CARTESIAN_POINT ( 'NONE',  ( 6.000000000000017764, 26.00000000000000355, 23.99999999999999645 ) ) ;
#48627 = DIRECTION ( 'NONE',  ( -0.000000000000000000, -0.000000000000000000, -1.000000000000000000 ) ) ;
#48628 = EDGE_CURVE ( 'NONE', #65704, #49292, #27063, .T. ) ;
#48629 = CARTESIAN_POINT ( 'NONE',  ( -45.00000000000000000, 8.841134989786979759, 6.848475133234977363 ) ) ;
#48630 = AXIS2_PLACEMENT_3D ( 'NONE', #55066, #32573, #64612 ) ;
#48631 =( NAMED_UNIT ( * ) PLANE_ANGLE_UNIT ( ) SI_UNIT ( $, .RADIAN. ) );
#48632 = ORIENTED_EDGE ( 'NONE', *, *, #66567, .F. ) ;
#48633 = CARTESIAN_POINT ( 'NONE',  ( -142.2549999999999955, -4.716976649647092401, 6.492361379858946790 ) ) ;
#48634 = VERTEX_POINT ( 'NONE', #9686 ) ;
#48635 = CARTESIAN_POINT ( 'NONE',  ( 60.00000000000000000, 1.797044900979284448E-15, 9.500000000000000000 ) ) ;
#48636 = DIRECTION ( 'NONE',  ( -0.000000000000000000, 1.000000000000000000, -0.000000000000000000 ) ) ;
#48637 = CIRCLE ( 'NONE', #68837, 5.000000000000000000 ) ;
#48638 = ORIENTED_EDGE ( 'NONE', *, *, #40871, .T. ) ;
#48639 = PRESENTATION_STYLE_ASSIGNMENT (( #32071 ) ) ;
#48640 = CARTESIAN_POINT ( 'NONE',  ( 3.999798566743339556, 49.09558629977726696, -2.000000000000000000 ) ) ;
#48641 = CARTESIAN_POINT ( 'NONE',  ( -3.094860106618434248, 134.7949999999999875, 9.525000000000000355 ) ) ;
#48642 = AXIS2_PLACEMENT_3D ( 'NONE', #52868, #42352, #15584 ) ;
#48643 = ORIENTED_EDGE ( 'NONE', *, *, #67258, .F. ) ;
#48644 = EDGE_CURVE ( 'NONE', #63556, #19085, #30144, .T. ) ;
#48645 = FILL_AREA_STYLE ('',( #60191 ) ) ;
#48646 = CARTESIAN_POINT ( 'NONE',  ( 8.102448949553181734, 134.1049999999999329, -5.886773742842746238 ) ) ;
#48647 = CARTESIAN_POINT ( 'NONE',  ( -60.80499999999998550, -8.437984349512086979, 5.166775262442717831E-16 ) ) ;
#48648 = CARTESIAN_POINT ( 'NONE',  ( -119.3949999999999676, -6.826472737025115478, -4.959722759717899443 ) ) ;
#48649 = LINE ( 'NONE', #348, #16147 ) ;
#48650 = ORIENTED_EDGE ( 'NONE', *, *, #62836, .T. ) ;
#48651 = CARTESIAN_POINT ( 'NONE',  ( -3.094860106618432471, 152.7049999999999841, -9.525000000000000355 ) ) ;
#48652 = ADVANCED_FACE ( 'NONE', ( #42414 ), #63802, .F. ) ;
#48653 = CARTESIAN_POINT ( 'NONE',  ( -75.00000000000000000, -2.215169945516535778E-14, -7.000000000000000888 ) ) ;
#48654 = ADVANCED_FACE ( 'NONE', ( #35706 ), #33199, .T. ) ;
#48655 = VECTOR ( 'NONE', #22865, 1000.000000000000000 ) ;
#48656 = SURFACE_STYLE_FILL_AREA ( #65830 ) ;
#48657 = CARTESIAN_POINT ( 'NONE',  ( 7.750000000000001776, 31.24999999999998579, -3.750000000000000000 ) ) ;
#48658 = ADVANCED_FACE ( 'NONE', ( #37831 ), #54432, .T. ) ;
#48659 = AXIS2_PLACEMENT_3D ( 'NONE', #31569, #41468, #52374 ) ;
#48660 = DIRECTION ( 'NONE',  ( -1.000000000000000000, 0.000000000000000000, 0.000000000000000000 ) ) ;
#48661 = ORIENTED_EDGE ( 'NONE', *, *, #13865, .F. ) ;
#48662 = CARTESIAN_POINT ( 'NONE',  ( -32.76090297675384022, -9.103123100735301065, -2.346905346906288603 ) ) ;
#48663 = FACE_OUTER_BOUND ( 'NONE', #39473, .T. ) ;
#48664 = CARTESIAN_POINT ( 'NONE',  ( -171.0549999999999784, -9.827790563157499189E-16, -8.024999999999991473 ) ) ;
#48665 = ORIENTED_EDGE ( 'NONE', *, *, #14976, .F. ) ;
#48666 = CARTESIAN_POINT ( 'NONE',  ( 10.00000000000000355, 43.00000000000000000, -74.38749456993816978 ) ) ;
#48667 = STYLED_ITEM ( 'NONE', ( #1772 ), #25963 ) ;
#48668 = CARTESIAN_POINT ( 'NONE',  ( 0.000000000000000000, 114.9999999999999574, 0.000000000000000000 ) ) ;
#48669 = SURFACE_STYLE_FILL_AREA ( #64798 ) ;
#48670 = CARTESIAN_POINT ( 'NONE',  ( 0.000000000000000000, -2.500000000000000000, 0.000000000000000000 ) ) ;
#48671 = VERTEX_POINT ( 'NONE', #21592 ) ;
#48672 = EDGE_CURVE ( 'NONE', #50329, #11349, #49999, .T. ) ;
#48673 = CARTESIAN_POINT ( 'NONE',  ( -45.91547274654412547, 9.430195758660492089, -3.559962078525838347 ) ) ;
#48674 =( NAMED_UNIT ( * ) SI_UNIT ( $, .STERADIAN. ) SOLID_ANGLE_UNIT ( ) );
#48675 = CARTESIAN_POINT ( 'NONE',  ( -81.20499999999999829, -2.607480562269071545, -8.024999999999991473 ) ) ;
#48676 = ORIENTED_EDGE ( 'NONE', *, *, #18330, .F. ) ;
#48677 = CARTESIAN_POINT ( 'NONE',  ( 45.50000000000000000, 1.797044900979284448E-15, -10.00000000000000000 ) ) ;
#48678 = CARTESIAN_POINT ( 'NONE',  ( -4.716976649647098618, 112.1429263765338220, 6.492361379858953008 ) ) ;
#48679 = CARTESIAN_POINT ( 'NONE',  ( 6.826472737025121695, 144.6070736234661354, -4.959722759717905660 ) ) ;
#48680 = DIRECTION ( 'NONE',  ( 1.000000000000000000, 0.000000000000000000, 0.000000000000000000 ) ) ;
#48681 = CARTESIAN_POINT ( 'NONE',  ( -67.10707362346616378, 8.102448949553171076, -5.886773742842744461 ) ) ;
#48682 = FILL_AREA_STYLE_COLOUR ( '', #19039 ) ;
#48683 = ORIENTED_EDGE ( 'NONE', *, *, #26464, .F. ) ;
#48684 = DIRECTION ( 'NONE',  ( 0.000000000000000000, 0.000000000000000000, -1.000000000000000000 ) ) ;
#48685 = CARTESIAN_POINT ( 'NONE',  ( -101.3050000000000068, 8.437984349512085203, -1.550032578732815448E-15 ) ) ;
#48686 = EDGE_CURVE ( 'NONE', #62878, #18810, #60062, .T. ) ;
#48687 = CARTESIAN_POINT ( 'NONE',  ( -3.094860106618432471, 130.5949999999999989, -9.525000000000000355 ) ) ;
#48688 = STYLED_ITEM ( 'NONE', ( #66409 ), #22970 ) ;
#48689 = CARTESIAN_POINT ( 'NONE',  ( -120.7449999999999903, 4.716976649647094177, 6.492361379858945902 ) ) ;
#48690 = AXIS2_PLACEMENT_3D ( 'NONE', #33388, #1669, #5593 ) ;
#48691 = DIRECTION ( 'NONE',  ( 0.000000000000000000, 0.000000000000000000, 1.000000000000000000 ) ) ;
#48692 = EDGE_CURVE ( 'NONE', #62763, #69376, #23026, .T. ) ;
#48693 = VECTOR ( 'NONE', #20406, 1000.000000000000000 ) ;
#48695 = CARTESIAN_POINT ( 'NONE',  ( -153.8070736234661808, 10.01517768586948698, -1.839758294383808966E-15 ) ) ;
#48694 = CARTESIAN_POINT ( 'NONE',  ( -34.31243252642629926, -10.02680648607947589, -3.499999999999429789 ) ) ;
#48696 = CARTESIAN_POINT ( 'NONE',  ( -166.6429263765338078, -5.598654528085801552, 7.705886871421367523 ) ) ;
#48697 =( LENGTH_UNIT ( ) NAMED_UNIT ( * ) SI_UNIT ( .MILLI., .METRE. ) );
#48698 = CARTESIAN_POINT ( 'NONE',  ( -176.2449999999999761, -4.716976649647093289, -6.492361379858945902 ) ) ;
#48699 = AXIS2_PLACEMENT_3D ( 'NONE', #11311, #32081, #21883 ) ;
#48700 = CARTESIAN_POINT ( 'NONE',  ( 0.000000000000000000, 109.9999999999999858, 0.000000000000000000 ) ) ;
#48701 = STYLED_ITEM ( 'NONE', ( #20244 ), #19473 ) ;
#48702 = CARTESIAN_POINT ( 'NONE',  ( -42.64069574594451950, -13.97002997391379608, 2.674443234125082558 ) ) ;
#48703 = EDGE_LOOP ( 'NONE', ( #32769, #55359, #46234 ) ) ;
#48704 = CARTESIAN_POINT ( 'NONE',  ( -71.49999999999998579, 64.07124727947029896, -7.500000000000000000 ) ) ;
#48705 = DIRECTION ( 'NONE',  ( 1.000000000000000000, 0.000000000000000000, 0.000000000000000000 ) ) ;
#48706 = ORIENTED_EDGE ( 'NONE', *, *, #20186, .T. ) ;
#48707 = CARTESIAN_POINT ( 'NONE',  ( -71.69292637653380496, 10.01517768586948698, -1.839758294383808571E-15 ) ) ;
#48708 = ITEM_DEFINED_TRANSFORMATION ( 'NONE', 'NONE', #37207,  #42840 ) ;
#48709 = DIRECTION ( 'NONE',  ( 0.000000000000000000, 1.000000000000000000, 0.000000000000000000 ) ) ;
#48710 =( BOUNDED_CURVE ( )  B_SPLINE_CURVE ( 2, ( #50848, #50503, #12856, #7581, #67365, #19162, #51533, #29736, #29369, #34322, #40306 ),
 .UNSPECIFIED., .F., .F. ) 
 B_SPLINE_CURVE_WITH_KNOTS ( ( 3, 2, 2, 2, 2, 3 ),
 ( 0.6521739130434628384, 0.6543478260869410867, 0.6565217391304192240, 0.6586956521738974724, 0.6608695652173756097, 0.6630434782608538580 ),
 .UNSPECIFIED. ) 
 CURVE ( )  GEOMETRIC_REPRESENTATION_ITEM ( )  RATIONAL_B_SPLINE_CURVE ( ( 1.000000000000347500, 0.9510565162948061424, 1.000000000000000000, 0.9510565162951535312, 1.000000000000000000, 0.9510565162951535312, 1.000000000000000000, 0.9510565162951535312, 1.000000000000000000, 0.9510565162955059160, 0.9999999999996476152 ) ) 
 REPRESENTATION_ITEM ( '' )  );
#48711 = CARTESIAN_POINT ( 'NONE',  ( -184.0000000000000000, 0.000000000000000000, 8.524999999999984368 ) ) ;
#48712 = CARTESIAN_POINT ( 'NONE',  ( -154.5570736234661808, -1.166476076187852838E-15, -9.524999999999991473 ) ) ;
#48713 = DIRECTION ( 'NONE',  ( 0.000000000000000000, 0.000000000000000000, 1.000000000000000000 ) ) ;
#48714 = CARTESIAN_POINT ( 'NONE',  ( -6.887213563469348543, -6.070996185493598318, 0.1702817813269538461 ) ) ;
#48715 = ORIENTED_EDGE ( 'NONE', *, *, #25876, .T. ) ;
#48716 = CARTESIAN_POINT ( 'NONE',  ( -179.4550000000000125, 7.632228543268599452, -2.479861379858951942 ) ) ;
#48717 = ORIENTED_EDGE ( 'NONE', *, *, #9222, .T. ) ;
#48718 = DIRECTION ( 'NONE',  ( -0.000000000000000000, -1.000000000000000000, 0.000000000000000000 ) ) ;
#48720 = EDGE_CURVE ( 'NONE', #65093, #7834, #1615, .T. ) ;
#48719 = DIRECTION ( 'NONE',  ( 0.000000000000000000, 1.000000000000000000, 0.000000000000000000 ) ) ;
#48721 = DIRECTION ( 'NONE',  ( 0.000000000000000000, 0.000000000000000000, -1.000000000000000000 ) ) ;
#48722 = DIRECTION ( 'NONE',  ( -1.000000000000000000, 0.000000000000000000, 0.000000000000000000 ) ) ;
#48723 = AXIS2_PLACEMENT_3D ( 'NONE', #16170, #28383, #6590 ) ;
#48724 = AXIS2_PLACEMENT_3D ( 'NONE', #68763, #59202, #43103 ) ;
#48725 = CARTESIAN_POINT ( 'NONE',  ( 7.632228543268608334, 138.4570736234661581, -2.479861379858951942 ) ) ;
#48726 = CIRCLE ( 'NONE', #47643, 5.000000000000000000 ) ;
#48727 = ORIENTED_EDGE ( 'NONE', *, *, #28513, .T. ) ;
#48728 = EDGE_CURVE ( 'NONE', #47709, #7106, #59912, .T. ) ;
#48729 = CARTESIAN_POINT ( 'NONE',  ( -180.4429263765338192, -1.166476076187852838E-15, -9.524999999999991473 ) ) ;
#48730 = CARTESIAN_POINT ( 'NONE',  ( -90.05499999999997840, -9.827790563157499189E-16, -8.024999999999991473 ) ) ;
#48731 = ORIENTED_EDGE ( 'NONE', *, *, #37783, .F. ) ;
#48732 = ADVANCED_FACE ( 'NONE', ( #11731 ), #1098, .T. ) ;
#48733 =( NAMED_UNIT ( * ) SI_UNIT ( $, .STERADIAN. ) SOLID_ANGLE_UNIT ( ) );
#48734 = VECTOR ( 'NONE', #36772, 1000.000000000000000 ) ;
#48735 = CARTESIAN_POINT ( 'NONE',  ( 22.00000000000000711, 50.00000000000000000, -54.99999999999998579 ) ) ;
#48736 = CARTESIAN_POINT ( 'NONE',  ( -9.000000000000003553, 27.99999999999998934, 4.000000000000000000 ) ) ;
#48737 = PRESENTATION_STYLE_ASSIGNMENT (( #32167 ) ) ;
#48738 = ORIENTED_EDGE ( 'NONE', *, *, #12220, .F. ) ;
#48739 = PRESENTATION_STYLE_ASSIGNMENT (( #27201 ) ) ;
#48740 = CARTESIAN_POINT ( 'NONE',  ( -67.04499999999997328, 7.632228543268600340, 2.479861379858949277 ) ) ;
#48741 = ORIENTED_EDGE ( 'NONE', *, *, #55976, .F. ) ;
#48742 = STYLED_ITEM ( 'NONE', ( #27984 ), #55765 ) ;
#48743 = CARTESIAN_POINT ( 'NONE',  ( -48.44292637653380496, -1.166476076187852838E-15, -9.524999999999991473 ) ) ;
#48744 = CARTESIAN_POINT ( 'NONE',  ( -45.00000000000000000, 9.371995676438096723, -6.584629826274035480 ) ) ;
#48745 = AXIS2_PLACEMENT_3D ( 'NONE', #64324, #27357, #16858 ) ;
#48746 = VERTEX_POINT ( 'NONE', #37487 ) ;
#48747 = SURFACE_STYLE_FILL_AREA ( #54657 ) ;
#48748 = LINE ( 'NONE', #12788, #69239 ) ;
#48749 = ORIENTED_EDGE ( 'NONE', *, *, #18590, .T. ) ;
#48750 = ADVANCED_FACE ( 'NONE', ( #21956 ), #24113, .F. ) ;
#48751 = VECTOR ( 'NONE', #44301, 1000.000000000000000 ) ;
#48752 = CARTESIAN_POINT ( 'NONE',  ( -23.71231517720798010, 113.4999999999999858, 10.00000000000000000 ) ) ;
#48753 = DIRECTION ( 'NONE',  ( -0.000000000000000000, 0.000000000000000000, -1.000000000000000000 ) ) ;
#48754 = CARTESIAN_POINT ( 'NONE',  ( -112.7049999999999699, 2.607480562269073321, 8.024999999999991473 ) ) ;
#48755 = VERTEX_POINT ( 'NONE', #42755 ) ;
#48756 = CARTESIAN_POINT ( 'NONE',  ( 3.409440450231731923, 1.719598803866702719, -7.000000000000003553 ) ) ;
#48757 = CARTESIAN_POINT ( 'NONE',  ( 8.000000000000035527, 5.000000000000000000, 77.00402776293825013 ) ) ;
#48758 = FACE_OUTER_BOUND ( 'NONE', #25642, .T. ) ;
#48759 = CARTESIAN_POINT ( 'NONE',  ( -164.1570736234661751, -9.058813317711329915, -2.943386871421370898 ) ) ;
#48760 = CARTESIAN_POINT ( 'NONE',  ( -3.094860106618434248, 131.7949999999999875, 9.525000000000000355 ) ) ;
#48761 = CARTESIAN_POINT ( 'NONE',  ( -93.05707362346616662, 0.000000000000000000, 9.524999999999991473 ) ) ;
#48762 = AXIS2_PLACEMENT_3D ( 'NONE', #33405, #33733, #13314 ) ;
#48763 = PRESENTATION_LAYER_ASSIGNMENT (  '', '', ( #28446 ) ) ;
#48764 = DIRECTION ( 'NONE',  ( -0.000000000000000000, 1.000000000000000000, -0.000000000000000000 ) ) ;
#48765 = ORIENTED_EDGE ( 'NONE', *, *, #52845, .T. ) ;
#48766 = FACE_OUTER_BOUND ( 'NONE', #15353, .T. ) ;
#48768 =( NAMED_UNIT ( * ) PLANE_ANGLE_UNIT ( ) SI_UNIT ( $, .RADIAN. ) );
#48767 = DIRECTION ( 'NONE',  ( -1.000000000000000000, -0.000000000000000000, -0.000000000000000000 ) ) ;
#48769 = CARTESIAN_POINT ( 'NONE',  ( -47.50000000000000000, 13.41640786499872284, 10.00000000000000000 ) ) ;
#48770 = CARTESIAN_POINT ( 'NONE',  ( -139.7049999999999841, 2.607480562269073321, 8.024999999999991473 ) ) ;
#48771 = LINE ( 'NONE', #60311, #59010 ) ;
#48772 = CARTESIAN_POINT ( 'NONE',  ( -141.2949999999999875, -2.607480562269069768, 8.024999999999991473 ) ) ;
#48773 = VECTOR ( 'NONE', #1271, 1000.000000000000000 ) ;
#48774 = CARTESIAN_POINT ( 'NONE',  ( -133.9449999999999932, -9.827790563157499189E-16, -8.024999999999991473 ) ) ;
#48775 = VERTEX_POINT ( 'NONE', #22992 ) ;
#48776 = CARTESIAN_POINT ( 'NONE',  ( 72.00000000000000000, 35.92875272052971525, -9.500000000000000000 ) ) ;
#48777 = AXIS2_PLACEMENT_3D ( 'NONE', #61251, #46148, #34858 ) ;
#48778 = PRESENTATION_STYLE_ASSIGNMENT (( #21291 ) ) ;
#48779 = UNCERTAINTY_MEASURE_WITH_UNIT (LENGTH_MEASURE( 1.000000000000000082E-05 ), #26672, 'distance_accuracy_value', 'NONE');
#48780 = CARTESIAN_POINT ( 'NONE',  ( -54.20499999999997698, -2.607480562269071545, -8.024999999999991473 ) ) ;
#48781 = CARTESIAN_POINT ( 'NONE',  ( -60.44499999999998607, 0.000000000000000000, 8.024999999999991473 ) ) ;
#48782 = SURFACE_SIDE_STYLE ('',( #5447 ) ) ;
#48783 = FILL_AREA_STYLE_COLOUR ( '', #60146 ) ;
#48784 = AXIS2_PLACEMENT_3D ( 'NONE', #33641, #33987, #49839 ) ;
#48785 = CARTESIAN_POINT ( 'NONE',  ( -55.65942242047054123, -8.713741708682274378, -1.106834464302784982 ) ) ;
#48786 = CARTESIAN_POINT ( 'NONE',  ( -106.6429263765338078, -5.598654528085801552, 7.705886871421367523 ) ) ;
#48787 = DIRECTION ( 'NONE',  ( -3.106759027390241145E-16, 0.0004343061746624778119, 0.9999999056890690463 ) ) ;
#48788 = CONICAL_SURFACE ( 'NONE', #61133, 7.000000000000000888, 0.7853981633974500554 ) ;
#48789 = FILL_AREA_STYLE_COLOUR ( '', #28137 ) ;
#48790 = CARTESIAN_POINT ( 'NONE',  ( 39.24999999999999289, 15.74999999999997513, 3.750000000000000000 ) ) ;
#48791 = SURFACE_STYLE_FILL_AREA ( #5816 ) ;
#48792 = AXIS2_PLACEMENT_3D ( 'NONE', #31277, #25660, #36271 ) ;
#48793 = B_SPLINE_CURVE_WITH_KNOTS ( 'NONE', 3,
 ( #19389, #29949, #51414, #24321, #62995, #46167, #67236, #67591, #56324, #61948 ),
 .UNSPECIFIED., .F., .F.,
 ( 4, 2, 2, 2, 4 ),
 ( 0.006344968262825391968, 0.006871805238692929065, 0.007398642214560467029, 0.007925479190428004125, 0.008452316166295541222 ),
 .UNSPECIFIED. ) ;
#48794 = AXIS2_PLACEMENT_3D ( 'NONE', #27863, #63874, #28208 ) ;
#48795 = CYLINDRICAL_SURFACE ( 'NONE', #18126, 1.000000000000000888 ) ;
#48796 = ORIENTED_EDGE ( 'NONE', *, *, #27401, .T. ) ;
#48797 = CARTESIAN_POINT ( 'NONE',  ( 0.000000000000000000, 137.9429263765338192, -8.025000000000000355 ) ) ;
#48798 = EDGE_CURVE ( 'NONE', #27464, #37986, #48868, .T. ) ;
#48799 = FILL_AREA_STYLE ('',( #27261 ) ) ;
#48800 = EDGE_LOOP ( 'NONE', ( #46345, #19770, #31121, #66489 ) ) ;
#48801 = TOROIDAL_SURFACE ( 'NONE', #54324, 22.50000000000000000, 0.5000000000000000000 ) ;
#48802 = CARTESIAN_POINT ( 'NONE',  ( -7.632228543268607446, 112.6570736234661609, -2.479861379858953718 ) ) ;
#48803 =( GEOMETRIC_REPRESENTATION_CONTEXT ( 3 ) GLOBAL_UNCERTAINTY_ASSIGNED_CONTEXT ( ( #52524 ) ) GLOBAL_UNIT_ASSIGNED_CONTEXT ( ( #29775, #51237, #52636 ) ) REPRESENTATION_CONTEXT ( 'NONE', 'WORKASPACE' ) );
#48804 = PRESENTATION_LAYER_ASSIGNMENT (  '', '', ( #30774 ) ) ;
#48805 = CARTESIAN_POINT ( 'NONE',  ( 20.71231517720797655, 149.4999999999999716, 10.00000000000000000 ) ) ;
#48806 = CARTESIAN_POINT ( 'NONE',  ( 4.716976649647099507, 138.7570736234661695, -6.492361379858953008 ) ) ;
#48807 = EDGE_CURVE ( 'NONE', #64274, #37913, #46471, .T. ) ;
#48808 = ORIENTED_EDGE ( 'NONE', *, *, #66235, .F. ) ;
#48809 = EDGE_LOOP ( 'NONE', ( #25374, #42099, #14189, #19310 ) ) ;
#48810 = DIRECTION ( 'NONE',  ( 0.000000000000000000, 0.000000000000000000, 1.000000000000000000 ) ) ;
#48811 = CARTESIAN_POINT ( 'NONE',  ( 17.75000000000000711, 31.24999999999999289, 3.750000000000000000 ) ) ;
#48812 = ADVANCED_FACE ( 'NONE', ( #62589 ), #3103, .T. ) ;
#48813 = FACE_OUTER_BOUND ( 'NONE', #23925, .T. ) ;
#48814 = ORIENTED_EDGE ( 'NONE', *, *, #59623, .T. ) ;
#48815 = CARTESIAN_POINT ( 'NONE',  ( -9.058813317711338797, 129.4549999999999841, 2.943386871421373563 ) ) ;
#48816 = CARTESIAN_POINT ( 'NONE',  ( -119.4570736234661723, -9.058813317711329915, 2.943386871421371787 ) ) ;
#48817 = ADVANCED_FACE ( 'NONE', ( #24597 ), #35178, .T. ) ;
#48818 = STYLED_ITEM ( 'NONE', ( #11104 ), #48453 ) ;
#48819 = MECHANICAL_DESIGN_GEOMETRIC_PRESENTATION_REPRESENTATION (  '', ( #44307 ), #55493 ) ;
#48820 = ADVANCED_FACE ( 'NONE', ( #1462, #55327 ), #36257, .F. ) ;
#48821 = CARTESIAN_POINT ( 'NONE',  ( -9.827790563157511022E-16, 133.4429263765338192, 8.025000000000000355 ) ) ;
#48822 = CARTESIAN_POINT ( 'NONE',  ( -94.49499999999999034, 6.826472737025113702, -4.959722759717902107 ) ) ;
#48823 = EDGE_LOOP ( 'NONE', ( #31189, #26607, #28924 ) ) ;
#48824 = CARTESIAN_POINT ( 'NONE',  ( 8.443840259832290585, 153.4094599605764984, 0.06244066176116176009 ) ) ;
#48825 = PLANE ( 'NONE',  #18737 ) ;
#48826 = EDGE_CURVE ( 'NONE', #49243, #31700, #56712, .T. ) ;
#48827 =( NAMED_UNIT ( * ) SI_UNIT ( $, .STERADIAN. ) SOLID_ANGLE_UNIT ( ) );
#48828 = ORIENTED_EDGE ( 'NONE', *, *, #5075, .T. ) ;
#48829 = CARTESIAN_POINT ( 'NONE',  ( 4.716976649647096842, 160.7429263765338021, 6.492361379858953896 ) ) ;
#48830 = FACE_OUTER_BOUND ( 'NONE', #3499, .T. ) ;
#48831 = CARTESIAN_POINT ( 'NONE',  ( 6.767634268437467959, -2.278113600022081631, 0.1324414877861178896 ) ) ;
#48832 = PRESENTATION_LAYER_ASSIGNMENT (  '', '', ( #9492 ) ) ;
#48833 = ORIENTED_EDGE ( 'NONE', *, *, #63046, .F. ) ;
#48834 = CARTESIAN_POINT ( 'NONE',  ( 4.750000000000000000, 5.817072295949927426E-16, 0.7500000000000000000 ) ) ;
#48835 = ORIENTED_EDGE ( 'NONE', *, *, #48109, .F. ) ;
#48836 = CARTESIAN_POINT ( 'NONE',  ( 30.75000000000001066, 15.99999999999997691, -3.750000000000000000 ) ) ;
#48837 = DIRECTION ( 'NONE',  ( 0.000000000000000000, 1.000000000000000000, 0.000000000000000000 ) ) ;
#48838 = CARTESIAN_POINT ( 'NONE',  ( 45.02564408151554431, 10.00854802717183389, 3.127379285698622446 ) ) ;
#48839 = LINE ( 'NONE', #62455, #49103 ) ;
#48840 =( GEOMETRIC_REPRESENTATION_CONTEXT ( 3 ) GLOBAL_UNCERTAINTY_ASSIGNED_CONTEXT ( ( #58134 ) ) GLOBAL_UNIT_ASSIGNED_CONTEXT ( ( #5623, #48611, #38405 ) ) REPRESENTATION_CONTEXT ( 'NONE', 'WORKASPACE' ) );
#48841 = LINE ( 'NONE', #11148, #58477 ) ;
#48842 = ORIENTED_EDGE ( 'NONE', *, *, #23649, .T. ) ;
#48843 = CARTESIAN_POINT ( 'NONE',  ( -161.9929263765337737, 8.102448949553172852, -5.886773742842744461 ) ) ;
#48844 = FILL_AREA_STYLE_COLOUR ( '', #47843 ) ;
#48845 = SURFACE_STYLE_FILL_AREA ( #33999 ) ;
#48846 = AXIS2_PLACEMENT_3D ( 'NONE', #2044, #62246, #35535 ) ;
#48847 =( NAMED_UNIT ( * ) PLANE_ANGLE_UNIT ( ) SI_UNIT ( $, .RADIAN. ) );
#48848 = ORIENTED_EDGE ( 'NONE', *, *, #44406, .F. ) ;
#48849 = CARTESIAN_POINT ( 'NONE',  ( 0.000000000000000000, -2.500000000000000000, 0.000000000000000000 ) ) ;
#48850 = CARTESIAN_POINT ( 'NONE',  ( -171.5049999999999386, -6.826472737025115478, -4.959722759717899443 ) ) ;
#48851 = CARTESIAN_POINT ( 'NONE',  ( 60.00000000000000000, 1.797044900979284448E-15, 10.00000000000000000 ) ) ;
#48852 = FACE_OUTER_BOUND ( 'NONE', #41501, .T. ) ;
#48853 = CARTESIAN_POINT ( 'NONE',  ( -171.7450000000000045, 4.716976649647094177, 6.492361379858945902 ) ) ;
#48854 = CARTESIAN_POINT ( 'NONE',  ( -169.0449999999999875, 7.632228543268600340, 2.479861379858949277 ) ) ;
#48855 = ORIENTED_EDGE ( 'NONE', *, *, #41110, .T. ) ;
#48856 = AXIS2_PLACEMENT_3D ( 'NONE', #57736, #63691, #46529 ) ;
#48857 =( GEOMETRIC_REPRESENTATION_CONTEXT ( 3 ) GLOBAL_UNCERTAINTY_ASSIGNED_CONTEXT ( ( #51053 ) ) GLOBAL_UNIT_ASSIGNED_CONTEXT ( ( #52365, #30508, #40413 ) ) REPRESENTATION_CONTEXT ( 'NONE', 'WORKASPACE' ) );
#48858 = CARTESIAN_POINT ( 'NONE',  ( 30.75000000000001066, 16.24999999999997513, -4.000000000000000000 ) ) ;
#48859 = DIRECTION ( 'NONE',  ( -0.000000000000000000, -0.000000000000000000, 1.000000000000000000 ) ) ;
#48860 = CARTESIAN_POINT ( 'NONE',  ( -80.75499999999999545, 4.716976649647091513, -6.492361379858946790 ) ) ;
#48861 = LINE ( 'NONE', #26306, #41011 ) ;
#48862 = DIRECTION ( 'NONE',  ( -0.000000000000000000, 1.000000000000000000, -0.000000000000000000 ) ) ;
#48863 = CYLINDRICAL_SURFACE ( 'NONE', #9049, 12.50000000000001066 ) ;
#48864 = CIRCLE ( 'NONE', #19585, 18.50000000000000355 ) ;
#48865 = CARTESIAN_POINT ( 'NONE',  ( -80.99499999999999034, -6.826472737025113702, 4.959722759717902107 ) ) ;
#48866 = CARTESIAN_POINT ( 'NONE',  ( 10.01517768586949231, 139.8050000000000068, 1.839758294383810543E-15 ) ) ;
#48867 = CARTESIAN_POINT ( 'NONE',  ( -133.5570736234661808, -1.166476076187852838E-15, -9.524999999999991473 ) ) ;
#48868 = CIRCLE ( 'NONE', #61173, 9.000000000000007105 ) ;
#48869 = AXIS2_PLACEMENT_3D ( 'NONE', #7925, #61709, #18821 ) ;
#48870 = DIRECTION ( 'NONE',  ( -0.7071067811865352493, 8.659560562354782482E-17, 0.7071067811865597852 ) ) ;
#48871 = UNCERTAINTY_MEASURE_WITH_UNIT (LENGTH_MEASURE( 1.000000000000000082E-05 ), #21677, 'distance_accuracy_value', 'NONE');
#48872 = SURFACE_STYLE_USAGE ( .BOTH. , #6948 ) ;
#48873 = SURFACE_STYLE_USAGE ( .BOTH. , #69586 ) ;
#48874 = ORIENTED_EDGE ( 'NONE', *, *, #21403, .F. ) ;
#48875 = FACE_OUTER_BOUND ( 'NONE', #36145, .T. ) ;
#48876 = DIRECTION ( 'NONE',  ( -0.7071067811865425767, 0.000000000000000000, -0.7071067811865525687 ) ) ;
#48877 = PRESENTATION_LAYER_ASSIGNMENT (  '', '', ( #15194 ) ) ;
#48878 = PRESENTATION_STYLE_ASSIGNMENT (( #9226 ) ) ;
#48879 = EDGE_CURVE ( 'NONE', #29587, #27240, #49952, .T. ) ;
#48880 = DIRECTION ( 'NONE',  ( 0.000000000000000000, 0.000000000000000000, 1.000000000000000000 ) ) ;
#48881 = FILL_AREA_STYLE ('',( #16516 ) ) ;
#48882 = ORIENTED_EDGE ( 'NONE', *, *, #13321, .T. ) ;
#48883 = ORIENTED_EDGE ( 'NONE', *, *, #54782, .T. ) ;
#48884 = AXIS2_PLACEMENT_3D ( 'NONE', #58522, #53269, #48026 ) ;
#48885 = CARTESIAN_POINT ( 'NONE',  ( 41.84210526315788314, 107.2928455055531600, 4.000000000000000000 ) ) ;
#48886 = VECTOR ( 'NONE', #8199, 1000.000000000000114 ) ;
#48887 = EDGE_CURVE ( 'NONE', #30297, #29473, #57681, .T. ) ;
#48888 = STYLED_ITEM ( 'NONE', ( #66737 ), #32089 ) ;
#48889 = DIRECTION ( 'NONE',  ( 1.000000000000000000, 0.000000000000000000, 0.000000000000000000 ) ) ;
#48890 = LINE ( 'NONE', #33016, #57696 ) ;
#48891 = CARTESIAN_POINT ( 'NONE',  ( 4.716976649647099507, 140.6429263765338078, -6.492361379858953008 ) ) ;
#48892 = ORIENTED_EDGE ( 'NONE', *, *, #15373, .F. ) ;
#48893 = CARTESIAN_POINT ( 'NONE',  ( -110.3049999999999926, 8.437984349512086979, -1.550032578732815448E-15 ) ) ;
#48894 = ORIENTED_EDGE ( 'NONE', *, *, #57754, .F. ) ;
#48895 = DIRECTION ( 'NONE',  ( -1.000000000000000000, -0.000000000000000000, -0.000000000000000000 ) ) ;
#48896 = CARTESIAN_POINT ( 'NONE',  ( -105.3570736234661780, 5.598654528085804216, 7.705886871421366635 ) ) ;
#48897 = ORIENTED_EDGE ( 'NONE', *, *, #41502, .F. ) ;
#48898 = CARTESIAN_POINT ( 'NONE',  ( -57.44292637653381206, -1.166476076187852838E-15, -9.524999999999991473 ) ) ;
#48899 = DIRECTION ( 'NONE',  ( -1.000000000000000000, 0.000000000000000000, 0.000000000000000000 ) ) ;
#48900 = ORIENTED_EDGE ( 'NONE', *, *, #17591, .T. ) ;
#48901 = ADVANCED_FACE ( 'NONE', ( #19334 ), #38772, .T. ) ;
#48902 = CARTESIAN_POINT ( 'NONE',  ( -9.058813317711338797, 158.3449999999999989, 2.943386871421373563 ) ) ;
#48903 = CARTESIAN_POINT ( 'NONE',  ( -72.00000000000000000, 14.49137674618942562, 9.500000000000000000 ) ) ;
#48904 = VERTEX_POINT ( 'NONE', #35540 ) ;
#48905 = VECTOR ( 'NONE', #32711, 1000.000000000000000 ) ;
#48906 = ORIENTED_EDGE ( 'NONE', *, *, #34335, .F. ) ;
#48907 = MECHANICAL_DESIGN_GEOMETRIC_PRESENTATION_REPRESENTATION (  '', ( #8456 ), #62319 ) ;
#48908 = CARTESIAN_POINT ( 'NONE',  ( 0.000000000000000000, 0.000000000000000000, 0.000000000000000000 ) ) ;
#48909 = DIRECTION ( 'NONE',  ( 0.000000000000000000, 0.000000000000000000, 1.000000000000000000 ) ) ;
#48910 = EDGE_CURVE ( 'NONE', #60780, #38982, #21074, .T. ) ;
#48911 = CARTESIAN_POINT ( 'NONE',  ( -129.8929263765338362, -8.102448949553174629, -5.886773742842741797 ) ) ;
#48912 = ORIENTED_EDGE ( 'NONE', *, *, #42698, .T. ) ;
#48913 = CARTESIAN_POINT ( 'NONE',  ( 7.632228543268607446, 137.0429263765338135, 2.479861379858954606 ) ) ;
#48914 = CARTESIAN_POINT ( 'NONE',  ( 13.50000000000000355, 27.99999999999998934, 3.750000000000000000 ) ) ;
#48915 = SPHERICAL_SURFACE ( 'NONE', #601, 7.499999999999992895 ) ;
#48916 = SURFACE_STYLE_USAGE ( .BOTH. , #27385 ) ;
#48917 = ORIENTED_EDGE ( 'NONE', *, *, #30893, .F. ) ;
#48918 = SURFACE_STYLE_FILL_AREA ( #50262 ) ;
#48919 = ORIENTED_EDGE ( 'NONE', *, *, #62081, .F. ) ;
#48920 = CARTESIAN_POINT ( 'NONE',  ( -52.34292637653378932, -9.058813317711329915, 2.943386871421371787 ) ) ;
#48921 = VECTOR ( 'NONE', #15733, 1000.000000000000000 ) ;
#48922 = CARTESIAN_POINT ( 'NONE',  ( -58.75000000000000000, -4.000000000000000000, 15.00000000000000178 ) ) ;
#48923 = DIRECTION ( 'NONE',  ( 1.596582957076308193E-15, 1.000000000000000000, -1.712231188808098028E-15 ) ) ;
#48924 = DIRECTION ( 'NONE',  ( -0.000000000000000000, 1.000000000000000000, -0.000000000000000000 ) ) ;
#48925 = AXIS2_PLACEMENT_3D ( 'NONE', #31534, #42845, #69519 ) ;
#48926 = CARTESIAN_POINT ( 'NONE',  ( -141.3550000000000182, -4.716976649647093289, -6.492361379858945902 ) ) ;
#48927 = CARTESIAN_POINT ( 'NONE',  ( -5.196152422706636465, -1.107695154586736175, -9.000000000000003553 ) ) ;
#48928 = DIRECTION ( 'NONE',  ( -1.000000000000000000, -1.224646799147353207E-16, -0.000000000000000000 ) ) ;
#48929 = UNCERTAINTY_MEASURE_WITH_UNIT (LENGTH_MEASURE( 1.000000000000000082E-05 ), #56602, 'distance_accuracy_value', 'NONE');
#48930 =( NAMED_UNIT ( * ) PLANE_ANGLE_UNIT ( ) SI_UNIT ( $, .RADIAN. ) );
#48931 = ORIENTED_EDGE ( 'NONE', *, *, #16095, .F. ) ;
#48932 = ORIENTED_EDGE ( 'NONE', *, *, #32613, .T. ) ;
#48933 = LINE ( 'NONE', #64722, #68760 ) ;
#48934 = CYLINDRICAL_SURFACE ( 'NONE', #69357, 10.00000000000000178 ) ;
#48935 = CARTESIAN_POINT ( 'NONE',  ( -58.70499999999997698, 2.607480562269073321, 8.024999999999991473 ) ) ;
#48937 = ORIENTED_EDGE ( 'NONE', *, *, #62690, .T. ) ;
#48936 =( GEOMETRIC_REPRESENTATION_CONTEXT ( 3 ) GLOBAL_UNCERTAINTY_ASSIGNED_CONTEXT ( ( #58056 ) ) GLOBAL_UNIT_ASSIGNED_CONTEXT ( ( #8196, #67269, #29979 ) ) REPRESENTATION_CONTEXT ( 'NONE', 'WORKASPACE' ) );
#48938 = CARTESIAN_POINT ( 'NONE',  ( 73.01088739851488185, 5.000000000000000000, -65.71817553072278884 ) ) ;
#48939 = DIRECTION ( 'NONE',  ( 1.000000000000000000, -0.000000000000000000, 1.982541115402069054E-16 ) ) ;
#48940 = FILL_AREA_STYLE ('',( #48591 ) ) ;
#48941 = CARTESIAN_POINT ( 'NONE',  ( -74.99999999999998579, 50.00000000000000000, 12.00000000000000000 ) ) ;
#48942 = PRESENTATION_LAYER_ASSIGNMENT (  '', '', ( #35439 ) ) ;
#48943 = CARTESIAN_POINT ( 'NONE',  ( -5.196152422706636465, 2.500000000000000000, -9.000000000000003553 ) ) ;
#48944 = EDGE_LOOP ( 'NONE', ( #30035, #55938, #63681, #13432 ) ) ;
#48945 = EDGE_CURVE ( 'NONE', #2052, #12977, #35376, .T. ) ;
#48946 = CIRCLE ( 'NONE', #18570, 19.99999999999998934 ) ;
#48947 = PRESENTATION_STYLE_ASSIGNMENT (( #16581 ) ) ;
#48948 = FACE_OUTER_BOUND ( 'NONE', #14164, .T. ) ;
#48949 = CARTESIAN_POINT ( 'NONE',  ( -106.4949999999999903, 6.826472737025113702, -4.959722759717902107 ) ) ;
#48950 = CARTESIAN_POINT ( 'NONE',  ( 0.000000000000000000, 110.5549999999999926, -9.525000000000000355 ) ) ;
#48951 = CARTESIAN_POINT ( 'NONE',  ( -82.94499999999999318, -9.827790563157499189E-16, -8.024999999999991473 ) ) ;
#48952 = FILL_AREA_STYLE_COLOUR ( '', #67890 ) ;
#48953 = SURFACE_STYLE_FILL_AREA ( #21838 ) ;
#48954 = DIRECTION ( 'NONE',  ( -1.000000000000000000, -0.000000000000000000, -0.000000000000000000 ) ) ;
#48955 = UNCERTAINTY_MEASURE_WITH_UNIT (LENGTH_MEASURE( 1.000000000000000082E-05 ), #51460, 'distance_accuracy_value', 'NONE');
#48956 = PRESENTATION_LAYER_ASSIGNMENT (  '', '', ( #5065 ) ) ;
#48957 = FILL_AREA_STYLE ('',( #26407 ) ) ;
#48958 = ORIENTED_EDGE ( 'NONE', *, *, #53728, .T. ) ;
#48959 = CARTESIAN_POINT ( 'NONE',  ( -120.5929263765337822, -3.094860106618431139, -9.524999999999991473 ) ) ;
#48960 = FILL_AREA_STYLE ('',( #55576 ) ) ;
#48961 = CARTESIAN_POINT ( 'NONE',  ( -149.8449999999999989, -7.632228543268599452, 2.479861379858951054 ) ) ;
#48962 = DIRECTION ( 'NONE',  ( 0.000000000000000000, 0.000000000000000000, 1.000000000000000000 ) ) ;
#48963 = EDGE_CURVE ( 'NONE', #51627, #2848, #21774, .T. ) ;
#48964 = MECHANICAL_DESIGN_GEOMETRIC_PRESENTATION_REPRESENTATION (  '', ( #39966 ), #65732 ) ;
#48965 = ADVANCED_FACE ( 'NONE', ( #59372 ), #28557, .T. ) ;
#48966 = CARTESIAN_POINT ( 'NONE',  ( -79.99999999999998579, 50.00000000000000000, 6.999999999999988454 ) ) ;
#48967 = CARTESIAN_POINT ( 'NONE',  ( -112.5570736234661808, -1.166476076187852838E-15, -9.524999999999991473 ) ) ;
#48968 = ORIENTED_EDGE ( 'NONE', *, *, #46270, .F. ) ;
#48969 = ORIENTED_EDGE ( 'NONE', *, *, #19604, .T. ) ;
#48970 = VECTOR ( 'NONE', #10822, 1000.000000000000000 ) ;
#48971 = EDGE_CURVE ( 'NONE', #39571, #36987, #19887, .T. ) ;
#48972 = CARTESIAN_POINT ( 'NONE',  ( -153.4429263765338192, -1.166476076187852838E-15, -9.524999999999991473 ) ) ;
#48973 = ADVANCED_FACE ( 'NONE', ( #4172, #26341 ), #10534, .T. ) ;
#48974 = FACE_OUTER_BOUND ( 'NONE', #67566, .T. ) ;
#48975 = FILL_AREA_STYLE_COLOUR ( '', #34829 ) ;
#48976 = DIRECTION ( 'NONE',  ( -0.000000000000000000, -0.000000000000000000, 1.000000000000000000 ) ) ;
#48977 = DIRECTION ( 'NONE',  ( 0.000000000000000000, 1.000000000000000000, 0.000000000000000000 ) ) ;
#48978 = ORIENTED_EDGE ( 'NONE', *, *, #3619, .T. ) ;
#48979 = CARTESIAN_POINT ( 'NONE',  ( -141.2050000000000125, -2.607480562269071545, -8.024999999999991473 ) ) ;
#48980 = ORIENTED_EDGE ( 'NONE', *, *, #6923, .F. ) ;
#48981 = MECHANICAL_DESIGN_GEOMETRIC_PRESENTATION_REPRESENTATION (  '', ( #16384 ), #42273 ) ;
#48982 = ORIENTED_EDGE ( 'NONE', *, *, #12377, .T. ) ;
#48983 = SURFACE_SIDE_STYLE ('',( #23248 ) ) ;
#48984 = ORIENTED_EDGE ( 'NONE', *, *, #47197, .F. ) ;
#48985 = EDGE_CURVE ( 'NONE', #38290, #16746, #5227, .T. ) ;
#48986 = CARTESIAN_POINT ( 'NONE',  ( -2.243484957755116138, 2.233878551459168360, -9.000000000000003553 ) ) ;
#48987 = PLANE ( 'NONE',  #26437 ) ;
#48988 = CARTESIAN_POINT ( 'NONE',  ( 9.058813317711338797, 126.8449999999999847, -2.943386871421372675 ) ) ;
#48989 = DIRECTION ( 'NONE',  ( 0.000000000000000000, 1.000000000000000000, 0.000000000000000000 ) ) ;
#48990 = ORIENTED_EDGE ( 'NONE', *, *, #67595, .F. ) ;
#48991 = DIRECTION ( 'NONE',  ( -0.000000000000000000, -0.000000000000000000, -1.000000000000000000 ) ) ;
#48992 = CARTESIAN_POINT ( 'NONE',  ( -9.058813317711337021, 132.1550000000000011, -2.943386871421374895 ) ) ;
#48993 = CARTESIAN_POINT ( 'NONE',  ( -58.25499999999997414, -4.716976649647092401, 6.492361379858946790 ) ) ;
#48994 = VECTOR ( 'NONE', #34543, 1000.000000000000000 ) ;
#48995 = CARTESIAN_POINT ( 'NONE',  ( -122.5449999999999875, -7.632228543268600340, -2.479861379858950166 ) ) ;
#48996 = EDGE_CURVE ( 'NONE', #68077, #32017, #44461, .T. ) ;
#48997 = FACE_OUTER_BOUND ( 'NONE', #67490, .T. ) ;
#48998 = ORIENTED_EDGE ( 'NONE', *, *, #63838, .F. ) ;
#48999 = CARTESIAN_POINT ( 'NONE',  ( -3.094860106618434248, 156.9050000000000011, 9.525000000000000355 ) ) ;
#49000 = LINE ( 'NONE', #63136, #26610 ) ;
#49001 = UNCERTAINTY_MEASURE_WITH_UNIT (LENGTH_MEASURE( 1.000000000000000082E-05 ), #26256, 'distance_accuracy_value', 'NONE');
#49002 = DIRECTION ( 'NONE',  ( -0.000000000000000000, -1.000000000000000000, -0.000000000000000000 ) ) ;
#49003 = ORIENTED_EDGE ( 'NONE', *, *, #5292, .T. ) ;
#49004 = CARTESIAN_POINT ( 'NONE',  ( -175.1050000000000182, -6.826472737025115478, 4.959722759717900331 ) ) ;
#49005 = ORIENTED_EDGE ( 'NONE', *, *, #13762, .T. ) ;
#49006 = UNCERTAINTY_MEASURE_WITH_UNIT (LENGTH_MEASURE( 1.000000000000000082E-05 ), #16538, 'distance_accuracy_value', 'NONE');
#49007 = AXIS2_PLACEMENT_3D ( 'NONE', #26878, #15690, #4761 ) ;
#49008 =( LENGTH_UNIT ( ) NAMED_UNIT ( * ) SI_UNIT ( .MILLI., .METRE. ) );
#49009 = FILL_AREA_STYLE_COLOUR ( '', #52307 ) ;
#49010 = PRESENTATION_STYLE_ASSIGNMENT (( #53886 ) ) ;
#49011 = ORIENTED_EDGE ( 'NONE', *, *, #33123, .F. ) ;
#49012 = CARTESIAN_POINT ( 'NONE',  ( -18.00000000000000711, 31.24999999999999289, -4.000000000000000000 ) ) ;
#49013 = CIRCLE ( 'NONE', #53445, 12.50000000000000355 ) ;
#49014 = CARTESIAN_POINT ( 'NONE',  ( -45.89905495956738690, 9.405628579031731107, -3.000000000000000444 ) ) ;
#49015 = CARTESIAN_POINT ( 'NONE',  ( -85.40499999999998693, -2.607480562269069768, 8.024999999999991473 ) ) ;
#49016 = ORIENTED_EDGE ( 'NONE', *, *, #39445, .T. ) ;
#49017 = CARTESIAN_POINT ( 'NONE',  ( -40.70406133565712992, -11.08928571428570997, 0.8979962945199000401 ) ) ;
#49018 = CARTESIAN_POINT ( 'NONE',  ( -21.02379604162863913, 114.4999999999999574, 10.00000000000000000 ) ) ;
#49019 = COLOUR_RGB ( '', 0.72549020, 0.75294118, 0.79215686) ;
#49020 = MECHANICAL_DESIGN_GEOMETRIC_PRESENTATION_REPRESENTATION (  '', ( #18651 ), #69217 ) ;
#49021 = MECHANICAL_DESIGN_GEOMETRIC_PRESENTATION_REPRESENTATION (  '', ( #36679 ), #16429 ) ;
#49022 =( BOUNDED_CURVE ( )  B_SPLINE_CURVE ( 2, ( #24797, #18507, #39997, #51213, #34661, #13555, #7943, #29385, #35022, #56475, #35385 ),
 .UNSPECIFIED., .F., .F. ) 
 B_SPLINE_CURVE_WITH_KNOTS ( ( 3, 2, 2, 2, 2, 3 ),
 ( 0.7826086956521739468, 0.7847826086956521952, 0.7869565217391304435, 0.7891304347826086918, 0.7913043478260869401, 0.7934782608695651884 ),
 .UNSPECIFIED. ) 
 CURVE ( )  GEOMETRIC_REPRESENTATION_ITEM ( )  RATIONAL_B_SPLINE_CURVE ( ( 1.000000000000000000, 0.9510565162951535312, 1.000000000000000000, 0.9510565162951535312, 1.000000000000000000, 0.9510565162951535312, 1.000000000000000000, 0.9510565162951535312, 1.000000000000000000, 0.9510565162951535312, 1.000000000000000000 ) ) 
 REPRESENTATION_ITEM ( '' )  );
#49023 = CARTESIAN_POINT ( 'NONE',  ( -60.00000000000000000, -2.024042244987997205E-14, -12.00000000000000000 ) ) ;
#49024 = DIRECTION ( 'NONE',  ( 0.000000000000000000, 1.000000000000000000, 0.000000000000000000 ) ) ;
#49025 = CARTESIAN_POINT ( 'NONE',  ( -64.10707362346616378, 8.102448949553171076, -5.886773742842744461 ) ) ;
#49026 = EDGE_CURVE ( 'NONE', #18324, #25577, #7303, .T. ) ;
#49027 = LINE ( 'NONE', #43746, #11174 ) ;
#49028 = ORIENTED_EDGE ( 'NONE', *, *, #19201, .F. ) ;
#49029 = CARTESIAN_POINT ( 'NONE',  ( 0.000000000000000000, 149.9999999999999716, 0.000000000000000000 ) ) ;
#49031 = CARTESIAN_POINT ( 'NONE',  ( 0.000000000000000000, 42.00000000000000000, -45.61250543006183733 ) ) ;
#49030 = DIRECTION ( 'NONE',  ( -0.000000000000000000, 1.000000000000000000, -0.000000000000000000 ) ) ;
#49032 = VECTOR ( 'NONE', #68158, 1000.000000000000000 ) ;
#49033 = CARTESIAN_POINT ( 'NONE',  ( -103.1049999999999756, -6.826472737025115478, 4.959722759717900331 ) ) ;
#49034 = CARTESIAN_POINT ( 'NONE',  ( 10.01517768586949231, 129.6949999999999648, 1.839758294383810543E-15 ) ) ;
#49035 = CARTESIAN_POINT ( 'NONE',  ( -118.1949999999999790, 8.437984349512085203, -1.550032578732815448E-15 ) ) ;
#49036 = CIRCLE ( 'NONE', #32124, 0.2500000000000002220 ) ;
#49038 = DIRECTION ( 'NONE',  ( 0.000000000000000000, 0.000000000000000000, -1.000000000000000000 ) ) ;
#49037 = CARTESIAN_POINT ( 'NONE',  ( 23.21231517720797655, 117.9999999999999716, -9.500000000000000000 ) ) ;
#49039 = EDGE_CURVE ( 'NONE', #31350, #18241, #26415, .T. ) ;
#49040 = CARTESIAN_POINT ( 'NONE',  ( -154.9429263765338192, 0.000000000000000000, 9.524999999999991473 ) ) ;
#49041 = CARTESIAN_POINT ( 'NONE',  ( -172.3449999999999989, 7.632228543268599452, -2.479861379858951942 ) ) ;
#49042 = EDGE_CURVE ( 'NONE', #2488, #4575, #42932, .T. ) ;
#49043 = EDGE_CURVE ( 'NONE', #8109, #4457, #23484, .T. ) ;
#49044 = CARTESIAN_POINT ( 'NONE',  ( -4.716976649647097730, 148.3570736234661638, -6.492361379858953896 ) ) ;
#49045 = CARTESIAN_POINT ( 'NONE',  ( -44.93692584854336758, -12.13384599889156945, 3.189947921310896994 ) ) ;
#49046 = ORIENTED_EDGE ( 'NONE', *, *, #16151, .F. ) ;
#49047 = DIRECTION ( 'NONE',  ( -1.000000000000000000, 0.000000000000000000, 0.000000000000000000 ) ) ;
#49048 =( NAMED_UNIT ( * ) SI_UNIT ( $, .STERADIAN. ) SOLID_ANGLE_UNIT ( ) );
#49049 = ORIENTED_EDGE ( 'NONE', *, *, #46171, .F. ) ;
#49050 = CARTESIAN_POINT ( 'NONE',  ( -64.04292637653379927, -9.058813317711329915, -2.943386871421370898 ) ) ;
#49051 = CONTEXT_DEPENDENT_SHAPE_REPRESENTATION ( #49162, #11528 ) ;
#49052 = DIRECTION ( 'NONE',  ( -1.000000000000000000, -0.000000000000000000, -0.000000000000000000 ) ) ;
#49053 = EDGE_CURVE ( 'NONE', #63380, #63408, #64596, .T. ) ;
#49054 = DIRECTION ( 'NONE',  ( 0.000000000000000000, 0.000000000000000000, 1.000000000000000000 ) ) ;
#49055 = CARTESIAN_POINT ( 'NONE',  ( 0.000000000000000000, 42.00000000000000000, 75.00000000000001421 ) ) ;
#49056 = DIRECTION ( 'NONE',  ( 1.000000000000000000, 0.000000000000000000, 0.000000000000000000 ) ) ;
#49057 = ADVANCED_FACE ( 'NONE', ( #6601 ), #12578, .T. ) ;
#49058 = FACE_OUTER_BOUND ( 'NONE', #36005, .T. ) ;
#49059 = COLOUR_RGB ( '', 0.66274510, 0.83137255, 0.94901961) ;
#49060 = ORIENTED_EDGE ( 'NONE', *, *, #46667, .F. ) ;
#49061 = CARTESIAN_POINT ( 'NONE',  ( -166.4049999999999727, -2.607480562269069768, 8.024999999999991473 ) ) ;
#49062 = ORIENTED_EDGE ( 'NONE', *, *, #30072, .F. ) ;
#49063 = CARTESIAN_POINT ( 'NONE',  ( 4.000000000000002665, 38.70020753820971748, -90.00000000000000000 ) ) ;
#49064 = FILL_AREA_STYLE ('',( #63800 ) ) ;
#49065 = CARTESIAN_POINT ( 'NONE',  ( -34.99999999999992895, 112.4999999999999858, -10.00000000000000000 ) ) ;
#49066 = VECTOR ( 'NONE', #48300, 1000.000000000000000 ) ;
#49067 = CARTESIAN_POINT ( 'NONE',  ( 44.25000000000000000, 19.24999999999998224, -3.750000000000000000 ) ) ;
#49068 = CARTESIAN_POINT ( 'NONE',  ( 6.826472737025119919, 150.0070736234661695, 4.959722759717908325 ) ) ;
#49069 = EDGE_LOOP ( 'NONE', ( #44804, #41133, #43003, #15773, #51200, #51352, #4805, #25403, #46758, #18320, #12407, #19686, #54240 ) ) ;
#49070 = CARTESIAN_POINT ( 'NONE',  ( -95.00499999999998124, 6.826472737025115478, 4.959722759717899443 ) ) ;
#49071 = UNCERTAINTY_MEASURE_WITH_UNIT (LENGTH_MEASURE( 1.000000000000000082E-05 ), #27531, 'distance_accuracy_value', 'NONE');
#49072 = DIRECTION ( 'NONE',  ( 1.300977106640434891E-16, -0.000000000000000000, 1.000000000000000000 ) ) ;
#49073 = ORIENTED_EDGE ( 'NONE', *, *, #13762, .F. ) ;
#49074 = DIRECTION ( 'NONE',  ( 0.000000000000000000, 1.000000000000000000, 0.000000000000000000 ) ) ;
#49075 = DIRECTION ( 'NONE',  ( -1.000000000000000000, 0.000000000000000000, 0.000000000000000000 ) ) ;
#49076 = ORIENTED_EDGE ( 'NONE', *, *, #32109, .T. ) ;
#49077 = PRESENTATION_STYLE_ASSIGNMENT (( #37846 ) ) ;
#49078 = ADVANCED_FACE ( 'NONE', ( #49904 ), #65374, .F. ) ;
#49079 = CARTESIAN_POINT ( 'NONE',  ( -60.44499999999998607, 0.000000000000000000, 8.024999999999991473 ) ) ;
#49080 = ORIENTED_EDGE ( 'NONE', *, *, #53794, .F. ) ;
#49081 = DIRECTION ( 'NONE',  ( 0.000000000000000000, 0.000000000000000000, 1.000000000000000000 ) ) ;
#49082 = CARTESIAN_POINT ( 'NONE',  ( -45.00000000000000000, 9.701542612659405762, -6.099661992412403144 ) ) ;
#49083 = ORIENTED_EDGE ( 'NONE', *, *, #65289, .T. ) ;
#49084 = FACE_OUTER_BOUND ( 'NONE', #27090, .T. ) ;
#49085 = CYLINDRICAL_SURFACE ( 'NONE', #50550, 0.2500000000000002220 ) ;
#49086 = ORIENTED_EDGE ( 'NONE', *, *, #41979, .T. ) ;
#49087 = CARTESIAN_POINT ( 'NONE',  ( 45.65811388298785545, 10.21937129432926916, -6.131267346259138940 ) ) ;
#49088 = CARTESIAN_POINT ( 'NONE',  ( -117.6550000000000011, -7.632228543268600340, -2.479861379858950166 ) ) ;
#49089 = VERTEX_POINT ( 'NONE', #1962 ) ;
#49090 = CARTESIAN_POINT ( 'NONE',  ( 45.00000000000000000, 99.99999999999992895, 9.500000000000000000 ) ) ;
#49091 = CARTESIAN_POINT ( 'NONE',  ( -73.94292637653379074, 0.000000000000000000, 9.524999999999991473 ) ) ;
#49092 = FACE_OUTER_BOUND ( 'NONE', #41231, .T. ) ;
#49093 = DIRECTION ( 'NONE',  ( 0.000000000000000000, 0.000000000000000000, 1.000000000000000000 ) ) ;
#49094 = CARTESIAN_POINT ( 'NONE',  ( 12.25000000000000533, 28.24999999999998224, -4.000000000000000000 ) ) ;
#49095 = CARTESIAN_POINT ( 'NONE',  ( -147.6570736234662036, 9.058813317711329915, 2.943386871421369566 ) ) ;
#49096 = CARTESIAN_POINT ( 'NONE',  ( 3.094860106618431583, 132.0949999999999989, 9.525000000000000355 ) ) ;
#49097 = CARTESIAN_POINT ( 'NONE',  ( -92.30707362346618083, -10.01517768586948698, 6.132527647946031529E-16 ) ) ;
#49098 = CARTESIAN_POINT ( 'NONE',  ( -0.3706977682293637888, 154.4502386517839341, -9.475238651784067656 ) ) ;
#49099 = EDGE_LOOP ( 'NONE', ( #25301, #39704, #41962, #35543 ) ) ;
#49100 = CARTESIAN_POINT ( 'NONE',  ( 0.000000000000000000, 0.000000000000000000, 0.000000000000000000 ) ) ;
#49102 = PLANE ( 'NONE',  #917 ) ;
#49101 = PRESENTATION_STYLE_ASSIGNMENT (( #49427 ) ) ;
#49104 = SURFACE_SIDE_STYLE ('',( #11424 ) ) ;
#49103 = VECTOR ( 'NONE', #66341, 1000.000000000000000 ) ;
#49105 = CARTESIAN_POINT ( 'NONE',  ( -128.3050000000000068, 8.437984349512085203, -1.550032578732815448E-15 ) ) ;
#49106 = CARTESIAN_POINT ( 'NONE',  ( -9.250000000000003553, 27.74999999999998934, -3.750000000000000000 ) ) ;
#49107 = AXIS2_PLACEMENT_3D ( 'NONE', #22935, #54226, #53880 ) ;
#49108 = DIRECTION ( 'NONE',  ( -1.000000000000000000, 2.055968564120660634E-14, 0.000000000000000000 ) ) ;
#49109 = CARTESIAN_POINT ( 'NONE',  ( -54.59292637653378222, -3.094860106618431139, -9.524999999999991473 ) ) ;
#49110 = EDGE_CURVE ( 'NONE', #26732, #9217, #2785, .T. ) ;
#49111 = CARTESIAN_POINT ( 'NONE',  ( -140.8449999999999989, -7.632228543268599452, 2.479861379858951054 ) ) ;
#49112 = CARTESIAN_POINT ( 'NONE',  ( -131.8449999999999989, -7.632228543268599452, 2.479861379858951054 ) ) ;
#49113 = ORIENTED_EDGE ( 'NONE', *, *, #54155, .T. ) ;
#49114 =( BOUNDED_CURVE ( )  B_SPLINE_CURVE ( 2, ( #15770, #37602, #21714, #21023, #5174, #37944, #59318, #32595, #32263, #26620, #42516 ),
 .UNSPECIFIED., .F., .F. ) 
 B_SPLINE_CURVE_WITH_KNOTS ( ( 3, 2, 2, 2, 2, 3 ),
 ( 0.08823529411764713393, 0.09411764705882361137, 0.1000000000000000888, 0.1058823529411765663, 0.1117647058823530437, 0.1176470588235295212 ),
 .UNSPECIFIED. ) 
 CURVE ( )  GEOMETRIC_REPRESENTATION_ITEM ( )  RATIONAL_B_SPLINE_CURVE ( ( 0.9999999999999994449, 0.9510565162951540863, 1.000000000000000000, 0.9510565162951535312, 1.000000000000000000, 0.9510565162951535312, 1.000000000000000000, 0.9510565162951535312, 1.000000000000000000, 0.9510565162951526430, 1.000000000000000888 ) ) 
 REPRESENTATION_ITEM ( '' )  );
#49115 = CARTESIAN_POINT ( 'NONE',  ( 45.00000000011532109, 10.00000000003076295, -3.953713388244109339 ) ) ;
#49116 = EDGE_CURVE ( 'NONE', #51841, #29900, #55140, .T. ) ;
#49117 = SURFACE_STYLE_FILL_AREA ( #27595 ) ;
#49118 = CARTESIAN_POINT ( 'NONE',  ( -182.9929263765338021, 8.102448949553171076, -5.886773742842744461 ) ) ;
#49119 = CARTESIAN_POINT ( 'NONE',  ( -62.09499999999998465, -2.607480562269071545, -8.024999999999991473 ) ) ;
#49120 = AXIS2_PLACEMENT_3D ( 'NONE', #49310, #13045, #22568 ) ;
#49121 = ADVANCED_FACE ( 'NONE', ( #66400 ), #1668, .F. ) ;
#49122 = CARTESIAN_POINT ( 'NONE',  ( -139.7929263765343535, -3.094860106609085726, 9.525000000006778933 ) ) ;
#49123 = CARTESIAN_POINT ( 'NONE',  ( -74.99999999999998579, 36.00000000000000711, 6.499999999999999112 ) ) ;
#49124 = DIRECTION ( 'NONE',  ( -0.4999999999999997780, 0.8660254037844387076, 0.000000000000000000 ) ) ;
#49125 = CARTESIAN_POINT ( 'NONE',  ( -108.5929263765338106, -3.094860106618431139, -9.524999999999991473 ) ) ;
#49126 = DIRECTION ( 'NONE',  ( -1.110223024625156540E-15, 0.9592475516106591105, 0.2825670446618929188 ) ) ;
#49127 = FACE_OUTER_BOUND ( 'NONE', #26383, .T. ) ;
#49128 = CARTESIAN_POINT ( 'NONE',  ( 18.25000000000000711, 33.74999999999999289, -4.000000000000000000 ) ) ;
#49129 = CARTESIAN_POINT ( 'NONE',  ( -99.05707362346618083, 0.000000000000000000, 9.524999999999991473 ) ) ;
#49130 = ADVANCED_FACE ( 'NONE', ( #38337 ), #18886, .F. ) ;
#49131 = DIRECTION ( 'NONE',  ( 0.000000000000000000, 0.000000000000000000, 1.000000000000000000 ) ) ;
#49132 = VERTEX_POINT ( 'NONE', #24866 ) ;
#49133 = PLANE ( 'NONE',  #3728 ) ;
#49134 = ORIENTED_EDGE ( 'NONE', *, *, #735, .F. ) ;
#49135 = CARTESIAN_POINT ( 'NONE',  ( -9.827790563157511022E-16, 122.5570736234661524, 8.025000000000000355 ) ) ;
#49136 = SURFACE_STYLE_FILL_AREA ( #5830 ) ;
#49137 = ORIENTED_EDGE ( 'NONE', *, *, #46270, .T. ) ;
#49138 = ORIENTED_EDGE ( 'NONE', *, *, #20160, .T. ) ;
#49139 = FACE_OUTER_BOUND ( 'NONE', #50112, .T. ) ;
#49140 = ORIENTED_EDGE ( 'NONE', *, *, #28157, .T. ) ;
#49141 = CIRCLE ( 'NONE', #27747, 0.2500000000000002220 ) ;
#49142 = CARTESIAN_POINT ( 'NONE',  ( -119.9070736234669567, -3.094860106605456185, 9.525000000009420376 ) ) ;
#49143 = DIRECTION ( 'NONE',  ( 1.000000000000000000, 0.000000000000000000, 0.000000000000000000 ) ) ;
#49144 = EDGE_CURVE ( 'NONE', #1306, #33888, #10713, .T. ) ;
#49145 = CARTESIAN_POINT ( 'NONE',  ( -93.29499999999998749, -2.607480562269069768, 8.024999999999991473 ) ) ;
#49146 = ORIENTED_EDGE ( 'NONE', *, *, #4171, .T. ) ;
#49147 = DIRECTION ( 'NONE',  ( -1.000000000000000000, 0.000000000000000000, 0.000000000000000000 ) ) ;
#49148 = CARTESIAN_POINT ( 'NONE',  ( 44.50000000000000000, 99.99999999999992895, -4.000000000000000000 ) ) ;
#49149 = DIRECTION ( 'NONE',  ( 0.000000000000000000, -1.000000000000000000, 0.000000000000000000 ) ) ;
#49150 = ORIENTED_EDGE ( 'NONE', *, *, #6372, .T. ) ;
#49151 = CARTESIAN_POINT ( 'NONE',  ( -8.437984349512095861, 159.6929263765338192, -5.166775262442723748E-16 ) ) ;
#49152 = AXIS2_PLACEMENT_3D ( 'NONE', #50945, #45360, #45702 ) ;
#49153 = CARTESIAN_POINT ( 'NONE',  ( 7.794228634059946259, 2.500000000000000000, -4.500000000000001776 ) ) ;
#49154 = ORIENTED_EDGE ( 'NONE', *, *, #49992, .T. ) ;
#49155 = CARTESIAN_POINT ( 'NONE',  ( -195.0000000000000000, 0.000000000000000000, 0.000000000000000000 ) ) ;
#49156 = ORIENTED_EDGE ( 'NONE', *, *, #49300, .F. ) ;
#49157 = CARTESIAN_POINT ( 'NONE',  ( -165.2070736234663855, 3.094860106621995399, 9.524999999997403322 ) ) ;
#49158 = DIRECTION ( 'NONE',  ( 0.000000000000000000, 0.000000000000000000, 1.000000000000000000 ) ) ;
#49159 = CARTESIAN_POINT ( 'NONE',  ( 12.75000000000000533, 28.24999999999998224, 3.750000000000000000 ) ) ;
#49160 = CARTESIAN_POINT ( 'NONE',  ( -182.9070736234661751, -3.094860106618429807, 9.524999999999991473 ) ) ;
#49161 = CARTESIAN_POINT ( 'NONE',  ( 44.25000000000000000, 19.24999999999998224, -4.000000000000000000 ) ) ;
#49162 =( REPRESENTATION_RELATIONSHIP ('NONE','NONE', #5102, #38844 ) REPRESENTATION_RELATIONSHIP_WITH_TRANSFORMATION ( #5726 )SHAPE_REPRESENTATION_RELATIONSHIP( ) );
#49163 = CARTESIAN_POINT ( 'NONE',  ( -5.196152422706634688, 9.000000000000008882, 1.392304845413263159 ) ) ;
#49164 = CARTESIAN_POINT ( 'NONE',  ( -3.105708046185574389, 153.1036296714643754, -7.531667776144036708 ) ) ;
#49165 = ORIENTED_EDGE ( 'NONE', *, *, #50529, .F. ) ;
#49166 = DIRECTION ( 'NONE',  ( 1.000000000000000000, 0.000000000000000000, 0.000000000000000000 ) ) ;
#49167 = DIRECTION ( 'NONE',  ( 0.000000000000000000, -1.000000000000000000, 0.000000000000000000 ) ) ;
#49168 = SURFACE_STYLE_USAGE ( .BOTH. , #12182 ) ;
#49169 = ORIENTED_EDGE ( 'NONE', *, *, #62001, .T. ) ;
#49170 =( NAMED_UNIT ( * ) PLANE_ANGLE_UNIT ( ) SI_UNIT ( $, .RADIAN. ) );
#49171 = CARTESIAN_POINT ( 'NONE',  ( -158.7549999999999670, 4.716976649647091513, -6.492361379858946790 ) ) ;
#49172 = DIRECTION ( 'NONE',  ( -1.000000000000000000, 0.000000000000000000, 0.000000000000000000 ) ) ;
#49173 = CARTESIAN_POINT ( 'NONE',  ( -183.8059463088887640, -8.116739841473526340, -3.200022323834349702 ) ) ;
#49174 = EDGE_CURVE ( 'NONE', #59012, #24116, #3733, .T. ) ;
#49175 = CARTESIAN_POINT ( 'NONE',  ( -175.1949999999999932, 8.437984349512085203, -1.550032578732815448E-15 ) ) ;
#49176 = CARTESIAN_POINT ( 'NONE',  ( -171.7450000000000045, 4.716976649647094177, 6.492361379858945902 ) ) ;
#49177 = EDGE_LOOP ( 'NONE', ( #20474, #57472, #8748, #41640 ) ) ;
#49178 = DIRECTION ( 'NONE',  ( 0.000000000000000000, 0.000000000000000000, -1.000000000000000000 ) ) ;
#49179 = CARTESIAN_POINT ( 'NONE',  ( 44.94709371290443300, 9.982364570967702022, 3.713690726390154850 ) ) ;
#49180 = CARTESIAN_POINT ( 'NONE',  ( -86.75499999999998124, 4.716976649647091513, -6.492361379858946790 ) ) ;
#49181 = CARTESIAN_POINT ( 'NONE',  ( -195.0000000000000000, 0.000000000000000000, 0.000000000000000000 ) ) ;
#49182 = MECHANICAL_DESIGN_GEOMETRIC_PRESENTATION_REPRESENTATION (  '', ( #58164 ), #37968 ) ;
#49183 = AXIS2_PLACEMENT_3D ( 'NONE', #28797, #27741, #49245 ) ;
#49184 = EDGE_CURVE ( 'NONE', #6631, #67791, #25272, .T. ) ;
#49185 = CARTESIAN_POINT ( 'NONE',  ( -77.54499999999998749, -7.632228543268600340, -2.479861379858950166 ) ) ;
#49186 = CARTESIAN_POINT ( 'NONE',  ( -9.058813317711338797, 132.4549999999999841, 2.943386871421373563 ) ) ;
#49187 = EDGE_CURVE ( 'NONE', #21071, #50108, #29084, .T. ) ;
#49188 = CARTESIAN_POINT ( 'NONE',  ( 3.569376287083594779, 154.2959099316039726, 8.618005638701651705 ) ) ;
#49189 = FACE_OUTER_BOUND ( 'NONE', #23228, .T. ) ;
#49190 = ORIENTED_EDGE ( 'NONE', *, *, #42143, .T. ) ;
#49191 = ADVANCED_FACE ( 'NONE', ( #35452 ), #2310, .T. ) ;
#49192 = CARTESIAN_POINT ( 'NONE',  ( 10.57623092156537936, 58.31681314173471975, -6.349999999999996092 ) ) ;
#49193 =( NAMED_UNIT ( * ) PLANE_ANGLE_UNIT ( ) SI_UNIT ( $, .RADIAN. ) );
#49194 = STYLED_ITEM ( 'NONE', ( #28276 ), #67472 ) ;
#49196 = EDGE_CURVE ( 'NONE', #17573, #46287, #40058, .T. ) ;
#49195 = VECTOR ( 'NONE', #16385, 1000.000000000000000 ) ;
#49197 = CARTESIAN_POINT ( 'NONE',  ( 11.00000000000001776, 42.00000000000000000, 29.68999999999999417 ) ) ;
#49198 = ORIENTED_EDGE ( 'NONE', *, *, #68793, .F. ) ;
#49199 = ORIENTED_EDGE ( 'NONE', *, *, #13363, .F. ) ;
#49200 = FILL_AREA_STYLE ('',( #27697 ) ) ;
#49201 = LINE ( 'NONE', #12571, #63099 ) ;
#49202 = CYLINDRICAL_SURFACE ( 'NONE', #2273, 1.000000000000000888 ) ;
#49203 = CARTESIAN_POINT ( 'NONE',  ( 0.000000000000000000, 0.000000000000000000, -3.000000000000000000 ) ) ;
#49204 = VERTEX_POINT ( 'NONE', #9767 ) ;
#49205 = CARTESIAN_POINT ( 'NONE',  ( -116.6049999999999898, 6.826472737025113702, -4.959722759717902107 ) ) ;
#49206 = ORIENTED_EDGE ( 'NONE', *, *, #16078, .T. ) ;
#49207 = PRESENTATION_STYLE_ASSIGNMENT (( #44653 ) ) ;
#49208 = VERTEX_POINT ( 'NONE', #16094 ) ;
#49209 = DIRECTION ( 'NONE',  ( 0.000000000000000000, 1.000000000000000000, -0.000000000000000000 ) ) ;
#49210 = CARTESIAN_POINT ( 'NONE',  ( -7.441974819423173848, -2.003239292658529180, 1.110121504110835877 ) ) ;
#49211 = ORIENTED_EDGE ( 'NONE', *, *, #26051, .T. ) ;
#49212 =( LENGTH_UNIT ( ) NAMED_UNIT ( * ) SI_UNIT ( .MILLI., .METRE. ) );
#49213 = VERTEX_POINT ( 'NONE', #37213 ) ;
#49214 = ORIENTED_EDGE ( 'NONE', *, *, #56594, .T. ) ;
#49215 = CARTESIAN_POINT ( 'NONE',  ( 72.50000000000000000, 35.92875272052971525, -10.00000000000000000 ) ) ;
#49216 = PRESENTATION_STYLE_ASSIGNMENT (( #12592 ) ) ;
#49217 = DIRECTION ( 'NONE',  ( 0.000000000000000000, 1.000000000000000000, 0.000000000000000000 ) ) ;
#49218 = ORIENTED_EDGE ( 'NONE', *, *, #2834, .F. ) ;
#49219 = CARTESIAN_POINT ( 'NONE',  ( -2.607480562269075097, 136.2929263765337851, 8.025000000000000355 ) ) ;
#49220 = CARTESIAN_POINT ( 'NONE',  ( -15.48999599679679662, 146.4999999999999716, -10.00000000000000000 ) ) ;
#49221 = CARTESIAN_POINT ( 'NONE',  ( -195.0000000000000000, 0.000000000000000000, 0.000000000000000000 ) ) ;
#49222 = PRESENTATION_LAYER_ASSIGNMENT (  '', '', ( #39104 ) ) ;
#49223 = AXIS2_PLACEMENT_3D ( 'NONE', #7609, #19554, #18846 ) ;
#49224 = DIRECTION ( 'NONE',  ( 1.000000000000000000, -0.000000000000000000, -0.000000000000000000 ) ) ;
#49225 = DIRECTION ( 'NONE',  ( 0.000000000000000000, 0.000000000000000000, -1.000000000000000000 ) ) ;
#49226 = ORIENTED_EDGE ( 'NONE', *, *, #8840, .F. ) ;
#49227 = DIRECTION ( 'NONE',  ( -1.000000000000000000, 0.000000000000000000, 0.000000000000000000 ) ) ;
#49228 = ORIENTED_EDGE ( 'NONE', *, *, #66881, .F. ) ;
#49229 = CARTESIAN_POINT ( 'NONE',  ( 61.74999999999998579, 31.24999999999999289, -4.000000000000000000 ) ) ;
#49230 = DIRECTION ( 'NONE',  ( 1.000000000000000000, 0.000000000000000000, 0.000000000000000000 ) ) ;
#49231 = PLANE ( 'NONE',  #31808 ) ;
#49233 = STYLED_ITEM ( 'NONE', ( #61427 ), #13966 ) ;
#49232 = CARTESIAN_POINT ( 'NONE',  ( -195.0000000000000000, 0.000000000000000000, 0.000000000000000000 ) ) ;
#49234 = CARTESIAN_POINT ( 'NONE',  ( -139.5549999999999784, 0.000000000000000000, 8.024999999999991473 ) ) ;
#49235 =( NAMED_UNIT ( * ) SI_UNIT ( $, .STERADIAN. ) SOLID_ANGLE_UNIT ( ) );
#49236 = SURFACE_STYLE_FILL_AREA ( #65033 ) ;
#49237 = ORIENTED_EDGE ( 'NONE', *, *, #11505, .F. ) ;
#49238 = CARTESIAN_POINT ( 'NONE',  ( -70.75000000000000000, -3.000000000000000000, 19.00000000000000000 ) ) ;
#49239 = DIRECTION ( 'NONE',  ( 0.000000000000000000, 0.000000000000000000, 1.000000000000000000 ) ) ;
#49240 = CARTESIAN_POINT ( 'NONE',  ( 92.41620014002536720, 5.000000000000000000, 24.00402776293825369 ) ) ;
#49241 = VERTEX_POINT ( 'NONE', #5470 ) ;
#49242 = AXIS2_PLACEMENT_3D ( 'NONE', #15978, #31410, #31071 ) ;
#49243 = VERTEX_POINT ( 'NONE', #58627 ) ;
#49244 = CARTESIAN_POINT ( 'NONE',  ( -45.91547277936962246, 9.430195807687219656, 3.611004237778676185 ) ) ;
#49245 = DIRECTION ( 'NONE',  ( 0.000000000000000000, 0.000000000000000000, -1.000000000000000000 ) ) ;
#49246 = CARTESIAN_POINT ( 'NONE',  ( -53.90499999999997272, 2.607480562269068880, -8.024999999999993250 ) ) ;
#49247 = EDGE_LOOP ( 'NONE', ( #64731, #499, #20533 ) ) ;
#49248 = CARTESIAN_POINT ( 'NONE',  ( -60.49999999999998579, 50.00000000000000000, 7.500000000000000000 ) ) ;
#49249 = SURFACE_STYLE_USAGE ( .BOTH. , #27748 ) ;
#49250 = EDGE_CURVE ( 'NONE', #56578, #2488, #30841, .T. ) ;
#49251 = DIRECTION ( 'NONE',  ( -0.000000000000000000, 1.000000000000000000, -0.000000000000000000 ) ) ;
#49252 = DIRECTION ( 'NONE',  ( 0.000000000000000000, -1.000000000000000000, 3.469446951953611033E-15 ) ) ;
#49254 = EDGE_CURVE ( 'NONE', #19782, #737, #28717, .T. ) ;
#49253 = ORIENTED_EDGE ( 'NONE', *, *, #40628, .T. ) ;
#49255 = EDGE_CURVE ( 'NONE', #14021, #40860, #14138, .T. ) ;
#49257 = FACE_OUTER_BOUND ( 'NONE', #35821, .T. ) ;
#49256 = MECHANICAL_DESIGN_GEOMETRIC_PRESENTATION_REPRESENTATION (  '', ( #9941 ), #13323 ) ;
#49258 = DIRECTION ( 'NONE',  ( 1.300977106640434891E-16, 0.000000000000000000, 1.000000000000000000 ) ) ;
#49259 = DIRECTION ( 'NONE',  ( -1.000000000000000000, 0.000000000000000000, 0.000000000000000000 ) ) ;
#49260 = DIRECTION ( 'NONE',  ( 0.000000000000000000, 0.000000000000000000, 1.000000000000000000 ) ) ;
#49261 = EDGE_CURVE ( 'NONE', #39699, #15837, #10789, .T. ) ;
#49262 = EDGE_CURVE ( 'NONE', #61842, #62248, #63532, .T. ) ;
#49263 = CARTESIAN_POINT ( 'NONE',  ( -112.7949999999999733, 2.607480562269069324, -8.024999999999993250 ) ) ;
#49264 = CARTESIAN_POINT ( 'NONE',  ( 9.058813317711338797, 159.8449999999999989, -2.943386871421372675 ) ) ;
#49265 = CARTESIAN_POINT ( 'NONE',  ( -86.99499999999997613, -6.826472737025115478, 4.959722759717900331 ) ) ;
#49266 = EDGE_CURVE ( 'NONE', #39293, #33880, #65794, .T. ) ;
#49267 = AXIS2_PLACEMENT_3D ( 'NONE', #57413, #9239, #31711 ) ;
#49268 = CARTESIAN_POINT ( 'NONE',  ( -1.000000000000028644, 0.000000000000000000, 11.99999999999999645 ) ) ;
#49269 =( LENGTH_UNIT ( ) NAMED_UNIT ( * ) SI_UNIT ( .MILLI., .METRE. ) );
#49270 = DIRECTION ( 'NONE',  ( 0.000000000000000000, 0.000000000000000000, -1.000000000000000000 ) ) ;
#49271 = PRESENTATION_STYLE_ASSIGNMENT (( #33089 ) ) ;
#49272 = ORIENTED_EDGE ( 'NONE', *, *, #49196, .F. ) ;
#49273 = EDGE_CURVE ( 'NONE', #12300, #17330, #32234, .T. ) ;
#49274 = CARTESIAN_POINT ( 'NONE',  ( -127.3429263765337964, -9.058813317711329915, 2.943386871421371787 ) ) ;
#49275 = CARTESIAN_POINT ( 'NONE',  ( -142.9449999999999932, -9.827790563157499189E-16, -8.024999999999991473 ) ) ;
#49276 = FACE_OUTER_BOUND ( 'NONE', #21595, .T. ) ;
#49277 = STYLED_ITEM ( 'NONE', ( #2183 ), #66610 ) ;
#49278 = CARTESIAN_POINT ( 'NONE',  ( -48.74499999999998323, 4.716976649647094177, 6.492361379858945902 ) ) ;
#49279 = LINE ( 'NONE', #988, #28251 ) ;
#49280 = VERTEX_POINT ( 'NONE', #52667 ) ;
#49281 = VECTOR ( 'NONE', #2578, 1000.000000000000000 ) ;
#49282 = ORIENTED_EDGE ( 'NONE', *, *, #8673, .T. ) ;
#49283 = DIRECTION ( 'NONE',  ( 0.000000000000000000, 0.000000000000000000, -1.000000000000000000 ) ) ;
#49284 = CARTESIAN_POINT ( 'NONE',  ( 0.000000000000000000, 2.000000000000000444, 0.000000000000000000 ) ) ;
#49285 = CARTESIAN_POINT ( 'NONE',  ( -44.99999999999998579, 119.9999999999999716, 7.000000000000000000 ) ) ;
#49286 =( NAMED_UNIT ( * ) SI_UNIT ( $, .STERADIAN. ) SOLID_ANGLE_UNIT ( ) );
#49287 = CIRCLE ( 'NONE', #32381, 0.5000000000000004441 ) ;
#49288 = DIRECTION ( 'NONE',  ( 1.000000000000000000, 0.000000000000000000, 0.000000000000000000 ) ) ;
#49289 = CARTESIAN_POINT ( 'NONE',  ( 45.50000000000000000, 9.639620389971920389, 6.999999999999999112 ) ) ;
#49290 = VERTEX_POINT ( 'NONE', #58976 ) ;
#49291 = CARTESIAN_POINT ( 'NONE',  ( -144.8049999999999500, -8.437984349512086979, 5.166775262442717831E-16 ) ) ;
#49292 = VERTEX_POINT ( 'NONE', #48458 ) ;
#49293 = ORIENTED_EDGE ( 'NONE', *, *, #24758, .T. ) ;
#49294 = LINE ( 'NONE', #1004, #45908 ) ;
#49295 = EDGE_LOOP ( 'NONE', ( #29780, #29624, #59783, #21073 ) ) ;
#49296 = CARTESIAN_POINT ( 'NONE',  ( -0.4575609230677349926, 2.491211107078686648, -9.000000000000003553 ) ) ;
#49297 =( LENGTH_UNIT ( ) NAMED_UNIT ( * ) SI_UNIT ( .MILLI., .METRE. ) );
#49298 = CARTESIAN_POINT ( 'NONE',  ( 10.01517768586949231, 126.6949999999999932, 1.839758294383810543E-15 ) ) ;
#49299 =( LENGTH_UNIT ( ) NAMED_UNIT ( * ) SI_UNIT ( .MILLI., .METRE. ) );
#49300 = EDGE_CURVE ( 'NONE', #32584, #16622, #32421, .T. ) ;
#49301 = EDGE_LOOP ( 'NONE', ( #59045, #6676, #52337, #28139 ) ) ;
#49302 = DIRECTION ( 'NONE',  ( 0.000000000000000000, -1.000000000000000000, 0.000000000000000000 ) ) ;
#49303 = CARTESIAN_POINT ( 'NONE',  ( -5.598654528085808657, 129.7549999999999955, 7.705886871421373741 ) ) ;
#49304 = CARTESIAN_POINT ( 'NONE',  ( -57.35499999999998977, -4.716976649647093289, -6.492361379858945902 ) ) ;
#49305 = CIRCLE ( 'NONE', #18938, 0.5000000000000004441 ) ;
#49306 = CARTESIAN_POINT ( 'NONE',  ( -121.4949999999999761, 6.826472737025113702, -4.959722759717902107 ) ) ;
#49307 = DIRECTION ( 'NONE',  ( 0.000000000000000000, 0.000000000000000000, -1.000000000000000000 ) ) ;
#49308 = ORIENTED_EDGE ( 'NONE', *, *, #57582, .F. ) ;
#49309 = CARTESIAN_POINT ( 'NONE',  ( -8.102448949553181734, 156.6049999999999329, 5.886773742842747126 ) ) ;
#49310 = CARTESIAN_POINT ( 'NONE',  ( 35.99999999999999289, 0.000000000000000000, 24.00402776293825369 ) ) ;
#49311 = DIRECTION ( 'NONE',  ( -0.000000000000000000, -1.000000000000000000, -0.000000000000000000 ) ) ;
#49312 = AXIS2_PLACEMENT_3D ( 'NONE', #49327, #28167, #60896 ) ;
#49313 = CARTESIAN_POINT ( 'NONE',  ( -9.827790563157511022E-16, 142.4429263765338192, 8.025000000000000355 ) ) ;
#49314 = DIRECTION ( 'NONE',  ( 0.000000000000000000, 0.000000000000000000, 1.000000000000000000 ) ) ;
#49315 = LINE ( 'NONE', #59857, #34026 ) ;
#49316 = ORIENTED_EDGE ( 'NONE', *, *, #3357, .F. ) ;
#49317 = CARTESIAN_POINT ( 'NONE',  ( -33.85304738437685046, -9.497883372643979527, -3.722847864133452145 ) ) ;
#49318 = DIRECTION ( 'NONE',  ( -0.000000000000000000, -1.000000000000000000, 0.000000000000000000 ) ) ;
#49319 = CARTESIAN_POINT ( 'NONE',  ( -167.7549999999999955, 4.716976649647091513, -6.492361379858946790 ) ) ;
#49320 = VERTEX_POINT ( 'NONE', #21324 ) ;
#49321 = DIRECTION ( 'NONE',  ( -0.000000000000000000, -1.000000000000000000, -0.000000000000000000 ) ) ;
#49322 = PRESENTATION_LAYER_ASSIGNMENT (  '', '', ( #61627 ) ) ;
#49323 = PRESENTATION_STYLE_ASSIGNMENT (( #16975 ) ) ;
#49324 = CARTESIAN_POINT ( 'NONE',  ( -44.99154893936433552, 9.591540374752312914, 3.000000000000000000 ) ) ;
#49325 = VERTEX_POINT ( 'NONE', #26921 ) ;
#49326 = DIRECTION ( 'NONE',  ( 0.000000000000000000, 0.000000000000000000, 1.000000000000000000 ) ) ;
#49327 = CARTESIAN_POINT ( 'NONE',  ( -195.0000000000000000, 0.000000000000000000, 0.000000000000000000 ) ) ;
#49328 = CARTESIAN_POINT ( 'NONE',  ( -82.85499999999998977, 4.716976649647094177, 6.492361379858945902 ) ) ;
#49329 = ORIENTED_EDGE ( 'NONE', *, *, #38570, .T. ) ;
#49330 = EDGE_CURVE ( 'NONE', #65996, #31245, #60165, .T. ) ;
#49331 = DIRECTION ( 'NONE',  ( 1.000000000000000000, 0.000000000000000000, -0.000000000000000000 ) ) ;
#49332 = VECTOR ( 'NONE', #24469, 1000.000000000000000 ) ;
#49333 = SURFACE_STYLE_USAGE ( .BOTH. , #43066 ) ;
#49334 = CARTESIAN_POINT ( 'NONE',  ( -56.60707362346616378, -8.102448949553172852, 5.886773742842742685 ) ) ;
#49335 = AXIS2_PLACEMENT_3D ( 'NONE', #51158, #55730, #55009 ) ;
#49336 = EDGE_CURVE ( 'NONE', #32528, #4254, #64647, .T. ) ;
#49337 = CARTESIAN_POINT ( 'NONE',  ( -75.00000000000000000, 9.027119726910738606, -6.778758691516489243 ) ) ;
#49338 = ORIENTED_EDGE ( 'NONE', *, *, #45575, .F. ) ;
#49339 = CIRCLE ( 'NONE', #63921, 9.000000000000000000 ) ;
#49341 = FACE_OUTER_BOUND ( 'NONE', #39269, .T. ) ;
#49340 = PLANE ( 'NONE',  #23438 ) ;
#49342 = CARTESIAN_POINT ( 'NONE',  ( -103.2549999999999812, -4.716976649647092401, 6.492361379858946790 ) ) ;
#49343 = CARTESIAN_POINT ( 'NONE',  ( 8.102448949553181734, 132.3949999999999534, 5.886773742842750679 ) ) ;
#49344 = CARTESIAN_POINT ( 'NONE',  ( -117.1449999999999818, -4.716976649647092401, 6.492361379858946790 ) ) ;
#49345 = ADVANCED_FACE ( 'NONE', ( #68498 ), #25906, .F. ) ;
#49346 = SURFACE_STYLE_FILL_AREA ( #59528 ) ;
#49347 = CARTESIAN_POINT ( 'NONE',  ( -18.96980255412093896, 11.60735904872732149, -3.057087346036348130 ) ) ;
#49348 = VECTOR ( 'NONE', #1864, 1000.000000000000000 ) ;
#49349 = EDGE_CURVE ( 'NONE', #59451, #31383, #36530, .T. ) ;
#49350 = CARTESIAN_POINT ( 'NONE',  ( -153.1429263765338078, 5.598654528085800663, -7.705886871421367523 ) ) ;
#49351 =( LENGTH_UNIT ( ) NAMED_UNIT ( * ) SI_UNIT ( .MILLI., .METRE. ) );
#49352 = CARTESIAN_POINT ( 'NONE',  ( -172.6449999999999818, 4.716976649647091513, -6.492361379858946790 ) ) ;
#49353 = VECTOR ( 'NONE', #59957, 1000.000000000000000 ) ;
#49354 = CARTESIAN_POINT ( 'NONE',  ( -43.75000000000000000, 0.000000000000000000, 16.97056274847714974 ) ) ;
#49355 = CIRCLE ( 'NONE', #32505, 3.100000000000005418 ) ;
#49356 = STYLED_ITEM ( 'NONE', ( #24121 ), #10590 ) ;
#49357 = CARTESIAN_POINT ( 'NONE',  ( 15.98999599679679839, 146.4999999999999716, 9.500000000000000000 ) ) ;
#49358 = ORIENTED_EDGE ( 'NONE', *, *, #8077, .F. ) ;
#49359 = FACE_OUTER_BOUND ( 'NONE', #35988, .T. ) ;
#49360 = FACE_OUTER_BOUND ( 'NONE', #29554, .T. ) ;
#49361 = VERTEX_POINT ( 'NONE', #20651 ) ;
#49362 = CARTESIAN_POINT ( 'NONE',  ( -71.39292637653379359, 8.102448949553176405, 5.886773742842740909 ) ) ;
#49363 = CIRCLE ( 'NONE', #19006, 1.000000000000001110 ) ;
#49364 = CIRCLE ( 'NONE', #44922, 7.000000000000001776 ) ;
#49365 = FILL_AREA_STYLE ('',( #23647 ) ) ;
#49366 = CIRCLE ( 'NONE', #58340, 1.000000000000000888 ) ;
#49367 = CARTESIAN_POINT ( 'NONE',  ( 8.000000000000035527, 0.000000000000000000, 77.00402776293825013 ) ) ;
#49368 = FACE_OUTER_BOUND ( 'NONE', #21153, .T. ) ;
#49369 = LINE ( 'NONE', #33523, #39288 ) ;
#49370 = COLOUR_RGB ( '', 0.08235294, 0.09019608, 0.10196078) ;
#49371 = FACE_OUTER_BOUND ( 'NONE', #20991, .T. ) ;
#49372 = ORIENTED_EDGE ( 'NONE', *, *, #47130, .F. ) ;
#49373 = CARTESIAN_POINT ( 'NONE',  ( -171.9549999999999841, -7.632228543268599452, 2.479861379858951054 ) ) ;
#49374 = ORIENTED_EDGE ( 'NONE', *, *, #29870, .F. ) ;
#49375 =( LENGTH_UNIT ( ) NAMED_UNIT ( * ) SI_UNIT ( .MILLI., .METRE. ) );
#49376 = DIRECTION ( 'NONE',  ( -1.000000000000000000, 0.000000000000000000, 0.000000000000000000 ) ) ;
#49377 = CARTESIAN_POINT ( 'NONE',  ( -4.750000000000002665, 24.99999999999998579, -3.750000000000000000 ) ) ;
#49378 = CARTESIAN_POINT ( 'NONE',  ( 4.716976649647099507, 153.7570736234661695, -6.492361379858953008 ) ) ;
#49379 = VECTOR ( 'NONE', #64749, 1000.000000000000000 ) ;
#49380 = EDGE_CURVE ( 'NONE', #61113, #9855, #32030, .T. ) ;
#49381 = ORIENTED_EDGE ( 'NONE', *, *, #49116, .F. ) ;
#49382 = CARTESIAN_POINT ( 'NONE',  ( -86.45499999999998408, 7.632228543268599452, -2.479861379858951942 ) ) ;
#49383 = PRESENTATION_LAYER_ASSIGNMENT (  '', '', ( #56096 ) ) ;
#49384 = DIRECTION ( 'NONE',  ( -1.000000000000000000, -0.000000000000000000, -0.000000000000000000 ) ) ;
#49385 = CARTESIAN_POINT ( 'NONE',  ( -24.21231517720798010, 113.4999999999999858, -7.500000000000000000 ) ) ;
#49386 = CARTESIAN_POINT ( 'NONE',  ( -169.6429263765338078, -5.598654528085801552, 7.705886871421367523 ) ) ;
#49387 = CARTESIAN_POINT ( 'NONE',  ( -60.00000000000000000, -2.024042244987997205E-14, -10.00000000000000000 ) ) ;
#49388 = DIRECTION ( 'NONE',  ( 0.9704308468600219006, -0.2413793103448194921, -0.000000000000000000 ) ) ;
#49389 = ORIENTED_EDGE ( 'NONE', *, *, #43771, .F. ) ;
#49390 = DIRECTION ( 'NONE',  ( 0.000000000000000000, 0.000000000000000000, 1.000000000000000000 ) ) ;
#49391 =( NAMED_UNIT ( * ) SI_UNIT ( $, .STERADIAN. ) SOLID_ANGLE_UNIT ( ) );
#49392 = MECHANICAL_DESIGN_GEOMETRIC_PRESENTATION_REPRESENTATION (  '', ( #53727 ), #66242 ) ;
#49393 = CARTESIAN_POINT ( 'NONE',  ( -59.54499999999998749, -7.632228543268600340, -2.479861379858950166 ) ) ;
#49394 = ORIENTED_EDGE ( 'NONE', *, *, #46283, .F. ) ;
#49395 =( BOUNDED_CURVE ( )  B_SPLINE_CURVE ( 2, ( #16244, #57834, #38046, #41679, #48614, #36034, #53505, #41326, #5988, #3987, #68050 ),
 .UNSPECIFIED., .F., .F. ) 
 B_SPLINE_CURVE_WITH_KNOTS ( ( 3, 2, 2, 2, 2, 3 ),
 ( 0.1086956521739105841, 0.1108695652173887908, 0.1130434782608669975, 0.1152173913043452180, 0.1173913043478234247, 0.1195652173913016314 ),
 .UNSPECIFIED. ) 
 CURVE ( )  GEOMETRIC_REPRESENTATION_ITEM ( )  RATIONAL_B_SPLINE_CURVE ( ( 1.000000000000055289, 0.9510565162950983531, 1.000000000000000000, 0.9510565162951535312, 1.000000000000000000, 0.9510565162951535312, 1.000000000000000000, 0.9510565162951535312, 1.000000000000000000, 0.9510565162952148155, 0.9999999999999387157 ) ) 
 REPRESENTATION_ITEM ( '' )  );
#49396 = FILL_AREA_STYLE_COLOUR ( '', #51898 ) ;
#49397 = EDGE_CURVE ( 'NONE', #36469, #23874, #22581, .T. ) ;
#49398 = LINE ( 'NONE', #23339, #23346 ) ;
#49399 = CARTESIAN_POINT ( 'NONE',  ( -45.91547277936962246, 9.430195807687216103, -6.000000000000000000 ) ) ;
#49400 = AXIS2_PLACEMENT_3D ( 'NONE', #15885, #42991, #32722 ) ;
#49401 = ORIENTED_EDGE ( 'NONE', *, *, #18869, .F. ) ;
#49402 = SURFACE_SIDE_STYLE ('',( #16718 ) ) ;
#49403 = DIRECTION ( 'NONE',  ( 0.000000000000000000, 0.000000000000000000, -1.000000000000000000 ) ) ;
#49404 = VERTEX_POINT ( 'NONE', #43876 ) ;
#49405 =( GEOMETRIC_REPRESENTATION_CONTEXT ( 3 ) GLOBAL_UNCERTAINTY_ASSIGNED_CONTEXT ( ( #10205 ) ) GLOBAL_UNIT_ASSIGNED_CONTEXT ( ( #8244, #33910, #18778 ) ) REPRESENTATION_CONTEXT ( 'NONE', 'WORKASPACE' ) );
#49406 = ADVANCED_FACE ( 'NONE', ( #49818 ), #11116, .T. ) ;
#49407 = CARTESIAN_POINT ( 'NONE',  ( 7.750000000000002665, 31.24999999999998579, 4.000000000000000000 ) ) ;
#49408 = CARTESIAN_POINT ( 'NONE',  ( -74.21332857261049298, 8.935426707107593458, 6.369485321263598010 ) ) ;
#49409 = CARTESIAN_POINT ( 'NONE',  ( -113.0049999999999812, 6.826472737025116366, 4.959722759717898555 ) ) ;
#49410 = ORIENTED_EDGE ( 'NONE', *, *, #8369, .F. ) ;
#49411 = ADVANCED_FACE ( 'NONE', ( #55061 ), #59653, .T. ) ;
#49412 = CARTESIAN_POINT ( 'NONE',  ( -22.25000000000000711, 34.24999999999999289, -4.000000000000000000 ) ) ;
#49413 = SURFACE_STYLE_FILL_AREA ( #6469 ) ;
#49414 = TOROIDAL_SURFACE ( 'NONE', #4419, 3.499999999999998668, 1.000000000000000000 ) ;
#49415 = SURFACE_STYLE_USAGE ( .BOTH. , #66623 ) ;
#49416 =( LENGTH_UNIT ( ) NAMED_UNIT ( * ) SI_UNIT ( .MILLI., .METRE. ) );
#49417 = AXIS2_PLACEMENT_3D ( 'NONE', #29305, #8226, #39917 ) ;
#49418 = CARTESIAN_POINT ( 'NONE',  ( -154.2570736234661979, 5.598654528085800663, -7.705886871421367523 ) ) ;
#49419 = CARTESIAN_POINT ( 'NONE',  ( 0.000000000000000000, 130.4449999999999648, -9.525000000000000355 ) ) ;
#49420 = CARTESIAN_POINT ( 'NONE',  ( -90.20707362346618652, 3.094860106618433360, 9.524999999999991473 ) ) ;
#49421 = ADVANCED_FACE ( 'NONE', ( #11471 ), #5833, .T. ) ;
#49422 = STYLED_ITEM ( 'NONE', ( #41646 ), #41802 ) ;
#49423 = CARTESIAN_POINT ( 'NONE',  ( 74.99999999999998579, 50.00000000000000000, -9.500000000000000000 ) ) ;
#49424 = VERTEX_POINT ( 'NONE', #836 ) ;
#49425 = VECTOR ( 'NONE', #37286, 1000.000000000000000 ) ;
#49426 = EDGE_CURVE ( 'NONE', #60408, #13725, #8520, .T. ) ;
#49428 =( NAMED_UNIT ( * ) PLANE_ANGLE_UNIT ( ) SI_UNIT ( $, .RADIAN. ) );
#49427 = SURFACE_STYLE_USAGE ( .BOTH. , #59246 ) ;
#49429 = CARTESIAN_POINT ( 'NONE',  ( -133.1050000000000182, -6.826472737025115478, 4.959722759717900331 ) ) ;
#49430 =( NAMED_UNIT ( * ) PLANE_ANGLE_UNIT ( ) SI_UNIT ( $, .RADIAN. ) );
#49431 = DIRECTION ( 'NONE',  ( -1.000000000000000000, 0.000000000000000000, 0.000000000000000000 ) ) ;
#49432 = DIRECTION ( 'NONE',  ( 0.000000000000000000, 1.000000000000000000, 0.000000000000000000 ) ) ;
#49433 = CARTESIAN_POINT ( 'NONE',  ( -145.1949999999999648, 8.437984349512085203, -1.550032578732815448E-15 ) ) ;
#49434 = ADVANCED_FACE ( 'NONE', ( #12497 ), #33961, .F. ) ;
#49435 = CARTESIAN_POINT ( 'NONE',  ( -124.9450000000000074, -9.827790563157499189E-16, -8.024999999999991473 ) ) ;
#49436 = ORIENTED_EDGE ( 'NONE', *, *, #63219, .F. ) ;
#49437 = LINE ( 'NONE', #1158, #52145 ) ;
#49438 = AXIS2_PLACEMENT_3D ( 'NONE', #656, #37724, #48256 ) ;
#49439 = CARTESIAN_POINT ( 'NONE',  ( 44.40987964080542838, 10.30029937056526990, -3.500456542365120605 ) ) ;
#49440 = STYLED_ITEM ( 'NONE', ( #28552 ), #53933 ) ;
#49441 = DIRECTION ( 'NONE',  ( 1.000000000000000000, 0.000000000000000000, 0.000000000000000000 ) ) ;
#49442 = UNCERTAINTY_MEASURE_WITH_UNIT (LENGTH_MEASURE( 1.000000000000000082E-05 ), #20447, 'distance_accuracy_value', 'NONE');
#49443 = EDGE_CURVE ( 'NONE', #45750, #7911, #2651, .T. ) ;
#49444 = CARTESIAN_POINT ( 'NONE',  ( -180.1429263765338078, 5.598654528085800663, -7.705886871421367523 ) ) ;
#49445 = SURFACE_SIDE_STYLE ('',( #6856 ) ) ;
#49446 = AXIS2_PLACEMENT_3D ( 'NONE', #7383, #39419, #39767 ) ;
#49447 = CARTESIAN_POINT ( 'NONE',  ( -54.89499999999997470, 6.826472737025116366, 4.959722759717898555 ) ) ;
#49448 = DIRECTION ( 'NONE',  ( -1.000000000000000000, 0.000000000000000000, 0.000000000000000000 ) ) ;
#49449 = DIRECTION ( 'NONE',  ( 1.000000000000000000, 0.000000000000000000, 0.000000000000000000 ) ) ;
#49450 = DIRECTION ( 'NONE',  ( 0.000000000000000000, -1.000000000000000000, 0.000000000000000000 ) ) ;
#49451 = FACE_OUTER_BOUND ( 'NONE', #12750, .T. ) ;
#49452 = CARTESIAN_POINT ( 'NONE',  ( -94.04292637653379927, -9.058813317711329915, -2.943386871421370898 ) ) ;
#49453 = DIRECTION ( 'NONE',  ( 0.000000000000000000, -1.000000000000000000, 0.000000000000000000 ) ) ;
#49454 = CARTESIAN_POINT ( 'NONE',  ( 13.50000000000000355, 28.24999999999998934, 4.000000000000000000 ) ) ;
#49455 = FILL_AREA_STYLE ('',( #27946 ) ) ;
#49456 = DIRECTION ( 'NONE',  ( 0.000000000000000000, 1.000000000000000000, 0.000000000000000000 ) ) ;
#49457 = ORIENTED_EDGE ( 'NONE', *, *, #29706, .F. ) ;
#49458 = CARTESIAN_POINT ( 'NONE',  ( -41.49999999999997868, 10.49999999999998046, -3.500000000000000000 ) ) ;
#49459 = AXIS2_PLACEMENT_3D ( 'NONE', #62916, #31607, #4877 ) ;
#49460 = PRESENTATION_LAYER_ASSIGNMENT (  '', '', ( #64050 ) ) ;
#49461 = VERTEX_POINT ( 'NONE', #60344 ) ;
#49462 = MECHANICAL_DESIGN_GEOMETRIC_PRESENTATION_REPRESENTATION (  '', ( #32609 ), #9037 ) ;
#49463 = CARTESIAN_POINT ( 'NONE',  ( -8.437984349512095861, 121.8070736234661666, -5.166775262442723748E-16 ) ) ;
#49465 = CIRCLE ( 'NONE', #19104, 9.000000000000000000 ) ;
#49464 = CARTESIAN_POINT ( 'NONE',  ( 34.99999999999992895, 110.4999999999999858, -9.500000000000000000 ) ) ;
#49466 = CARTESIAN_POINT ( 'NONE',  ( 74.59716837049624871, 19.66257108179103241, -6.399833413891735212 ) ) ;
#49467 = VERTEX_POINT ( 'NONE', #12150 ) ;
#49468 = ORIENTED_EDGE ( 'NONE', *, *, #26195, .T. ) ;
#49469 = CARTESIAN_POINT ( 'NONE',  ( -5.705565085145811288, -2.472216779103303175, -4.117671386636410524 ) ) ;
#49470 =( NAMED_UNIT ( * ) SI_UNIT ( $, .STERADIAN. ) SOLID_ANGLE_UNIT ( ) );
#49471 = ORIENTED_EDGE ( 'NONE', *, *, #7322, .T. ) ;
#49472 = CARTESIAN_POINT ( 'NONE',  ( -24.00000000000000000, 0.000000000000000000, -3.000000000000000000 ) ) ;
#49473 = CARTESIAN_POINT ( 'NONE',  ( 25.75000000000001066, 21.74999999999998224, 3.750000000000000000 ) ) ;
#49474 = STYLED_ITEM ( 'NONE', ( #16165 ), #17652 ) ;
#49475 = AXIS2_PLACEMENT_3D ( 'NONE', #29150, #41155, #62555 ) ;
#49476 = CARTESIAN_POINT ( 'NONE',  ( 9.250000000000003553, 27.74999999999998934, 3.750000000000000000 ) ) ;
#49477 = CARTESIAN_POINT ( 'NONE',  ( -88.19499999999996476, 8.437984349512085203, -1.550032578732815448E-15 ) ) ;
#49478 = EDGE_LOOP ( 'NONE', ( #16343, #9000, #14675, #53600 ) ) ;
#49479 = AXIS2_PLACEMENT_3D ( 'NONE', #8079, #62229, #19669 ) ;
#49480 = CARTESIAN_POINT ( 'NONE',  ( -4.716976649647098618, 124.1429263765338220, 6.492361379858953008 ) ) ;
#49481 = EDGE_CURVE ( 'NONE', #45878, #34731, #7927, .T. ) ;
#49482 = CARTESIAN_POINT ( 'NONE',  ( 0.000000000000000000, 2.500000000000000000, 0.000000000000000000 ) ) ;
#49483 = FACE_OUTER_BOUND ( 'NONE', #31982, .T. ) ;
#49484 = UNCERTAINTY_MEASURE_WITH_UNIT (LENGTH_MEASURE( 1.000000000000000082E-05 ), #14337, 'distance_accuracy_value', 'NONE');
#49485 = ORIENTED_EDGE ( 'NONE', *, *, #60110, .F. ) ;
#49486 = DIRECTION ( 'NONE',  ( 0.000000000000000000, 0.000000000000000000, -1.000000000000000000 ) ) ;
#49487 =( NAMED_UNIT ( * ) PLANE_ANGLE_UNIT ( ) SI_UNIT ( $, .RADIAN. ) );
#49488 = AXIS2_PLACEMENT_3D ( 'NONE', #50557, #12548, #2280 ) ;
#49489 = EDGE_CURVE ( 'NONE', #43509, #55165, #48710, .T. ) ;
#49490 = EDGE_CURVE ( 'NONE', #33880, #60416, #2605, .T. ) ;
#49491 = VERTEX_POINT ( 'NONE', #30067 ) ;
#49492 = SURFACE_STYLE_USAGE ( .BOTH. , #38968 ) ;
#49493 = VERTEX_POINT ( 'NONE', #55775 ) ;
#49494 = CARTESIAN_POINT ( 'NONE',  ( 25.00000000000001421, 43.00000000000000000, 0.000000000000000000 ) ) ;
#49495 = DIRECTION ( 'NONE',  ( 0.000000000000000000, 0.000000000000000000, 1.000000000000000000 ) ) ;
#49496 = DIRECTION ( 'NONE',  ( -0.000000000000000000, -1.000000000000000000, -0.000000000000000000 ) ) ;
#49497 = DIRECTION ( 'NONE',  ( 0.000000000000000000, 0.000000000000000000, -1.000000000000000000 ) ) ;
#49498 = FACE_OUTER_BOUND ( 'NONE', #32727, .T. ) ;
#49499 =( BOUNDED_CURVE ( )  B_SPLINE_CURVE ( 2, ( #20190, #62057, #13888, #24765, #24094, #50833, #46647, #30378, #51882, #19851, #41345 ),
 .UNSPECIFIED., .F., .F. ) 
 B_SPLINE_CURVE_WITH_KNOTS ( ( 3, 2, 2, 2, 2, 3 ),
 ( 0.1847826086956478042, 0.1869565217391260248, 0.1891304347826042176, 0.1913043478260824382, 0.1934782608695606310, 0.1956521739130388515 ),
 .UNSPECIFIED. ) 
 CURVE ( )  GEOMETRIC_REPRESENTATION_ITEM ( )  RATIONAL_B_SPLINE_CURVE ( ( 1.000000000000097922, 0.9510565162950552764, 1.000000000000000000, 0.9510565162951535312, 1.000000000000000000, 0.9510565162951535312, 1.000000000000000000, 0.9510565162951535312, 1.000000000000000000, 0.9510565162952578921, 0.9999999999998956390 ) ) 
 REPRESENTATION_ITEM ( '' )  );
#49500 = MECHANICAL_DESIGN_GEOMETRIC_PRESENTATION_REPRESENTATION (  '', ( #4586 ), #59617 ) ;
#49501 = CARTESIAN_POINT ( 'NONE',  ( -68.39292637653379359, 8.102448949553176405, 5.886773742842740909 ) ) ;
#49502 = AXIS2_PLACEMENT_3D ( 'NONE', #62634, #3158, #61582 ) ;
#49503 = CARTESIAN_POINT ( 'NONE',  ( -23.21231517720797655, 117.9999999999999716, 7.000000000000000000 ) ) ;
#49504 = VERTEX_POINT ( 'NONE', #40663 ) ;
#49505 = DIRECTION ( 'NONE',  ( 0.2413793103448194644, 0.9704308468600220117, 0.000000000000000000 ) ) ;
#49506 = CARTESIAN_POINT ( 'NONE',  ( 61.99999999999998579, 31.24999999999999289, 3.750000000000000000 ) ) ;
#49507 = EDGE_CURVE ( 'NONE', #54282, #10026, #24109, .T. ) ;
#49508 =( NAMED_UNIT ( * ) SI_UNIT ( $, .STERADIAN. ) SOLID_ANGLE_UNIT ( ) );
#49509 = SURFACE_STYLE_FILL_AREA ( #53404 ) ;
#49510 = ORIENTED_EDGE ( 'NONE', *, *, #7843, .F. ) ;
#49511 = CARTESIAN_POINT ( 'NONE',  ( -157.8549999999999898, 4.716976649647094177, 6.492361379858945902 ) ) ;
#49512 = DIRECTION ( 'NONE',  ( 1.000000000000000000, 0.000000000000000000, 0.000000000000000000 ) ) ;
#49513 = SURFACE_SIDE_STYLE ('',( #28003 ) ) ;
#49514 = AXIS2_PLACEMENT_3D ( 'NONE', #59904, #18038, #12055 ) ;
#49515 = CARTESIAN_POINT ( 'NONE',  ( -173.2449999999999761, -4.716976649647093289, -6.492361379858945902 ) ) ;
#49516 = AXIS2_PLACEMENT_3D ( 'NONE', #14731, #47113, #36205 ) ;
#49517 = CARTESIAN_POINT ( 'NONE',  ( -156.8950000000000387, 6.826472737025115478, 4.959722759717899443 ) ) ;
#49518 = ORIENTED_EDGE ( 'NONE', *, *, #43269, .T. ) ;
#49519 = AXIS2_PLACEMENT_3D ( 'NONE', #42, #36427, #59187 ) ;
#49520 = SURFACE_SIDE_STYLE ('',( #59338 ) ) ;
#49521 = CARTESIAN_POINT ( 'NONE',  ( 44.82448674805887379, 10.57670410873373079, 3.609649266065623863 ) ) ;
#49522 = PLANE ( 'NONE',  #67570 ) ;
#49523 = CARTESIAN_POINT ( 'NONE',  ( -71.00499999999996703, 6.826472737025116366, 4.959722759717898555 ) ) ;
#49524 = CARTESIAN_POINT ( 'NONE',  ( -35.83032615006315780, -11.56233257873206810, 3.252572872672070847 ) ) ;
#49525 = CYLINDRICAL_SURFACE ( 'NONE', #14676, 0.2500000000000002220 ) ;
#49526 = CARTESIAN_POINT ( 'NONE',  ( -69.14499999999998181, -4.716976649647092401, 6.492361379858946790 ) ) ;
#49527 = CARTESIAN_POINT ( 'NONE',  ( 5.598654528085805993, 133.3549999999999898, 7.705886871421374629 ) ) ;
#49528 = ADVANCED_FACE ( 'NONE', ( #35718 ), #8637, .F. ) ;
#49529 = CARTESIAN_POINT ( 'NONE',  ( -9.827790563157511022E-16, 127.4429263765338192, 8.025000000000000355 ) ) ;
#49530 = CARTESIAN_POINT ( 'NONE',  ( 0.7252983342190405525, 154.1754443422797465, 9.200444342279759269 ) ) ;
#49531 = ADVANCED_FACE ( 'NONE', ( #62073 ), #39981, .T. ) ;
#49532 = UNCERTAINTY_MEASURE_WITH_UNIT (LENGTH_MEASURE( 1.000000000000000082E-05 ), #22071, 'distance_accuracy_value', 'NONE');
#49533 = AXIS2_PLACEMENT_3D ( 'NONE', #41419, #45994, #56514 ) ;
#49534 = AXIS2_PLACEMENT_3D ( 'NONE', #21303, #16074, #16433 ) ;
#49535 = SURFACE_SIDE_STYLE ('',( #28024 ) ) ;
#49536 = VERTEX_POINT ( 'NONE', #66318 ) ;
#49537 = FACE_OUTER_BOUND ( 'NONE', #66896, .T. ) ;
#49538 = CYLINDRICAL_SURFACE ( 'NONE', #13906, 9.524999999999991473 ) ;
#49539 = ORIENTED_EDGE ( 'NONE', *, *, #21849, .T. ) ;
#49540 = ORIENTED_EDGE ( 'NONE', *, *, #56710, .F. ) ;
#49541 = DIRECTION ( 'NONE',  ( 1.000000000000000000, 0.000000000000000000, 0.000000000000000000 ) ) ;
#49542 = MECHANICAL_DESIGN_GEOMETRIC_PRESENTATION_REPRESENTATION (  '', ( #2255 ), #51806 ) ;
#49543 = VECTOR ( 'NONE', #58805, 1000.000000000000000 ) ;
#49544 = MECHANICAL_DESIGN_GEOMETRIC_PRESENTATION_REPRESENTATION (  '', ( #52917 ), #18111 ) ;
#49545 = SURFACE_STYLE_FILL_AREA ( #34041 ) ;
#49546 =( NAMED_UNIT ( * ) SI_UNIT ( $, .STERADIAN. ) SOLID_ANGLE_UNIT ( ) );
#49547 = ORIENTED_EDGE ( 'NONE', *, *, #50456, .F. ) ;
#49548 = CIRCLE ( 'NONE', #9136, 0.9999999999999987788 ) ;
#49549 = CARTESIAN_POINT ( 'NONE',  ( -115.4049999999999727, -2.607480562269069768, 8.024999999999991473 ) ) ;
#49550 = ORIENTED_EDGE ( 'NONE', *, *, #43501, .T. ) ;
#49551 = PRESENTATION_STYLE_ASSIGNMENT (( #33364 ) ) ;
#49552 = ORIENTED_EDGE ( 'NONE', *, *, #63585, .F. ) ;
#49553 = DIRECTION ( 'NONE',  ( 1.000000000000000000, 0.000000000000000000, 0.000000000000000000 ) ) ;
#49554 = DIRECTION ( 'NONE',  ( -1.000000000000000000, 0.000000000000000000, 0.000000000000000000 ) ) ;
#49555 = VERTEX_POINT ( 'NONE', #46301 ) ;
#49556 = EDGE_CURVE ( 'NONE', #51168, #5580, #16371, .T. ) ;
#49557 = AXIS2_PLACEMENT_3D ( 'NONE', #22194, #6692, #65802 ) ;
#49558 = SPHERICAL_SURFACE ( 'NONE', #29857, 7.500000000000000000 ) ;
#49559 = FACE_OUTER_BOUND ( 'NONE', #8189, .T. ) ;
#49560 = DIRECTION ( 'NONE',  ( 1.000000000000000000, -0.000000000000000000, 0.000000000000000000 ) ) ;
#49561 = ORIENTED_EDGE ( 'NONE', *, *, #2193, .F. ) ;
#49562 = ORIENTED_EDGE ( 'NONE', *, *, #28578, .F. ) ;
#49563 = CARTESIAN_POINT ( 'NONE',  ( -5.735626173591136023, 110.4999999999999858, -7.617005373172553995 ) ) ;
#49564 = DIRECTION ( 'NONE',  ( 0.000000000000000000, 0.000000000000000000, -1.000000000000000000 ) ) ;
#49565 = CARTESIAN_POINT ( 'NONE',  ( 44.99999999999999289, 10.69371294336139400, 3.707106781186544353 ) ) ;
#49566 = ORIENTED_EDGE ( 'NONE', *, *, #63256, .F. ) ;
#49567 = CARTESIAN_POINT ( 'NONE',  ( 8.437984349512095861, 134.1929263765338192, 1.550032578732817026E-15 ) ) ;
#49568 = DIRECTION ( 'NONE',  ( 0.000000000000000000, -1.000000000000000000, 0.000000000000000000 ) ) ;
#49569 = CARTESIAN_POINT ( 'NONE',  ( 17.00000000000000711, 27.74999999999998224, 3.750000000000000000 ) ) ;
#49570 =( GEOMETRIC_REPRESENTATION_CONTEXT ( 3 ) GLOBAL_UNCERTAINTY_ASSIGNED_CONTEXT ( ( #27079 ) ) GLOBAL_UNIT_ASSIGNED_CONTEXT ( ( #36697, #58114, #36339 ) ) REPRESENTATION_CONTEXT ( 'NONE', 'WORKASPACE' ) );
#49571 = CARTESIAN_POINT ( 'NONE',  ( -9.827790563157511022E-16, 124.4429263765338192, 8.025000000000000355 ) ) ;
#49572 = ADVANCED_FACE ( 'NONE', ( #45259 ), #66681, .T. ) ;
#49573 = DIRECTION ( 'NONE',  ( 0.000000000000000000, 0.000000000000000000, 1.000000000000000000 ) ) ;
#49574 = EDGE_LOOP ( 'NONE', ( #38250, #13260 ) ) ;
#49575 = PRESENTATION_LAYER_ASSIGNMENT (  '', '', ( #10263 ) ) ;
#49576 = PRESENTATION_STYLE_ASSIGNMENT (( #61149 ) ) ;
#49577 = EDGE_LOOP ( 'NONE', ( #5701, #3045, #4371, #24125 ) ) ;
#49578 = SURFACE_SIDE_STYLE ('',( #65738 ) ) ;
#49579 = LINE ( 'NONE', #43638, #69361 ) ;
#49580 = SURFACE_SIDE_STYLE ('',( #33718 ) ) ;
#49581 = CARTESIAN_POINT ( 'NONE',  ( -140.9050000000000011, 2.607480562269068880, -8.024999999999993250 ) ) ;
#49582 = CARTESIAN_POINT ( 'NONE',  ( -74.50000000000000000, -2.220952357103124925E-14, 6.999999999999999112 ) ) ;
#49583 = DIRECTION ( 'NONE',  ( -0.000000000000000000, 0.000000000000000000, -1.000000000000000000 ) ) ;
#49584 = UNCERTAINTY_MEASURE_WITH_UNIT (LENGTH_MEASURE( 1.000000000000000082E-05 ), #36125, 'distance_accuracy_value', 'NONE');
#49585 = ORIENTED_EDGE ( 'NONE', *, *, #23428, .F. ) ;
#49586 = AXIS2_PLACEMENT_3D ( 'NONE', #65174, #12390, #17711 ) ;
#49587 = AXIS2_PLACEMENT_3D ( 'NONE', #21659, #53345, #64586 ) ;
#49588 = DIRECTION ( 'NONE',  ( -1.000000000000000000, 0.000000000000000000, 1.982541115402069054E-16 ) ) ;
#49589 = FACE_OUTER_BOUND ( 'NONE', #62277, .T. ) ;
#49590 = CARTESIAN_POINT ( 'NONE',  ( -45.00000000000000000, 9.708372675170616972, -6.100915009778865361 ) ) ;
#49591 = ORIENTED_EDGE ( 'NONE', *, *, #45312, .T. ) ;
#49592 = VECTOR ( 'NONE', #46869, 1000.000000000000000 ) ;
#49593 = VERTEX_POINT ( 'NONE', #35008 ) ;
#49594 = DIRECTION ( 'NONE',  ( 0.000000000000000000, 0.000000000000000000, -1.000000000000000000 ) ) ;
#49595 = EDGE_CURVE ( 'NONE', #21468, #67711, #26473, .T. ) ;
#49596 = CARTESIAN_POINT ( 'NONE',  ( -61.25499999999998835, -4.716976649647092401, 6.492361379858946790 ) ) ;
#49597 = ORIENTED_EDGE ( 'NONE', *, *, #50203, .F. ) ;
#49598 = CARTESIAN_POINT ( 'NONE',  ( 21.02379604162863913, 110.4999999999999858, -10.50000000000000000 ) ) ;
#49599 =( LENGTH_UNIT ( ) NAMED_UNIT ( * ) SI_UNIT ( .MILLI., .METRE. ) );
#49600 =( GEOMETRIC_REPRESENTATION_CONTEXT ( 3 ) GLOBAL_UNCERTAINTY_ASSIGNED_CONTEXT ( ( #3805 ) ) GLOBAL_UNIT_ASSIGNED_CONTEXT ( ( #63707, #15554, #67976 ) ) REPRESENTATION_CONTEXT ( 'NONE', 'WORKASPACE' ) );
#49601 = DIRECTION ( 'NONE',  ( 1.224646799147353207E-16, 1.000000000000000000, -0.000000000000000000 ) ) ;
#49602 = EDGE_LOOP ( 'NONE', ( #37451, #35139, #31729, #4445 ) ) ;
#49603 = VECTOR ( 'NONE', #44232, 1000.000000000000000 ) ;
#49604 = AXIS2_PLACEMENT_3D ( 'NONE', #12193, #41061, #18857 ) ;
#49605 = DIRECTION ( 'NONE',  ( -0.000000000000000000, -1.000000000000000000, -0.000000000000000000 ) ) ;
#49606 = FILL_AREA_STYLE ('',( #54515 ) ) ;
#49607 = SURFACE_SIDE_STYLE ('',( #59800 ) ) ;
#49608 = AXIS2_PLACEMENT_3D ( 'NONE', #15970, #42031, #15282 ) ;
#49609 = CARTESIAN_POINT ( 'NONE',  ( -108.1449999999999960, -4.716976649647092401, 6.492361379858946790 ) ) ;
#49610 = CARTESIAN_POINT ( 'NONE',  ( 3.094860106618435136, 160.2949999999999875, -9.525000000000000355 ) ) ;
#49611 = CARTESIAN_POINT ( 'NONE',  ( -76.19499999999999318, 8.437984349512085203, -1.550032578732815448E-15 ) ) ;
#49612 = MECHANICAL_DESIGN_GEOMETRIC_PRESENTATION_REPRESENTATION (  '', ( #64201 ), #51870 ) ;
#49613 = DIRECTION ( 'NONE',  ( -7.709882115452441682E-16, -1.000000000000000000, 0.000000000000000000 ) ) ;
#49614 = VECTOR ( 'NONE', #41013, 1000.000000000000000 ) ;
#49615 = CARTESIAN_POINT ( 'NONE',  ( 39.74999999999999289, 18.74999999999997868, 4.000000000000000000 ) ) ;
#49616 = UNCERTAINTY_MEASURE_WITH_UNIT (LENGTH_MEASURE( 1.000000000000000082E-05 ), #37311, 'distance_accuracy_value', 'NONE');
#49617 = VECTOR ( 'NONE', #62748, 1000.000000000000000 ) ;
#49618 = FILL_AREA_STYLE ('',( #34113 ) ) ;
#49619 = ORIENTED_EDGE ( 'NONE', *, *, #10104, .T. ) ;
#49620 = CARTESIAN_POINT ( 'NONE',  ( -124.0429263765337993, -9.058813317711329915, -2.943386871421370898 ) ) ;
#49621 = CARTESIAN_POINT ( 'NONE',  ( -136.0449999999999875, 7.632228543268600340, 2.479861379858949277 ) ) ;
#49623 = CYLINDRICAL_SURFACE ( 'NONE', #67337, 5.000000000000004441 ) ;
#49622 = AXIS2_PLACEMENT_3D ( 'NONE', #64497, #20540, #16342 ) ;
#49624 = AXIS2_PLACEMENT_3D ( 'NONE', #29588, #66539, #40522 ) ;
#49625 = CARTESIAN_POINT ( 'NONE',  ( -67.40707362346614673, 3.094860106618428031, -9.524999999999993250 ) ) ;
#49626 = FACE_OUTER_BOUND ( 'NONE', #15259, .T. ) ;
#49627 = ORIENTED_EDGE ( 'NONE', *, *, #48565, .T. ) ;
#49628 = ORIENTED_EDGE ( 'NONE', *, *, #35040, .F. ) ;
#49629 = CARTESIAN_POINT ( 'NONE',  ( 98.00000000000000000, 16.00000000000000000, 5.000000000000004441 ) ) ;
#49630 = DIRECTION ( 'NONE',  ( -1.000000000000000000, 0.000000000000000000, 0.000000000000000000 ) ) ;
#49631 = DIRECTION ( 'NONE',  ( 0.000000000000000000, 0.000000000000000000, -1.000000000000000000 ) ) ;
#49632 = CARTESIAN_POINT ( 'NONE',  ( -49.85707362346617089, -5.598654528085803328, -7.705886871421366635 ) ) ;
#49633 = LINE ( 'NONE', #11983, #67951 ) ;
#49634 = EDGE_LOOP ( 'NONE', ( #60461, #34745, #32784, #39781 ) ) ;
#49635 = CARTESIAN_POINT ( 'NONE',  ( -143.9050000000000011, 2.607480562269069324, -8.024999999999993250 ) ) ;
#49636 = VERTEX_POINT ( 'NONE', #37137 ) ;
#49637 = ORIENTED_EDGE ( 'NONE', *, *, #2293, .F. ) ;
#49638 = PRESENTATION_STYLE_ASSIGNMENT (( #60858 ) ) ;
#49639 = FACE_OUTER_BOUND ( 'NONE', #44955, .T. ) ;
#49640 = ORIENTED_EDGE ( 'NONE', *, *, #12094, .F. ) ;
#49641 = EDGE_CURVE ( 'NONE', #42412, #24967, #66914, .T. ) ;
#49642 = AXIS2_PLACEMENT_3D ( 'NONE', #29533, #51003, #2768 ) ;
#49643 = CARTESIAN_POINT ( 'NONE',  ( 82.09357085539578236, 0.000000000000000000, 32.00402776293825724 ) ) ;
#49644 = CARTESIAN_POINT ( 'NONE',  ( -1.166476076187854022E-15, 125.9449999999999790, 9.525000000000000355 ) ) ;
#49645 = CYLINDRICAL_SURFACE ( 'NONE', #47546, 0.5000000000000004441 ) ;
#49646 = EDGE_LOOP ( 'NONE', ( #41963, #34051, #5843, #63557 ) ) ;
#49647 = CYLINDRICAL_SURFACE ( 'NONE', #29626, 0.5000000000000004441 ) ;
#49648 = CARTESIAN_POINT ( 'NONE',  ( -8.102448949553179958, 126.0049999999999812, -5.886773742842749790 ) ) ;
#49649 = AXIS2_PLACEMENT_3D ( 'NONE', #46630, #19834, #48253 ) ;
#49650 = CARTESIAN_POINT ( 'NONE',  ( -59.45499999999997698, 7.632228543268599452, -2.479861379858951942 ) ) ;
#49651 = ORIENTED_EDGE ( 'NONE', *, *, #49507, .T. ) ;
#49652 = CARTESIAN_POINT ( 'NONE',  ( -9.058813317711337021, 153.1549999999999727, -2.943386871421374895 ) ) ;
#49653 = DIRECTION ( 'NONE',  ( 1.000000000000000000, -0.000000000000000000, -0.000000000000000000 ) ) ;
#49654 = UNCERTAINTY_MEASURE_WITH_UNIT (LENGTH_MEASURE( 1.000000000000000082E-05 ), #46465, 'distance_accuracy_value', 'NONE');
#49655 = AXIS2_PLACEMENT_3D ( 'NONE', #67809, #14329, #9070 ) ;
#49656 = EDGE_CURVE ( 'NONE', #19259, #45832, #31104, .T. ) ;
#49657 = AXIS2_PLACEMENT_3D ( 'NONE', #16658, #38126, #6750 ) ;
#49658 = SURFACE_STYLE_USAGE ( .BOTH. , #28515 ) ;
#49659 = EDGE_CURVE ( 'NONE', #42163, #6374, #45605, .T. ) ;
#49660 = ORIENTED_EDGE ( 'NONE', *, *, #29654, .F. ) ;
#49661 = VECTOR ( 'NONE', #67434, 1000.000000000000000 ) ;
#49662 = EDGE_CURVE ( 'NONE', #51850, #63169, #55512, .T. ) ;
#49663 = ORIENTED_EDGE ( 'NONE', *, *, #63786, .T. ) ;
#49664 = CARTESIAN_POINT ( 'NONE',  ( -33.39017047773998570, -9.443833522994566465, -2.300020890958864861 ) ) ;
#49665 = SURFACE_STYLE_USAGE ( .BOTH. , #64793 ) ;
#49666 = CARTESIAN_POINT ( 'NONE',  ( -171.3550000000000182, -4.716976649647093289, -6.492361379858945902 ) ) ;
#49669 = ORIENTED_EDGE ( 'NONE', *, *, #5658, .F. ) ;
#49668 = EDGE_CURVE ( 'NONE', #7860, #29261, #18603, .T. ) ;
#49667 = VECTOR ( 'NONE', #3201, 1000.000000000000000 ) ;
#49670 = DIRECTION ( 'NONE',  ( 0.000000000000000000, 0.000000000000000000, -1.000000000000000000 ) ) ;
#49671 = UNCERTAINTY_MEASURE_WITH_UNIT (LENGTH_MEASURE( 1.000000000000000082E-05 ), #14794, 'distance_accuracy_value', 'NONE');
#49672 = COLOUR_RGB ( '', 0.40784314, 0.44705882, 0.49803922) ;
#49673 =( REPRESENTATION_RELATIONSHIP ('NONE','NONE', #5102, #67568 ) REPRESENTATION_RELATIONSHIP_WITH_TRANSFORMATION ( #37818 )SHAPE_REPRESENTATION_RELATIONSHIP( ) );
#49674 = PLANE ( 'NONE',  #67237 ) ;
#49675 = EDGE_CURVE ( 'NONE', #48195, #35027, #24809, .T. ) ;
#49676 = SURFACE_STYLE_USAGE ( .BOTH. , #27489 ) ;
#49677 = CARTESIAN_POINT ( 'NONE',  ( 2.999999999999993339, 5.000000000000000000, 24.00402776293822882 ) ) ;
#49678 = CARTESIAN_POINT ( 'NONE',  ( -77.39292637653380780, 8.102448949553176405, 5.886773742842740909 ) ) ;
#49679 = ORIENTED_EDGE ( 'NONE', *, *, #53152, .T. ) ;
#49680 = ORIENTED_EDGE ( 'NONE', *, *, #1203, .F. ) ;
#49681 = CARTESIAN_POINT ( 'NONE',  ( -44.99154893906889896, 9.591540376338688390, -3.113676943954755139 ) ) ;
#49682 = CARTESIAN_POINT ( 'NONE',  ( -5.603096392576914830, 1.514639124457109354, 8.295152368350901639 ) ) ;
#49683 = AXIS2_PLACEMENT_3D ( 'NONE', #50612, #66083, #33394 ) ;
#49684 = CARTESIAN_POINT ( 'NONE',  ( -82.10499999999998977, -6.826472737025115478, 4.959722759717900331 ) ) ;
#49685 = ORIENTED_EDGE ( 'NONE', *, *, #48504, .F. ) ;
#49686 = FILL_AREA_STYLE_COLOUR ( '', #3632 ) ;
#49687 = STYLED_ITEM ( 'NONE', ( #55543 ), #18880 ) ;
#49688 =( NAMED_UNIT ( * ) SI_UNIT ( $, .STERADIAN. ) SOLID_ANGLE_UNIT ( ) );
#49689 = COLOUR_RGB ( '', 0.66274510, 0.83137255, 0.94901961) ;
#49690 = CARTESIAN_POINT ( 'NONE',  ( -75.00000000000000000, 8.411230060884987481, -6.233452521073311381 ) ) ;
#49691 = ORIENTED_EDGE ( 'NONE', *, *, #20080, .F. ) ;
#49692 = FILL_AREA_STYLE ('',( #7463 ) ) ;
#49693 = MECHANICAL_DESIGN_GEOMETRIC_PRESENTATION_REPRESENTATION (  '', ( #47516 ), #41877 ) ;
#49694 = CARTESIAN_POINT ( 'NONE',  ( 5.598654528085805993, 126.2449999999999903, 7.705886871421374629 ) ) ;
#49695 = CARTESIAN_POINT ( 'NONE',  ( -110.9950000000000045, -6.826472737025115478, 4.959722759717900331 ) ) ;
#49696 = CIRCLE ( 'NONE', #41843, 0.5000000000000004441 ) ;
#49697 = CARTESIAN_POINT ( 'NONE',  ( -15.65902202074856397, 10.92377308316372897, -4.967528286585814357 ) ) ;
#49698 = AXIS2_PLACEMENT_3D ( 'NONE', #53543, #58821, #25753 ) ;
#49699 = CARTESIAN_POINT ( 'NONE',  ( -153.5929263765338249, -3.094860106618431139, -9.524999999999991473 ) ) ;
#49700 = CARTESIAN_POINT ( 'NONE',  ( -175.6449999999999818, 4.716976649647091513, -6.492361379858946790 ) ) ;
#49701 = STYLED_ITEM ( 'NONE', ( #48739 ), #23705 ) ;
#49702 = CARTESIAN_POINT ( 'NONE',  ( -75.75000000000000000, -0.9999999999999995559, 6.000000000000001776 ) ) ;
#49703 = AXIS2_PLACEMENT_3D ( 'NONE', #10284, #5660, #63395 ) ;
#49704 = CARTESIAN_POINT ( 'NONE',  ( -41.49999999999997868, 10.49999999999998401, 3.500000000000000000 ) ) ;
#49705 = ORIENTED_EDGE ( 'NONE', *, *, #59147, .T. ) ;
#49706 = CARTESIAN_POINT ( 'NONE',  ( -12.74999999999999822, -3.000000000000000000, 7.000000000000001776 ) ) ;
#49707 = VERTEX_POINT ( 'NONE', #52604 ) ;
#49708 = CARTESIAN_POINT ( 'NONE',  ( -70.34292637653381064, -9.058813317711329915, 2.943386871421371787 ) ) ;
#49709 = SURFACE_STYLE_FILL_AREA ( #49365 ) ;
#49710 = DIRECTION ( 'NONE',  ( 0.000000000000000000, 1.000000000000000000, 0.000000000000000000 ) ) ;
#49711 = AXIS2_PLACEMENT_3D ( 'NONE', #54974, #6802, #25755 ) ;
#49712 = CARTESIAN_POINT ( 'NONE',  ( 98.00000000000000000, 14.00000000000000000, -12.50000000000000178 ) ) ;
#49713 =( NAMED_UNIT ( * ) PLANE_ANGLE_UNIT ( ) SI_UNIT ( $, .RADIAN. ) );
#49714 = DIRECTION ( 'NONE',  ( -0.000000000000000000, -1.000000000000000000, -0.000000000000000000 ) ) ;
#49715 = ORIENTED_EDGE ( 'NONE', *, *, #23823, .T. ) ;
#49716 = CARTESIAN_POINT ( 'NONE',  ( -168.2049999999999841, -2.607480562269071545, -8.024999999999991473 ) ) ;
#49717 = MECHANICAL_DESIGN_GEOMETRIC_PRESENTATION_REPRESENTATION (  '', ( #39606 ), #17148 ) ;
#49718 = ORIENTED_EDGE ( 'NONE', *, *, #13085, .F. ) ;
#49719 = VECTOR ( 'NONE', #66713, 1000.000000000000000 ) ;
#49720 = SURFACE_SIDE_STYLE ('',( #33860 ) ) ;
#49721 = SPHERICAL_SURFACE ( 'NONE', #1684, 1.000000000000000000 ) ;
#49722 = DIRECTION ( 'NONE',  ( 0.000000000000000000, 0.000000000000000000, 1.000000000000000000 ) ) ;
#49723 = EDGE_CURVE ( 'NONE', #32327, #59351, #65614, .T. ) ;
#49724 = CARTESIAN_POINT ( 'NONE',  ( 0.000000000000000000, -3.500000000000000000, 24.00000000000000000 ) ) ;
#49725 = FACE_BOUND ( 'NONE', #711, .T. ) ;
#49726 = CARTESIAN_POINT ( 'NONE',  ( 8.437984349512095861, 150.3070736234661240, 1.550032578732817026E-15 ) ) ;
#49727 = EDGE_CURVE ( 'NONE', #54121, #599, #58204, .T. ) ;
#49728 = ORIENTED_EDGE ( 'NONE', *, *, #53917, .F. ) ;
#49729 = LINE ( 'NONE', #1470, #39534 ) ;
#49730 = CARTESIAN_POINT ( 'NONE',  ( -86.60500000000000398, 6.826472737025113702, -4.959722759717902107 ) ) ;
#49731 = UNCERTAINTY_MEASURE_WITH_UNIT (LENGTH_MEASURE( 1.000000000000000082E-05 ), #25437, 'distance_accuracy_value', 'NONE');
#49732 = CIRCLE ( 'NONE', #59867, 0.5000000000000004441 ) ;
#49733 = CARTESIAN_POINT ( 'NONE',  ( -127.4929263765338163, -8.102448949553174629, 5.886773742842742685 ) ) ;
#49734 = DIRECTION ( 'NONE',  ( 0.000000000000000000, 0.000000000000000000, -1.000000000000000000 ) ) ;
#49735 = EDGE_CURVE ( 'NONE', #29559, #2089, #20869, .T. ) ;
#49736 = SURFACE_SIDE_STYLE ('',( #65905 ) ) ;
#49737 = ORIENTED_EDGE ( 'NONE', *, *, #54189, .F. ) ;
#49738 = VECTOR ( 'NONE', #12175, 1000.000000000000000 ) ;
#49739 = CIRCLE ( 'NONE', #54288, 0.5000000000000004441 ) ;
#49740 =( LENGTH_UNIT ( ) NAMED_UNIT ( * ) SI_UNIT ( .MILLI., .METRE. ) );
#49741 = CARTESIAN_POINT ( 'NONE',  ( -62.99499999999996902, -6.826472737025115478, 4.959722759717900331 ) ) ;
#49742 = ORIENTED_EDGE ( 'NONE', *, *, #54854, .F. ) ;
#49743 =( NAMED_UNIT ( * ) PLANE_ANGLE_UNIT ( ) SI_UNIT ( $, .RADIAN. ) );
#49744 = STYLED_ITEM ( 'NONE', ( #22480 ), #46507 ) ;
#49745 = CARTESIAN_POINT ( 'NONE',  ( -49.79292637653379217, -3.094860106618429807, 9.524999999999991473 ) ) ;
#49746 = CARTESIAN_POINT ( 'NONE',  ( -45.00000000000000711, 8.554981036081898083, -6.127545679190936845 ) ) ;
#49747 = EDGE_CURVE ( 'NONE', #49208, #33374, #52938, .T. ) ;
#49748 = ORIENTED_EDGE ( 'NONE', *, *, #51887, .F. ) ;
#49749 = CARTESIAN_POINT ( 'NONE',  ( -55.19499999999998607, 8.437984349512086979, -1.550032578732815448E-15 ) ) ;
#49750 = SPHERICAL_SURFACE ( 'NONE', #31436, 0.2500000000000000000 ) ;
#49751 = ORIENTED_EDGE ( 'NONE', *, *, #29739, .F. ) ;
#49752 = PRESENTATION_LAYER_ASSIGNMENT (  '', '', ( #261 ) ) ;
#49753 = CARTESIAN_POINT ( 'NONE',  ( -75.00000000000000000, 7.951225523245171622, 6.457238017240461758 ) ) ;
#49754 = CARTESIAN_POINT ( 'NONE',  ( -110.1549999999999869, 7.632228543268600340, 2.479861379858949277 ) ) ;
#49755 = EDGE_LOOP ( 'NONE', ( #20503, #28395, #18693, #19437 ) ) ;
#49757 = AXIS2_PLACEMENT_3D ( 'NONE', #49911, #44661, #66053 ) ;
#49756 = CARTESIAN_POINT ( 'NONE',  ( 2.418047948276646597, 2.101261491285135286, -7.000000000000001776 ) ) ;
#49758 = CARTESIAN_POINT ( 'NONE',  ( 21.75000000000001066, 21.99999999999998224, -3.750000000000000000 ) ) ;
#49759 = DIRECTION ( 'NONE',  ( 1.000000000000000000, 0.000000000000000000, 0.000000000000000000 ) ) ;
#49760 = CYLINDRICAL_SURFACE ( 'NONE', #7271, 0.2500000000000002220 ) ;
#49761 =( NAMED_UNIT ( * ) SI_UNIT ( $, .STERADIAN. ) SOLID_ANGLE_UNIT ( ) );
#49762 = CARTESIAN_POINT ( 'NONE',  ( -146.4570736234661865, -9.058813317711329915, 2.943386871421371787 ) ) ;
#49763 =( NAMED_UNIT ( * ) PLANE_ANGLE_UNIT ( ) SI_UNIT ( $, .RADIAN. ) );
#49764 = CARTESIAN_POINT ( 'NONE',  ( 9.058813317711338797, 135.8449999999999989, -2.943386871421372675 ) ) ;
#49765 = CARTESIAN_POINT ( 'NONE',  ( -86.00707362346616947, -8.102448949553172852, -5.886773742842741797 ) ) ;
#49766 = MECHANICAL_DESIGN_GEOMETRIC_PRESENTATION_REPRESENTATION (  '', ( #48599 ), #58750 ) ;
#49767 = DIRECTION ( 'NONE',  ( 0.000000000000000000, -1.000000000000000000, 0.000000000000000000 ) ) ;
#49768 = ORIENTED_EDGE ( 'NONE', *, *, #56954, .T. ) ;
#49769 =( NAMED_UNIT ( * ) SI_UNIT ( $, .STERADIAN. ) SOLID_ANGLE_UNIT ( ) );
#49770 = CARTESIAN_POINT ( 'NONE',  ( 0.000000000000000000, 21.74999999999998579, 4.000000000000000000 ) ) ;
#49772 = AXIS2_PLACEMENT_3D ( 'NONE', #16462, #16108, #68868 ) ;
#49771 = PRESENTATION_STYLE_ASSIGNMENT (( #6841 ) ) ;
#49773 = CARTESIAN_POINT ( 'NONE',  ( -135.2050000000000125, -2.607480562269071545, -8.024999999999991473 ) ) ;
#49774 = CARTESIAN_POINT ( 'NONE',  ( -165.4429263765337907, -1.166476076187852838E-15, -9.524999999999991473 ) ) ;
#49775 = PRESENTATION_STYLE_ASSIGNMENT (( #54680 ) ) ;
#49776 = CARTESIAN_POINT ( 'NONE',  ( -55.79292637653379927, -3.094860106618429807, 9.524999999999991473 ) ) ;
#49777 = CARTESIAN_POINT ( 'NONE',  ( -133.6449999999999818, 4.716976649647091513, -6.492361379858946790 ) ) ;
#49778 = CARTESIAN_POINT ( 'NONE',  ( -129.2949999999999875, -2.607480562269069768, 8.024999999999991473 ) ) ;
#49779 = ORIENTED_EDGE ( 'NONE', *, *, #50250, .T. ) ;
#49780 = ADVANCED_FACE ( 'NONE', ( #46663 ), #26525, .T. ) ;
#49781 = CARTESIAN_POINT ( 'NONE',  ( 28.00000000000002842, 38.70020753820971748, 89.00000000000000000 ) ) ;
#49782 = SPHERICAL_SURFACE ( 'NONE', #32296, 0.5000000000000000000 ) ;
#49783 = FILL_AREA_STYLE_COLOUR ( '', #37338 ) ;
#49784 = CARTESIAN_POINT ( 'NONE',  ( -178.4929263765338021, -8.102448949553172852, 5.886773742842742685 ) ) ;
#49785 =( BOUNDED_CURVE ( )  B_SPLINE_CURVE ( 2, ( #51960, #26245, #57570, #36138, #69175, #9404, #63540, #57936, #57212, #30824, #52323 ),
 .UNSPECIFIED., .F., .F. ) 
 B_SPLINE_CURVE_WITH_KNOTS ( ( 3, 2, 2, 2, 2, 3 ),
 ( 0.04347826086956422392, 0.04565217391304243755, 0.04782608695652065117, 0.04999999999999885786, 0.05217391304347706454, 0.05434782608695527817 ),
 .UNSPECIFIED. ) 
 CURVE ( )  GEOMETRIC_REPRESENTATION_ITEM ( )  RATIONAL_B_SPLINE_CURVE ( ( 1.000000000000022427, 0.9510565162951313267, 1.000000000000000000, 0.9510565162951535312, 1.000000000000000000, 0.9510565162951535312, 1.000000000000000000, 0.9510565162951535312, 1.000000000000000000, 0.9510565162951815088, 0.9999999999999720224 ) ) 
 REPRESENTATION_ITEM ( '' )  );
#49786 = DIRECTION ( 'NONE',  ( 1.000000000000000000, 0.000000000000000000, 0.000000000000000000 ) ) ;
#49787 = CARTESIAN_POINT ( 'NONE',  ( -63.29499999999998749, -2.607480562269069768, 8.024999999999991473 ) ) ;
#49788 = CARTESIAN_POINT ( 'NONE',  ( 36.00000000000002132, 0.000000000000000000, -77.00402776293825013 ) ) ;
#49789 = SURFACE_STYLE_FILL_AREA ( #18118 ) ;
#49790 = DIRECTION ( 'NONE',  ( 0.000000000000000000, 0.000000000000000000, 1.000000000000000000 ) ) ;
#49791 =( NAMED_UNIT ( * ) SI_UNIT ( $, .STERADIAN. ) SOLID_ANGLE_UNIT ( ) );
#49792 = CARTESIAN_POINT ( 'NONE',  ( -90.74292637653380211, -5.598654528085803328, -7.705886871421366635 ) ) ;
#49793 = SHAPE_DEFINITION_REPRESENTATION ( #27116, #67568 ) ;
#49794 = CARTESIAN_POINT ( 'NONE',  ( -48.85491959229422321, -13.04958088359142288, 1.031244760999817212 ) ) ;
#49795 = DIRECTION ( 'NONE',  ( 0.000000000000000000, 0.000000000000000000, 1.000000000000000000 ) ) ;
#49796 = CIRCLE ( 'NONE', #31798, 0.2500000000000002220 ) ;
#49797 = DIRECTION ( 'NONE',  ( 0.000000000000000000, 0.000000000000000000, -1.000000000000000000 ) ) ;
#49798 = DIRECTION ( 'NONE',  ( 0.000000000000000000, 0.000000000000000000, -1.000000000000000000 ) ) ;
#49799 = CARTESIAN_POINT ( 'NONE',  ( -41.84210526315788314, 107.2928455055531600, 4.000000000000000000 ) ) ;
#49800 = EDGE_CURVE ( 'NONE', #68674, #15666, #16427, .T. ) ;
#49801 = DIRECTION ( 'NONE',  ( 1.000000000000000000, 0.000000000000000000, 0.000000000000000000 ) ) ;
#49802 = EDGE_CURVE ( 'NONE', #61721, #59451, #54971, .T. ) ;
#49803 = EDGE_LOOP ( 'NONE', ( #16102, #945, #21427, #29813 ) ) ;
#49804 = DIRECTION ( 'NONE',  ( 1.000000000000000000, 0.000000000000000000, 0.000000000000000000 ) ) ;
#49805 = MANIFOLD_SOLID_BREP ( 'Chamfer1', #17188 ) ;
#49806 = CARTESIAN_POINT ( 'NONE',  ( 27.99999999999999289, 43.00000000000000000, -90.00000000000000000 ) ) ;
#49807 = EDGE_LOOP ( 'NONE', ( #64772, #65424, #349, #44740 ) ) ;
#49808 = CARTESIAN_POINT ( 'NONE',  ( 6.000000000000017764, 26.00000000000000355, 23.99999999999999645 ) ) ;
#49809 = CIRCLE ( 'NONE', #16139, 5.499999999999984901 ) ;
#49810 = CARTESIAN_POINT ( 'NONE',  ( -2.607480562269073765, 121.2070736234661581, -8.025000000000000355 ) ) ;
#49811 = CIRCLE ( 'NONE', #19467, 3.599999999999992095 ) ;
#49812 = EDGE_CURVE ( 'NONE', #65754, #54235, #41939, .T. ) ;
#49813 = CARTESIAN_POINT ( 'NONE',  ( 23.50000000000001776, -3.148064030671221758, -27.18999999999999417 ) ) ;
#49815 = FACE_OUTER_BOUND ( 'NONE', #44472, .T. ) ;
#49814 = TOROIDAL_SURFACE ( 'NONE', #36402, 0.7500000000000000000, 0.2500000000000000000 ) ;
#49816 = DIRECTION ( 'NONE',  ( 1.000000000000000000, 0.000000000000000000, 0.000000000000000000 ) ) ;
#49817 = VERTEX_POINT ( 'NONE', #59922 ) ;
#49818 = FACE_OUTER_BOUND ( 'NONE', #28934, .T. ) ;
#49819 = DIRECTION ( 'NONE',  ( 0.000000000000000000, 0.000000000000000000, -1.000000000000000000 ) ) ;
#49820 = ORIENTED_EDGE ( 'NONE', *, *, #24897, .T. ) ;
#49821 = SURFACE_SIDE_STYLE ('',( #38609 ) ) ;
#49822 = ADVANCED_FACE ( 'NONE', ( #12414 ), #27194, .T. ) ;
#49823 = CARTESIAN_POINT ( 'NONE',  ( 3.000000000000002665, 35.42594141563417054, -80.00402776293826435 ) ) ;
#49824 = CARTESIAN_POINT ( 'NONE',  ( -94.04499999999998749, 7.632228543268600340, 2.479861379858949277 ) ) ;
#49825 = ORIENTED_EDGE ( 'NONE', *, *, #28439, .T. ) ;
#49826 = AXIS2_PLACEMENT_3D ( 'NONE', #25947, #52024, #3062 ) ;
#49827 = CARTESIAN_POINT ( 'NONE',  ( 32.00000000000001421, 42.00000000000000000, 35.50000000000000000 ) ) ;
#49828 = CIRCLE ( 'NONE', #34100, 22.00000000000001421 ) ;
#49829 = DIRECTION ( 'NONE',  ( 0.000000000000000000, -1.000000000000000000, 0.000000000000000000 ) ) ;
#49830 = EDGE_CURVE ( 'NONE', #21095, #5051, #53501, .T. ) ;
#49831 = EDGE_LOOP ( 'NONE', ( #66972, #63501, #46054, #46873 ) ) ;
#49832 = CARTESIAN_POINT ( 'NONE',  ( 7.632228543268607446, 161.0429263765338419, 2.479861379858954606 ) ) ;
#49833 = CARTESIAN_POINT ( 'NONE',  ( -23.21231517720797655, 117.4999999999999716, -9.500000000000000000 ) ) ;
#49834 = ORIENTED_EDGE ( 'NONE', *, *, #60685, .F. ) ;
#49835 = LINE ( 'NONE', #27646, #16189 ) ;
#49836 = ORIENTED_EDGE ( 'NONE', *, *, #38583, .T. ) ;
#49837 = DIRECTION ( 'NONE',  ( 0.000000000000000000, 0.000000000000000000, -1.000000000000000000 ) ) ;
#49838 =( NAMED_UNIT ( * ) PLANE_ANGLE_UNIT ( ) SI_UNIT ( $, .RADIAN. ) );
#49839 = DIRECTION ( 'NONE',  ( 0.000000000000000000, 0.000000000000000000, 1.000000000000000000 ) ) ;
#49840 = CARTESIAN_POINT ( 'NONE',  ( 0.000000000000000000, 0.000000000000000000, 1.000000000000000000 ) ) ;
#49841 = VECTOR ( 'NONE', #2679, 1000.000000000000000 ) ;
#49842 = MECHANICAL_DESIGN_GEOMETRIC_PRESENTATION_REPRESENTATION (  '', ( #19488 ), #6086 ) ;
#49843 = CARTESIAN_POINT ( 'NONE',  ( -177.3570736234661638, 5.598654528085804216, 7.705886871421366635 ) ) ;
#49844 = B_SPLINE_CURVE_WITH_KNOTS ( 'NONE', 3,
 ( #20409, #68965, #63667, #58743, #15510, #64006, #37333, #55166 ),
 .UNSPECIFIED., .F., .F.,
 ( 4, 2, 2, 4 ),
 ( 2.544316211735830308E-07, 0.002094919859796804274, 0.003142252573884619406, 0.004189585287972434971 ),
 .UNSPECIFIED. ) ;
#49845 = DIRECTION ( 'NONE',  ( -1.000000000000000000, 0.000000000000000000, 0.000000000000000000 ) ) ;
#49846 = DIRECTION ( 'NONE',  ( -0.000000000000000000, -0.000000000000000000, -1.000000000000000000 ) ) ;
#49847 = CARTESIAN_POINT ( 'NONE',  ( -114.5070736234661979, 8.102448949553176405, 5.886773742842740909 ) ) ;
#49848 = PRESENTATION_LAYER_ASSIGNMENT (  '', '', ( #20615 ) ) ;
#49849 = VECTOR ( 'NONE', #33868, 1000.000000000000000 ) ;
#49850 = CARTESIAN_POINT ( 'NONE',  ( -2.244403820859647070, 9.000000000000012434, 0.2663676893021043601 ) ) ;
#49851 = DIRECTION ( 'NONE',  ( -1.000000000000000000, 0.000000000000000000, 0.000000000000000000 ) ) ;
#49852 = ORIENTED_EDGE ( 'NONE', *, *, #19749, .F. ) ;
#49853 = CARTESIAN_POINT ( 'NONE',  ( 7.342319042881613633, -2.499999999999998224, -5.282730372348551029 ) ) ;
#49854 = CARTESIAN_POINT ( 'NONE',  ( 74.49999999999998579, 119.9999999999997584, 9.500000000000000000 ) ) ;
#49855 = CARTESIAN_POINT ( 'NONE',  ( -149.4570736234661581, -9.058813317711329915, 2.943386871421371787 ) ) ;
#49856 = VERTEX_POINT ( 'NONE', #33875 ) ;
#49857 = AXIS2_PLACEMENT_3D ( 'NONE', #9228, #3540, #35958 ) ;
#49858 = CARTESIAN_POINT ( 'NONE',  ( -156.6550000000000011, -7.632228543268600340, -2.479861379858950166 ) ) ;
#49859 = FACE_OUTER_BOUND ( 'NONE', #19938, .T. ) ;
#49860 = CARTESIAN_POINT ( 'NONE',  ( 27.99999999999998224, 0.000000000000000000, 72.00402776293822171 ) ) ;
#49861 = CARTESIAN_POINT ( 'NONE',  ( -170.0949999999999704, -2.607480562269071545, -8.024999999999991473 ) ) ;
#49862 = TOROIDAL_SURFACE ( 'NONE', #2596, 1.000000000000000000, 0.5000000000000000000 ) ;
#49863 = CARTESIAN_POINT ( 'NONE',  ( -156.1450000000000102, -4.716976649647092401, 6.492361379858946790 ) ) ;
#49864 = ORIENTED_EDGE ( 'NONE', *, *, #18178, .F. ) ;
#49865 = EDGE_CURVE ( 'NONE', #6562, #25647, #34363, .T. ) ;
#49866 = CARTESIAN_POINT ( 'NONE',  ( -90.14292637653380780, 5.598654528085800663, -7.705886871421367523 ) ) ;
#49867 = CARTESIAN_POINT ( 'NONE',  ( 44.24703880899742359, 10.19173881602634246, 3.568710496479965411 ) ) ;
#49868 = SURFACE_STYLE_USAGE ( .BOTH. , #27671 ) ;
#49869 = CARTESIAN_POINT ( 'NONE',  ( -75.35499999999998977, -4.716976649647093289, -6.492361379858945902 ) ) ;
#49870 = CARTESIAN_POINT ( 'NONE',  ( 23.67886883698855272, 24.55989583710066171, 27.18999999999999062 ) ) ;
#49871 = DIRECTION ( 'NONE',  ( -0.000000000000000000, -1.000000000000000000, -0.000000000000000000 ) ) ;
#49872 = CIRCLE ( 'NONE', #28488, 10.02499999999997904 ) ;
#49873 = CARTESIAN_POINT ( 'NONE',  ( -75.44499999999997897, 0.000000000000000000, 8.024999999999991473 ) ) ;
#49874 = CARTESIAN_POINT ( 'NONE',  ( 3.094860106618435136, 146.4050000000000011, -9.525000000000000355 ) ) ;
#49875 = CYLINDRICAL_SURFACE ( 'NONE', #32033, 9.524999999999991473 ) ;
#49876 = VECTOR ( 'NONE', #11307, 1000.000000000000000 ) ;
#49877 = CARTESIAN_POINT ( 'NONE',  ( -51.84221223720477667, -8.171052631578943348, 2.722470280083839178 ) ) ;
#49878 = AXIS2_PLACEMENT_3D ( 'NONE', #16054, #472, #32903 ) ;
#49879 = SURFACE_SIDE_STYLE ('',( #12913 ) ) ;
#49880 = FILL_AREA_STYLE_COLOUR ( '', #3432 ) ;
#49881 = COLOUR_RGB ( '', 0.72549020, 0.75294118, 0.79215686) ;
#49882 = ORIENTED_EDGE ( 'NONE', *, *, #57514, .F. ) ;
#49883 = ADVANCED_FACE ( 'NONE', ( #2871 ), #66598, .T. ) ;
#49884 = FILL_AREA_STYLE_COLOUR ( '', #10099 ) ;
#49885 = DIRECTION ( 'NONE',  ( 0.000000000000000000, 0.000000000000000000, 1.000000000000000000 ) ) ;
#49886 = EDGE_CURVE ( 'NONE', #17642, #6589, #23675, .T. ) ;
#49887 = AXIS2_PLACEMENT_3D ( 'NONE', #52699, #31910, #68882 ) ;
#49888 = DIRECTION ( 'NONE',  ( 0.000000000000000000, -1.000000000000000000, 0.000000000000000000 ) ) ;
#49889 = ADVANCED_FACE ( 'NONE', ( #45178 ), #34929, .F. ) ;
#49890 = CARTESIAN_POINT ( 'NONE',  ( -119.9929263765338021, 8.102448949553172852, -5.886773742842744461 ) ) ;
#49891 = EDGE_LOOP ( 'NONE', ( #12060, #8878, #18271, #46112 ) ) ;
#49893 = ORIENTED_EDGE ( 'NONE', *, *, #38075, .F. ) ;
#49892 = AXIS2_PLACEMENT_3D ( 'NONE', #37128, #58535, #14244 ) ;
#49894 = COLOUR_RGB ( '', 0.31764706, 0.68627451, 0.89019608) ;
#49895 = CARTESIAN_POINT ( 'NONE',  ( 0.000000000000000000, 134.9429263765338192, -8.025000000000000355 ) ) ;
#49896 = CARTESIAN_POINT ( 'NONE',  ( -195.0000000000000000, 0.000000000000000000, 7.499999999999985789 ) ) ;
#49897 = ADVANCED_FACE ( 'NONE', ( #7840 ), #19076, .T. ) ;
#49898 = CARTESIAN_POINT ( 'NONE',  ( 1.000000000000000000, 36.74999999999999289, -3.000000000000000000 ) ) ;
#49899 = FACE_OUTER_BOUND ( 'NONE', #36554, .T. ) ;
#49900 = ADVANCED_FACE ( 'NONE', ( #58135 ), #62681, .T. ) ;
#49901 = VERTEX_POINT ( 'NONE', #63044 ) ;
#49902 = CARTESIAN_POINT ( 'NONE',  ( -114.0549999999999926, -9.827790563157499189E-16, -8.024999999999991473 ) ) ;
#49903 = ORIENTED_EDGE ( 'NONE', *, *, #64894, .F. ) ;
#49904 = FACE_OUTER_BOUND ( 'NONE', #49602, .T. ) ;
#49905 = CARTESIAN_POINT ( 'NONE',  ( 6.898093598910799429, -6.052151411320861207, 0.1381979515792686741 ) ) ;
#49906 = CIRCLE ( 'NONE', #420, 0.2500000000000002220 ) ;
#49907 = ORIENTED_EDGE ( 'NONE', *, *, #42320, .F. ) ;
#49908 = CARTESIAN_POINT ( 'NONE',  ( 9.827790563157511022E-16, 87.30187232391182306, -8.025000000000000355 ) ) ;
#49909 = VERTEX_POINT ( 'NONE', #4269 ) ;
#49910 = CIRCLE ( 'NONE', #64511, 0.2500000000000002220 ) ;
#49911 = CARTESIAN_POINT ( 'NONE',  ( 48.25000000000000000, 22.24999999999998579, 3.750000000000000000 ) ) ;
#49912 = VERTEX_POINT ( 'NONE', #47979 ) ;
#49913 = PRESENTATION_LAYER_ASSIGNMENT (  '', '', ( #63358 ) ) ;
#49914 =( BOUNDED_CURVE ( )  B_SPLINE_CURVE ( 2, ( #28705, #7279, #34351, #55800, #12528, #7962, #45644, #29405, #60374, #12176, #50879 ),
 .UNSPECIFIED., .F., .F. ) 
 B_SPLINE_CURVE_WITH_KNOTS ( ( 3, 2, 2, 2, 2, 3 ),
 ( 0.7065217391304348116, 0.7086956521739130599, 0.7108695652173913082, 0.7130434782608695565, 0.7152173913043478048, 0.7173913043478260532 ),
 .UNSPECIFIED. ) 
 CURVE ( )  GEOMETRIC_REPRESENTATION_ITEM ( )  RATIONAL_B_SPLINE_CURVE ( ( 1.000000000000000000, 0.9510565162951535312, 1.000000000000000000, 0.9510565162951535312, 1.000000000000000000, 0.9510565162951535312, 1.000000000000000000, 0.9510565162951535312, 1.000000000000000000, 0.9510565162951535312, 1.000000000000000000 ) ) 
 REPRESENTATION_ITEM ( '' )  );
#49915 = ORIENTED_EDGE ( 'NONE', *, *, #51406, .F. ) ;
#49916 = LINE ( 'NONE', #1970, #40064 ) ;
#49917 = DIRECTION ( 'NONE',  ( -0.000000000000000000, 1.000000000000000000, 0.000000000000000000 ) ) ;
#49918 = CARTESIAN_POINT ( 'NONE',  ( -152.7570736234661979, -5.598654528085801552, 7.705886871421367523 ) ) ;
#49919 = CARTESIAN_POINT ( 'NONE',  ( -9.566487832665403701, -1.863712308906138704, -1.430357023834059271 ) ) ;
#49920 = CIRCLE ( 'NONE', #22951, 4.999999999999990230 ) ;
#49921 = EDGE_LOOP ( 'NONE', ( #24600, #31023, #57678, #54551 ) ) ;
#49922 = CARTESIAN_POINT ( 'NONE',  ( -6.826472737025120807, 132.9929263765338305, 4.959722759717906548 ) ) ;
#49923 = DIRECTION ( 'NONE',  ( 0.000000000000000000, 1.000000000000000000, 0.000000000000000000 ) ) ;
#49924 = FACE_OUTER_BOUND ( 'NONE', #14610, .T. ) ;
#49925 = DIRECTION ( 'NONE',  ( -0.000000000000000000, 1.000000000000000000, -0.000000000000000000 ) ) ;
#49926 = DIRECTION ( 'NONE',  ( 0.000000000000000000, 0.000000000000000000, -1.000000000000000000 ) ) ;
#49927 = ADVANCED_FACE ( 'NONE', ( #30318 ), #9614, .T. ) ;
#49928 = ORIENTED_EDGE ( 'NONE', *, *, #38403, .F. ) ;
#49929 = ORIENTED_EDGE ( 'NONE', *, *, #27688, .T. ) ;
#49930 = CARTESIAN_POINT ( 'NONE',  ( 22.75000000000000711, 0.000000000000000000, 3.750000000000000000 ) ) ;
#49931 = CARTESIAN_POINT ( 'NONE',  ( -44.50000000000000000, 99.99999999999992895, 4.000000000000000000 ) ) ;
#49932 = AXIS2_PLACEMENT_3D ( 'NONE', #31024, #14502, #52176 ) ;
#49933 = CARTESIAN_POINT ( 'NONE',  ( -130.1049999999999898, -6.826472737025115478, 4.959722759717900331 ) ) ;
#49934 = FACE_OUTER_BOUND ( 'NONE', #43664, .T. ) ;
#49935 = EDGE_CURVE ( 'NONE', #48634, #15615, #31725, .T. ) ;
#49936 = ORIENTED_EDGE ( 'NONE', *, *, #59547, .F. ) ;
#49937 = COLOUR_RGB ( '', 0.66274510, 0.83137255, 0.94901961) ;
#49938 = STYLED_ITEM ( 'NONE', ( #51303 ), #7858 ) ;
#49939 = CARTESIAN_POINT ( 'NONE',  ( 22.75000000000000711, 37.00000000000000000, 3.750000000000000000 ) ) ;
#49940 = CARTESIAN_POINT ( 'NONE',  ( -156.5929263765341375, -3.094860106624447660, -9.524999999995621636 ) ) ;
#49941 = SURFACE_STYLE_USAGE ( .BOTH. , #50962 ) ;
#49942 = ORIENTED_EDGE ( 'NONE', *, *, #13815, .T. ) ;
#49943 = ORIENTED_EDGE ( 'NONE', *, *, #37637, .F. ) ;
#49944 = CARTESIAN_POINT ( 'NONE',  ( -45.00000000000000000, 9.708372675170618749, 3.611004237778676185 ) ) ;
#49945 = DIRECTION ( 'NONE',  ( -0.000000000000000000, -1.000000000000000000, -0.000000000000000000 ) ) ;
#49946 = AXIS2_PLACEMENT_3D ( 'NONE', #36663, #26041, #47579 ) ;
#49947 = ORIENTED_EDGE ( 'NONE', *, *, #19621, .F. ) ;
#49948 = CARTESIAN_POINT ( 'NONE',  ( -75.75000000000000000, 0.000000000000000000, 7.000000000000001776 ) ) ;
#49949 = SURFACE_SIDE_STYLE ('',( #22862 ) ) ;
#49950 = DIRECTION ( 'NONE',  ( 0.000000000000000000, 1.000000000000000000, 0.000000000000000000 ) ) ;
#49951 = DIRECTION ( 'NONE',  ( 0.000000000000000000, 0.000000000000000000, 1.000000000000000000 ) ) ;
#49952 = CIRCLE ( 'NONE', #27459, 1.000000000000000888 ) ;
#49953 = PRESENTATION_LAYER_ASSIGNMENT (  '', '', ( #65639 ) ) ;
#49954 = CARTESIAN_POINT ( 'NONE',  ( -71.74137931034479720, 63.10081643261027295, -9.500000000000000000 ) ) ;
#49955 = CARTESIAN_POINT ( 'NONE',  ( 16.75000000000000711, 27.74999999999998224, 4.000000000000000000 ) ) ;
#49956 = ORIENTED_EDGE ( 'NONE', *, *, #51160, .T. ) ;
#49957 = FILL_AREA_STYLE ('',( #43426 ) ) ;
#49958 = CARTESIAN_POINT ( 'NONE',  ( -144.0570736234661808, 0.000000000000000000, 9.524999999999991473 ) ) ;
#49959 = LINE ( 'NONE', #33412, #7961 ) ;
#49960 = DIRECTION ( 'NONE',  ( 1.000000000000000000, 0.000000000000000000, 0.000000000000000000 ) ) ;
#49961 =( LENGTH_UNIT ( ) NAMED_UNIT ( * ) SI_UNIT ( .MILLI., .METRE. ) );
#49962 = DIRECTION ( 'NONE',  ( 0.000000000000000000, 0.000000000000000000, 1.000000000000000000 ) ) ;
#49963 = CIRCLE ( 'NONE', #47756, 0.5000000000000004441 ) ;
#49964 = CARTESIAN_POINT ( 'NONE',  ( -101.6949999999999648, -8.437984349512086979, 5.166775262442717831E-16 ) ) ;
#49965 = CARTESIAN_POINT ( 'NONE',  ( -3.094860106618432471, 113.7049999999999699, -9.525000000000000355 ) ) ;
#49966 = CARTESIAN_POINT ( 'NONE',  ( -78.44499999999999318, 0.000000000000000000, 8.024999999999991473 ) ) ;
#49967 = EDGE_CURVE ( 'NONE', #45388, #42340, #14184, .T. ) ;
#49968 =( LENGTH_UNIT ( ) NAMED_UNIT ( * ) SI_UNIT ( .MILLI., .METRE. ) );
#49969 =( GEOMETRIC_REPRESENTATION_CONTEXT ( 3 ) GLOBAL_UNCERTAINTY_ASSIGNED_CONTEXT ( ( #28511 ) ) GLOBAL_UNIT_ASSIGNED_CONTEXT ( ( #38764, #48631, #32062 ) ) REPRESENTATION_CONTEXT ( 'NONE', 'WORKASPACE' ) );
#49970 = CYLINDRICAL_SURFACE ( 'NONE', #4525, 0.2500000000000002220 ) ;
#49971 = DIRECTION ( 'NONE',  ( -1.000000000000000000, 0.000000000000000000, 0.000000000000000000 ) ) ;
#49972 = MECHANICAL_DESIGN_GEOMETRIC_PRESENTATION_REPRESENTATION (  '', ( #47763 ), #22996 ) ;
#49973 = CARTESIAN_POINT ( 'NONE',  ( -13.75000000000000533, 30.74999999999999289, -3.750000000000000000 ) ) ;
#49974 = ORIENTED_EDGE ( 'NONE', *, *, #5707, .T. ) ;
#49975 = EDGE_CURVE ( 'NONE', #45120, #18574, #47268, .T. ) ;
#49976 = CARTESIAN_POINT ( 'NONE',  ( -128.3929263765338078, 8.102448949553176405, 5.886773742842740909 ) ) ;
#49977 = AXIS2_PLACEMENT_3D ( 'NONE', #37720, #1347, #49613 ) ;
#49978 = PRESENTATION_STYLE_ASSIGNMENT (( #59813 ) ) ;
#49979 = CARTESIAN_POINT ( 'NONE',  ( -142.6449999999999818, 4.716976649647091513, -6.492361379858946790 ) ) ;
#49980 = SURFACE_STYLE_FILL_AREA ( #28472 ) ;
#49981 = EDGE_CURVE ( 'NONE', #149, #28296, #68123, .T. ) ;
#49982 = DIRECTION ( 'NONE',  ( 0.000000000000000000, 1.000000000000000000, -0.000000000000000000 ) ) ;
#49983 = EDGE_LOOP ( 'NONE', ( #37979, #15182, #44304, #44215 ) ) ;
#49984 = VERTEX_POINT ( 'NONE', #20849 ) ;
#49985 = CARTESIAN_POINT ( 'NONE',  ( -74.99999999999998579, 50.00000000000000000, -12.00000000000000000 ) ) ;
#49986 = AXIS2_PLACEMENT_3D ( 'NONE', #57286, #35843, #53068 ) ;
#49987 = CIRCLE ( 'NONE', #44450, 0.5000000000000004441 ) ;
#49988 = DIRECTION ( 'NONE',  ( -1.000000000000000000, 0.000000000000000000, 0.000000000000000000 ) ) ;
#49989 = CARTESIAN_POINT ( 'NONE',  ( -131.9070736234668004, -3.094860106607875583, 9.525000000007660006 ) ) ;
#49990 = LINE ( 'NONE', #24592, #27436 ) ;
#49992 = EDGE_CURVE ( 'NONE', #30142, #45750, #47631, .T. ) ;
#49991 = SURFACE_STYLE_USAGE ( .BOTH. , #67432 ) ;
#49993 = ORIENTED_EDGE ( 'NONE', *, *, #43590, .F. ) ;
#49994 = CARTESIAN_POINT ( 'NONE',  ( -140.9050000000000011, 2.607480562269069324, -8.024999999999993250 ) ) ;
#49995 = ORIENTED_EDGE ( 'NONE', *, *, #54623, .F. ) ;
#49996 = CIRCLE ( 'NONE', #54428, 1.000000000000000000 ) ;
#49997 = EDGE_LOOP ( 'NONE', ( #40142, #62615, #40652, #56886 ) ) ;
#49998 = ORIENTED_EDGE ( 'NONE', *, *, #18019, .T. ) ;
#49999 = CIRCLE ( 'NONE', #42151, 1.000000000000000000 ) ;
#50000 =( GEOMETRIC_REPRESENTATION_CONTEXT ( 3 ) GLOBAL_UNCERTAINTY_ASSIGNED_CONTEXT ( ( #19993 ) ) GLOBAL_UNIT_ASSIGNED_CONTEXT ( ( #3942, #35284, #30316 ) ) REPRESENTATION_CONTEXT ( 'NONE', 'WORKASPACE' ) );
#50001 = AXIS2_PLACEMENT_3D ( 'NONE', #16779, #40227, #19072 ) ;
#50002 = DIRECTION ( 'NONE',  ( -1.000000000000000000, 0.000000000000000000, 0.000000000000000000 ) ) ;
#50003 = SURFACE_STYLE_USAGE ( .BOTH. , #7427 ) ;
#50004 = CARTESIAN_POINT ( 'NONE',  ( 8.102448949553181734, 129.3949999999999818, 5.886773742842750679 ) ) ;
#50005 = ORIENTED_EDGE ( 'NONE', *, *, #16780, .F. ) ;
#50006 =( LENGTH_UNIT ( ) NAMED_UNIT ( * ) SI_UNIT ( .MILLI., .METRE. ) );
#50007 = CARTESIAN_POINT ( 'NONE',  ( 5.598654528085809545, 137.2549999999999955, -7.705886871421373741 ) ) ;
#50008 = CARTESIAN_POINT ( 'NONE',  ( -56.45499999999997698, 7.632228543268599452, -2.479861379858951942 ) ) ;
#50009 = FACE_OUTER_BOUND ( 'NONE', #64101, .T. ) ;
#50010 = VERTEX_POINT ( 'NONE', #30676 ) ;
#50011 = CARTESIAN_POINT ( 'NONE',  ( 5.598654528085809545, 161.2549999999999955, -7.705886871421373741 ) ) ;
#50012 = PLANE ( 'NONE',  #9783 ) ;
#50013 = VECTOR ( 'NONE', #52463, 1000.000000000000000 ) ;
#50014 = DIRECTION ( 'NONE',  ( 0.000000000000000000, -0.000000000000000000, -1.000000000000000000 ) ) ;
#50015 = FACE_OUTER_BOUND ( 'NONE', #32911, .T. ) ;
#50016 = STYLED_ITEM ( 'NONE', ( #47332 ), #38742 ) ;
#50017 = CYLINDRICAL_SURFACE ( 'NONE', #18564, 0.2500000000000002220 ) ;
#50018 = ORIENTED_EDGE ( 'NONE', *, *, #69568, .F. ) ;
#50019 = CIRCLE ( 'NONE', #26393, 4.999999999999990230 ) ;
#50020 = ORIENTED_EDGE ( 'NONE', *, *, #28580, .T. ) ;
#50021 = FACE_OUTER_BOUND ( 'NONE', #33477, .T. ) ;
#50022 = SURFACE_STYLE_FILL_AREA ( #60528 ) ;
#50023 = CARTESIAN_POINT ( 'NONE',  ( -158.3049999999999500, 8.437984349512085203, -1.550032578732815448E-15 ) ) ;
#50024 = VERTEX_POINT ( 'NONE', #68690 ) ;
#50025 = ADVANCED_FACE ( 'NONE', ( #9259 ), #14510, .T. ) ;
#50026 = CARTESIAN_POINT ( 'NONE',  ( -71.49999999999998579, 64.07124727947029896, -7.500000000000000000 ) ) ;
#50027 = AXIS2_PLACEMENT_3D ( 'NONE', #18405, #34917, #61625 ) ;
#50028 = FACE_OUTER_BOUND ( 'NONE', #22300, .T. ) ;
#50029 = CARTESIAN_POINT ( 'NONE',  ( -9.827790563157511022E-16, 130.4429263765338192, 8.025000000000000355 ) ) ;
#50030 = CARTESIAN_POINT ( 'NONE',  ( -144.0570736234661808, 0.000000000000000000, 9.524999999999991473 ) ) ;
#50031 = EDGE_LOOP ( 'NONE', ( #49561, #21813, #21459, #15466 ) ) ;
#50032 = ORIENTED_EDGE ( 'NONE', *, *, #46911, .F. ) ;
#50033 = SURFACE_STYLE_USAGE ( .BOTH. , #1047 ) ;
#50034 = CARTESIAN_POINT ( 'NONE',  ( 0.000000000000000000, 0.000000000000000000, 42.50000000000000000 ) ) ;
#50035 = CARTESIAN_POINT ( 'NONE',  ( -83.30500000000000682, 8.437984349512085203, -1.550032578732815448E-15 ) ) ;
#50036 = ORIENTED_EDGE ( 'NONE', *, *, #13369, .F. ) ;
#50037 = SURFACE_SIDE_STYLE ('',( #7785 ) ) ;
#50038 = CARTESIAN_POINT ( 'NONE',  ( 0.000000000000000000, 0.000000000000000000, 0.7500000000000000000 ) ) ;
#50039 = CARTESIAN_POINT ( 'NONE',  ( 0.000000000000000000, 33.74999999999999289, 4.000000000000000000 ) ) ;
#50040 = PRESENTATION_LAYER_ASSIGNMENT (  '', '', ( #43354 ) ) ;
#50041 = STYLED_ITEM ( 'NONE', ( #29045 ), #8448 ) ;
#50042 = CARTESIAN_POINT ( 'NONE',  ( -75.00000000000000000, 8.592356338113649628, -6.069948737346060774 ) ) ;
#50043 = ORIENTED_EDGE ( 'NONE', *, *, #45228, .T. ) ;
#50044 = DIRECTION ( 'NONE',  ( -7.816271194327172234E-17, -0.000000000000000000, -1.000000000000000000 ) ) ;
#50046 = PRESENTATION_STYLE_ASSIGNMENT (( #38821 ) ) ;
#50045 = CARTESIAN_POINT ( 'NONE',  ( 75.00000000000000000, -2.215169945516535778E-14, 10.00000000000000000 ) ) ;
#50047 = PRESENTATION_LAYER_ASSIGNMENT (  '', '', ( #51143 ) ) ;
#50048 = CARTESIAN_POINT ( 'NONE',  ( 3.094860106618431583, 126.0949999999999847, 9.525000000000000355 ) ) ;
#50049 = CARTESIAN_POINT ( 'NONE',  ( -107.5449999999999875, -7.632228543268600340, -2.479861379858950166 ) ) ;
#50050 = EDGE_CURVE ( 'NONE', #48372, #43611, #37886, .T. ) ;
#50051 = MANIFOLD_SOLID_BREP ( 'Chamfer1', #32879 ) ;
#50052 = AXIS2_PLACEMENT_3D ( 'NONE', #55503, #50241, #65005 ) ;
#50053 = COLOUR_RGB ( '', 0.72549020, 0.75294118, 0.79215686) ;
#50055 = CARTESIAN_POINT ( 'NONE',  ( -18.30771561979323891, 11.39710497969720571, 3.763356312794146508 ) ) ;
#50054 = CARTESIAN_POINT ( 'NONE',  ( 45.65811388300841855, 10.21937129433612235, 3.999999999999999112 ) ) ;
#50056 = CARTESIAN_POINT ( 'NONE',  ( -152.5429263765338135, 9.058813317711329915, 2.943386871421369566 ) ) ;
#50057 = SURFACE_STYLE_USAGE ( .BOTH. , #17699 ) ;
#50058 = CARTESIAN_POINT ( 'NONE',  ( -164.0949999999999989, -2.607480562269071545, -8.024999999999991473 ) ) ;
#50059 =( GEOMETRIC_REPRESENTATION_CONTEXT ( 3 ) GLOBAL_UNCERTAINTY_ASSIGNED_CONTEXT ( ( #51732 ) ) GLOBAL_UNIT_ASSIGNED_CONTEXT ( ( #49375, #44141, #28920 ) ) REPRESENTATION_CONTEXT ( 'NONE', 'WORKASPACE' ) );
#50060 = ADVANCED_FACE ( 'NONE', ( #25072 ), #46579, .T. ) ;
#50061 = DIRECTION ( 'NONE',  ( 0.000000000000000000, 0.000000000000000000, 1.000000000000000000 ) ) ;
#50062 = CIRCLE ( 'NONE', #61240, 1.000000000000000888 ) ;
#50063 = ORIENTED_EDGE ( 'NONE', *, *, #36998, .F. ) ;
#50064 = EDGE_LOOP ( 'NONE', ( #4110, #49540, #21960, #67436 ) ) ;
#50065 = EDGE_CURVE ( 'NONE', #5853, #60408, #28820, .T. ) ;
#50066 = CARTESIAN_POINT ( 'NONE',  ( -63.74292637653379501, -5.598654528085803328, -7.705886871421366635 ) ) ;
#50067 = AXIS2_PLACEMENT_3D ( 'NONE', #32393, #4631, #32757 ) ;
#50068 = CARTESIAN_POINT ( 'NONE',  ( 0.000000000000000000, 14.00000000000000000, -36.49999999999999289 ) ) ;
#50069 = EDGE_CURVE ( 'NONE', #14677, #51230, #59149, .T. ) ;
#50070 = SURFACE_STYLE_FILL_AREA ( #1451 ) ;
#50071 = DIRECTION ( 'NONE',  ( 1.000000000000000000, 0.000000000000000000, 0.000000000000000000 ) ) ;
#50072 = FACE_OUTER_BOUND ( 'NONE', #55509, .T. ) ;
#50073 = DIRECTION ( 'NONE',  ( -0.000000000000000000, -0.000000000000000000, 1.000000000000000000 ) ) ;
#50074 = ADVANCED_FACE ( 'NONE', ( #26771 ), #7493, .T. ) ;
#50075 = ORIENTED_EDGE ( 'NONE', *, *, #45796, .T. ) ;
#50076 = CARTESIAN_POINT ( 'NONE',  ( -174.6550000000000011, -7.632228543268600340, -2.479861379858950166 ) ) ;
#50077 = ORIENTED_EDGE ( 'NONE', *, *, #22435, .F. ) ;
#50078 = FILL_AREA_STYLE ('',( #33530 ) ) ;
#50079 = CARTESIAN_POINT ( 'NONE',  ( 4.716976649647099507, 150.7570736234661695, -6.492361379858953008 ) ) ;
#50080 = B_SPLINE_CURVE_WITH_KNOTS ( 'NONE', 3,
 ( #68854, #31885, #36864, #58977, #58277, #20654, #52670, #15404 ),
 .UNSPECIFIED., .F., .F.,
 ( 4, 2, 2, 4 ),
 ( 0.000000000000000000, 0.0004110476197876519158, 0.0006165714296814797440, 0.0008220952395753075180 ),
 .UNSPECIFIED. ) ;
#50081 =( GEOMETRIC_REPRESENTATION_CONTEXT ( 3 ) GLOBAL_UNCERTAINTY_ASSIGNED_CONTEXT ( ( #52458 ) ) GLOBAL_UNIT_ASSIGNED_CONTEXT ( ( #27915, #14132, #62308 ) ) REPRESENTATION_CONTEXT ( 'NONE', 'WORKASPACE' ) );
#50082 = EDGE_LOOP ( 'NONE', ( #39369, #26830 ) ) ;
#50083 = DIRECTION ( 'NONE',  ( 1.000000000000000000, -0.000000000000000000, 0.000000000000000000 ) ) ;
#50084 = SURFACE_STYLE_USAGE ( .BOTH. , #28584 ) ;
#50085 = CARTESIAN_POINT ( 'NONE',  ( -83.90499999999998693, 2.607480562269069324, -8.024999999999993250 ) ) ;
#50086 = CARTESIAN_POINT ( 'NONE',  ( 19.89974874213240597, 115.4999999999999574, -10.00000000000000000 ) ) ;
#50087 = CARTESIAN_POINT ( 'NONE',  ( -3.094860106618434248, 129.9050000000000011, 9.525000000000000355 ) ) ;
#50088 = CARTESIAN_POINT ( 'NONE',  ( -118.9429263765338050, 0.000000000000000000, 9.524999999999991473 ) ) ;
#50089 = CARTESIAN_POINT ( 'NONE',  ( -47.50000000000000000, 1.797044900979284448E-15, -9.500000000000000000 ) ) ;
#50090 = CARTESIAN_POINT ( 'NONE',  ( -72.35707362346617799, 5.598654528085804216, 7.705886871421366635 ) ) ;
#50091 = CARTESIAN_POINT ( 'NONE',  ( -113.0929263765346917, 3.094860106633356978, 9.524999999989150368 ) ) ;
#50092 =( NAMED_UNIT ( * ) PLANE_ANGLE_UNIT ( ) SI_UNIT ( $, .RADIAN. ) );
#50093 = CARTESIAN_POINT ( 'NONE',  ( -113.0070736234661695, -8.102448949553174629, -5.886773742842741797 ) ) ;
#50094 = COLOUR_RGB ( '', 0.66274510, 0.83137255, 0.94901961) ;
#50095 = VERTEX_POINT ( 'NONE', #48653 ) ;
#50096 = AXIS2_PLACEMENT_3D ( 'NONE', #7330, #22461, #55850 ) ;
#50097 = SURFACE_STYLE_FILL_AREA ( #60603 ) ;
#50098 = CARTESIAN_POINT ( 'NONE',  ( -52.79499999999997328, 2.607480562269068880, -8.024999999999993250 ) ) ;
#50099 = ORIENTED_EDGE ( 'NONE', *, *, #43801, .T. ) ;
#50100 = PLANE ( 'NONE',  #191 ) ;
#50101 = CARTESIAN_POINT ( 'NONE',  ( -83.49999999999998579, 4.336808689942018722E-16, 0.000000000000000000 ) ) ;
#50102 = CARTESIAN_POINT ( 'NONE',  ( -138.2070736234667550, 3.094860106627642882, 9.524999999993303490 ) ) ;
#50103 = CARTESIAN_POINT ( 'NONE',  ( -12.74999999999999822, -4.000000000000000000, 7.000000000000001776 ) ) ;
#50104 = ORIENTED_EDGE ( 'NONE', *, *, #8275, .F. ) ;
#50105 = CARTESIAN_POINT ( 'NONE',  ( -52.68151331240365920, -10.81621879791169150, 3.669590361806503775 ) ) ;
#50106 = CARTESIAN_POINT ( 'NONE',  ( -49.64499999999999602, 4.716976649647091513, -6.492361379858946790 ) ) ;
#50107 = SPHERICAL_SURFACE ( 'NONE', #35547, 1.000000000000000000 ) ;
#50108 = VERTEX_POINT ( 'NONE', #353 ) ;
#50109 = VECTOR ( 'NONE', #8797, 1000.000000000000000 ) ;
#50110 = CARTESIAN_POINT ( 'NONE',  ( -75.00000000000000000, 8.254931070086577449, 5.606557580296888332 ) ) ;
#50111 = CARTESIAN_POINT ( 'NONE',  ( -116.4549999999999841, 7.632228543268599452, -2.479861379858951942 ) ) ;
#50112 = EDGE_LOOP ( 'NONE', ( #26715, #61034, #30052, #616 ) ) ;
#50113 = CARTESIAN_POINT ( 'NONE',  ( -7.632228543268607446, 118.6570736234661609, -2.479861379858953718 ) ) ;
#50114 =( NAMED_UNIT ( * ) SI_UNIT ( $, .STERADIAN. ) SOLID_ANGLE_UNIT ( ) );
#50115 = VECTOR ( 'NONE', #38708, 1000.000000000000000 ) ;
#50116 = DIRECTION ( 'NONE',  ( 0.000000000000000000, 0.000000000000000000, -1.000000000000000000 ) ) ;
#50117 = STYLED_ITEM ( 'NONE', ( #49010 ), #1741 ) ;
#50118 = CARTESIAN_POINT ( 'NONE',  ( -153.2070736234662149, 3.094860106618433360, 9.524999999999991473 ) ) ;
#50119 = DIRECTION ( 'NONE',  ( -1.000000000000000000, 0.000000000000000000, -0.000000000000000000 ) ) ;
#50120 = CARTESIAN_POINT ( 'NONE',  ( 3.094860106618435136, 130.2949999999999591, -9.525000000000000355 ) ) ;
#50121 = CARTESIAN_POINT ( 'NONE',  ( -81.80707362346615241, 10.01517768586948698, -1.839758294383808571E-15 ) ) ;
#50122 = CARTESIAN_POINT ( 'NONE',  ( -95.09292637653494751, 3.094860106637121522, 9.524999999986416555 ) ) ;
#50123 = ORIENTED_EDGE ( 'NONE', *, *, #55822, .F. ) ;
#50124 = CYLINDRICAL_SURFACE ( 'NONE', #49335, 0.5000000000000004441 ) ;
#50125 = DIRECTION ( 'NONE',  ( 0.000000000000000000, -1.000000000000000000, 0.000000000000000000 ) ) ;
#50126 = CARTESIAN_POINT ( 'NONE',  ( -126.8050000000000068, -8.437984349512085203, 5.166775262442717831E-16 ) ) ;
#50127 = FACE_OUTER_BOUND ( 'NONE', #16610, .T. ) ;
#50128 = SURFACE_STYLE_FILL_AREA ( #59965 ) ;
#50129 = FACE_OUTER_BOUND ( 'NONE', #27962, .T. ) ;
#50130 = CARTESIAN_POINT ( 'NONE',  ( -133.1950000000000216, 8.437984349512085203, -1.550032578732815448E-15 ) ) ;
#50131 = EDGE_CURVE ( 'NONE', #38290, #19166, #43716, .T. ) ;
#50132 = CARTESIAN_POINT ( 'NONE',  ( -132.7450000000000045, 4.716976649647094177, 6.492361379858945902 ) ) ;
#50133 = DIRECTION ( 'NONE',  ( 0.000000000000000000, 0.000000000000000000, 1.000000000000000000 ) ) ;
#50134 = ORIENTED_EDGE ( 'NONE', *, *, #27445, .F. ) ;
#50135 = EDGE_CURVE ( 'NONE', #20601, #47060, #18706, .T. ) ;
#50136 = CARTESIAN_POINT ( 'NONE',  ( 47.50000000000000000, 99.99999999999992895, 10.00000000000000000 ) ) ;
#50137 = MECHANICAL_DESIGN_GEOMETRIC_PRESENTATION_REPRESENTATION (  '', ( #61349 ), #64733 ) ;
#50138 = DIRECTION ( 'NONE',  ( 0.000000000000000000, 0.000000000000000000, -1.000000000000000000 ) ) ;
#50139 = CARTESIAN_POINT ( 'NONE',  ( -179.3929263765337794, 8.102448949553176405, 5.886773742842740909 ) ) ;
#50140 = CARTESIAN_POINT ( 'NONE',  ( -49.94499999999998607, -9.827790563157499189E-16, -8.024999999999991473 ) ) ;
#50141 = EDGE_CURVE ( 'NONE', #61874, #47060, #54634, .T. ) ;
#50142 = CARTESIAN_POINT ( 'NONE',  ( -34.99999999999999289, 99.99999999999998579, -4.000000000000000000 ) ) ;
#50143 = CARTESIAN_POINT ( 'NONE',  ( 71.49999999999998579, 64.07124727947029896, 10.00000000000000000 ) ) ;
#50144 = ADVANCED_FACE ( 'NONE', ( #43038 ), #32773, .T. ) ;
#50145 =( GEOMETRIC_REPRESENTATION_CONTEXT ( 3 ) GLOBAL_UNCERTAINTY_ASSIGNED_CONTEXT ( ( #3166 ) ) GLOBAL_UNIT_ASSIGNED_CONTEXT ( ( #64161, #26177, #69 ) ) REPRESENTATION_CONTEXT ( 'NONE', 'WORKASPACE' ) );
#50146 = FACE_OUTER_BOUND ( 'NONE', #13111, .T. ) ;
#50147 = CARTESIAN_POINT ( 'NONE',  ( -15.98999599679679839, 146.4999999999999716, 7.500000000000000000 ) ) ;
#50148 = UNCERTAINTY_MEASURE_WITH_UNIT (LENGTH_MEASURE( 1.000000000000000082E-05 ), #17944, 'distance_accuracy_value', 'NONE');
#50149 = CARTESIAN_POINT ( 'NONE',  ( -97.94292637653380496, 0.000000000000000000, 9.524999999999991473 ) ) ;
#50150 = PRODUCT_CONTEXT ( 'NONE', #29818, 'mechanical' ) ;
#50151 = FILL_AREA_STYLE_COLOUR ( '', #22223 ) ;
#50152 = CARTESIAN_POINT ( 'NONE',  ( -162.0570736234661808, 0.000000000000000000, 9.524999999999991473 ) ) ;
#50153 = EDGE_CURVE ( 'NONE', #46287, #12301, #51039, .T. ) ;
#50154 = DIRECTION ( 'NONE',  ( 0.000000000000000000, 0.000000000000000000, 1.000000000000000000 ) ) ;
#50155 = CARTESIAN_POINT ( 'NONE',  ( 44.25000000000000000, 21.74999999999998579, -3.750000000000000000 ) ) ;
#50156 = CARTESIAN_POINT ( 'NONE',  ( -41.27272961514525917, 107.3325180337009215, 3.464233254638040549 ) ) ;
#50157 = VECTOR ( 'NONE', #48899, 1000.000000000000000 ) ;
#50158 = FILL_AREA_STYLE ('',( #28661 ) ) ;
#50159 = ORIENTED_EDGE ( 'NONE', *, *, #49802, .T. ) ;
#50160 = DIRECTION ( 'NONE',  ( 0.000000000000000000, 0.000000000000000000, -1.000000000000000000 ) ) ;
#50161 = MANIFOLD_SOLID_BREP ( 'Boss-Extrude1', #3655 ) ;
#50162 = ORIENTED_EDGE ( 'NONE', *, *, #3541, .F. ) ;
#50163 = DIRECTION ( 'NONE',  ( 0.000000000000000000, 0.000000000000000000, 1.000000000000000000 ) ) ;
#50164 = CARTESIAN_POINT ( 'NONE',  ( 7.632228543268608334, 123.4570736234661581, -2.479861379858951942 ) ) ;
#50165 = SURFACE_STYLE_FILL_AREA ( #7242 ) ;
#50166 = FACE_OUTER_BOUND ( 'NONE', #47167, .T. ) ;
#50167 = FACE_OUTER_BOUND ( 'NONE', #61836, .T. ) ;
#50168 = EDGE_LOOP ( 'NONE', ( #16616, #7811, #41404, #52673 ) ) ;
#50169 = CARTESIAN_POINT ( 'NONE',  ( -115.7070736234670250, -3.094860106632346675, -9.524999999989880450 ) ) ;
#50170 = SURFACE_STYLE_USAGE ( .BOTH. , #6519 ) ;
#50171 = VERTEX_POINT ( 'NONE', #28512 ) ;
#50172 = CARTESIAN_POINT ( 'NONE',  ( 71.49999999999998579, 64.07124727947029896, -9.500000000000000000 ) ) ;
#50173 = DIRECTION ( 'NONE',  ( 0.000000000000000000, 0.000000000000000000, 1.000000000000000000 ) ) ;
#50174 = CARTESIAN_POINT ( 'NONE',  ( -95.39499999999999602, -6.826472737025115478, -4.959722759717899443 ) ) ;
#50175 = ORIENTED_EDGE ( 'NONE', *, *, #62379, .F. ) ;
#50176 = EDGE_CURVE ( 'NONE', #3393, #31013, #18340, .T. ) ;
#50177 = FILL_AREA_STYLE_COLOUR ( '', #27691 ) ;
#50178 = VERTEX_POINT ( 'NONE', #8484 ) ;
#50179 =( LENGTH_UNIT ( ) NAMED_UNIT ( * ) SI_UNIT ( .MILLI., .METRE. ) );
#50180 = DIRECTION ( 'NONE',  ( 0.000000000000000000, 0.000000000000000000, -1.000000000000000000 ) ) ;
#50181 = STYLED_ITEM ( 'NONE', ( #44600 ), #64946 ) ;
#50182 = SURFACE_STYLE_USAGE ( .BOTH. , #23100 ) ;
#50183 = ORIENTED_EDGE ( 'NONE', *, *, #56549, .F. ) ;
#50184 = CARTESIAN_POINT ( 'NONE',  ( 45.50000000000000000, -1.414600137340999687E-14, -7.000000000000000888 ) ) ;
#50185 = EDGE_LOOP ( 'NONE', ( #18207, #55356, #36928, #60367 ) ) ;
#50186 = LINE ( 'NONE', #13925, #2649 ) ;
#50187 = DIRECTION ( 'NONE',  ( 0.000000000000000000, -1.000000000000000000, 0.000000000000000000 ) ) ;
#50188 = CARTESIAN_POINT ( 'NONE',  ( -178.7070736234661581, -3.094860106618431139, -9.524999999999991473 ) ) ;
#50189 = LINE ( 'NONE', #27990, #2747 ) ;
#50190 = LINE ( 'NONE', #66344, #2622 ) ;
#50191 = CARTESIAN_POINT ( 'NONE',  ( -117.3570736234661780, 5.598654528085804216, 7.705886871421366635 ) ) ;
#50192 = SURFACE_SIDE_STYLE ('',( #34679 ) ) ;
#50193 = CARTESIAN_POINT ( 'NONE',  ( 3.414213562373124677, 42.99999999999999289, 79.58981420056515788 ) ) ;
#50194 = ORIENTED_EDGE ( 'NONE', *, *, #13495, .T. ) ;
#50195 =( BOUNDED_CURVE ( )  B_SPLINE_CURVE ( 2, ( #27250, #5448, #809, #48437, #16426 ),
 .UNSPECIFIED., .F., .F. ) 
 B_SPLINE_CURVE_WITH_KNOTS ( ( 3, 2, 3 ),
 ( 0.8529411764705880916, 0.8588235294117646523, 0.8616293943929277388 ),
 .UNSPECIFIED. ) 
 CURVE ( )  GEOMETRIC_REPRESENTATION_ITEM ( )  RATIONAL_B_SPLINE_CURVE ( ( 1.000000000000000888, 0.9510565162951526430, 1.000000000000000000, 0.9766541028127959656, 0.9755800536518708377 ) ) 
 REPRESENTATION_ITEM ( '' )  );
#50196 = CARTESIAN_POINT ( 'NONE',  ( 6.021969435454494146, -1.863712308906143589, -7.569642976165943615 ) ) ;
#50197 = DIRECTION ( 'NONE',  ( -1.156482317317873451E-16, -1.000000000000000000, 0.000000000000000000 ) ) ;
#50198 = ADVANCED_FACE ( 'NONE', ( #24287 ), #60518, .T. ) ;
#50199 = CARTESIAN_POINT ( 'NONE',  ( 44.99999999999977973, 149.4999999999999716, -9.500000000000000000 ) ) ;
#50201 = EDGE_LOOP ( 'NONE', ( #30968, #41186, #12971 ) ) ;
#50200 = MECHANICAL_DESIGN_GEOMETRIC_PRESENTATION_REPRESENTATION (  '', ( #4067 ), #60275 ) ;
#50202 = CARTESIAN_POINT ( 'NONE',  ( -160.7049999999999841, 2.607480562269073321, 8.024999999999991473 ) ) ;
#50203 = EDGE_CURVE ( 'NONE', #62287, #24376, #39821, .T. ) ;
#50204 = CARTESIAN_POINT ( 'NONE',  ( 34.99999999999992895, 112.4999999999999858, -9.500000000000000000 ) ) ;
#50205 = LINE ( 'NONE', #1925, #51530 ) ;
#50206 = CARTESIAN_POINT ( 'NONE',  ( -160.4949999999999761, 6.826472737025113702, -4.959722759717902107 ) ) ;
#50207 = CARTESIAN_POINT ( 'NONE',  ( -155.6949999999999932, -8.437984349512086979, 5.166775262442717831E-16 ) ) ;
#50208 = EDGE_LOOP ( 'NONE', ( #62295, #48900, #43044, #11243 ) ) ;
#50209 = EDGE_CURVE ( 'NONE', #25180, #19879, #45690, .T. ) ;
#50210 = CARTESIAN_POINT ( 'NONE',  ( 60.00000000000000000, -2.024042244987997205E-14, 9.500000000000000000 ) ) ;
#50211 = AXIS2_PLACEMENT_3D ( 'NONE', #9773, #31182, #47436 ) ;
#50212 = CYLINDRICAL_SURFACE ( 'NONE', #66019, 0.5000000000000004441 ) ;
#50213 = CARTESIAN_POINT ( 'NONE',  ( -162.4429263765338192, -1.166476076187852838E-15, -9.524999999999991473 ) ) ;
#50214 = CARTESIAN_POINT ( 'NONE',  ( -78.05499999999997840, -9.827790563157499189E-16, -8.024999999999991473 ) ) ;
#50215 = CARTESIAN_POINT ( 'NONE',  ( 23.50000000000001776, 24.55989583710066171, 27.18999999999999062 ) ) ;
#50216 =( LENGTH_UNIT ( ) NAMED_UNIT ( * ) SI_UNIT ( .MILLI., .METRE. ) );
#50217 = CARTESIAN_POINT ( 'NONE',  ( -70.04499999999998749, 7.632228543268600340, 2.479861379858949277 ) ) ;
#50218 = CARTESIAN_POINT ( 'NONE',  ( 8.102448949553181734, 142.5049999999999955, 5.886773742842750679 ) ) ;
#50219 = EDGE_CURVE ( 'NONE', #52874, #31166, #3630, .T. ) ;
#50220 = SURFACE_SIDE_STYLE ('',( #11529 ) ) ;
#50221 = UNCERTAINTY_MEASURE_WITH_UNIT (LENGTH_MEASURE( 1.000000000000000082E-05 ), #55025, 'distance_accuracy_value', 'NONE');
#50222 = LINE ( 'NONE', #66377, #1156 ) ;
#50223 = ADVANCED_FACE ( 'NONE', ( #65829 ), #33804, .T. ) ;
#50224 = CARTESIAN_POINT ( 'NONE',  ( -57.51969600708471830, 0.000000000000000000, -3.499999999999999112 ) ) ;
#50225 = FILL_AREA_STYLE_COLOUR ( '', #55057 ) ;
#50226 =( GEOMETRIC_REPRESENTATION_CONTEXT ( 3 ) GLOBAL_UNCERTAINTY_ASSIGNED_CONTEXT ( ( #891 ) ) GLOBAL_UNIT_ASSIGNED_CONTEXT ( ( #17075, #12099, #49761 ) ) REPRESENTATION_CONTEXT ( 'NONE', 'WORKASPACE' ) );
#50227 = LINE ( 'NONE', #60405, #42826 ) ;
#50228 = MECHANICAL_DESIGN_GEOMETRIC_PRESENTATION_REPRESENTATION (  '', ( #34452 ), #42394 ) ;
#50229 = CARTESIAN_POINT ( 'NONE',  ( 13.25000000000000355, 27.74999999999998934, -4.000000000000000000 ) ) ;
#50230 = MECHANICAL_DESIGN_GEOMETRIC_PRESENTATION_REPRESENTATION (  '', ( #51337 ), #40120 ) ;
#50231 = VERTEX_POINT ( 'NONE', #68605 ) ;
#50232 = EDGE_LOOP ( 'NONE', ( #27790, #10820, #51440, #64615 ) ) ;
#50233 = CARTESIAN_POINT ( 'NONE',  ( -15.98999599679679839, 146.4999999999999716, -9.500000000000000000 ) ) ;
#50234 = FILL_AREA_STYLE_COLOUR ( '', #111 ) ;
#50235 = FILL_AREA_STYLE ('',( #29079 ) ) ;
#50236 = FILL_AREA_STYLE ('',( #7324 ) ) ;
#50237 = DIRECTION ( 'NONE',  ( -1.000000000000000000, 0.000000000000000000, 0.000000000000000000 ) ) ;
#50238 = ORIENTED_EDGE ( 'NONE', *, *, #22503, .T. ) ;
#50239 = CARTESIAN_POINT ( 'NONE',  ( -101.4549999999999841, 7.632228543268599452, -2.479861379858951942 ) ) ;
#50240 = ORIENTED_EDGE ( 'NONE', *, *, #62228, .T. ) ;
#50241 = DIRECTION ( 'NONE',  ( 0.000000000000000000, 1.000000000000000000, -0.000000000000000000 ) ) ;
#50242 = CIRCLE ( 'NONE', #15421, 27.49999999999999645 ) ;
#50243 = FACE_OUTER_BOUND ( 'NONE', #43974, .T. ) ;
#50244 = ORIENTED_EDGE ( 'NONE', *, *, #53577, .T. ) ;
#50245 = FACE_OUTER_BOUND ( 'NONE', #23571, .T. ) ;
#50246 = ORIENTED_EDGE ( 'NONE', *, *, #49443, .T. ) ;
#50247 = DIRECTION ( 'NONE',  ( -0.000000000000000000, -1.000000000000000000, -0.000000000000000000 ) ) ;
#50248 = CARTESIAN_POINT ( 'NONE',  ( 8.250000000000001776, 31.24999999999998579, -3.750000000000000000 ) ) ;
#50249 = ORIENTED_EDGE ( 'NONE', *, *, #27819, .T. ) ;
#50250 = EDGE_CURVE ( 'NONE', #45861, #2564, #3482, .T. ) ;
#50251 = VERTEX_POINT ( 'NONE', #30592 ) ;
#50252 = FILL_AREA_STYLE_COLOUR ( '', #22055 ) ;
#50253 = PRESENTATION_STYLE_ASSIGNMENT (( #66415 ) ) ;
#50254 = CYLINDRICAL_SURFACE ( 'NONE', #47669, 0.5000000000000004441 ) ;
#50255 = ORIENTED_EDGE ( 'NONE', *, *, #57023, .F. ) ;
#50256 = CARTESIAN_POINT ( 'NONE',  ( -2.607480562269075097, 133.2929263765338135, 8.025000000000000355 ) ) ;
#50257 = CARTESIAN_POINT ( 'NONE',  ( 1.000000000000000000, 42.00000000000000000, -79.00402776293826435 ) ) ;
#50258 = FACE_OUTER_BOUND ( 'NONE', #32504, .T. ) ;
#50259 = DIRECTION ( 'NONE',  ( -0.000000000000000000, -0.000000000000000000, -1.000000000000000000 ) ) ;
#50260 = DIRECTION ( 'NONE',  ( -1.000000000000000000, 0.000000000000000000, 0.000000000000000000 ) ) ;
#50261 = VERTEX_POINT ( 'NONE', #35560 ) ;
#50262 = FILL_AREA_STYLE ('',( #11927 ) ) ;
#50263 = ORIENTED_EDGE ( 'NONE', *, *, #8845, .T. ) ;
#50264 = DIRECTION ( 'NONE',  ( 1.000000000000000000, 0.000000000000000000, 0.000000000000000000 ) ) ;
#50265 = CARTESIAN_POINT ( 'NONE',  ( -12.72792206135785698, 149.9999999999999716, 10.50000000000000000 ) ) ;
#50266 = PRESENTATION_STYLE_ASSIGNMENT (( #17249 ) ) ;
#50267 = CARTESIAN_POINT ( 'NONE',  ( -137.0049999999999670, 6.826472737025116366, 4.959722759717898555 ) ) ;
#50268 = DIRECTION ( 'NONE',  ( 0.000000000000000000, 1.000000000000000000, -0.000000000000000000 ) ) ;
#50269 = DIRECTION ( 'NONE',  ( 1.000000000000000000, 0.000000000000000000, 0.000000000000000000 ) ) ;
#50270 = ORIENTED_EDGE ( 'NONE', *, *, #14223, .F. ) ;
#50271 = EDGE_CURVE ( 'NONE', #19853, #20918, #8655, .T. ) ;
#50272 = DIRECTION ( 'NONE',  ( 0.000000000000000000, 0.000000000000000000, -1.000000000000000000 ) ) ;
#50273 = EDGE_CURVE ( 'NONE', #54371, #39475, #29764, .T. ) ;
#50274 = CARTESIAN_POINT ( 'NONE',  ( -156.4429263765338192, -1.166476076187852838E-15, -9.524999999999991473 ) ) ;
#50275 = ORIENTED_EDGE ( 'NONE', *, *, #39642, .T. ) ;
#50276 = MECHANICAL_DESIGN_GEOMETRIC_PRESENTATION_REPRESENTATION (  '', ( #33397 ), #30023 ) ;
#50277 = ORIENTED_EDGE ( 'NONE', *, *, #69176, .F. ) ;
#50278 = CARTESIAN_POINT ( 'NONE',  ( -30.82866448558605299, -8.500000000000099476, -0.2278223570949065857 ) ) ;
#50279 = ADVANCED_FACE ( 'NONE', ( #52781 ), #57342, .T. ) ;
#50280 = CARTESIAN_POINT ( 'NONE',  ( -50.30499999999999261, 8.437984349512085203, -1.550032578732815448E-15 ) ) ;
#50281 = ORIENTED_EDGE ( 'NONE', *, *, #56214, .T. ) ;
#50282 = PRESENTATION_STYLE_ASSIGNMENT (( #41138 ) ) ;
#50283 = CARTESIAN_POINT ( 'NONE',  ( -28.74999999999999645, -8.499999999999996447, 11.89999999999999680 ) ) ;
#50284 = ADVANCED_FACE ( 'NONE', ( #25331 ), #51766, .T. ) ;
#50285 = AXIS2_PLACEMENT_3D ( 'NONE', #58742, #54134, #22489 ) ;
#50286 = CARTESIAN_POINT ( 'NONE',  ( -182.6949999999999648, -8.437984349512086979, 5.166775262442717831E-16 ) ) ;
#50287 = CYLINDRICAL_SURFACE ( 'NONE', #21920, 0.2500000000000002220 ) ;
#50288 = VERTEX_POINT ( 'NONE', #32953 ) ;
#50289 = CARTESIAN_POINT ( 'NONE',  ( -74.99027199483633410, 35.52740363875328455, -9.609103569194060057 ) ) ;
#50290 = EDGE_CURVE ( 'NONE', #32986, #52357, #54683, .T. ) ;
#50291 = CYLINDRICAL_SURFACE ( 'NONE', #69475, 16.94999999999999218 ) ;
#50292 = CARTESIAN_POINT ( 'NONE',  ( -48.00000000000000000, 14.49137674618942562, 10.00000000000000000 ) ) ;
#50293 = CARTESIAN_POINT ( 'NONE',  ( -59.14773785255846406, -8.499999999999992895, 0.8380523509896478096 ) ) ;
#50295 = DIRECTION ( 'NONE',  ( -0.000000000000000000, -0.000000000000000000, -1.000000000000000000 ) ) ;
#50294 = MECHANICAL_DESIGN_GEOMETRIC_PRESENTATION_REPRESENTATION (  '', ( #49194 ), #35688 ) ;
#50296 = EDGE_CURVE ( 'NONE', #62390, #64972, #18153, .T. ) ;
#50297 = CIRCLE ( 'NONE', #13209, 8.999999999999994671 ) ;
#50298 = CARTESIAN_POINT ( 'NONE',  ( -104.5449999999999875, -7.632228543268600340, -2.479861379858950166 ) ) ;
#50299 = CARTESIAN_POINT ( 'NONE',  ( 5.598654528085809545, 122.2549999999999955, -7.705886871421373741 ) ) ;
#50300 = CARTESIAN_POINT ( 'NONE',  ( -78.29499999999997328, -2.607480562269069768, 8.024999999999991473 ) ) ;
#50301 = CARTESIAN_POINT ( 'NONE',  ( -22.25000000000000711, 33.99999999999999289, -3.750000000000000000 ) ) ;
#50302 = LINE ( 'NONE', #22526, #4678 ) ;
#50303 = CARTESIAN_POINT ( 'NONE',  ( -74.99999999999998579, 50.00000000000000000, -41.30495168499704306 ) ) ;
#50304 = FACE_OUTER_BOUND ( 'NONE', #49997, .T. ) ;
#50305 = UNCERTAINTY_MEASURE_WITH_UNIT (LENGTH_MEASURE( 1.000000000000000082E-05 ), #9617, 'distance_accuracy_value', 'NONE');
#50306 = DIRECTION ( 'NONE',  ( 1.000000000000000000, 0.000000000000000000, 0.000000000000000000 ) ) ;
#50307 = CARTESIAN_POINT ( 'NONE',  ( -71.49999999999998579, 64.07124727947029896, -7.000000000000000000 ) ) ;
#50308 = ORIENTED_EDGE ( 'NONE', *, *, #67041, .T. ) ;
#50309 = CARTESIAN_POINT ( 'NONE',  ( -114.4429263765338050, -1.166476076187852838E-15, -9.524999999999991473 ) ) ;
#50310 = CARTESIAN_POINT ( 'NONE',  ( -135.5949999999999989, 2.607480562269073321, 8.024999999999991473 ) ) ;
#50311 = DIRECTION ( 'NONE',  ( -0.000000000000000000, -1.000000000000000000, -0.000000000000000000 ) ) ;
#50312 = CARTESIAN_POINT ( 'NONE',  ( -4.683753779217435742, 5.887500484252664812, 0.4948905776603345075 ) ) ;
#50313 = DIRECTION ( 'NONE',  ( 0.000000000000000000, 0.000000000000000000, 1.000000000000000000 ) ) ;
#50314 = ORIENTED_EDGE ( 'NONE', *, *, #4417, .T. ) ;
#50315 = ORIENTED_EDGE ( 'NONE', *, *, #48578, .T. ) ;
#50316 = EDGE_CURVE ( 'NONE', #8462, #5088, #68215, .T. ) ;
#50317 = CARTESIAN_POINT ( 'NONE',  ( -29.42522945561020364, -7.714901950938580555, -0.5387317027069097319 ) ) ;
#50318 = CARTESIAN_POINT ( 'NONE',  ( 5.196152422706629359, 9.000000000000008882, 7.500000000000000000 ) ) ;
#50319 =( BOUNDED_CURVE ( )  B_SPLINE_CURVE ( 2, ( #44825, #11031, #38163, #59565, #54640, #32478, #11385, #6793, #27876, #1103, #53940 ),
 .UNSPECIFIED., .F., .F. ) 
 B_SPLINE_CURVE_WITH_KNOTS ( ( 3, 2, 2, 2, 2, 3 ),
 ( 0.5000000000000002220, 0.5058823529411766717, 0.5117647058823531214, 0.5176470588235296821, 0.5235294117647061318, 0.5294117647058825815 ),
 .UNSPECIFIED. ) 
 CURVE ( )  GEOMETRIC_REPRESENTATION_ITEM ( )  RATIONAL_B_SPLINE_CURVE ( ( 0.9999999999999981126, 0.9510565162951554186, 1.000000000000000000, 0.9510565162951535312, 1.000000000000000000, 0.9510565162951535312, 1.000000000000000000, 0.9510565162951535312, 1.000000000000000000, 0.9510565162951516438, 1.000000000000001776 ) ) 
 REPRESENTATION_ITEM ( '' )  );
#50320 =( GEOMETRIC_REPRESENTATION_CONTEXT ( 3 ) GLOBAL_UNCERTAINTY_ASSIGNED_CONTEXT ( ( #34025 ) ) GLOBAL_UNIT_ASSIGNED_CONTEXT ( ( #30271, #52132, #15206 ) ) REPRESENTATION_CONTEXT ( 'NONE', 'WORKASPACE' ) );
#50321 = LINE ( 'NONE', #28124, #4486 ) ;
#50322 = VECTOR ( 'NONE', #44842, 1000.000000000000114 ) ;
#50323 = DIRECTION ( 'NONE',  ( -1.000000000000000000, -0.000000000000000000, -0.000000000000000000 ) ) ;
#50325 =( NAMED_UNIT ( * ) SI_UNIT ( $, .STERADIAN. ) SOLID_ANGLE_UNIT ( ) );
#50324 = AXIS2_PLACEMENT_3D ( 'NONE', #68448, #58935, #69478 ) ;
#50326 = ORIENTED_EDGE ( 'NONE', *, *, #33983, .T. ) ;
#50327 = CARTESIAN_POINT ( 'NONE',  ( -130.2549999999999955, -4.716976649647092401, 6.492361379858946790 ) ) ;
#50328 = EDGE_LOOP ( 'NONE', ( #16631, #41102, #22575, #39879 ) ) ;
#50329 = VERTEX_POINT ( 'NONE', #54722 ) ;
#50330 = PRESENTATION_STYLE_ASSIGNMENT (( #28846 ) ) ;
#50331 = VERTEX_POINT ( 'NONE', #39633 ) ;
#50332 = STYLED_ITEM ( 'NONE', ( #30820 ), #13999 ) ;
#50333 = SURFACE_STYLE_FILL_AREA ( #66141 ) ;
#50334 = CARTESIAN_POINT ( 'NONE',  ( 9.058813317711337021, 141.5449999999999875, 2.943386871421375783 ) ) ;
#50335 = ORIENTED_EDGE ( 'NONE', *, *, #57769, .T. ) ;
#50336 = PRESENTATION_STYLE_ASSIGNMENT (( #7432 ) ) ;
#50337 = CARTESIAN_POINT ( 'NONE',  ( -10.01517768586949408, 138.3049999999999500, -6.132527647946036459E-16 ) ) ;
#50338 = CARTESIAN_POINT ( 'NONE',  ( -52.40499999999997982, -2.607480562269069768, 8.024999999999991473 ) ) ;
#50339 = FACE_OUTER_BOUND ( 'NONE', #55847, .T. ) ;
#50340 = EDGE_LOOP ( 'NONE', ( #1291, #19979, #45278, #6392 ) ) ;
#50341 = CARTESIAN_POINT ( 'NONE',  ( -3.094860106618432471, 155.7049999999999841, -9.525000000000000355 ) ) ;
#50342 = FACE_OUTER_BOUND ( 'NONE', #3361, .T. ) ;
#50343 = UNCERTAINTY_MEASURE_WITH_UNIT (LENGTH_MEASURE( 1.000000000000000082E-05 ), #22193, 'distance_accuracy_value', 'NONE');
#50344 = PRESENTATION_LAYER_ASSIGNMENT (  '', '', ( #31230 ) ) ;
#50345 = CIRCLE ( 'NONE', #47017, 0.2500000000000002220 ) ;
#50346 = CARTESIAN_POINT ( 'NONE',  ( 0.000000000000000000, 0.000000000000000000, 1.000000000000000000 ) ) ;
#50347 = VERTEX_POINT ( 'NONE', #54387 ) ;
#50348 = LINE ( 'NONE', #1028, #57581 ) ;
#50349 = ORIENTED_EDGE ( 'NONE', *, *, #47735, .T. ) ;
#50350 = CARTESIAN_POINT ( 'NONE',  ( 0.000000000000000000, 87.30187232391182306, 8.025000000000000355 ) ) ;
#50351 = FILL_AREA_STYLE ('',( #23269 ) ) ;
#50352 = CARTESIAN_POINT ( 'NONE',  ( -49.99277014337361891, -10.94657273824542187, 3.697228369969763673 ) ) ;
#50353 = CARTESIAN_POINT ( 'NONE',  ( -164.4549999999999841, 7.632228543268599452, -2.479861379858951942 ) ) ;
#50354 = ORIENTED_EDGE ( 'NONE', *, *, #23912, .F. ) ;
#50355 = FACE_OUTER_BOUND ( 'NONE', #34048, .T. ) ;
#50356 = UNCERTAINTY_MEASURE_WITH_UNIT (LENGTH_MEASURE( 1.000000000000000082E-05 ), #50179, 'distance_accuracy_value', 'NONE');
#50357 = EDGE_CURVE ( 'NONE', #41509, #38350, #33351, .T. ) ;
#50358 = CARTESIAN_POINT ( 'NONE',  ( 60.00000000000000000, 1.797044900979284448E-15, -10.49999999999999822 ) ) ;
#50359 = PRESENTATION_STYLE_ASSIGNMENT (( #13759 ) ) ;
#50360 = VERTEX_POINT ( 'NONE', #59662 ) ;
#50361 = ORIENTED_EDGE ( 'NONE', *, *, #9064, .F. ) ;
#50362 = DIRECTION ( 'NONE',  ( 0.000000000000000000, 1.000000000000000000, -0.000000000000000000 ) ) ;
#50364 = EDGE_CURVE ( 'NONE', #8679, #11393, #64790, .T. ) ;
#50363 = CYLINDRICAL_SURFACE ( 'NONE', #18944, 5.000000000000000000 ) ;
#50365 = CARTESIAN_POINT ( 'NONE',  ( -72.35499999999998977, -4.716976649647093289, -6.492361379858945902 ) ) ;
#50366 = EDGE_LOOP ( 'NONE', ( #24202, #61176, #16979, #23512 ) ) ;
#50367 = LINE ( 'NONE', #9200, #57601 ) ;
#50368 = CARTESIAN_POINT ( 'NONE',  ( 6.000000000000017764, 43.00000000000000000, -29.49447654986460776 ) ) ;
#50369 =( NAMED_UNIT ( * ) PLANE_ANGLE_UNIT ( ) SI_UNIT ( $, .RADIAN. ) );
#50370 = AXIS2_PLACEMENT_3D ( 'NONE', #33716, #30159, #24892 ) ;
#50371 = ORIENTED_EDGE ( 'NONE', *, *, #43345, .F. ) ;
#50372 = SURFACE_SIDE_STYLE ('',( #12035 ) ) ;
#50373 =( GEOMETRIC_REPRESENTATION_CONTEXT ( 3 ) GLOBAL_UNCERTAINTY_ASSIGNED_CONTEXT ( ( #37018 ) ) GLOBAL_UNIT_ASSIGNED_CONTEXT ( ( #49008, #22582, #27820 ) ) REPRESENTATION_CONTEXT ( 'NONE', 'WORKASPACE' ) );
#50374 = DIRECTION ( 'NONE',  ( 0.000000000000000000, 1.000000000000000000, 0.000000000000000000 ) ) ;
#50375 = COLOUR_RGB ( '', 0.08235294, 0.09019608, 0.10196078) ;
#50376 = EDGE_CURVE ( 'NONE', #17255, #53011, #33296, .T. ) ;
#50377 = CARTESIAN_POINT ( 'NONE',  ( 5.598654528085809545, 142.1449999999999818, -7.705886871421373741 ) ) ;
#50378 = CARTESIAN_POINT ( 'NONE',  ( -109.1949999999999648, 8.437984349512085203, -1.550032578732815448E-15 ) ) ;
#50379 = MANIFOLD_SOLID_BREP ( 'Boss-Extrude1', #26135 ) ;
#50380 = AXIS2_PLACEMENT_3D ( 'NONE', #56434, #62410, #18121 ) ;
#50381 = FACE_OUTER_BOUND ( 'NONE', #84, .T. ) ;
#50382 = VECTOR ( 'NONE', #30497, 1000.000000000000000 ) ;
#50384 = CARTESIAN_POINT ( 'NONE',  ( -19.73190520809190929, 11.89070917026893603, 1.623664015870753596 ) ) ;
#50383 = CYLINDRICAL_SURFACE ( 'NONE', #68318, 0.2500000000000002220 ) ;
#50385 = CARTESIAN_POINT ( 'NONE',  ( -153.2929263765337566, 3.094860106618428031, -9.524999999999993250 ) ) ;
#50386 = CARTESIAN_POINT ( 'NONE',  ( -169.1949999999999932, 8.437984349512085203, -1.550032578732815448E-15 ) ) ;
#50387 = AXIS2_PLACEMENT_3D ( 'NONE', #60804, #65766, #39407 ) ;
#50388 = ADVANCED_FACE ( 'NONE', ( #38956 ), #38617, .T. ) ;
#50389 = FILL_AREA_STYLE_COLOUR ( '', #65823 ) ;
#50390 = VERTEX_POINT ( 'NONE', #27287 ) ;
#50391 = CARTESIAN_POINT ( 'NONE',  ( -4.716976649647097730, 127.3570736234661496, -6.492361379858953896 ) ) ;
#50392 = ORIENTED_EDGE ( 'NONE', *, *, #19452, .F. ) ;
#50393 = CARTESIAN_POINT ( 'NONE',  ( -69.14292637653379359, 5.598654528085800663, -7.705886871421367523 ) ) ;
#50394 = ADVANCED_FACE ( 'NONE', ( #1569 ), #48825, .F. ) ;
#50395 = DIRECTION ( 'NONE',  ( -0.000000000000000000, 1.000000000000000000, 0.000000000000000000 ) ) ;
#50396 = CIRCLE ( 'NONE', #35781, 0.2500000000000002220 ) ;
#50397 = CARTESIAN_POINT ( 'NONE',  ( -48.81081081081080697, 14.09971791521133255, 7.000000000000000000 ) ) ;
#50398 = PRESENTATION_STYLE_ASSIGNMENT (( #18039 ) ) ;
#50399 = SURFACE_SIDE_STYLE ('',( #22630 ) ) ;
#50400 = CIRCLE ( 'NONE', #57121, 0.7499999999999997780 ) ;
#50401 = VERTEX_POINT ( 'NONE', #68095 ) ;
#50402 = CARTESIAN_POINT ( 'NONE',  ( -173.7549999999999955, 4.716976649647091513, -6.492361379858946790 ) ) ;
#50403 = VERTEX_POINT ( 'NONE', #39992 ) ;
#50404 = DIRECTION ( 'NONE',  ( 0.000000000000000000, 0.000000000000000000, 1.000000000000000000 ) ) ;
#50405 = FILL_AREA_STYLE ('',( #34226 ) ) ;
#50406 = PRESENTATION_STYLE_ASSIGNMENT (( #43782 ) ) ;
#50407 = STYLED_ITEM ( 'NONE', ( #32315 ), #10177 ) ;
#50408 = CARTESIAN_POINT ( 'NONE',  ( -75.50000000000000000, -6.499999999999992006, 21.00000000000000000 ) ) ;
#50409 = CARTESIAN_POINT ( 'NONE',  ( 4.716976649647096842, 155.8570736234661638, 6.492361379858953896 ) ) ;
#50410 = STYLED_ITEM ( 'NONE', ( #35031 ), #4408 ) ;
#50411 = VERTEX_POINT ( 'NONE', #46310 ) ;
#50412 =( NAMED_UNIT ( * ) PLANE_ANGLE_UNIT ( ) SI_UNIT ( $, .RADIAN. ) );
#50413 = CARTESIAN_POINT ( 'NONE',  ( 8.102448949553179958, 115.5049999999999812, 5.886773742842750679 ) ) ;
#50414 = CARTESIAN_POINT ( 'NONE',  ( -83.75499999999998124, 4.716976649647091513, -6.492361379858946790 ) ) ;
#50415 = DIRECTION ( 'NONE',  ( 0.000000000000000000, 0.000000000000000000, -1.000000000000000000 ) ) ;
#50416 = CARTESIAN_POINT ( 'NONE',  ( -8.102448949553181734, 132.0049999999999386, -5.886773742842749790 ) ) ;
#50417 = UNCERTAINTY_MEASURE_WITH_UNIT (LENGTH_MEASURE( 1.000000000000000082E-05 ), #52037, 'distance_accuracy_value', 'NONE');
#50418 = CARTESIAN_POINT ( 'NONE',  ( 8.437984349512095861, 132.3070736234661524, 1.550032578732816828E-15 ) ) ;
#50419 = PRESENTATION_LAYER_ASSIGNMENT (  '', '', ( #35804 ) ) ;
#50420 = AXIS2_PLACEMENT_3D ( 'NONE', #67238, #50374, #7794 ) ;
#50421 = CARTESIAN_POINT ( 'NONE',  ( 20.22843684326250369, 114.9428328902810676, 10.38991920486588327 ) ) ;
#50422 = CARTESIAN_POINT ( 'NONE',  ( -174.4429263765337907, -1.166476076187852838E-15, -9.524999999999991473 ) ) ;
#50423 = DIRECTION ( 'NONE',  ( -1.000000000000000000, 0.000000000000000000, 0.000000000000000000 ) ) ;
#50424 = ADVANCED_FACE ( 'NONE', ( #40313 ), #8307, .T. ) ;
#50425 = ORIENTED_EDGE ( 'NONE', *, *, #40622, .T. ) ;
#50426 = CARTESIAN_POINT ( 'NONE',  ( -140.9070736234666583, -3.094860106609825134, 9.525000000006246026 ) ) ;
#50427 = CARTESIAN_POINT ( 'NONE',  ( -56.24499999999999034, -4.716976649647093289, -6.492361379858945902 ) ) ;
#50428 = ORIENTED_EDGE ( 'NONE', *, *, #23047, .F. ) ;
#50429 = CARTESIAN_POINT ( 'NONE',  ( 6.117035285937317823, 43.00000000000000711, 28.67160620906787472 ) ) ;
#50430 = CARTESIAN_POINT ( 'NONE',  ( 16.00000000000001776, -3.148064030671221758, -29.68999999999999417 ) ) ;
#50431 = CARTESIAN_POINT ( 'NONE',  ( -54.25383070671073682, -8.228704836117380239, -2.000000000000000000 ) ) ;
#50432 = CARTESIAN_POINT ( 'NONE',  ( 34.99999999999999289, 118.4999999999999716, -7.000000000000000000 ) ) ;
#50433 = EDGE_LOOP ( 'NONE', ( #34714, #44356, #25972, #43633 ) ) ;
#50434 = CARTESIAN_POINT ( 'NONE',  ( -49.97293742689555529, -12.55532684748290784, 1.207170231723877718 ) ) ;
#50435 = CARTESIAN_POINT ( 'NONE',  ( -56.24499999999999034, -4.716976649647093289, -6.492361379858945902 ) ) ;
#50436 = EDGE_LOOP ( 'NONE', ( #39743, #25436, #47604 ) ) ;
#50438 = EDGE_CURVE ( 'NONE', #32928, #21392, #37921, .T. ) ;
#50437 = CARTESIAN_POINT ( 'NONE',  ( -74.99999999999998579, 8.554981036082050849, 6.127545679190784078 ) ) ;
#50439 = CARTESIAN_POINT ( 'NONE',  ( -105.6549999999999869, -7.632228543268600340, -2.479861379858950166 ) ) ;
#50440 = ORIENTED_EDGE ( 'NONE', *, *, #63538, .F. ) ;
#50441 = FACE_OUTER_BOUND ( 'NONE', #50708, .T. ) ;
#50442 = CARTESIAN_POINT ( 'NONE',  ( 15.98999599679679839, 118.4999999999999716, -7.500000000000000000 ) ) ;
#50443 = DIRECTION ( 'NONE',  ( -0.000000000000000000, -0.000000000000000000, 1.000000000000000000 ) ) ;
#50444 = CARTESIAN_POINT ( 'NONE',  ( -149.4570736234661581, -9.058813317711329915, 2.943386871421371787 ) ) ;
#50445 = ADVANCED_FACE ( 'NONE', ( #67040 ), #26690, .F. ) ;
#50446 = DIRECTION ( 'NONE',  ( 0.000000000000000000, 0.000000000000000000, -1.000000000000000000 ) ) ;
#50447 = CARTESIAN_POINT ( 'NONE',  ( -3.094860106618434248, 146.7949999999999875, 9.525000000000000355 ) ) ;
#50448 = CARTESIAN_POINT ( 'NONE',  ( -83.60707362346616378, -8.102448949553172852, 5.886773742842742685 ) ) ;
#50449 = VECTOR ( 'NONE', #30183, 1000.000000000000000 ) ;
#50450 = SURFACE_SIDE_STYLE ('',( #55727 ) ) ;
#50451 = CARTESIAN_POINT ( 'NONE',  ( 23.71231517720798010, 117.9999999999999716, 7.000000000000000000 ) ) ;
#50452 = ORIENTED_EDGE ( 'NONE', *, *, #68734, .T. ) ;
#50453 = FILL_AREA_STYLE ('',( #28961 ) ) ;
#50454 = SURFACE_STYLE_USAGE ( .BOTH. , #7535 ) ;
#50455 = AXIS2_PLACEMENT_3D ( 'NONE', #69146, #52293, #40693 ) ;
#50456 = EDGE_CURVE ( 'NONE', #58700, #64993, #68303, .T. ) ;
#50457 = CARTESIAN_POINT ( 'NONE',  ( -134.3050000000000352, 8.437984349512085203, -1.550032578732815448E-15 ) ) ;
#50458 = DIRECTION ( 'NONE',  ( 0.000000000000000000, 0.000000000000000000, -1.000000000000000000 ) ) ;
#50459 = LINE ( 'NONE', #16740, #66187 ) ;
#50460 = CARTESIAN_POINT ( 'NONE',  ( -3.094860106618432471, 112.5949999999999989, -9.525000000000000355 ) ) ;
#50461 = CARTESIAN_POINT ( 'NONE',  ( -132.2949999999999875, -2.607480562269069768, 8.024999999999991473 ) ) ;
#50462 = CIRCLE ( 'NONE', #20104, 15.00000000000000000 ) ;
#50463 = MECHANICAL_DESIGN_GEOMETRIC_PRESENTATION_REPRESENTATION (  '', ( #57218 ), #7765 ) ;
#50464 = CARTESIAN_POINT ( 'NONE',  ( -131.9949999999999761, -6.826472737025113702, 4.959722759717902107 ) ) ;
#50465 = DIRECTION ( 'NONE',  ( 1.000000000000000000, 0.000000000000000000, 0.000000000000000000 ) ) ;
#50466 = ORIENTED_EDGE ( 'NONE', *, *, #42250, .F. ) ;
#50467 = AXIS2_PLACEMENT_3D ( 'NONE', #13561, #39301, #25171 ) ;
#50468 = CARTESIAN_POINT ( 'NONE',  ( -145.8570736234661638, -5.598654528085803328, -7.705886871421366635 ) ) ;
#50469 = LINE ( 'NONE', #7215, #65349 ) ;
#50470 = CARTESIAN_POINT ( 'NONE',  ( -177.2929263765337851, 3.094860106618428031, -9.524999999999993250 ) ) ;
#50471 =( NAMED_UNIT ( * ) SI_UNIT ( $, .STERADIAN. ) SOLID_ANGLE_UNIT ( ) );
#50472 = CARTESIAN_POINT ( 'NONE',  ( -50.84499999999997044, -7.632228543268599452, 2.479861379858951054 ) ) ;
#50473 = MECHANICAL_DESIGN_GEOMETRIC_PRESENTATION_REPRESENTATION (  '', ( #4387 ), #40381 ) ;
#50474 = CYLINDRICAL_SURFACE ( 'NONE', #47086, 0.2500000000000002220 ) ;
#50475 = LINE ( 'NONE', #50821, #1695 ) ;
#50476 = AXIS2_PLACEMENT_3D ( 'NONE', #20525, #24395, #30351 ) ;
#50477 = CARTESIAN_POINT ( 'NONE',  ( 75.83633811589984930, 13.00000000000000178, -66.72655454856717938 ) ) ;
#50478 = CARTESIAN_POINT ( 'NONE',  ( -96.44292637653380496, -1.166476076187852838E-15, -9.524999999999991473 ) ) ;
#50479 = SHAPE_DEFINITION_REPRESENTATION ( #20952, #31597 ) ;
#50480 = AXIS2_PLACEMENT_3D ( 'NONE', #2552, #29689, #34273 ) ;
#50481 = CARTESIAN_POINT ( 'NONE',  ( -47.71347897792733761, -13.42724224818812040, 0.9185643661977238583 ) ) ;
#50482 = CARTESIAN_POINT ( 'NONE',  ( 12.72792206135785698, 149.9999999999999716, -10.50000000000000000 ) ) ;
#50483 = APPLICATION_CONTEXT ( 'automotive_design' ) ;
#50484 = CARTESIAN_POINT ( 'NONE',  ( -81.20707362346617231, 3.094860106618433360, 9.524999999999991473 ) ) ;
#50485 = SURFACE_STYLE_FILL_AREA ( #7566 ) ;
#50486 = FACE_OUTER_BOUND ( 'NONE', #67811, .T. ) ;
#50487 = VECTOR ( 'NONE', #644, 1000.000000000000000 ) ;
#50488 = SURFACE_STYLE_USAGE ( .BOTH. , #54701 ) ;
#50489 = ORIENTED_EDGE ( 'NONE', *, *, #39482, .F. ) ;
#50490 =( NAMED_UNIT ( * ) PLANE_ANGLE_UNIT ( ) SI_UNIT ( $, .RADIAN. ) );
#50491 = SURFACE_STYLE_USAGE ( .BOTH. , #50837 ) ;
#50492 = MANIFOLD_SOLID_BREP ( 'Fillet3', #58736 ) ;
#50493 = CARTESIAN_POINT ( 'NONE',  ( -56.40813336638051112, -8.020529956771616398, -1.478673499587473295 ) ) ;
#50494 = EDGE_LOOP ( 'NONE', ( #3326, #66397, #23472, #13767 ) ) ;
#50495 = CARTESIAN_POINT ( 'NONE',  ( -9.827790563157511022E-16, 134.5570736234661808, 8.025000000000000355 ) ) ;
#50496 =( GEOMETRIC_REPRESENTATION_CONTEXT ( 3 ) GLOBAL_UNCERTAINTY_ASSIGNED_CONTEXT ( ( #32724 ) ) GLOBAL_UNIT_ASSIGNED_CONTEXT ( ( #37859, #53307, #31466 ) ) REPRESENTATION_CONTEXT ( 'NONE', 'WORKASPACE' ) );
#50497 = CARTESIAN_POINT ( 'NONE',  ( 6.826472737025121695, 120.6070736234661496, -4.959722759717905660 ) ) ;
#50498 = STYLED_ITEM ( 'NONE', ( #36028 ), #43940 ) ;
#50499 = CARTESIAN_POINT ( 'NONE',  ( 10.00000000000001954, 43.00000000000000000, 28.38386403503541899 ) ) ;
#50500 = CYLINDRICAL_SURFACE ( 'NONE', #61174, 5.000000000000000000 ) ;
#50502 = ORIENTED_EDGE ( 'NONE', *, *, #11112, .T. ) ;
#50501 = STYLED_ITEM ( 'NONE', ( #59518 ), #43032 ) ;
#50503 = CARTESIAN_POINT ( 'NONE',  ( -94.79292637653489351, -3.094860106599741201, 9.525000000013569945 ) ) ;
#50504 = CARTESIAN_POINT ( 'NONE',  ( -18.25000000000000711, 33.74999999999999289, 3.750000000000000000 ) ) ;
#50505 =( NAMED_UNIT ( * ) SI_UNIT ( $, .STERADIAN. ) SOLID_ANGLE_UNIT ( ) );
#50506 = ADVANCED_FACE ( 'NONE', ( #10720 ), #50518, .T. ) ;
#50507 = CIRCLE ( 'NONE', #3299, 0.5000000000000004441 ) ;
#50508 = CARTESIAN_POINT ( 'NONE',  ( -70.55707362346616662, -1.166476076187852838E-15, -9.524999999999991473 ) ) ;
#50509 = CARTESIAN_POINT ( 'NONE',  ( -83.99499999999999034, -6.826472737025115478, 4.959722759717900331 ) ) ;
#50511 = EDGE_LOOP ( 'NONE', ( #27001, #10873, #49146, #21438 ) ) ;
#50510 = AXIS2_PLACEMENT_3D ( 'NONE', #1089, #54953, #7821 ) ;
#50512 = AXIS2_PLACEMENT_3D ( 'NONE', #46242, #14531, #19099 ) ;
#50513 = EDGE_CURVE ( 'NONE', #36379, #58413, #54757, .T. ) ;
#50514 =( BOUNDED_CURVE ( )  B_SPLINE_CURVE ( 2, ( #60132, #23523, #45034, #66443, #18260, #39748, #12974, #949, #22504, #44002, #34434 ),
 .UNSPECIFIED., .F., .T. ) 
 B_SPLINE_CURVE_WITH_KNOTS ( ( 3, 2, 2, 2, 2, 3 ),
 ( 0.9456521739130434590, 0.9478260869565217073, 0.9499999999999999556, 0.9521739130434783149, 0.9543478260869565633, 0.9565217391304348116 ),
 .UNSPECIFIED. ) 
 CURVE ( )  GEOMETRIC_REPRESENTATION_ITEM ( )  RATIONAL_B_SPLINE_CURVE ( ( 1.000000000000000000, 0.9510565162951535312, 1.000000000000000000, 0.9510565162951535312, 1.000000000000000000, 0.9510565162951535312, 1.000000000000000000, 0.9510565162951535312, 1.000000000000000000, 0.9510565162951535312, 1.000000000000000000 ) ) 
 REPRESENTATION_ITEM ( '' )  );
#50515 = VECTOR ( 'NONE', #3640, 1000.000000000000000 ) ;
#50516 = CARTESIAN_POINT ( 'NONE',  ( -6.826472737025120807, 123.9929263765338163, 4.959722759717906548 ) ) ;
#50517 = EDGE_CURVE ( 'NONE', #60543, #12588, #36799, .T. ) ;
#50518 = CYLINDRICAL_SURFACE ( 'NONE', #35715, 15.00000000000000000 ) ;
#50519 = COLOUR_RGB ( '', 0.09019608, 0.27058824, 0.51372549) ;
#50520 = ORIENTED_EDGE ( 'NONE', *, *, #108, .F. ) ;
#50521 = DIRECTION ( 'NONE',  ( 0.000000000000000000, 1.000000000000000000, 0.000000000000000000 ) ) ;
#50522 = SURFACE_SIDE_STYLE ('',( #24798 ) ) ;
#50523 = AXIS2_PLACEMENT_3D ( 'NONE', #29882, #51345, #24580 ) ;
#50524 = EDGE_CURVE ( 'NONE', #12357, #47623, #904, .T. ) ;
#50525 = CARTESIAN_POINT ( 'NONE',  ( -65.50000000000000000, -2.024042244987997205E-14, 6.500000000000000000 ) ) ;
#50526 = EDGE_CURVE ( 'NONE', #61802, #43189, #80, .T. ) ;
#50527 = ORIENTED_EDGE ( 'NONE', *, *, #40366, .T. ) ;
#50528 = DIRECTION ( 'NONE',  ( 0.000000000000000000, 0.000000000000000000, -1.000000000000000000 ) ) ;
#50529 = EDGE_CURVE ( 'NONE', #10363, #26930, #36078, .T. ) ;
#50530 = ORIENTED_EDGE ( 'NONE', *, *, #58282, .F. ) ;
#50531 = SURFACE_SIDE_STYLE ('',( #56126 ) ) ;
#50532 = CARTESIAN_POINT ( 'NONE',  ( -67.99999999999998579, -2.024042244987997205E-14, 11.50000000000000000 ) ) ;
#50533 = CARTESIAN_POINT ( 'NONE',  ( -180.5070736234661979, 8.102448949553176405, 5.886773742842740909 ) ) ;
#50534 = EDGE_CURVE ( 'NONE', #6975, #59919, #33440, .T. ) ;
#50535 = CARTESIAN_POINT ( 'NONE',  ( -10.01517768586949408, 113.1949999999999790, -6.132527647946036459E-16 ) ) ;
#50536 = CARTESIAN_POINT ( 'NONE',  ( -111.5070736234661837, 8.102448949553176405, 5.886773742842740909 ) ) ;
#50537 = EDGE_CURVE ( 'NONE', #27751, #21970, #17673, .T. ) ;
#50538 = LINE ( 'NONE', #6918, #65043 ) ;
#50539 = ORIENTED_EDGE ( 'NONE', *, *, #27452, .F. ) ;
#50540 = LINE ( 'NONE', #45295, #49719 ) ;
#50541 =( NAMED_UNIT ( * ) PLANE_ANGLE_UNIT ( ) SI_UNIT ( $, .RADIAN. ) );
#50542 = CARTESIAN_POINT ( 'NONE',  ( -60.00000000000000000, -2.024042244987997205E-14, -6.500000000000000000 ) ) ;
#50543 = DIRECTION ( 'NONE',  ( -0.000000000000000000, -0.000000000000000000, -1.000000000000000000 ) ) ;
#50544 = EDGE_LOOP ( 'NONE', ( #29998, #47640, #30287, #24194 ) ) ;
#50545 = CARTESIAN_POINT ( 'NONE',  ( -164.3049999999999784, 8.437984349512085203, -1.550032578732815448E-15 ) ) ;
#50546 = CARTESIAN_POINT ( 'NONE',  ( -45.00000000000000000, 9.999999999999978684, -4.000000000000000000 ) ) ;
#50547 = CARTESIAN_POINT ( 'NONE',  ( -183.3519149756361912, 1.436423777000723276E-13, -9.173085024363883733 ) ) ;
#50548 = CARTESIAN_POINT ( 'NONE',  ( -164.6949999999999648, -8.437984349512085203, 5.166775262442717831E-16 ) ) ;
#50549 = CARTESIAN_POINT ( 'NONE',  ( -152.9950000000000045, -6.826472737025113702, 4.959722759717902107 ) ) ;
#50550 = AXIS2_PLACEMENT_3D ( 'NONE', #44168, #11052, #54989 ) ;
#50551 = AXIS2_PLACEMENT_3D ( 'NONE', #33726, #45719, #18614 ) ;
#50552 = VERTEX_POINT ( 'NONE', #42096 ) ;
#50553 =( NAMED_UNIT ( * ) SI_UNIT ( $, .STERADIAN. ) SOLID_ANGLE_UNIT ( ) );
#50554 = AXIS2_PLACEMENT_3D ( 'NONE', #45820, #35598, #3523 ) ;
#50555 = CARTESIAN_POINT ( 'NONE',  ( 10.39230484541326582, -1.107695154586738839, 1.440973567693753677E-18 ) ) ;
#50556 = CARTESIAN_POINT ( 'NONE',  ( -77.90500000000000114, 2.607480562269068880, -8.024999999999993250 ) ) ;
#50557 = CARTESIAN_POINT ( 'NONE',  ( 25.75000000000001066, 21.99999999999998224, -3.750000000000000000 ) ) ;
#50558 = CARTESIAN_POINT ( 'NONE',  ( -166.9429263765337907, 0.000000000000000000, 9.524999999999991473 ) ) ;
#50559 = CARTESIAN_POINT ( 'NONE',  ( -67.79499999999998749, 2.607480562269069324, -8.024999999999993250 ) ) ;
#50560 = CARTESIAN_POINT ( 'NONE',  ( 5.598654528085809545, 146.2549999999999955, -7.705886871421373741 ) ) ;
#50561 = DIRECTION ( 'NONE',  ( -1.000000000000000000, 0.000000000000000000, 0.000000000000000000 ) ) ;
#50562 = VECTOR ( 'NONE', #45836, 1000.000000000000000 ) ;
#50563 = LINE ( 'NONE', #18559, #15858 ) ;
#50564 = VECTOR ( 'NONE', #35434, 1000.000000000000000 ) ;
#50565 = CARTESIAN_POINT ( 'NONE',  ( 3.249999999999998668, 36.74999999999999289, -4.000000000000000000 ) ) ;
#50566 = CARTESIAN_POINT ( 'NONE',  ( 8.701243704650551081, 2.329718218673044738, -2.929003814506405678 ) ) ;
#50567 = COLOUR_RGB ( '', 0.31764706, 0.68627451, 0.89019608) ;
#50568 = LINE ( 'NONE', #39687, #66361 ) ;
#50569 = CARTESIAN_POINT ( 'NONE',  ( -120.2929263765346377, 3.094860106604916616, -9.525000000009809398 ) ) ;
#50570 = DIRECTION ( 'NONE',  ( -1.000000000000000000, 0.000000000000000000, 0.000000000000000000 ) ) ;
#50571 = VERTEX_POINT ( 'NONE', #69460 ) ;
#50572 = AXIS2_PLACEMENT_3D ( 'NONE', #29865, #7710, #23893 ) ;
#50573 = ORIENTED_EDGE ( 'NONE', *, *, #54238, .F. ) ;
#50574 = CARTESIAN_POINT ( 'NONE',  ( -156.1429263765338078, 5.598654528085800663, -7.705886871421367523 ) ) ;
#50575 = DIRECTION ( 'NONE',  ( -0.000000000000000000, 0.000000000000000000, -1.000000000000000000 ) ) ;
#50576 = CARTESIAN_POINT ( 'NONE',  ( 5.196152422706631135, 1.107695154586740394, 9.000000000000001776 ) ) ;
#50577 = EDGE_LOOP ( 'NONE', ( #17968, #30831, #11103, #29810 ) ) ;
#50578 = EDGE_LOOP ( 'NONE', ( #9497, #31633, #67020, #45297 ) ) ;
#50579 = CARTESIAN_POINT ( 'NONE',  ( 30.75000000000001066, 15.74999999999997513, 4.000000000000000000 ) ) ;
#50580 = EDGE_CURVE ( 'NONE', #67023, #25443, #12090, .T. ) ;
#50581 = ORIENTED_EDGE ( 'NONE', *, *, #28625, .T. ) ;
#50582 = LINE ( 'NONE', #66763, #35541 ) ;
#50583 = ORIENTED_EDGE ( 'NONE', *, *, #68550, .T. ) ;
#50584 = EDGE_CURVE ( 'NONE', #27560, #60303, #5756, .T. ) ;
#50585 = DIRECTION ( 'NONE',  ( 1.000000000000000000, 0.000000000000000000, 0.000000000000000000 ) ) ;
#50586 = CARTESIAN_POINT ( 'NONE',  ( -110.6949999999999932, -8.437984349512085203, 5.166775262442717831E-16 ) ) ;
#50587 = EDGE_LOOP ( 'NONE', ( #54547, #8792, #29198, #2876 ) ) ;
#50588 = EDGE_CURVE ( 'NONE', #33393, #1575, #12702, .T. ) ;
#50589 = ORIENTED_EDGE ( 'NONE', *, *, #60364, .T. ) ;
#50590 = PLANE ( 'NONE',  #18705 ) ;
#50591 = CARTESIAN_POINT ( 'NONE',  ( -71.49999999999998579, 64.07124727947029896, 7.500000000000000000 ) ) ;
#50592 = CARTESIAN_POINT ( 'NONE',  ( -10.26016645771925262, -11.89338941245402737, 1.624758447612887347 ) ) ;
#50593 = AXIS2_PLACEMENT_3D ( 'NONE', #37974, #21053, #42227 ) ;
#50594 = DIRECTION ( 'NONE',  ( -0.000000000000000000, -1.000000000000000000, -0.000000000000000000 ) ) ;
#50595 = ORIENTED_EDGE ( 'NONE', *, *, #3337, .F. ) ;
#50596 = CARTESIAN_POINT ( 'NONE',  ( -9.827790563157511022E-16, 145.4429263765338192, 8.025000000000000355 ) ) ;
#50597 = CARTESIAN_POINT ( 'NONE',  ( -6.826472737025120807, 114.9929263765338163, 4.959722759717906548 ) ) ;
#50598 = VERTEX_POINT ( 'NONE', #37851 ) ;
#50599 = EDGE_CURVE ( 'NONE', #11349, #66584, #1830, .T. ) ;
#50600 = EDGE_LOOP ( 'NONE', ( #50665, #37816, #6440, #58838 ) ) ;
#50601 = SURFACE_SIDE_STYLE ('',( #60784 ) ) ;
#50602 = CARTESIAN_POINT ( 'NONE',  ( -6.826472737025120807, 139.5070736234661126, -4.959722759717907437 ) ) ;
#50603 = CARTESIAN_POINT ( 'NONE',  ( -20.40217977176332553, 114.8427411095148472, 10.33293932795019643 ) ) ;
#50604 = CARTESIAN_POINT ( 'NONE',  ( -157.5570736234661808, -1.166476076187852838E-15, -9.524999999999991473 ) ) ;
#50605 = CARTESIAN_POINT ( 'NONE',  ( -131.3050000000000068, 8.437984349512085203, -1.550032578732815448E-15 ) ) ;
#50606 = DIRECTION ( 'NONE',  ( -0.000000000000000000, -0.000000000000000000, -1.000000000000000000 ) ) ;
#50607 = AXIS2_PLACEMENT_3D ( 'NONE', #16522, #36942, #48889 ) ;
#50608 = CARTESIAN_POINT ( 'NONE',  ( 60.00000000000000000, 1.797044900979284448E-15, -12.00000000000000000 ) ) ;
#50609 = ORIENTED_EDGE ( 'NONE', *, *, #18692, .T. ) ;
#50610 = DIRECTION ( 'NONE',  ( -1.000000000000000000, 0.000000000000000000, 0.000000000000000000 ) ) ;
#50611 = EDGE_CURVE ( 'NONE', #52417, #65027, #57045, .T. ) ;
#50612 = CARTESIAN_POINT ( 'NONE',  ( -60.00000000000000000, -2.024042244987997205E-14, 6.999999999999995559 ) ) ;
#50613 = CYLINDRICAL_SURFACE ( 'NONE', #15765, 0.2500000000000002220 ) ;
#50614 = ORIENTED_EDGE ( 'NONE', *, *, #65365, .F. ) ;
#50615 = AXIS2_PLACEMENT_3D ( 'NONE', #28566, #12393, #1798 ) ;
#50616 = ORIENTED_EDGE ( 'NONE', *, *, #29619, .T. ) ;
#50617 = CARTESIAN_POINT ( 'NONE',  ( -24.21231517720798010, 113.4999999999999858, 7.000000000000000000 ) ) ;
#50618 =( NAMED_UNIT ( * ) PLANE_ANGLE_UNIT ( ) SI_UNIT ( $, .RADIAN. ) );
#50619 = DIRECTION ( 'NONE',  ( -0.000000000000000000, -0.000000000000000000, -1.000000000000000000 ) ) ;
#50620 = ORIENTED_EDGE ( 'NONE', *, *, #38094, .T. ) ;
#50621 = PLANE ( 'NONE',  #34885 ) ;
#50622 = CARTESIAN_POINT ( 'NONE',  ( -184.5550000000000068, 0.000000000000000000, 8.024999999999991473 ) ) ;
#50623 = LINE ( 'NONE', #8053, #7096 ) ;
#50624 = CARTESIAN_POINT ( 'NONE',  ( 2.418535808707042101, 7.000000000000006217, 0.3989014552058406382 ) ) ;
#50625 =( GEOMETRIC_REPRESENTATION_CONTEXT ( 3 ) GLOBAL_UNCERTAINTY_ASSIGNED_CONTEXT ( ( #15904 ) ) GLOBAL_UNIT_ASSIGNED_CONTEXT ( ( #28086, #13313, #34772 ) ) REPRESENTATION_CONTEXT ( 'NONE', 'WORKASPACE' ) );
#50626 = CARTESIAN_POINT ( 'NONE',  ( -51.35707362346617089, 5.598654528085804216, 7.705886871421366635 ) ) ;
#50627 = DIRECTION ( 'NONE',  ( 0.9704308468600219006, -0.2413793103448194366, -0.000000000000000000 ) ) ;
#50628 = CARTESIAN_POINT ( 'NONE',  ( -177.8070736234661808, 10.01517768586948698, -1.839758294383808966E-15 ) ) ;
#50629 = ORIENTED_EDGE ( 'NONE', *, *, #66575, .T. ) ;
#50630 = PRODUCT_DEFINITION_FORMATION_WITH_SPECIFIED_SOURCE ( 'ANY', '', #20359, .NOT_KNOWN. ) ;
#50631 = CARTESIAN_POINT ( 'NONE',  ( -145.1070736234661638, 8.102448949553172852, -5.886773742842744461 ) ) ;
#50632 = FACE_OUTER_BOUND ( 'NONE', #31969, .T. ) ;
#50633 = CARTESIAN_POINT ( 'NONE',  ( -98.60499999999997556, 6.826472737025113702, -4.959722759717902107 ) ) ;
#50634 = CARTESIAN_POINT ( 'NONE',  ( 8.111916646337986592, 154.4999999999999147, -5.069419100131139722 ) ) ;
#50635 = PRESENTATION_STYLE_ASSIGNMENT (( #12280 ) ) ;
#50636 =( NAMED_UNIT ( * ) SI_UNIT ( $, .STERADIAN. ) SOLID_ANGLE_UNIT ( ) );
#50637 = CARTESIAN_POINT ( 'NONE',  ( -96.44499999999999318, 0.000000000000000000, 8.024999999999991473 ) ) ;
#50638 = CARTESIAN_POINT ( 'NONE',  ( -8.102448949553181734, 120.0049999999999955, -5.886773742842749790 ) ) ;
#50639 = CARTESIAN_POINT ( 'NONE',  ( -81.59499999999997044, 2.607480562269073321, 8.024999999999991473 ) ) ;
#50640 = LINE ( 'NONE', #61867, #7228 ) ;
#50641 = CARTESIAN_POINT ( 'NONE',  ( -4.716976649647098618, 142.1429263765338078, 6.492361379858953008 ) ) ;
#50642 = DIRECTION ( 'NONE',  ( 1.000000000000000000, 0.000000000000000000, 0.000000000000000000 ) ) ;
#50643 =( GEOMETRIC_REPRESENTATION_CONTEXT ( 3 ) GLOBAL_UNCERTAINTY_ASSIGNED_CONTEXT ( ( #67874 ) ) GLOBAL_UNIT_ASSIGNED_CONTEXT ( ( #53082, #42552, #17539 ) ) REPRESENTATION_CONTEXT ( 'NONE', 'WORKASPACE' ) );
#50644 = CARTESIAN_POINT ( 'NONE',  ( -195.0000000000000000, 0.000000000000000000, 0.000000000000000000 ) ) ;
#50645 = EDGE_CURVE ( 'NONE', #46401, #48506, #28946, .T. ) ;
#50646 = LINE ( 'NONE', #12293, #34264 ) ;
#50648 = ORIENTED_EDGE ( 'NONE', *, *, #12218, .T. ) ;
#50647 = CIRCLE ( 'NONE', #62991, 0.5000000000000004441 ) ;
#50649 = CARTESIAN_POINT ( 'NONE',  ( -117.7429263765338021, -5.598654528085803328, -7.705886871421366635 ) ) ;
#50650 = CARTESIAN_POINT ( 'NONE',  ( -138.1449999999999818, -4.716976649647092401, 6.492361379858946790 ) ) ;
#50651 = EDGE_CURVE ( 'NONE', #3770, #1012, #49398, .T. ) ;
#50652 = PRESENTATION_STYLE_ASSIGNMENT (( #54860 ) ) ;
#50653 = CARTESIAN_POINT ( 'NONE',  ( -34.99999999999999289, 99.99999999999998579, 4.000000000000000000 ) ) ;
#50654 = CIRCLE ( 'NONE', #39437, 0.2500000000000002220 ) ;
#50655 = PRESENTATION_STYLE_ASSIGNMENT (( #2034 ) ) ;
#50656 = ORIENTED_EDGE ( 'NONE', *, *, #59090, .F. ) ;
#50657 = ORIENTED_EDGE ( 'NONE', *, *, #59242, .T. ) ;
#50658 = CIRCLE ( 'NONE', #58536, 0.5000000000000006661 ) ;
#50659 = DIRECTION ( 'NONE',  ( -0.000000000000000000, 1.000000000000000000, 0.000000000000000000 ) ) ;
#50660 = DIRECTION ( 'NONE',  ( 0.000000000000000000, 0.000000000000000000, 1.000000000000000000 ) ) ;
#50661 = COLOUR_RGB ( '', 0.40784314, 0.44705882, 0.49803922) ;
#50662 = FACE_OUTER_BOUND ( 'NONE', #10797, .T. ) ;
#50663 = CARTESIAN_POINT ( 'NONE',  ( 66.74999999999998579, 37.00000000000000000, 4.000000000000000000 ) ) ;
#50664 = FACE_OUTER_BOUND ( 'NONE', #29089, .T. ) ;
#50665 = ORIENTED_EDGE ( 'NONE', *, *, #63648, .F. ) ;
#50666 = CARTESIAN_POINT ( 'NONE',  ( -134.7549999999999955, 4.716976649647091513, -6.492361379858946790 ) ) ;
#50668 = EDGE_CURVE ( 'NONE', #57165, #49424, #42475, .T. ) ;
#50667 = ORIENTED_EDGE ( 'NONE', *, *, #26584, .F. ) ;
#50669 = EDGE_CURVE ( 'NONE', #33948, #40021, #65210, .T. ) ;
#50670 = ORIENTED_EDGE ( 'NONE', *, *, #29636, .F. ) ;
#50671 = CARTESIAN_POINT ( 'NONE',  ( -60.99999999999998579, 50.00000000000000000, -9.500000000000000000 ) ) ;
#50672 = CARTESIAN_POINT ( 'NONE',  ( -83.99292637653380211, 8.102448949553172852, -5.886773742842744461 ) ) ;
#50673 = ORIENTED_EDGE ( 'NONE', *, *, #63528, .F. ) ;
#50674 = VECTOR ( 'NONE', #59311, 1000.000000000000000 ) ;
#50675 = CARTESIAN_POINT ( 'NONE',  ( -102.4429263765338050, -1.166476076187852838E-15, -9.524999999999991473 ) ) ;
#50676 = CARTESIAN_POINT ( 'NONE',  ( 0.000000000000000000, 87.30187232391182306, 0.000000000000000000 ) ) ;
#50677 = CARTESIAN_POINT ( 'NONE',  ( 3.094860106618431583, 144.0949999999999704, 9.525000000000000355 ) ) ;
#50678 = DIRECTION ( 'NONE',  ( -1.000000000000000000, 0.000000000000000000, 0.000000000000000000 ) ) ;
#50679 = AXIS2_PLACEMENT_3D ( 'NONE', #36134, #56879, #30118 ) ;
#50680 = EDGE_LOOP ( 'NONE', ( #49154, #50246, #51109, #32610, #23289, #14331 ) ) ;
#50681 = DIRECTION ( 'NONE',  ( -0.000000000000000000, -1.000000000000000000, 0.000000000000000000 ) ) ;
#50683 = EDGE_CURVE ( 'NONE', #5601, #66072, #767, .T. ) ;
#50682 = CARTESIAN_POINT ( 'NONE',  ( -9.058813317711338797, 135.4549999999999841, 2.943386871421373563 ) ) ;
#50684 = CARTESIAN_POINT ( 'NONE',  ( -49.40499999999997982, -2.607480562269069768, 8.024999999999991473 ) ) ;
#50685 = CARTESIAN_POINT ( 'NONE',  ( -55.00000000000000000, -2.024042244987997205E-14, -7.000000000000024869 ) ) ;
#50686 = ORIENTED_EDGE ( 'NONE', *, *, #28625, .F. ) ;
#50687 = CARTESIAN_POINT ( 'NONE',  ( 8.437984349512095861, 116.1929263765338192, 1.550032578732817026E-15 ) ) ;
#50688 = DIRECTION ( 'NONE',  ( 0.000000000000000000, 0.000000000000000000, -1.000000000000000000 ) ) ;
#50689 =( LENGTH_UNIT ( ) NAMED_UNIT ( * ) SI_UNIT ( .MILLI., .METRE. ) );
#50690 = EDGE_CURVE ( 'NONE', #3382, #63631, #6809, .T. ) ;
#50691 = DIRECTION ( 'NONE',  ( 0.000000000000000000, 0.000000000000000000, 1.000000000000000000 ) ) ;
#50692 = EDGE_LOOP ( 'NONE', ( #35890, #23576 ) ) ;
#50693 = EDGE_CURVE ( 'NONE', #15233, #54902, #38540, .T. ) ;
#50694 = ORIENTED_EDGE ( 'NONE', *, *, #40697, .F. ) ;
#50695 = DIRECTION ( 'NONE',  ( 1.000000000000000000, 0.000000000000000000, 0.000000000000000000 ) ) ;
#50696 = CARTESIAN_POINT ( 'NONE',  ( -32.35935878254957743, -8.628464621395343315, -2.363854359607545419 ) ) ;
#50697 = DIRECTION ( 'NONE',  ( -0.000000000000000000, -0.000000000000000000, 1.000000000000000000 ) ) ;
#50699 = CARTESIAN_POINT ( 'NONE',  ( -158.4549999999999841, 7.632228543268599452, -2.479861379858951942 ) ) ;
#50698 = CONICAL_SURFACE ( 'NONE', #65290, 22.49999999999999645, 0.7853981633974239651 ) ;
#50700 = ORIENTED_EDGE ( 'NONE', *, *, #37388, .T. ) ;
#50701 = VECTOR ( 'NONE', #37580, 1000.000000000000000 ) ;
#50702 = COLOUR_RGB ( '', 0.40784314, 0.44705882, 0.49803922) ;
#50703 =( LENGTH_UNIT ( ) NAMED_UNIT ( * ) SI_UNIT ( .MILLI., .METRE. ) );
#50704 = EDGE_CURVE ( 'NONE', #53882, #61196, #21091, .T. ) ;
#50705 = FILL_AREA_STYLE_COLOUR ( '', #15912 ) ;
#50706 = SURFACE_STYLE_FILL_AREA ( #39840 ) ;
#50707 = ORIENTED_EDGE ( 'NONE', *, *, #12624, .T. ) ;
#50708 = EDGE_LOOP ( 'NONE', ( #39349, #2794, #34586, #25167 ) ) ;
#50709 = LINE ( 'NONE', #7780, #51884 ) ;
#50710 =( GEOMETRIC_REPRESENTATION_CONTEXT ( 3 ) GLOBAL_UNCERTAINTY_ASSIGNED_CONTEXT ( ( #32687 ) ) GLOBAL_UNIT_ASSIGNED_CONTEXT ( ( #24936, #67163, #67873 ) ) REPRESENTATION_CONTEXT ( 'NONE', 'WORKASPACE' ) );
#50711 = CARTESIAN_POINT ( 'NONE',  ( 1.000000000000000000, 36.99999999999999289, 3.000000000000000000 ) ) ;
#50712 = CARTESIAN_POINT ( 'NONE',  ( -73.85499999999998977, 4.716976649647094177, 6.492361379858945902 ) ) ;
#50713 = ORIENTED_EDGE ( 'NONE', *, *, #66964, .T. ) ;
#50714 = DIRECTION ( 'NONE',  ( 0.000000000000000000, 0.000000000000000000, 1.000000000000000000 ) ) ;
#50715 = CIRCLE ( 'NONE', #61883, 0.2500000000000002220 ) ;
#50716 =( GEOMETRIC_REPRESENTATION_CONTEXT ( 3 ) GLOBAL_UNCERTAINTY_ASSIGNED_CONTEXT ( ( #27120 ) ) GLOBAL_UNIT_ASSIGNED_CONTEXT ( ( #2942, #14248, #34646 ) ) REPRESENTATION_CONTEXT ( 'NONE', 'WORKASPACE' ) );
#50717 =( NAMED_UNIT ( * ) PLANE_ANGLE_UNIT ( ) SI_UNIT ( $, .RADIAN. ) );
#50718 = STYLED_ITEM ( 'NONE', ( #4791 ), #54120 ) ;
#50719 =( LENGTH_UNIT ( ) NAMED_UNIT ( * ) SI_UNIT ( .MILLI., .METRE. ) );
#50720 = ORIENTED_EDGE ( 'NONE', *, *, #68793, .T. ) ;
#50721 = CARTESIAN_POINT ( 'NONE',  ( -60.00000000000000000, -2.024042244987997205E-14, -11.50000000000000355 ) ) ;
#50722 = AXIS2_PLACEMENT_3D ( 'NONE', #19227, #40736, #13974 ) ;
#50724 = FILL_AREA_STYLE_COLOUR ( '', #23488 ) ;
#50723 = DIRECTION ( 'NONE',  ( 0.000000000000000000, 0.000000000000000000, -1.000000000000000000 ) ) ;
#50725 = CARTESIAN_POINT ( 'NONE',  ( -3.094860106618434248, 140.7950000000000159, 9.525000000000000355 ) ) ;
#50726 = CARTESIAN_POINT ( 'NONE',  ( -106.4950000000000045, 6.826472737025113702, -4.959722759717902107 ) ) ;
#50727 = CIRCLE ( 'NONE', #65328, 0.5000000000000004441 ) ;
#50728 = DIRECTION ( 'NONE',  ( 0.000000000000000000, 0.000000000000000000, -1.000000000000000000 ) ) ;
#50729 = DIRECTION ( 'NONE',  ( 0.000000000000000000, 0.000000000000000000, 1.000000000000000000 ) ) ;
#50730 = VECTOR ( 'NONE', #33518, 1000.000000000000000 ) ;
#50731 = ADVANCED_FACE ( 'NONE', ( #39210 ), #41356, .T. ) ;
#50732 = PRESENTATION_LAYER_ASSIGNMENT (  '', '', ( #58603 ) ) ;
#50734 = CARTESIAN_POINT ( 'NONE',  ( -19.96671590325603418, 11.98602375733942438, -0.6633104301215919651 ) ) ;
#50733 = SURFACE_SIDE_STYLE ('',( #61958 ) ) ;
#50735 = CARTESIAN_POINT ( 'NONE',  ( -140.2429263765338021, 5.598654528085804216, 7.705886871421366635 ) ) ;
#50736 = CARTESIAN_POINT ( 'NONE',  ( -164.3950000000000102, -6.826472737025115478, -4.959722759717899443 ) ) ;
#50737 =( GEOMETRIC_REPRESENTATION_CONTEXT ( 3 ) GLOBAL_UNCERTAINTY_ASSIGNED_CONTEXT ( ( #13117 ) ) GLOBAL_UNIT_ASSIGNED_CONTEXT ( ( #18254, #7007, #45378 ) ) REPRESENTATION_CONTEXT ( 'NONE', 'WORKASPACE' ) );
#50738 = SURFACE_STYLE_FILL_AREA ( #46187 ) ;
#50739 = ORIENTED_EDGE ( 'NONE', *, *, #33504, .T. ) ;
#50740 = CARTESIAN_POINT ( 'NONE',  ( -8.437984349512095861, 127.8070736234661666, -5.166775262442723748E-16 ) ) ;
#50741 = EDGE_LOOP ( 'NONE', ( #19348, #29948, #35920, #6803 ) ) ;
#50742 = CIRCLE ( 'NONE', #49642, 16.44999999999999218 ) ;
#50743 = PRESENTATION_LAYER_ASSIGNMENT (  '', '', ( #41788 ) ) ;
#50744 = EDGE_CURVE ( 'NONE', #37946, #61027, #38876, .T. ) ;
#50745 = VECTOR ( 'NONE', #27427, 1000.000000000000000 ) ;
#50746 = DIRECTION ( 'NONE',  ( -1.000000000000000000, 0.000000000000000000, 0.000000000000000000 ) ) ;
#50747 = DIRECTION ( 'NONE',  ( 0.000000000000000000, 0.000000000000000000, -1.000000000000000000 ) ) ;
#50748 = CARTESIAN_POINT ( 'NONE',  ( 17.25000000000000711, 24.99999999999998224, -3.750000000000000000 ) ) ;
#50749 = AXIS2_PLACEMENT_3D ( 'NONE', #62513, #56904, #24185 ) ;
#50750 = COLOUR_RGB ( '', 0.72549020, 0.75294118, 0.79215686) ;
#50751 = ORIENTED_EDGE ( 'NONE', *, *, #37863, .T. ) ;
#50752 = CARTESIAN_POINT ( 'NONE',  ( -160.2549999999999670, -4.716976649647092401, 6.492361379858946790 ) ) ;
#50753 = EDGE_CURVE ( 'NONE', #20985, #63718, #27835, .T. ) ;
#50754 = EDGE_CURVE ( 'NONE', #40436, #3748, #54636, .T. ) ;
#50755 = EDGE_LOOP ( 'NONE', ( #32575, #19336, #45381, #30392, #56000, #1298, #7090, #9836, #66725, #56273, #22898, #21410, #10033, #62956, #4976, #64236, #44351, #57628 ) ) ;
#50756 = DIRECTION ( 'NONE',  ( -0.000000000000000000, -0.000000000000000000, -1.000000000000000000 ) ) ;
#50757 = STYLED_ITEM ( 'NONE', ( #15142 ), #22003 ) ;
#50758 = SURFACE_SIDE_STYLE ('',( #28921 ) ) ;
#50759 = CARTESIAN_POINT ( 'NONE',  ( 4.000000000000030198, 38.70020753820971748, 90.00000000000000000 ) ) ;
#50760 = CARTESIAN_POINT ( 'NONE',  ( 98.00000000000000000, 16.00000000000000000, 0.000000000000000000 ) ) ;
#50761 = CARTESIAN_POINT ( 'NONE',  ( -9.827790563157511022E-16, 158.5570736234661524, 8.025000000000000355 ) ) ;
#50762 = EDGE_LOOP ( 'NONE', ( #39715, #24940, #7448, #38608 ) ) ;
#50763 = CYLINDRICAL_SURFACE ( 'NONE', #31932, 0.2500000000000002220 ) ;
#50765 = EDGE_CURVE ( 'NONE', #58968, #54047, #6503, .T. ) ;
#50764 = CARTESIAN_POINT ( 'NONE',  ( -9.058813317711337021, 114.1549999999999869, -2.943386871421374895 ) ) ;
#50766 = CARTESIAN_POINT ( 'NONE',  ( -77.00499999999999545, 6.826472737025115478, 4.959722759717899443 ) ) ;
#50767 = LINE ( 'NONE', #61992, #42155 ) ;
#50768 = CARTESIAN_POINT ( 'NONE',  ( -1.166476076187854022E-15, 127.0549999999999784, 9.525000000000000355 ) ) ;
#50769 = CIRCLE ( 'NONE', #31509, 6.999999999999997335 ) ;
#50770 = SURFACE_SIDE_STYLE ('',( #17729 ) ) ;
#50771 = EDGE_CURVE ( 'NONE', #16969, #50010, #19086, .T. ) ;
#50772 = CIRCLE ( 'NONE', #28282, 10.00000000000000533 ) ;
#50773 = CARTESIAN_POINT ( 'NONE',  ( 20.44241585271047867, 115.3856657692246444, 10.00000000000000000 ) ) ;
#50774 = AXIS2_PLACEMENT_3D ( 'NONE', #63336, #58754, #5263 ) ;
#50775 = CARTESIAN_POINT ( 'NONE',  ( -113.7570736234661837, -5.598654528085801552, 7.705886871421367523 ) ) ;
#50776 = ORIENTED_EDGE ( 'NONE', *, *, #43516, .T. ) ;
#50777 = CARTESIAN_POINT ( 'NONE',  ( -57.29499999999998039, -2.607480562269069768, 8.024999999999991473 ) ) ;
#50778 = ORIENTED_EDGE ( 'NONE', *, *, #32623, .F. ) ;
#50779 = DIRECTION ( 'NONE',  ( -0.2413793103448194644, 0.9704308468600220117, 0.000000000000000000 ) ) ;
#50780 = AXIS2_PLACEMENT_3D ( 'NONE', #10317, #26120, #62703 ) ;
#50781 = FACE_OUTER_BOUND ( 'NONE', #68680, .T. ) ;
#50782 = ORIENTED_EDGE ( 'NONE', *, *, #48426, .T. ) ;
#50783 = CARTESIAN_POINT ( 'NONE',  ( -53.60138881051016568, -9.947368421052628307, 2.722470280083840066 ) ) ;
#50784 = CARTESIAN_POINT ( 'NONE',  ( -53.24499999999999034, -4.716976649647093289, -6.492361379858945902 ) ) ;
#50785 = SURFACE_STYLE_USAGE ( .BOTH. , #55712 ) ;
#50786 = ORIENTED_EDGE ( 'NONE', *, *, #3952, .F. ) ;
#50787 = STYLED_ITEM ( 'NONE', ( #12082 ), #24315 ) ;
#50788 = CARTESIAN_POINT ( 'NONE',  ( -75.00000000000000000, 9.701542612659364906, 6.099661992412386269 ) ) ;
#50789 = CARTESIAN_POINT ( 'NONE',  ( -107.4549999999999983, 7.632228543268599452, -2.479861379858951942 ) ) ;
#50790 = ORIENTED_EDGE ( 'NONE', *, *, #46425, .T. ) ;
#50791 = EDGE_CURVE ( 'NONE', #60808, #22472, #56035, .T. ) ;
#50792 = DIRECTION ( 'NONE',  ( 1.000000000000000000, 0.000000000000000000, 0.000000000000000000 ) ) ;
#50793 = PLANE ( 'NONE',  #42123 ) ;
#50794 = CARTESIAN_POINT ( 'NONE',  ( -144.6570736234662036, 9.058813317711329915, 2.943386871421369566 ) ) ;
#50795 = PRESENTATION_LAYER_ASSIGNMENT (  '', '', ( #40722 ) ) ;
#50796 = EDGE_CURVE ( 'NONE', #13760, #30149, #15501, .T. ) ;
#50797 = CARTESIAN_POINT ( 'NONE',  ( -60.00000000000000000, -2.024042244987997205E-14, 6.999999999999995559 ) ) ;
#50798 = CARTESIAN_POINT ( 'NONE',  ( -10.01517768586949408, 143.1949999999999932, -6.132527647946036459E-16 ) ) ;
#50799 = CARTESIAN_POINT ( 'NONE',  ( -88.55707362346616662, -1.166476076187852838E-15, -9.524999999999991473 ) ) ;
#50800 = CIRCLE ( 'NONE', #49698, 4.999999999999997335 ) ;
#50801 = VECTOR ( 'NONE', #55210, 1000.000000000000000 ) ;
#50802 = FILL_AREA_STYLE ('',( #33571 ) ) ;
#50803 = FILL_AREA_STYLE_COLOUR ( '', #23772 ) ;
#50805 = DIRECTION ( 'NONE',  ( 0.000000000000000000, 0.000000000000000000, -1.000000000000000000 ) ) ;
#50804 = CIRCLE ( 'NONE', #63151, 5.500000000000005329 ) ;
#50806 = CARTESIAN_POINT ( 'NONE',  ( -117.0549999999999926, -9.827790563157499189E-16, -8.024999999999991473 ) ) ;
#50807 = CARTESIAN_POINT ( 'NONE',  ( -9.000000000000003553, 27.74999999999998934, 3.750000000000000000 ) ) ;
#50808 = CARTESIAN_POINT ( 'NONE',  ( -159.2929263765341261, 3.094860106613084305, -9.525000000003878142 ) ) ;
#50809 = CARTESIAN_POINT ( 'NONE',  ( 5.598654528085809545, 115.1449999999999818, -7.705886871421373741 ) ) ;
#50810 = CARTESIAN_POINT ( 'NONE',  ( -138.5949999999999420, 2.607480562269073321, 8.024999999999991473 ) ) ;
#50811 = CARTESIAN_POINT ( 'NONE',  ( -118.3449999999999989, 7.632228543268599452, -2.479861379858951942 ) ) ;
#50812 = MECHANICAL_DESIGN_GEOMETRIC_PRESENTATION_REPRESENTATION (  '', ( #12567 ), #63163 ) ;
#50813 = CYLINDRICAL_SURFACE ( 'NONE', #3179, 0.5000000000000004441 ) ;
#50814 = ORIENTED_EDGE ( 'NONE', *, *, #22324, .F. ) ;
#50815 = DIRECTION ( 'NONE',  ( 0.000000000000000000, 1.000000000000000000, 0.000000000000000000 ) ) ;
#50816 = CARTESIAN_POINT ( 'NONE',  ( -171.7429263765338305, -5.598654528085803328, -7.705886871421366635 ) ) ;
#50817 = PRESENTATION_STYLE_ASSIGNMENT (( #14565 ) ) ;
#50818 = CARTESIAN_POINT ( 'NONE',  ( -49.19499999999999318, 8.437984349512085203, -1.550032578732815448E-15 ) ) ;
#50819 = STYLED_ITEM ( 'NONE', ( #37084 ), #28748 ) ;
#50820 = CARTESIAN_POINT ( 'NONE',  ( -71.99999999999998579, 119.9999999999997868, -7.500000000000000000 ) ) ;
#50821 = CARTESIAN_POINT ( 'NONE',  ( -45.00000000000000000, -2.024042244987997205E-14, 10.00000000000000000 ) ) ;
#50822 = VECTOR ( 'NONE', #27739, 1000.000000000000000 ) ;
#50823 = EDGE_CURVE ( 'NONE', #49491, #45655, #25638, .T. ) ;
#50824 = DIRECTION ( 'NONE',  ( -0.000000000000000000, 1.000000000000000000, 0.000000000000000000 ) ) ;
#50826 = CARTESIAN_POINT ( 'NONE',  ( -100.0429263765338135, -9.058813317711329915, -2.943386871421370898 ) ) ;
#50825 =( BOUNDED_CURVE ( )  B_SPLINE_CURVE ( 2, ( #59673, #6220, #32257, #6537, #43563, #179, #21704, #27299, #27648, #49157, #64625 ),
 .UNSPECIFIED., .F., .F. ) 
 B_SPLINE_CURVE_WITH_KNOTS ( ( 3, 2, 2, 2, 2, 3 ),
 ( 0.1195652173913016314, 0.1217391304347798520, 0.1239130434782580725, 0.1260869565217362653, 0.1282608695652145137, 0.1304347826086927065 ),
 .UNSPECIFIED. ) 
 CURVE ( )  GEOMETRIC_REPRESENTATION_ITEM ( )  RATIONAL_B_SPLINE_CURVE ( ( 1.000000000000061284, 0.9510565162950922469, 1.000000000000000000, 0.9510565162951535312, 1.000000000000000000, 0.9510565162951535312, 1.000000000000000000, 0.9510565162951535312, 1.000000000000000000, 0.9510565162952198115, 0.9999999999999337197 ) ) 
 REPRESENTATION_ITEM ( '' )  );
#50827 = APPLICATION_PROTOCOL_DEFINITION ( 'draft international standard', 'automotive_design', 1998, #15477 ) ;
#50828 = DIRECTION ( 'NONE',  ( 1.000000000000000000, 0.000000000000000000, 0.000000000000000000 ) ) ;
#50829 = CIRCLE ( 'NONE', #44146, 0.5000000000000004441 ) ;
#50830 = EDGE_CURVE ( 'NONE', #15666, #49707, #35299, .T. ) ;
#50831 = CARTESIAN_POINT ( 'NONE',  ( 2.607480562269030688, 151.5929263765338249, 8.025000000000034106 ) ) ;
#50832 = CIRCLE ( 'NONE', #68826, 0.4999999999999991118 ) ;
#50833 = CARTESIAN_POINT ( 'NONE',  ( -156.8070736234661524, 10.01517768586948698, -1.839758294383808966E-15 ) ) ;
#50834 = ADVANCED_FACE ( 'NONE', ( #45545 ), #3223, .F. ) ;
#50835 = EDGE_LOOP ( 'NONE', ( #17414, #8089, #14194, #44933, #7996, #44901, #12622, #69419 ) ) ;
#50836 = CARTESIAN_POINT ( 'NONE',  ( 36.00000000000002842, 5.000000000000000000, 77.00402776293825013 ) ) ;
#50837 = SURFACE_SIDE_STYLE ('',( #53759 ) ) ;
#50838 = ORIENTED_EDGE ( 'NONE', *, *, #35241, .T. ) ;
#50839 = CARTESIAN_POINT ( 'NONE',  ( 57.00000000000000000, 14.00000000000000000, -60.00402776293827145 ) ) ;
#50840 = VECTOR ( 'NONE', #35215, 1000.000000000000000 ) ;
#50841 = VECTOR ( 'NONE', #54019, 1000.000000000000000 ) ;
#50842 = CARTESIAN_POINT ( 'NONE',  ( 0.000000000000000000, 133.0570736234661524, -8.025000000000000355 ) ) ;
#50843 =( GEOMETRIC_REPRESENTATION_CONTEXT ( 3 ) GLOBAL_UNCERTAINTY_ASSIGNED_CONTEXT ( ( #24832 ) ) GLOBAL_UNIT_ASSIGNED_CONTEXT ( ( #9868, #42592, #15171 ) ) REPRESENTATION_CONTEXT ( 'NONE', 'WORKASPACE' ) );
#50844 = DIRECTION ( 'NONE',  ( -0.000000000000000000, -0.000000000000000000, 1.000000000000000000 ) ) ;
#50845 = FILL_AREA_STYLE_COLOUR ( '', #46320 ) ;
#50846 = AXIS2_PLACEMENT_3D ( 'NONE', #54304, #21607, #43121 ) ;
#50847 = VERTEX_POINT ( 'NONE', #24711 ) ;
#50848 = CARTESIAN_POINT ( 'NONE',  ( -94.94292637653380496, 0.000000000000000000, 9.524999999999991473 ) ) ;
#50849 = ADVANCED_FACE ( 'NONE', ( #67650 ), #19450, .F. ) ;
#50850 = CIRCLE ( 'NONE', #54202, 0.5000000000000004441 ) ;
#50851 = LINE ( 'NONE', #18499, #16528 ) ;
#50852 = DIRECTION ( 'NONE',  ( -1.156482317317873451E-16, -1.000000000000000000, 0.000000000000000000 ) ) ;
#50853 = CIRCLE ( 'NONE', #2486, 5.000000000000000000 ) ;
#50854 = STYLED_ITEM ( 'NONE', ( #39138 ), #35927 ) ;
#50855 = LINE ( 'NONE', #18827, #54196 ) ;
#50856 = CARTESIAN_POINT ( 'NONE',  ( -78.14499999999999602, -4.716976649647092401, 6.492361379858946790 ) ) ;
#50857 = ORIENTED_EDGE ( 'NONE', *, *, #25475, .T. ) ;
#50858 = PRESENTATION_LAYER_ASSIGNMENT (  '', '', ( #51972 ) ) ;
#50859 = LINE ( 'NONE', #35382, #59999 ) ;
#50860 = UNCERTAINTY_MEASURE_WITH_UNIT (LENGTH_MEASURE( 1.000000000000000082E-05 ), #27904, 'distance_accuracy_value', 'NONE');
#50861 = ORIENTED_EDGE ( 'NONE', *, *, #63605, .F. ) ;
#50862 = AXIS2_PLACEMENT_3D ( 'NONE', #23414, #49829, #23095 ) ;
#50863 = CIRCLE ( 'NONE', #20537, 18.00000000000000355 ) ;
#50864 = SURFACE_STYLE_FILL_AREA ( #67380 ) ;
#50865 = ORIENTED_EDGE ( 'NONE', *, *, #28648, .F. ) ;
#50866 = AXIS2_PLACEMENT_3D ( 'NONE', #68531, #42521, #15097 ) ;
#50867 = DIRECTION ( 'NONE',  ( 0.000000000000000000, 0.000000000000000000, -1.000000000000000000 ) ) ;
#50868 = ORIENTED_EDGE ( 'NONE', *, *, #3485, .T. ) ;
#50869 = DIRECTION ( 'NONE',  ( -1.000000000000000000, -0.000000000000000000, -0.000000000000000000 ) ) ;
#50870 =( NAMED_UNIT ( * ) SI_UNIT ( $, .STERADIAN. ) SOLID_ANGLE_UNIT ( ) );
#50871 = CARTESIAN_POINT ( 'NONE',  ( -44.50000000000000000, 10.49999999999998224, -3.000000000000000444 ) ) ;
#50872 =( NAMED_UNIT ( * ) PLANE_ANGLE_UNIT ( ) SI_UNIT ( $, .RADIAN. ) );
#50873 = CARTESIAN_POINT ( 'NONE',  ( -168.6570736234661751, 9.058813317711329915, 2.943386871421369566 ) ) ;
#50874 = DIRECTION ( 'NONE',  ( 1.000000000000000000, -0.000000000000000000, -0.000000000000000000 ) ) ;
#50875 = CARTESIAN_POINT ( 'NONE',  ( -9.058813317711337021, 116.0449999999999875, -2.943386871421374895 ) ) ;
#50876 = CARTESIAN_POINT ( 'NONE',  ( -117.0570736234661808, 0.000000000000000000, 9.524999999999991473 ) ) ;
#50877 = CIRCLE ( 'NONE', #1352, 8.999999999999994671 ) ;
#50878 = CARTESIAN_POINT ( 'NONE',  ( -183.1589919394749586, 4.545776238418753223, -8.196812015063720480 ) ) ;
#50879 = CARTESIAN_POINT ( 'NONE',  ( -84.05707362346618083, 0.000000000000000000, 9.524999999999991473 ) ) ;
#50880 = ORIENTED_EDGE ( 'NONE', *, *, #67258, .T. ) ;
#50881 = LINE ( 'NONE', #7607, #10414 ) ;
#50882 = DIRECTION ( 'NONE',  ( -0.000000000000000000, -0.000000000000000000, -1.000000000000000000 ) ) ;
#50883 = DIRECTION ( 'NONE',  ( -1.000000000000000000, 0.000000000000000000, 0.000000000000000000 ) ) ;
#50884 = CARTESIAN_POINT ( 'NONE',  ( 26.00000000000001776, 42.00000000000000000, 29.68999999999999417 ) ) ;
#50885 = CARTESIAN_POINT ( 'NONE',  ( -149.0049999999999386, 6.826472737025116366, 4.959722759717898555 ) ) ;
#50886 = DIRECTION ( 'NONE',  ( 0.000000000000000000, -1.000000000000000000, 0.000000000000000000 ) ) ;
#50887 = CARTESIAN_POINT ( 'NONE',  ( -164.3950000000000102, -6.826472737025115478, -4.959722759717899443 ) ) ;
#50888 = AXIS2_PLACEMENT_3D ( 'NONE', #22496, #11586, #628 ) ;
#50889 =( GEOMETRIC_REPRESENTATION_CONTEXT ( 3 ) GLOBAL_UNCERTAINTY_ASSIGNED_CONTEXT ( ( #12201 ) ) GLOBAL_UNIT_ASSIGNED_CONTEXT ( ( #15648, #63471, #58 ) ) REPRESENTATION_CONTEXT ( 'NONE', 'WORKASPACE' ) );
#50890 = CARTESIAN_POINT ( 'NONE',  ( -160.4949999999999761, 6.826472737025113702, -4.959722759717902107 ) ) ;
#50891 = ORIENTED_EDGE ( 'NONE', *, *, #56962, .T. ) ;
#50892 = CARTESIAN_POINT ( 'NONE',  ( 45.50000000000000000, -1.469576158976824618E-14, -10.00000000000000000 ) ) ;
#50893 = AXIS2_PLACEMENT_3D ( 'NONE', #69538, #16465, #12785 ) ;
#50894 = CARTESIAN_POINT ( 'NONE',  ( 14.98999599679679662, 118.4999999999999716, -9.500000000000000000 ) ) ;
#50895 = CARTESIAN_POINT ( 'NONE',  ( -69.95499999999998408, -7.632228543268599452, 2.479861379858951054 ) ) ;
#50896 = CARTESIAN_POINT ( 'NONE',  ( -37.98355297219490723, -12.77435968235000985, 2.829136785577898827 ) ) ;
#50897 = PRESENTATION_STYLE_ASSIGNMENT (( #45311 ) ) ;
#50898 = CARTESIAN_POINT ( 'NONE',  ( -73.64499999999998181, 4.716976649647091513, -6.492361379858946790 ) ) ;
#50899 = CARTESIAN_POINT ( 'NONE',  ( -1.166476076187854022E-15, 148.0549999999999784, 9.525000000000000355 ) ) ;
#50900 = CIRCLE ( 'NONE', #59882, 18.99999999999998934 ) ;
#50901 = CARTESIAN_POINT ( 'NONE',  ( 0.000000000000000000, 110.4999999999999858, 22.50000000000000000 ) ) ;
#50902 = ADVANCED_FACE ( 'NONE', ( #4658 ), #14397, .T. ) ;
#50903 = AXIS2_PLACEMENT_3D ( 'NONE', #8818, #7767, #34173 ) ;
#50904 = CARTESIAN_POINT ( 'NONE',  ( -195.0000000000000000, 0.000000000000000000, 9.524999999999991473 ) ) ;
#50905 = UNCERTAINTY_MEASURE_WITH_UNIT (LENGTH_MEASURE( 1.000000000000000082E-05 ), #36036, 'distance_accuracy_value', 'NONE');
#50906 = VECTOR ( 'NONE', #53787, 1000.000000000000000 ) ;
#50907 = CARTESIAN_POINT ( 'NONE',  ( 0.3542414993972760051, 42.77450856510287736, -45.47201648568073296 ) ) ;
#50908 = DIRECTION ( 'NONE',  ( -0.000000000000000000, -0.000000000000000000, 1.000000000000000000 ) ) ;
#50909 = VECTOR ( 'NONE', #24264, 1000.000000000000000 ) ;
#50910 = CARTESIAN_POINT ( 'NONE',  ( -7.647808743681030030, 110.5000000000002984, 5.677732506914710875 ) ) ;
#50911 = SURFACE_SIDE_STYLE ('',( #8357 ) ) ;
#50912 = MECHANICAL_DESIGN_GEOMETRIC_PRESENTATION_REPRESENTATION (  '', ( #58970 ), #9350 ) ;
#50913 = CARTESIAN_POINT ( 'NONE',  ( 71.74137931034481142, 36.89918356738973415, -9.500000000000000000 ) ) ;
#50914 = EDGE_CURVE ( 'NONE', #36781, #66538, #16700, .T. ) ;
#50915 = EDGE_CURVE ( 'NONE', #53532, #17136, #53221, .T. ) ;
#50916 = SURFACE_STYLE_USAGE ( .BOTH. , #1948 ) ;
#50917 = DIRECTION ( 'NONE',  ( 0.000000000000000000, 1.000000000000000000, 0.000000000000000000 ) ) ;
#50918 = ORIENTED_EDGE ( 'NONE', *, *, #28257, .F. ) ;
#50919 = VERTEX_POINT ( 'NONE', #68703 ) ;
#50920 = EDGE_CURVE ( 'NONE', #20026, #56901, #10307, .T. ) ;
#50921 = DIRECTION ( 'NONE',  ( -1.000000000000000000, -0.000000000000000000, -0.000000000000000000 ) ) ;
#50922 =( BOUNDED_CURVE ( )  B_SPLINE_CURVE ( 2, ( #29603, #44787, #39499, #39860, #51415, #61584, #13074, #3160, #23291, #34528, #1780 ),
 .UNSPECIFIED., .F., .F. ) 
 B_SPLINE_CURVE_WITH_KNOTS ( ( 3, 2, 2, 2, 2, 3 ),
 ( 0.9347826086956522174, 0.9369565217391304657, 0.9391304347826087140, 0.9413043478260869623, 0.9434782608695652106, 0.9456521739130434590 ),
 .UNSPECIFIED. ) 
 CURVE ( )  GEOMETRIC_REPRESENTATION_ITEM ( )  RATIONAL_B_SPLINE_CURVE ( ( 1.000000000000000000, 0.9510565162951535312, 1.000000000000000000, 0.9510565162951535312, 1.000000000000000000, 0.9510565162951535312, 1.000000000000000000, 0.9510565162951535312, 1.000000000000000000, 0.9510565162951535312, 1.000000000000000000 ) ) 
 REPRESENTATION_ITEM ( '' )  );
#50923 = MECHANICAL_DESIGN_GEOMETRIC_PRESENTATION_REPRESENTATION (  '', ( #9366 ), #18353 ) ;
#50924 = EDGE_CURVE ( 'NONE', #62693, #47990, #34636, .T. ) ;
#50925 = DIRECTION ( 'NONE',  ( -1.000000000000000000, 0.000000000000000000, 0.000000000000000000 ) ) ;
#50926 = DIRECTION ( 'NONE',  ( 0.000000000000000000, 0.000000000000000000, -1.000000000000000000 ) ) ;
#50927 = ORIENTED_EDGE ( 'NONE', *, *, #38372, .T. ) ;
#50928 = VERTEX_POINT ( 'NONE', #35996 ) ;
#50929 = DIRECTION ( 'NONE',  ( 0.000000000000000000, 0.000000000000000000, 1.000000000000000000 ) ) ;
#50930 = ORIENTED_EDGE ( 'NONE', *, *, #956, .T. ) ;
#50931 = DIRECTION ( 'NONE',  ( 0.000000000000000000, 0.000000000000000000, 1.000000000000000000 ) ) ;
#50932 = CARTESIAN_POINT ( 'NONE',  ( -19.89974874213240597, 115.4999999999999574, -10.00000000000000000 ) ) ;
#50933 = ORIENTED_EDGE ( 'NONE', *, *, #29984, .T. ) ;
#50934 = TOROIDAL_SURFACE ( 'NONE', #48723, 18.50000000000000355, 0.5000000000000000000 ) ;
#50935 =( GEOMETRIC_REPRESENTATION_CONTEXT ( 3 ) GLOBAL_UNCERTAINTY_ASSIGNED_CONTEXT ( ( #31238 ) ) GLOBAL_UNIT_ASSIGNED_CONTEXT ( ( #46990, #25137, #36055 ) ) REPRESENTATION_CONTEXT ( 'NONE', 'WORKASPACE' ) );
#50936 =( LENGTH_UNIT ( ) NAMED_UNIT ( * ) SI_UNIT ( .MILLI., .METRE. ) );
#50937 = CARTESIAN_POINT ( 'NONE',  ( -112.9449999999999932, -9.827790563157499189E-16, -8.024999999999991473 ) ) ;
#50938 = VERTEX_POINT ( 'NONE', #25425 ) ;
#50939 = TOROIDAL_SURFACE ( 'NONE', #67812, 7.499999999999998224, 0.5000000000000000000 ) ;
#50940 = CARTESIAN_POINT ( 'NONE',  ( -5.377101922857332461, 110.5000000000000000, -7.874436908571754934 ) ) ;
#50941 = CARTESIAN_POINT ( 'NONE',  ( -11.03049116848387001, -11.60726128400439805, -3.057421598022181719 ) ) ;
#50942 = FACE_OUTER_BOUND ( 'NONE', #65397, .T. ) ;
#50943 = VERTEX_POINT ( 'NONE', #9959 ) ;
#50944 = CARTESIAN_POINT ( 'NONE',  ( 8.437984349512095861, 143.1929263765338192, 1.550032578732817026E-15 ) ) ;
#50945 = CARTESIAN_POINT ( 'NONE',  ( 62.24999999999998579, 33.74999999999999289, -3.750000000000000000 ) ) ;
#50946 = FILL_AREA_STYLE ('',( #18239 ) ) ;
#50947 =( NAMED_UNIT ( * ) PLANE_ANGLE_UNIT ( ) SI_UNIT ( $, .RADIAN. ) );
#50948 = VECTOR ( 'NONE', #21580, 1000.000000000000000 ) ;
#50949 = ORIENTED_EDGE ( 'NONE', *, *, #25736, .F. ) ;
#50950 = MANIFOLD_SOLID_BREP ( 'Fillet4', #31758 ) ;
#50951 = PLANE ( 'NONE',  #21731 ) ;
#50952 = VERTEX_POINT ( 'NONE', #57799 ) ;
#50953 =( NAMED_UNIT ( * ) SI_UNIT ( $, .STERADIAN. ) SOLID_ANGLE_UNIT ( ) );
#50954 = CARTESIAN_POINT ( 'NONE',  ( 40.99999999999998579, 107.7459666924148252, -3.000000000000000444 ) ) ;
#50955 = CARTESIAN_POINT ( 'NONE',  ( -135.3549999999999898, -4.716976649647093289, -6.492361379858945902 ) ) ;
#50956 = MECHANICAL_DESIGN_GEOMETRIC_PRESENTATION_REPRESENTATION (  '', ( #25140 ), #68941 ) ;
#50957 = DIRECTION ( 'NONE',  ( 0.000000000000000000, 0.000000000000000000, -1.000000000000000000 ) ) ;
#50958 = ORIENTED_EDGE ( 'NONE', *, *, #30772, .T. ) ;
#50959 =( NAMED_UNIT ( * ) SI_UNIT ( $, .STERADIAN. ) SOLID_ANGLE_UNIT ( ) );
#50960 = MECHANICAL_DESIGN_GEOMETRIC_PRESENTATION_REPRESENTATION (  '', ( #45376 ), #40949 ) ;
#50961 = FILL_AREA_STYLE_COLOUR ( '', #36181 ) ;
#50962 = SURFACE_SIDE_STYLE ('',( #60454 ) ) ;
#50963 = ORIENTED_EDGE ( 'NONE', *, *, #1556, .F. ) ;
#50964 = VERTEX_POINT ( 'NONE', #9625 ) ;
#50965 = CARTESIAN_POINT ( 'NONE',  ( -31.48711616987651141, -8.174231546256825354, -1.747660327496908916 ) ) ;
#50966 = PRESENTATION_STYLE_ASSIGNMENT (( #29128 ) ) ;
#50967 = CARTESIAN_POINT ( 'NONE',  ( -49.40499999999996561, -2.607480562269069768, 8.024999999999991473 ) ) ;
#50968 = ORIENTED_EDGE ( 'NONE', *, *, #32756, .T. ) ;
#50969 = CARTESIAN_POINT ( 'NONE',  ( 23.50000000000001776, 15.00000000000000000, -27.18999999999999417 ) ) ;
#50970 = DIRECTION ( 'NONE',  ( 1.000000000000000000, 0.000000000000000000, -0.000000000000000000 ) ) ;
#50971 =( LENGTH_UNIT ( ) NAMED_UNIT ( * ) SI_UNIT ( .MILLI., .METRE. ) );
#50972 = CARTESIAN_POINT ( 'NONE',  ( -52.10707362346616378, 8.102448949553171076, -5.886773742842744461 ) ) ;
#50973 = SURFACE_STYLE_USAGE ( .BOTH. , #55553 ) ;
#50974 = DIRECTION ( 'NONE',  ( 1.000000000000000000, 0.000000000000000000, 0.000000000000000000 ) ) ;
#50975 = EDGE_LOOP ( 'NONE', ( #8504, #1002, #7824, #52073 ) ) ;
#50976 = VECTOR ( 'NONE', #48501, 1000.000000000000114 ) ;
#50977 =( NAMED_UNIT ( * ) PLANE_ANGLE_UNIT ( ) SI_UNIT ( $, .RADIAN. ) );
#50978 =( GEOMETRIC_REPRESENTATION_CONTEXT ( 3 ) GLOBAL_UNCERTAINTY_ASSIGNED_CONTEXT ( ( #58069 ) ) GLOBAL_UNIT_ASSIGNED_CONTEXT ( ( #39270, #50490, #7912 ) ) REPRESENTATION_CONTEXT ( 'NONE', 'WORKASPACE' ) );
#50979 = SURFACE_STYLE_FILL_AREA ( #13324 ) ;
#50980 = CARTESIAN_POINT ( 'NONE',  ( -106.1049999999999756, -6.826472737025115478, 4.959722759717900331 ) ) ;
#50981 = CARTESIAN_POINT ( 'NONE',  ( -27.86698944841959147, -8.499999999999998224, 0.009747179837370825370 ) ) ;
#50982 =( NAMED_UNIT ( * ) PLANE_ANGLE_UNIT ( ) SI_UNIT ( $, .RADIAN. ) );
#50983 = AXIS2_PLACEMENT_3D ( 'NONE', #57457, #31395, #69402 ) ;
#50984 = CARTESIAN_POINT ( 'NONE',  ( -102.5949999999999847, 2.607480562269072433, 8.024999999999991473 ) ) ;
#50985 = CARTESIAN_POINT ( 'NONE',  ( 8.102448949553181734, 118.5049999999999955, 5.886773742842750679 ) ) ;
#50986 = CARTESIAN_POINT ( 'NONE',  ( -67.04499999999997328, 7.632228543268600340, 2.479861379858949277 ) ) ;
#50987 = EDGE_CURVE ( 'NONE', #57704, #44431, #11035, .T. ) ;
#50988 = STYLED_ITEM ( 'NONE', ( #25899 ), #48340 ) ;
#50989 = AXIS2_PLACEMENT_3D ( 'NONE', #4888, #25990, #41183 ) ;
#50990 = DIRECTION ( 'NONE',  ( 1.000000000000000000, 0.000000000000000000, 0.000000000000000000 ) ) ;
#50991 = DIRECTION ( 'NONE',  ( -1.000000000000000000, -9.811390859391773608E-17, 0.000000000000000000 ) ) ;
#50992 = UNCERTAINTY_MEASURE_WITH_UNIT (LENGTH_MEASURE( 1.000000000000000082E-05 ), #43295, 'distance_accuracy_value', 'NONE');
#50993 = ADVANCED_FACE ( 'NONE', ( #1040 ), #8786, .T. ) ;
#50994 = CARTESIAN_POINT ( 'NONE',  ( -75.00000000000000000, 9.708372675170620525, -6.000000000000000000 ) ) ;
#50995 = COLOUR_RGB ( '', 0.40784314, 0.44705882, 0.49803922) ;
#50996 = ORIENTED_EDGE ( 'NONE', *, *, #19838, .F. ) ;
#50997 = CARTESIAN_POINT ( 'NONE',  ( -117.8929263765337794, -8.102448949553172852, -5.886773742842741797 ) ) ;
#50998 = CARTESIAN_POINT ( 'NONE',  ( -135.8949999999999818, 6.826472737025116366, 4.959722759717898555 ) ) ;
#50999 = ADVANCED_FACE ( 'NONE', ( #59502 ), #49674, .T. ) ;
#51000 = CARTESIAN_POINT ( 'NONE',  ( 68.00000000000000000, 2.776762340297169183E-15, 11.50000000000000000 ) ) ;
#51001 = ADVANCED_FACE ( 'NONE', ( #48311 ), #39158, .F. ) ;
#51002 = CARTESIAN_POINT ( 'NONE',  ( 26.25000000000001066, 19.24999999999997868, -4.000000000000000000 ) ) ;
#51003 = DIRECTION ( 'NONE',  ( 0.000000000000000000, 0.000000000000000000, 1.000000000000000000 ) ) ;
#51004 = VERTEX_POINT ( 'NONE', #64797 ) ;
#51005 = VERTEX_POINT ( 'NONE', #22232 ) ;
#51006 = AXIS2_PLACEMENT_3D ( 'NONE', #6222, #59312, #5169 ) ;
#51007 = CARTESIAN_POINT ( 'NONE',  ( 34.99999999999992895, 112.9999999999999858, -9.500000000000000000 ) ) ;
#51008 = DIRECTION ( 'NONE',  ( -1.000000000000000000, 0.000000000000000000, 0.000000000000000000 ) ) ;
#51009 = ADVANCED_FACE ( 'NONE', ( #43728 ), #14635, .T. ) ;
#51010 = VECTOR ( 'NONE', #17618, 1000.000000000000000 ) ;
#51011 = CARTESIAN_POINT ( 'NONE',  ( -74.99999999999998579, 50.00000000000000000, -10.00000000000000000 ) ) ;
#51012 = CARTESIAN_POINT ( 'NONE',  ( 3.409440450227774644, 1.719598803868655601, 7.000000000000001776 ) ) ;
#51013 = DIRECTION ( 'NONE',  ( 0.000000000000000000, -1.000000000000000000, 0.000000000000000000 ) ) ;
#51014 = CARTESIAN_POINT ( 'NONE',  ( 53.25000000000000000, 25.24999999999998579, -4.000000000000000000 ) ) ;
#51015 = EDGE_LOOP ( 'NONE', ( #34950, #14995, #37415, #57103 ) ) ;
#51016 = CARTESIAN_POINT ( 'NONE',  ( -131.9050000000000011, 2.607480562269069324, -8.024999999999993250 ) ) ;
#51017 = ORIENTED_EDGE ( 'NONE', *, *, #5007, .F. ) ;
#51018 = VECTOR ( 'NONE', #13094, 1000.000000000000000 ) ;
#51019 = DIRECTION ( 'NONE',  ( -1.000000000000000000, 0.000000000000000000, 0.000000000000000000 ) ) ;
#51020 = CARTESIAN_POINT ( 'NONE',  ( -123.8070736234661808, 10.01517768586948698, -1.839758294383808571E-15 ) ) ;
#51021 = ORIENTED_EDGE ( 'NONE', *, *, #501, .T. ) ;
#51022 = CARTESIAN_POINT ( 'NONE',  ( -172.7929263765339840, -3.094860106616026396, 9.525000000001739409 ) ) ;
#51023 = CARTESIAN_POINT ( 'NONE',  ( -97.94292637653380496, 0.000000000000000000, 9.524999999999991473 ) ) ;
#51024 = ORIENTED_EDGE ( 'NONE', *, *, #50580, .T. ) ;
#51025 = MECHANICAL_DESIGN_GEOMETRIC_PRESENTATION_REPRESENTATION (  '', ( #65626 ), #54367 ) ;
#51026 = FILL_AREA_STYLE_COLOUR ( '', #32647 ) ;
#51027 = CARTESIAN_POINT ( 'NONE',  ( 9.058813317711338797, 138.8449999999999989, -2.943386871421372675 ) ) ;
#51028 =( NAMED_UNIT ( * ) PLANE_ANGLE_UNIT ( ) SI_UNIT ( $, .RADIAN. ) );
#51029 = ORIENTED_EDGE ( 'NONE', *, *, #4252, .T. ) ;
#51030 = COLOUR_RGB ( '', 0.09019608, 0.27058824, 0.51372549) ;
#51031 = FACE_OUTER_BOUND ( 'NONE', #69391, .T. ) ;
#51032 = CARTESIAN_POINT ( 'NONE',  ( -5.598654528085808657, 138.7549999999999955, 7.705886871421373741 ) ) ;
#51033 =( NAMED_UNIT ( * ) SI_UNIT ( $, .STERADIAN. ) SOLID_ANGLE_UNIT ( ) );
#51034 = CARTESIAN_POINT ( 'NONE',  ( 41.08002123031661768, 107.6301924976394702, -3.280722492564373205 ) ) ;
#51035 = EDGE_LOOP ( 'NONE', ( #57588, #13266, #65852 ) ) ;
#51036 = CARTESIAN_POINT ( 'NONE',  ( -8.437984349512095861, 114.6929263765338050, -5.166775262442723748E-16 ) ) ;
#51037 = DIRECTION ( 'NONE',  ( 0.000000000000000000, 0.000000000000000000, -1.000000000000000000 ) ) ;
#51038 = UNCERTAINTY_MEASURE_WITH_UNIT (LENGTH_MEASURE( 1.000000000000000082E-05 ), #55225, 'distance_accuracy_value', 'NONE');
#51039 = LINE ( 'NONE', #61919, #16473 ) ;
#51040 = STYLED_ITEM ( 'NONE', ( #37792 ), #63109 ) ;
#51041 =( NAMED_UNIT ( * ) SI_UNIT ( $, .STERADIAN. ) SOLID_ANGLE_UNIT ( ) );
#51042 = ORIENTED_EDGE ( 'NONE', *, *, #18268, .T. ) ;
#51043 = CARTESIAN_POINT ( 'NONE',  ( 11.00000000000000000, 8.000000000000000000, 3.500000000000003997 ) ) ;
#51044 = ORIENTED_EDGE ( 'NONE', *, *, #25327, .F. ) ;
#51045 = LINE ( 'NONE', #39829, #29134 ) ;
#51046 = AXIS2_PLACEMENT_3D ( 'NONE', #28667, #13895, #50163 ) ;
#51047 = AXIS2_PLACEMENT_3D ( 'NONE', #43537, #64923, #65280 ) ;
#51048 = CARTESIAN_POINT ( 'NONE',  ( 8.000000000000001776, 30.99999999999998579, 3.750000000000000000 ) ) ;
#51049 = CARTESIAN_POINT ( 'NONE',  ( 14.98999599679679662, 118.4999999999999716, -10.00000000000000000 ) ) ;
#51050 = CARTESIAN_POINT ( 'NONE',  ( -163.4050000000000011, -2.607480562269069768, 8.024999999999991473 ) ) ;
#51051 = ORIENTED_EDGE ( 'NONE', *, *, #41265, .T. ) ;
#51052 = SURFACE_SIDE_STYLE ('',( #2447 ) ) ;
#51053 = UNCERTAINTY_MEASURE_WITH_UNIT (LENGTH_MEASURE( 1.000000000000000082E-05 ), #52365, 'distance_accuracy_value', 'NONE');
#51054 = EDGE_CURVE ( 'NONE', #20368, #31194, #11091, .T. ) ;
#51055 = SURFACE_STYLE_USAGE ( .BOTH. , #14435 ) ;
#51056 = LINE ( 'NONE', #28528, #59706 ) ;
#51057 = DIRECTION ( 'NONE',  ( -0.000000000000000000, 0.000000000000000000, 1.000000000000000000 ) ) ;
#51058 = DIRECTION ( 'NONE',  ( -2.312964634635740689E-15, 1.000000000000000000, -0.000000000000000000 ) ) ;
#51059 = ORIENTED_EDGE ( 'NONE', *, *, #13188, .T. ) ;
#51060 = ORIENTED_EDGE ( 'NONE', *, *, #41565, .T. ) ;
#51061 = DIRECTION ( 'NONE',  ( -1.000000000000000000, 0.000000000000000000, 0.000000000000000000 ) ) ;
#51062 = CARTESIAN_POINT ( 'NONE',  ( 48.50000000000000000, 14.49137674618942384, -7.500000000000000000 ) ) ;
#51063 = CARTESIAN_POINT ( 'NONE',  ( -60.00000000000000000, -2.024042244987997205E-14, -9.500000000000000000 ) ) ;
#51064 = CARTESIAN_POINT ( 'NONE',  ( -74.45499999999999829, 7.632228543268599452, -2.479861379858951942 ) ) ;
#51066 = VERTEX_POINT ( 'NONE', #43173 ) ;
#51065 = CIRCLE ( 'NONE', #52183, 3.499999999999999556 ) ;
#51067 =( LENGTH_UNIT ( ) NAMED_UNIT ( * ) SI_UNIT ( .MILLI., .METRE. ) );
#51068 =( NAMED_UNIT ( * ) PLANE_ANGLE_UNIT ( ) SI_UNIT ( $, .RADIAN. ) );
#51069 = CARTESIAN_POINT ( 'NONE',  ( -150.2070736234665560, 3.094860106625255458, 9.524999999995031885 ) ) ;
#51070 = CIRCLE ( 'NONE', #31963, 1.000000000000000888 ) ;
#51071 = CARTESIAN_POINT ( 'NONE',  ( -75.00000000000000000, 8.588294701370022821, -5.575869277511084299 ) ) ;
#51072 = AXIS2_PLACEMENT_3D ( 'NONE', #9826, #41855, #25287 ) ;
#51073 = ORIENTED_EDGE ( 'NONE', *, *, #23310, .F. ) ;
#51074 =( NAMED_UNIT ( * ) SI_UNIT ( $, .STERADIAN. ) SOLID_ANGLE_UNIT ( ) );
#51075 = FACE_OUTER_BOUND ( 'NONE', #67270, .T. ) ;
#51076 = EDGE_CURVE ( 'NONE', #51005, #35517, #8201, .T. ) ;
#51077 = AXIS2_PLACEMENT_3D ( 'NONE', #61894, #39449, #61211 ) ;
#51078 = ADVANCED_FACE ( 'NONE', ( #68828 ), #47769, .F. ) ;
#51079 = CARTESIAN_POINT ( 'NONE',  ( -1.166476076187854022E-15, 137.9449999999999932, 9.525000000000000355 ) ) ;
#51080 = CARTESIAN_POINT ( 'NONE',  ( -109.9449999999999932, -9.827790563157499189E-16, -8.024999999999991473 ) ) ;
#51081 = DIRECTION ( 'NONE',  ( -1.000000000000000000, -0.000000000000000000, -0.000000000000000000 ) ) ;
#51082 = CARTESIAN_POINT ( 'NONE',  ( -43.99999999999998579, 0.000000000000000000, 0.000000000000000000 ) ) ;
#51083 = UNCERTAINTY_MEASURE_WITH_UNIT (LENGTH_MEASURE( 1.000000000000000082E-05 ), #19792, 'distance_accuracy_value', 'NONE');
#51084 = EDGE_CURVE ( 'NONE', #53024, #35471, #55841, .T. ) ;
#51085 = VECTOR ( 'NONE', #60993, 1000.000000000000000 ) ;
#51087 = DIRECTION ( 'NONE',  ( 0.000000000000000000, 0.000000000000000000, 1.000000000000000000 ) ) ;
#51086 = CARTESIAN_POINT ( 'NONE',  ( -96.65707362346617515, 9.058813317711329915, 2.943386871421369566 ) ) ;
#51088 = EDGE_CURVE ( 'NONE', #33844, #31555, #48191, .T. ) ;
#51089 = CARTESIAN_POINT ( 'NONE',  ( -144.2929263765337566, 3.094860106618428031, -9.524999999999993250 ) ) ;
#51090 = CARTESIAN_POINT ( 'NONE',  ( -161.9950000000000045, -6.826472737025115478, 4.959722759717900331 ) ) ;
#51091 = VECTOR ( 'NONE', #39411, 1000.000000000000000 ) ;
#51092 = ADVANCED_FACE ( 'NONE', ( #53341 ), #48094, .F. ) ;
#51093 = COLOUR_RGB ( '', 0.08235294, 0.09019608, 0.10196078) ;
#51095 = DIRECTION ( 'NONE',  ( -0.000000000000000000, -1.000000000000000000, -0.000000000000000000 ) ) ;
#51094 = VECTOR ( 'NONE', #32482, 1000.000000000000000 ) ;
#51096 = ORIENTED_EDGE ( 'NONE', *, *, #59549, .T. ) ;
#51097 = LINE ( 'NONE', #23644, #17103 ) ;
#51098 = VERTEX_POINT ( 'NONE', #43846 ) ;
#51099 = AXIS2_PLACEMENT_3D ( 'NONE', #48811, #45533, #39542 ) ;
#51100 = CYLINDRICAL_SURFACE ( 'NONE', #58837, 1.000000000000000888 ) ;
#51101 = ADVANCED_FACE ( 'NONE', ( #11793 ), #6170, .T. ) ;
#51102 =( LENGTH_UNIT ( ) NAMED_UNIT ( * ) SI_UNIT ( .MILLI., .METRE. ) );
#51103 = DIRECTION ( 'NONE',  ( -0.000000000000000000, -0.000000000000000000, -1.000000000000000000 ) ) ;
#51104 = CARTESIAN_POINT ( 'NONE',  ( 0.000000000000000000, 154.9999999999999716, -22.49999999999999645 ) ) ;
#51105 = CIRCLE ( 'NONE', #16291, 0.5000000000000004441 ) ;
#51106 =( LENGTH_UNIT ( ) NAMED_UNIT ( * ) SI_UNIT ( .MILLI., .METRE. ) );
#51107 = ORIENTED_EDGE ( 'NONE', *, *, #28655, .T. ) ;
#51108 = CARTESIAN_POINT ( 'NONE',  ( -156.5049999999999955, -6.826472737025113702, -4.959722759717900331 ) ) ;
#51109 = ORIENTED_EDGE ( 'NONE', *, *, #23903, .T. ) ;
#51110 = CARTESIAN_POINT ( 'NONE',  ( -21.02379604162863913, 114.4999999999999574, -10.00000000000000000 ) ) ;
#51111 = CARTESIAN_POINT ( 'NONE',  ( -9.000000000000003553, 24.74999999999998579, -3.750000000000000000 ) ) ;
#51112 = ORIENTED_EDGE ( 'NONE', *, *, #49662, .T. ) ;
#51113 = B_SPLINE_CURVE_WITH_KNOTS ( 'NONE', 3,
 ( #20677, #67464, #9088, #42187, #14009, #63579 ),
 .UNSPECIFIED., .F., .F.,
 ( 4, 2, 4 ),
 ( 0.000000000000000000, 0.0003058591473678551830, 0.0006117182947357103660 ),
 .UNSPECIFIED. ) ;
#51114 = SURFACE_STYLE_USAGE ( .BOTH. , #61624 ) ;
#51115 = CARTESIAN_POINT ( 'NONE',  ( -57.80707362346616662, 10.01517768586948698, -1.839758294383808966E-15 ) ) ;
#51116 = CARTESIAN_POINT ( 'NONE',  ( 0.000000000000000000, 115.4449999999999932, -9.525000000000000355 ) ) ;
#51117 = VERTEX_POINT ( 'NONE', #27601 ) ;
#51118 = FILL_AREA_STYLE_COLOUR ( '', #4885 ) ;
#51119 = CARTESIAN_POINT ( 'NONE',  ( -9.058813317711338797, 111.4549999999999841, 2.943386871421373563 ) ) ;
#51120 = CARTESIAN_POINT ( 'NONE',  ( -71.60499999999998977, 6.826472737025113702, -4.959722759717902107 ) ) ;
#51121 = VECTOR ( 'NONE', #37189, 1000.000000000000000 ) ;
#51122 = CARTESIAN_POINT ( 'NONE',  ( -6.826472737025120807, 121.5070736234661410, -4.959722759717907437 ) ) ;
#51123 = CARTESIAN_POINT ( 'NONE',  ( -5.598654528085808657, 141.7549999999999955, 7.705886871421373741 ) ) ;
#51124 = UNCERTAINTY_MEASURE_WITH_UNIT (LENGTH_MEASURE( 1.000000000000000082E-05 ), #47660, 'distance_accuracy_value', 'NONE');
#51125 = FILL_AREA_STYLE_COLOUR ( '', #44412 ) ;
#51126 =( NAMED_UNIT ( * ) SI_UNIT ( $, .STERADIAN. ) SOLID_ANGLE_UNIT ( ) );
#51127 = CARTESIAN_POINT ( 'NONE',  ( 21.02379605245189964, 114.6413612702713465, 10.00000000000000000 ) ) ;
#51128 = LINE ( 'NONE', #12416, #54445 ) ;
#51129 = ORIENTED_EDGE ( 'NONE', *, *, #48594, .T. ) ;
#51130 = DIRECTION ( 'NONE',  ( -1.000000000000000000, 1.047380211910525101E-15, 0.000000000000000000 ) ) ;
#51131 = CARTESIAN_POINT ( 'NONE',  ( -71.49999999999998579, 64.07124727947029896, -7.500000000000000000 ) ) ;
#51132 = CARTESIAN_POINT ( 'NONE',  ( -53.24499999999999034, -4.716976649647093289, -6.492361379858945902 ) ) ;
#51133 = ORIENTED_EDGE ( 'NONE', *, *, #62836, .F. ) ;
#51134 = DIRECTION ( 'NONE',  ( -0.000000000000000000, -1.000000000000000000, -0.000000000000000000 ) ) ;
#51135 = CIRCLE ( 'NONE', #10661, 13.00000000000000533 ) ;
#51136 = EDGE_CURVE ( 'NONE', #59005, #51323, #28650, .T. ) ;
#51137 = CIRCLE ( 'NONE', #1604, 30.00000000000000000 ) ;
#51138 = CARTESIAN_POINT ( 'NONE',  ( 22.99999999999995381, 5.000000000000000000, 32.00402776293825724 ) ) ;
#51139 = FILL_AREA_STYLE_COLOUR ( '', #46526 ) ;
#51140 = ORIENTED_EDGE ( 'NONE', *, *, #18440, .T. ) ;
#51141 = CARTESIAN_POINT ( 'NONE',  ( -49.19499999999998607, 8.437984349512086979, -1.550032578732815448E-15 ) ) ;
#51142 = ORIENTED_EDGE ( 'NONE', *, *, #65532, .T. ) ;
#51143 = STYLED_ITEM ( 'NONE', ( #483 ), #64083 ) ;
#51144 =( NAMED_UNIT ( * ) SI_UNIT ( $, .STERADIAN. ) SOLID_ANGLE_UNIT ( ) );
#51145 = CARTESIAN_POINT ( 'NONE',  ( -102.9549999999999841, -7.632228543268599452, 2.479861379858951054 ) ) ;
#51146 = VERTEX_POINT ( 'NONE', #66290 ) ;
#51147 = CYLINDRICAL_SURFACE ( 'NONE', #60903, 0.5000000000000004441 ) ;
#51148 = COLOUR_RGB ( '', 0.72549020, 0.75294118, 0.79215686) ;
#51149 = CARTESIAN_POINT ( 'NONE',  ( -139.4070736234661751, 3.094860106618428031, -9.524999999999993250 ) ) ;
#51150 = CIRCLE ( 'NONE', #12963, 24.00000000000001421 ) ;
#51151 = FACE_BOUND ( 'NONE', #58208, .T. ) ;
#51152 = CARTESIAN_POINT ( 'NONE',  ( 9.058813317711337021, 138.5449999999999875, 2.943386871421375783 ) ) ;
#51153 = CARTESIAN_POINT ( 'NONE',  ( -85.70707362346617231, -3.094860106618431139, -9.524999999999991473 ) ) ;
#51154 = PRODUCT_RELATED_PRODUCT_CATEGORY ( 'part', '', ( #21518 ) ) ;
#51155 = EDGE_CURVE ( 'NONE', #15634, #59936, #69497, .T. ) ;
#51156 = FILL_AREA_STYLE ('',( #15280 ) ) ;
#51157 = PRESENTATION_STYLE_ASSIGNMENT (( #14918 ) ) ;
#51158 = CARTESIAN_POINT ( 'NONE',  ( 15.98999599679679839, 99.99999999999998579, 7.500000000000000000 ) ) ;
#51159 = CARTESIAN_POINT ( 'NONE',  ( -6.239160159721276244, 2.499999999999999556, 3.193457606803197013 ) ) ;
#51160 = EDGE_CURVE ( 'NONE', #41299, #27775, #34284, .T. ) ;
#51161 = CIRCLE ( 'NONE', #56778, 0.5000000000000004441 ) ;
#51162 = CARTESIAN_POINT ( 'NONE',  ( -122.0049999999999670, 6.826472737025116366, 4.959722759717898555 ) ) ;
#51163 = EDGE_CURVE ( 'NONE', #51004, #26634, #22350, .T. ) ;
#51164 = CARTESIAN_POINT ( 'NONE',  ( -137.5449999999999875, -7.632228543268600340, -2.479861379858950166 ) ) ;
#51165 = AXIS2_PLACEMENT_3D ( 'NONE', #50346, #13382, #35561 ) ;
#51166 = CARTESIAN_POINT ( 'NONE',  ( -115.0449999999999875, 7.632228543268600340, 2.479861379858949277 ) ) ;
#51167 = DIRECTION ( 'NONE',  ( 1.000000000000000000, -7.709882115452469292E-16, 0.000000000000000000 ) ) ;
#51168 = VERTEX_POINT ( 'NONE', #7220 ) ;
#51169 = DIRECTION ( 'NONE',  ( 1.000000000000000000, 0.000000000000000000, -1.300977106640434891E-16 ) ) ;
#51170 = ADVANCED_FACE ( 'NONE', ( #59625 ), #25697, .T. ) ;
#51171 = FILL_AREA_STYLE_COLOUR ( '', #60869 ) ;
#51172 = AXIS2_PLACEMENT_3D ( 'NONE', #58597, #58954, #10764 ) ;
#51173 = CARTESIAN_POINT ( 'NONE',  ( -175.9429263765337907, 0.000000000000000000, 9.524999999999991473 ) ) ;
#51174 = DIRECTION ( 'NONE',  ( -1.000000000000000000, 0.000000000000000000, 0.000000000000000000 ) ) ;
#51175 = EDGE_CURVE ( 'NONE', #47726, #53938, #41451, .T. ) ;
#51176 = CYLINDRICAL_SURFACE ( 'NONE', #26744, 0.5000000000000004441 ) ;
#51177 = CARTESIAN_POINT ( 'NONE',  ( 0.9999999999999991118, 43.00000000000000000, -74.38749456993816978 ) ) ;
#51178 = ORIENTED_EDGE ( 'NONE', *, *, #18513, .T. ) ;
#51179 = CARTESIAN_POINT ( 'NONE',  ( -84.44292637653380496, -1.166476076187852838E-15, -9.524999999999991473 ) ) ;
#51180 = CONTEXT_DEPENDENT_SHAPE_REPRESENTATION ( #61262, #42345 ) ;
#51181 = AXIS2_PLACEMENT_3D ( 'NONE', #60718, #34357, #1594 ) ;
#51182 = CARTESIAN_POINT ( 'NONE',  ( -179.5429263765338135, 9.058813317711329915, 2.943386871421369566 ) ) ;
#51183 = CARTESIAN_POINT ( 'NONE',  ( -13.50000000000000355, 27.99999999999998934, 3.750000000000000000 ) ) ;
#51184 = CARTESIAN_POINT ( 'NONE',  ( -78.95707362346617231, 9.058813317711329915, -2.943386871421373119 ) ) ;
#51185 = CARTESIAN_POINT ( 'NONE',  ( 24.21231517720798010, 113.4999999999999858, -7.500000000000000000 ) ) ;
#51186 = ORIENTED_EDGE ( 'NONE', *, *, #13114, .T. ) ;
#51187 = CARTESIAN_POINT ( 'NONE',  ( 23.21231517720797655, 118.4999999999999716, 7.000000000000000000 ) ) ;
#51188 = FILL_AREA_STYLE_COLOUR ( '', #28633 ) ;
#51189 = CARTESIAN_POINT ( 'NONE',  ( 36.00000000000002842, 5.000000000000000000, -32.00402776293825724 ) ) ;
#51191 = ORIENTED_EDGE ( 'NONE', *, *, #46435, .T. ) ;
#51190 = VECTOR ( 'NONE', #8978, 1000.000000000000000 ) ;
#51192 = SURFACE_STYLE_USAGE ( .BOTH. , #12847 ) ;
#51193 = VECTOR ( 'NONE', #3329, 1000.000000000000000 ) ;
#51194 = ADVANCED_FACE ( 'NONE', ( #13512 ), #63365, .T. ) ;
#51195 = CARTESIAN_POINT ( 'NONE',  ( 6.826472737025119919, 138.0070736234661695, 4.959722759717908325 ) ) ;
#51196 = EDGE_LOOP ( 'NONE', ( #35792, #21531, #51710 ) ) ;
#51197 = CARTESIAN_POINT ( 'NONE',  ( 0.000000000000000000, 0.000000000000000000, 2.000000000000000000 ) ) ;
#51198 = DIRECTION ( 'NONE',  ( 0.000000000000000000, 0.000000000000000000, -1.000000000000000000 ) ) ;
#51199 = CARTESIAN_POINT ( 'NONE',  ( 0.000000000000000000, 0.000000000000000000, 0.2499999999999924227 ) ) ;
#51200 = ORIENTED_EDGE ( 'NONE', *, *, #8102, .T. ) ;
#51201 = FILL_AREA_STYLE ('',( #34649 ) ) ;
#51202 = VECTOR ( 'NONE', #15237, 1000.000000000000000 ) ;
#51203 = FACE_OUTER_BOUND ( 'NONE', #43643, .T. ) ;
#51204 = DIRECTION ( 'NONE',  ( 0.000000000000000000, 0.000000000000000000, 1.000000000000000000 ) ) ;
#51205 = FILL_AREA_STYLE_COLOUR ( '', #28345 ) ;
#51206 = CIRCLE ( 'NONE', #20881, 1.000000000000000000 ) ;
#51207 = MECHANICAL_DESIGN_GEOMETRIC_PRESENTATION_REPRESENTATION (  '', ( #50117 ), #36644 ) ;
#51208 = FACE_OUTER_BOUND ( 'NONE', #56907, .T. ) ;
#51209 = CARTESIAN_POINT ( 'NONE',  ( -79.94499999999999318, -9.827790563157499189E-16, -8.024999999999991473 ) ) ;
#51210 = ORIENTED_EDGE ( 'NONE', *, *, #12210, .T. ) ;
#51211 = AXIS2_PLACEMENT_3D ( 'NONE', #33178, #44118, #38834 ) ;
#51212 = ORIENTED_EDGE ( 'NONE', *, *, #33291, .T. ) ;
#51213 = CARTESIAN_POINT ( 'NONE',  ( -76.49292637653380211, -8.102448949553174629, 5.886773742842742685 ) ) ;
#51214 =( NAMED_UNIT ( * ) PLANE_ANGLE_UNIT ( ) SI_UNIT ( $, .RADIAN. ) );
#51215 = B_SPLINE_CURVE_WITH_KNOTS ( 'NONE', 3,
 ( #42970, #9195, #36990, #52117, #14820, #3872, #20059, #26384, #4576, #26031, #62978, #47568, #25354, #68978, #42292, #36300, #4211, #46874, #63677, #30969, #52467, #15521, #53142, #10227, #4933, #69316 ),
 .UNSPECIFIED., .F., .F.,
 ( 4, 2, 2, 2, 2, 2, 2, 2, 2, 2, 2, 2, 4 ),
 ( 0.000000000000000000, 0.0002642488042135191515, 0.0005284976084270383030, 0.0007927464126405575628, 0.001056995216854076606, 0.001585492825281106452, 0.002113990433708136298, 0.002642488042135166144, 0.002906736846348681718, 0.003170985650562197725, 0.003435234454775714166, 0.003699483258989229740, 0.004227980867416260453 ),
 .UNSPECIFIED. ) ;
#51216 = LINE ( 'NONE', #52278, #68471 ) ;
#51217 = ORIENTED_EDGE ( 'NONE', *, *, #46893, .T. ) ;
#51218 = CARTESIAN_POINT ( 'NONE',  ( 8.250000000000001776, 30.99999999999998579, -3.750000000000000000 ) ) ;
#51219 = ORIENTED_EDGE ( 'NONE', *, *, #20599, .T. ) ;
#51220 = CARTESIAN_POINT ( 'NONE',  ( 3.000000000000030198, 38.00000000000000711, 90.00000000000000000 ) ) ;
#51221 = SURFACE_SIDE_STYLE ('',( #29030 ) ) ;
#51222 = SURFACE_STYLE_USAGE ( .BOTH. , #45636 ) ;
#51223 = CARTESIAN_POINT ( 'NONE',  ( -173.1570736234662036, -9.058813317711329915, -2.943386871421370898 ) ) ;
#51224 = LINE ( 'NONE', #41043, #27473 ) ;
#51225 = CARTESIAN_POINT ( 'NONE',  ( -7.647808743681030030, 110.5000000000002984, 5.677732506914710875 ) ) ;
#51226 = CARTESIAN_POINT ( 'NONE',  ( -111.8070736234661666, 10.01517768586948698, -1.839758294383808571E-15 ) ) ;
#51227 = AXIS2_PLACEMENT_3D ( 'NONE', #1511, #39586, #22686 ) ;
#51228 = ADVANCED_FACE ( 'NONE', ( #55751 ), #20074, .T. ) ;
#51229 = DIRECTION ( 'NONE',  ( 0.000000000000000000, 0.000000000000000000, 1.000000000000000000 ) ) ;
#51230 = VERTEX_POINT ( 'NONE', #31333 ) ;
#51231 = CARTESIAN_POINT ( 'NONE',  ( 2.607480562269030688, 121.5929263765338249, 8.025000000000034106 ) ) ;
#51232 = CARTESIAN_POINT ( 'NONE',  ( 0.000000000000000000, 36.75000000000000000, 4.000000000000000000 ) ) ;
#51234 = SPHERICAL_SURFACE ( 'NONE', #66904, 0.2500000000000000000 ) ;
#51233 = CIRCLE ( 'NONE', #53496, 18.00000000000000355 ) ;
#51235 = ADVANCED_FACE ( 'NONE', ( #12826 ), #50474, .T. ) ;
#51236 = CARTESIAN_POINT ( 'NONE',  ( -146.4550000000000125, 7.632228543268599452, -2.479861379858951942 ) ) ;
#51237 =( NAMED_UNIT ( * ) PLANE_ANGLE_UNIT ( ) SI_UNIT ( $, .RADIAN. ) );
#51238 = CARTESIAN_POINT ( 'NONE',  ( -6.087059439501893543, 111.0522570712095103, -6.604466948054985131 ) ) ;
#51239 = CARTESIAN_POINT ( 'NONE',  ( -164.5449999999999875, -7.632228543268600340, -2.479861379858950166 ) ) ;
#51240 = CIRCLE ( 'NONE', #20913, 1.000000000000000888 ) ;
#51241 = AXIS2_PLACEMENT_3D ( 'NONE', #18887, #56896, #61793 ) ;
#51242 = CARTESIAN_POINT ( 'NONE',  ( -145.0449999999999875, 7.632228543268600340, 2.479861379858949277 ) ) ;
#51243 =( BOUNDED_CURVE ( )  B_SPLINE_CURVE ( 2, ( #59066, #10885, #47894, #27026, #21790, #43304, #65021, #45357, #27719, #11918, #66775 ),
 .UNSPECIFIED., .F., .F. ) 
 B_SPLINE_CURVE_WITH_KNOTS ( ( 3, 2, 2, 2, 2, 3 ),
 ( 0.02173913043478211196, 0.02391304347826032212, 0.02608695652173853227, 0.02826086956521674243, 0.03043478260869495605, 0.03260869565217316274 ),
 .UNSPECIFIED. ) 
 CURVE ( )  GEOMETRIC_REPRESENTATION_ITEM ( )  RATIONAL_B_SPLINE_CURVE ( ( 1.000000000000011102, 0.9510565162951423179, 1.000000000000000000, 0.9510565162951535312, 1.000000000000000000, 0.9510565162951535312, 1.000000000000000000, 0.9510565162951535312, 1.000000000000000000, 0.9510565162951704066, 0.9999999999999831246 ) ) 
 REPRESENTATION_ITEM ( '' )  );
#51244 = ORIENTED_EDGE ( 'NONE', *, *, #26539, .F. ) ;
#51245 = SURFACE_STYLE_FILL_AREA ( #3341 ) ;
#51246 = CARTESIAN_POINT ( 'NONE',  ( -67.25499999999998124, -4.716976649647092401, 6.492361379858946790 ) ) ;
#51247 = CARTESIAN_POINT ( 'NONE',  ( 71.74137931034479720, 63.10081643261027295, 9.500000000000000000 ) ) ;
#51248 = FACE_OUTER_BOUND ( 'NONE', #9298, .T. ) ;
#51249 = EDGE_CURVE ( 'NONE', #60023, #46872, #38112, .T. ) ;
#51250 = CIRCLE ( 'NONE', #23183, 1.000000000000000888 ) ;
#51251 = CARTESIAN_POINT ( 'NONE',  ( -59.54499999999998749, -7.632228543268600340, -2.479861379858950166 ) ) ;
#51252 = CARTESIAN_POINT ( 'NONE',  ( -5.598654528085806881, 149.8549999999999898, -7.705886871421374629 ) ) ;
#51253 = CARTESIAN_POINT ( 'NONE',  ( -0.3558155365998594277, 2.493171897977953577, -7.000000000000002665 ) ) ;
#51254 = CIRCLE ( 'NONE', #5190, 1.000000000000000888 ) ;
#51255 = DIRECTION ( 'NONE',  ( -1.298988366203102052E-16, 0.05527174654752588928, -0.9984713486292864371 ) ) ;
#51256 = VECTOR ( 'NONE', #39203, 1000.000000000000000 ) ;
#51257 = CARTESIAN_POINT ( 'NONE',  ( -159.8070736234661808, 10.01517768586948698, -1.839758294383808966E-15 ) ) ;
#51258 = CARTESIAN_POINT ( 'NONE',  ( -20.43039690318515156, 114.8190495831791793, -10.32375696423105360 ) ) ;
#51259 = CARTESIAN_POINT ( 'NONE',  ( -5.812336001415696174, 110.6020537967688284, 7.425621158969065938 ) ) ;
#51260 = DIRECTION ( 'NONE',  ( -1.000000000000000000, -0.000000000000000000, -0.000000000000000000 ) ) ;
#51261 = DIRECTION ( 'NONE',  ( 0.000000000000000000, 1.000000000000000000, -0.000000000000000000 ) ) ;
#51262 = FILL_AREA_STYLE ('',( #8697 ) ) ;
#51263 = CARTESIAN_POINT ( 'NONE',  ( -2.243484957755116138, -2.233878551459168360, -9.000000000000003553 ) ) ;
#51264 = ORIENTED_EDGE ( 'NONE', *, *, #33292, .F. ) ;
#51265 = EDGE_LOOP ( 'NONE', ( #33892, #43264, #35932, #51834 ) ) ;
#51266 = LINE ( 'NONE', #67093, #15067 ) ;
#51267 = EDGE_CURVE ( 'NONE', #7454, #20493, #5486, .T. ) ;
#51268 = PLANE ( 'NONE',  #31618 ) ;
#51269 = DIRECTION ( 'NONE',  ( -1.156482317317873451E-16, 1.000000000000000000, 0.000000000000000000 ) ) ;
#51270 = CARTESIAN_POINT ( 'NONE',  ( 60.00000000000000000, 117.4999999999999716, -9.500000000000000000 ) ) ;
#51271 = VERTEX_POINT ( 'NONE', #50820 ) ;
#51272 = ORIENTED_EDGE ( 'NONE', *, *, #48826, .F. ) ;
#51273 = DIRECTION ( 'NONE',  ( -1.000000000000000000, -0.000000000000000000, -0.000000000000000000 ) ) ;
#51274 = CARTESIAN_POINT ( 'NONE',  ( 33.00000000000002132, 14.00000000000000000, 79.00402776293826435 ) ) ;
#51275 = VERTEX_POINT ( 'NONE', #67004 ) ;
#51276 = CARTESIAN_POINT ( 'NONE',  ( 8.102448949553181734, 112.5049999999999670, 5.886773742842750679 ) ) ;
#51277 = DIRECTION ( 'NONE',  ( 0.000000000000000000, 0.000000000000000000, 1.000000000000000000 ) ) ;
#51278 = PRESENTATION_LAYER_ASSIGNMENT (  '', '', ( #23220 ) ) ;
#51279 = VERTEX_POINT ( 'NONE', #3903 ) ;
#51280 = FACE_OUTER_BOUND ( 'NONE', #25844, .T. ) ;
#51281 = CARTESIAN_POINT ( 'NONE',  ( -110.3949999999999818, -6.826472737025115478, -4.959722759717899443 ) ) ;
#51282 = ORIENTED_EDGE ( 'NONE', *, *, #12454, .T. ) ;
#51283 = CARTESIAN_POINT ( 'NONE',  ( 25.75000000000001066, 21.74999999999998224, -4.000000000000000000 ) ) ;
#51284 = FACE_OUTER_BOUND ( 'NONE', #63805, .T. ) ;
#51285 = CARTESIAN_POINT ( 'NONE',  ( -15.00000000000000000, -10.90871211463571022, -5.000000000000000000 ) ) ;
#51286 = CARTESIAN_POINT ( 'NONE',  ( -40.99999999999998579, 108.0000000000000000, 3.500000000000000000 ) ) ;
#51287 = ORIENTED_EDGE ( 'NONE', *, *, #52743, .F. ) ;
#51288 = CARTESIAN_POINT ( 'NONE',  ( -6.826472737025120807, 144.3929263765338078, -4.959722759717907437 ) ) ;
#51289 = CARTESIAN_POINT ( 'NONE',  ( -53.79830117337122175, -9.480064694306525652, -3.454096298679953048 ) ) ;
#51290 = SURFACE_STYLE_USAGE ( .BOTH. , #19617 ) ;
#51291 = SURFACE_STYLE_FILL_AREA ( #8724 ) ;
#51292 = CIRCLE ( 'NONE', #54645, 0.5000000000000004441 ) ;
#51293 = LINE ( 'NONE', #34744, #27783 ) ;
#51294 = ORIENTED_EDGE ( 'NONE', *, *, #10650, .T. ) ;
#51295 = EDGE_CURVE ( 'NONE', #62934, #33844, #42999, .T. ) ;
#51296 = DIRECTION ( 'NONE',  ( 0.000000000000000000, 0.000000000000000000, 1.000000000000000000 ) ) ;
#51297 = ORIENTED_EDGE ( 'NONE', *, *, #26210, .T. ) ;
#51298 = DIRECTION ( 'NONE',  ( 0.000000000000000000, 0.000000000000000000, -1.000000000000000000 ) ) ;
#51299 = CARTESIAN_POINT ( 'NONE',  ( 0.000000000000000000, 139.0570736234661808, -8.025000000000000355 ) ) ;
#51300 = DIRECTION ( 'NONE',  ( 1.000000000000000000, 0.000000000000000000, 0.000000000000000000 ) ) ;
#51301 = CARTESIAN_POINT ( 'NONE',  ( -158.1570736234661751, -9.058813317711329915, -2.943386871421370898 ) ) ;
#51302 = CARTESIAN_POINT ( 'NONE',  ( -123.8049999999999926, -8.437984349512085203, 5.166775262442717831E-16 ) ) ;
#51303 = PRESENTATION_STYLE_ASSIGNMENT (( #15087 ) ) ;
#51304 = VERTEX_POINT ( 'NONE', #42642 ) ;
#51305 = LINE ( 'NONE', #52010, #11855 ) ;
#51306 = CARTESIAN_POINT ( 'NONE',  ( -75.00000000000000000, 36.00000000000000711, 9.581200359586295789 ) ) ;
#51307 = DIRECTION ( 'NONE',  ( -1.000000000000000000, 0.000000000000000000, 0.000000000000000000 ) ) ;
#51308 = ORIENTED_EDGE ( 'NONE', *, *, #58628, .F. ) ;
#51309 =( GEOMETRIC_REPRESENTATION_CONTEXT ( 3 ) GLOBAL_UNCERTAINTY_ASSIGNED_CONTEXT ( ( #11484 ) ) GLOBAL_UNIT_ASSIGNED_CONTEXT ( ( #19867, #14974, #71 ) ) REPRESENTATION_CONTEXT ( 'NONE', 'WORKASPACE' ) );
#51310 = EDGE_LOOP ( 'NONE', ( #63472, #15645, #47722, #19146, #23795, #58763, #62834, #55880, #38767, #1115, #21218, #31750, #40107, #27864, #51217, #21543, #57266, #45346, #62504, #45426, #64433, #11150, #61238, #37747, #10466, #22946, #52509, #5796 ) ) ;
#51311 = CARTESIAN_POINT ( 'NONE',  ( -29.91370621994246548, -7.761720733523306492, -0.7755720678496379472 ) ) ;
#51312 = LINE ( 'NONE', #46063, #60393 ) ;
#51313 = VERTEX_POINT ( 'NONE', #5291 ) ;
#51314 = CARTESIAN_POINT ( 'NONE',  ( -124.4070736234668857, 3.094860106606395433, -9.525000000008736478 ) ) ;
#51315 = EDGE_CURVE ( 'NONE', #8903, #54396, #11277, .T. ) ;
#51316 = CARTESIAN_POINT ( 'NONE',  ( -183.3549999999999898, -4.716976649647093289, -6.492361379858945902 ) ) ;
#51317 = CARTESIAN_POINT ( 'NONE',  ( 31.00000000000000355, 42.00000000000000000, -36.50000000000000000 ) ) ;
#51318 = CYLINDRICAL_SURFACE ( 'NONE', #53782, 0.5000000000000004441 ) ;
#51319 = CARTESIAN_POINT ( 'NONE',  ( -52.70707362346615099, -3.094860106618431139, -9.524999999999991473 ) ) ;
#51320 = ADVANCED_FACE ( 'NONE', ( #49276 ), #38052, .T. ) ;
#51321 = CARTESIAN_POINT ( 'NONE',  ( -173.0949999999999989, -2.607480562269071545, -8.024999999999991473 ) ) ;
#51322 = LINE ( 'NONE', #44362, #24110 ) ;
#51323 = VERTEX_POINT ( 'NONE', #58784 ) ;
#51324 = EDGE_CURVE ( 'NONE', #47479, #20521, #11628, .T. ) ;
#51325 = CARTESIAN_POINT ( 'NONE',  ( 0.000000000000000000, 118.0570736234661524, -8.025000000000000355 ) ) ;
#51326 = CARTESIAN_POINT ( 'NONE',  ( -90.80499999999996419, -8.437984349512085203, 5.166775262442717831E-16 ) ) ;
#51327 = CARTESIAN_POINT ( 'NONE',  ( 2.182090618630762702, 154.5000000000000284, -9.281935407964393647 ) ) ;
#51328 = FILL_AREA_STYLE ('',( #52038 ) ) ;
#51329 = PLANE ( 'NONE',  #50572 ) ;
#51330 = STYLED_ITEM ( 'NONE', ( #65227 ), #65333 ) ;
#51331 = EDGE_CURVE ( 'NONE', #60430, #44784, #64404, .T. ) ;
#51332 = CARTESIAN_POINT ( 'NONE',  ( -101.8449999999999847, -7.632228543268599452, 2.479861379858951054 ) ) ;
#51333 = CARTESIAN_POINT ( 'NONE',  ( 3.094860106618431583, 121.2049999999999841, 9.525000000000000355 ) ) ;
#51334 = AXIS2_PLACEMENT_3D ( 'NONE', #65482, #54899, #6726 ) ;
#51335 = CARTESIAN_POINT ( 'NONE',  ( -63.74499999999998323, 4.716976649647094177, 6.492361379858945902 ) ) ;
#51336 = PRESENTATION_STYLE_ASSIGNMENT (( #28456 ) ) ;
#51337 = STYLED_ITEM ( 'NONE', ( #58381 ), #50279 ) ;
#51338 = DIRECTION ( 'NONE',  ( 0.000000000000000000, -1.000000000000000000, 0.000000000000000000 ) ) ;
#51339 = CARTESIAN_POINT ( 'NONE',  ( 27.99999999999999645, 5.000000000000000000, -72.00402776293822171 ) ) ;
#51340 =( BOUNDED_CURVE ( )  B_SPLINE_CURVE ( 2, ( #64845, #16693, #65189, #31796, #42415, #38158, #32846, #54289, #10370, #53276, #6107 ),
 .UNSPECIFIED., .F., .F. ) 
 B_SPLINE_CURVE_WITH_KNOTS ( ( 3, 2, 2, 2, 2, 3 ),
 ( 0.0004239242079884921540, 0.002173913043478220130, 0.004347826086956429852, 0.006521739130434640007, 0.008695652173912851030, 0.01086956521739105945 ),
 .UNSPECIFIED. ) 
 CURVE ( )  GEOMETRIC_REPRESENTATION_ITEM ( )  RATIONAL_B_SPLINE_CURVE ( ( 0.9846338866369153120, 0.9606007469754098693, 1.000000000000000000, 0.9510565162951535312, 1.000000000000000000, 0.9510565162951535312, 1.000000000000000000, 0.9510565162951535312, 1.000000000000000000, 0.9510565162951590823, 0.9999999999999944489 ) ) 
 REPRESENTATION_ITEM ( '' )  );
#51341 =( NAMED_UNIT ( * ) PLANE_ANGLE_UNIT ( ) SI_UNIT ( $, .RADIAN. ) );
#51342 = ORIENTED_EDGE ( 'NONE', *, *, #16304, .T. ) ;
#51343 = CARTESIAN_POINT ( 'NONE',  ( -110.6929263765338050, 10.01517768586948698, -1.839758294383808571E-15 ) ) ;
#51344 = CARTESIAN_POINT ( 'NONE',  ( -127.4950000000000045, 6.826472737025113702, -4.959722759717902107 ) ) ;
#51345 = DIRECTION ( 'NONE',  ( 0.000000000000000000, 0.000000000000000000, -1.000000000000000000 ) ) ;
#51346 = VECTOR ( 'NONE', #55615, 1000.000000000000000 ) ;
#51347 = FACE_OUTER_BOUND ( 'NONE', #15481, .T. ) ;
#51349 =( LENGTH_UNIT ( ) NAMED_UNIT ( * ) SI_UNIT ( .MILLI., .METRE. ) );
#51348 = DIRECTION ( 'NONE',  ( 1.000000000000000000, 0.000000000000000000, 0.000000000000000000 ) ) ;
#51350 = PRESENTATION_STYLE_ASSIGNMENT (( #39097 ) ) ;
#51351 = VERTEX_POINT ( 'NONE', #48260 ) ;
#51352 = ORIENTED_EDGE ( 'NONE', *, *, #46754, .T. ) ;
#51353 = CARTESIAN_POINT ( 'NONE',  ( 30.99999999999998579, 5.000000000000000000, 72.00402776293822171 ) ) ;
#51354 = PRESENTATION_STYLE_ASSIGNMENT (( #29895 ) ) ;
#51355 = DIRECTION ( 'NONE',  ( -1.000000000000000000, -0.000000000000000000, -0.000000000000000000 ) ) ;
#51356 = CARTESIAN_POINT ( 'NONE',  ( -126.2070736234668686, 3.094860106630264784, 9.524999999991395683 ) ) ;
#51357 = ORIENTED_EDGE ( 'NONE', *, *, #57841, .F. ) ;
#51358 = CARTESIAN_POINT ( 'NONE',  ( -134.1550000000000011, 7.632228543268600340, 2.479861379858949277 ) ) ;
#51359 = ORIENTED_EDGE ( 'NONE', *, *, #45504, .F. ) ;
#51360 = CARTESIAN_POINT ( 'NONE',  ( 33.00000000000001421, 15.00000000000000000, 36.49999999999999289 ) ) ;
#51361 = CARTESIAN_POINT ( 'NONE',  ( -120.0570736234661808, 0.000000000000000000, 9.524999999999991473 ) ) ;
#51362 = ORIENTED_EDGE ( 'NONE', *, *, #39279, .F. ) ;
#51363 = CARTESIAN_POINT ( 'NONE',  ( 5.196152422706629359, 9.000000000000008882, 7.500000000000000000 ) ) ;
#51364 = ORIENTED_EDGE ( 'NONE', *, *, #29472, .F. ) ;
#51365 = FILL_AREA_STYLE_COLOUR ( '', #18628 ) ;
#51366 = CARTESIAN_POINT ( 'NONE',  ( -9.058813317711337021, 137.0449999999999875, -2.943386871421374895 ) ) ;
#51367 = PRESENTATION_STYLE_ASSIGNMENT (( #30228 ) ) ;
#51368 = ORIENTED_EDGE ( 'NONE', *, *, #57852, .T. ) ;
#51369 = CARTESIAN_POINT ( 'NONE',  ( 10.00000000000001776, 42.25685517452260598, -28.66913060635885913 ) ) ;
#51370 = CARTESIAN_POINT ( 'NONE',  ( -8.102448949553179958, 141.6049999999999613, 5.886773742842747126 ) ) ;
#51371 = DIRECTION ( 'NONE',  ( 1.000000000000000000, 0.000000000000000000, -0.000000000000000000 ) ) ;
#51372 = SURFACE_SIDE_STYLE ('',( #19706 ) ) ;
#51373 = PRODUCT_DEFINITION_SHAPE ( 'NONE', 'NONE',  #69702 ) ;
#51374 = ORIENTED_EDGE ( 'NONE', *, *, #56954, .F. ) ;
#51375 = CARTESIAN_POINT ( 'NONE',  ( 0.000000000000000000, 113.9429263765338192, -8.025000000000000355 ) ) ;
#51376 = AXIS2_PLACEMENT_3D ( 'NONE', #43141, #58925, #64550 ) ;
#51377 = FACE_OUTER_BOUND ( 'NONE', #15062, .T. ) ;
#51378 = CARTESIAN_POINT ( 'NONE',  ( -16.75000000000000000, -0.9999999999999995559, 19.00000000000000000 ) ) ;
#51379 =( GEOMETRIC_REPRESENTATION_CONTEXT ( 3 ) GLOBAL_UNCERTAINTY_ASSIGNED_CONTEXT ( ( #29748 ) ) GLOBAL_UNIT_ASSIGNED_CONTEXT ( ( #19720, #57352, #30956 ) ) REPRESENTATION_CONTEXT ( 'NONE', 'WORKASPACE' ) );
#51380 = ORIENTED_EDGE ( 'NONE', *, *, #52123, .T. ) ;
#51381 = EDGE_CURVE ( 'NONE', #53103, #67023, #29080, .T. ) ;
#51382 = CYLINDRICAL_SURFACE ( 'NONE', #40843, 0.2500000000000002220 ) ;
#51383 = EDGE_LOOP ( 'NONE', ( #63262, #10978, #7647, #67655 ) ) ;
#51384 = DIRECTION ( 'NONE',  ( 1.000000000000000000, 0.000000000000000000, 0.000000000000000000 ) ) ;
#51385 = FACE_OUTER_BOUND ( 'NONE', #16551, .T. ) ;
#51386 = CARTESIAN_POINT ( 'NONE',  ( -190.0000000000000000, 0.000000000000000000, 0.000000000000000000 ) ) ;
#51387 = CARTESIAN_POINT ( 'NONE',  ( -166.8549999999999898, 4.716976649647094177, 6.492361379858945902 ) ) ;
#51388 = ORIENTED_EDGE ( 'NONE', *, *, #8361, .F. ) ;
#51389 = DIRECTION ( 'NONE',  ( 0.000000000000000000, 0.000000000000000000, 1.000000000000000000 ) ) ;
#51390 = ADVANCED_FACE ( 'NONE', ( #315 ), #27435, .F. ) ;
#51391 = EDGE_CURVE ( 'NONE', #8806, #52357, #3380, .T. ) ;
#51392 = LINE ( 'NONE', #9188, #50840 ) ;
#51393 = CARTESIAN_POINT ( 'NONE',  ( -57.11974195712092239, -8.499999999999996447, 7.999999999999972466 ) ) ;
#51394 = CARTESIAN_POINT ( 'NONE',  ( 75.00000000000000000, 19.90218225813096353, 6.307374275523923934 ) ) ;
#51395 = VERTEX_POINT ( 'NONE', #16930 ) ;
#51396 = STYLED_ITEM ( 'NONE', ( #31148 ), #67420 ) ;
#51397 = EDGE_CURVE ( 'NONE', #51672, #4018, #43775, .T. ) ;
#51398 = ORIENTED_EDGE ( 'NONE', *, *, #20434, .F. ) ;
#51399 = CARTESIAN_POINT ( 'NONE',  ( -6.062177826491072175, -3.499999999999998668, 0.000000000000000000 ) ) ;
#51400 = CIRCLE ( 'NONE', #23316, 0.5000000000000004441 ) ;
#51401 = CARTESIAN_POINT ( 'NONE',  ( -5.710692600061824997, 2.499999999999999112, 4.108790270285303414 ) ) ;
#51402 = CARTESIAN_POINT ( 'NONE',  ( -71.75499999999998124, 4.716976649647091513, -6.492361379858946790 ) ) ;
#51403 = ORIENTED_EDGE ( 'NONE', *, *, #67587, .T. ) ;
#51404 = EDGE_CURVE ( 'NONE', #1721, #7517, #27980, .T. ) ;
#51405 =( NAMED_UNIT ( * ) PLANE_ANGLE_UNIT ( ) SI_UNIT ( $, .RADIAN. ) );
#51406 = EDGE_CURVE ( 'NONE', #15243, #39399, #47144, .T. ) ;
#51407 = EDGE_CURVE ( 'NONE', #23681, #8511, #3263, .T. ) ;
#51408 = DIRECTION ( 'NONE',  ( 0.000000000000000000, 0.000000000000000000, -1.000000000000000000 ) ) ;
#51409 = CARTESIAN_POINT ( 'NONE',  ( 34.99999999999992895, 112.9999999999999858, 7.000000000000000000 ) ) ;
#51410 = APPLICATION_CONTEXT ( 'automotive_design' ) ;
#51411 = ADVANCED_FACE ( 'NONE', ( #44725 ), #22391, .T. ) ;
#51412 = CARTESIAN_POINT ( 'NONE',  ( -74.12583008533032114, 9.273068908601683091, -6.223864456579094373 ) ) ;
#51413 = ORIENTED_EDGE ( 'NONE', *, *, #50290, .F. ) ;
#51414 = CARTESIAN_POINT ( 'NONE',  ( 23.14659390890733448, 27.39756892443129743, -27.21001191564729282 ) ) ;
#51416 =( NAMED_UNIT ( * ) SI_UNIT ( $, .STERADIAN. ) SOLID_ANGLE_UNIT ( ) );
#51415 = CARTESIAN_POINT ( 'NONE',  ( -53.45707362346615810, -9.058813317711329915, 2.943386871421371787 ) ) ;
#51417 = CARTESIAN_POINT ( 'NONE',  ( 3.094860106618431583, 138.0949999999999989, 9.525000000000000355 ) ) ;
#51418 = CARTESIAN_POINT ( 'NONE',  ( -96.74499999999999034, 4.716976649647094177, 6.492361379858945902 ) ) ;
#51419 = CARTESIAN_POINT ( 'NONE',  ( 39.24999999999999289, 16.24999999999997513, 4.000000000000000000 ) ) ;
#51420 = CARTESIAN_POINT ( 'NONE',  ( -40.99999999999998579, 107.7459666924148394, -3.000000000000000444 ) ) ;
#51421 = AXIS2_PLACEMENT_3D ( 'NONE', #62475, #30444, #56151 ) ;
#51422 = CARTESIAN_POINT ( 'NONE',  ( -145.1929263765338192, -10.01517768586948698, 6.132527647946031529E-16 ) ) ;
#51423 = SURFACE_STYLE_FILL_AREA ( #2841 ) ;
#51424 = PRESENTATION_STYLE_ASSIGNMENT (( #18117 ) ) ;
#51425 = CARTESIAN_POINT ( 'NONE',  ( -169.7949999999999875, 2.607480562269068880, -8.024999999999993250 ) ) ;
#51426 = STYLED_ITEM ( 'NONE', ( #45947 ), #50492 ) ;
#51427 = CARTESIAN_POINT ( 'NONE',  ( 6.062177826491070398, 3.500000000000002665, 0.000000000000000000 ) ) ;
#51428 = LINE ( 'NONE', #66201, #46258 ) ;
#51429 = ORIENTED_EDGE ( 'NONE', *, *, #63538, .T. ) ;
#51430 = AXIS2_PLACEMENT_3D ( 'NONE', #29431, #30454, #19578 ) ;
#51431 = DIRECTION ( 'NONE',  ( 0.000000000000000000, 0.000000000000000000, 1.000000000000000000 ) ) ;
#51432 = ORIENTED_EDGE ( 'NONE', *, *, #54628, .T. ) ;
#51433 = CARTESIAN_POINT ( 'NONE',  ( 1.000000000000000000, 1.000000000000000888, -4.000000000000000000 ) ) ;
#51434 = ADVANCED_FACE ( 'NONE', ( #60484 ), #49623, .F. ) ;
#51435 = SURFACE_SIDE_STYLE ('',( #34904 ) ) ;
#51436 = CARTESIAN_POINT ( 'NONE',  ( -45.00000000000000000, 8.121151660575840481, 6.396433738441380079 ) ) ;
#51437 = CARTESIAN_POINT ( 'NONE',  ( -173.4570736234661865, -9.058813317711329915, 2.943386871421371787 ) ) ;
#51438 = CARTESIAN_POINT ( 'NONE',  ( 0.000000000000000000, 27.74999999999998224, 3.750000000000000000 ) ) ;
#51439 =( GEOMETRIC_REPRESENTATION_CONTEXT ( 3 ) GLOBAL_UNCERTAINTY_ASSIGNED_CONTEXT ( ( #58732 ) ) GLOBAL_UNIT_ASSIGNED_CONTEXT ( ( #28654, #29349, #59985 ) ) REPRESENTATION_CONTEXT ( 'NONE', 'WORKASPACE' ) );
#51440 = ORIENTED_EDGE ( 'NONE', *, *, #26651, .F. ) ;
#51441 = CARTESIAN_POINT ( 'NONE',  ( -163.1049999999999898, -6.826472737025113702, 4.959722759717902107 ) ) ;
#51442 = EDGE_LOOP ( 'NONE', ( #6722, #38431, #5832, #42257 ) ) ;
#51443 = CARTESIAN_POINT ( 'NONE',  ( 109.0067032876572171, 13.00000000000000178, 19.20378738324562917 ) ) ;
#51444 = VERTEX_POINT ( 'NONE', #34464 ) ;
#51445 =( LENGTH_UNIT ( ) NAMED_UNIT ( * ) SI_UNIT ( .MILLI., .METRE. ) );
#51446 = B_SPLINE_CURVE_WITH_KNOTS ( 'NONE', 3,
 ( #56301, #7446, #67214, #28869, #50352, #39832, #62285, #2079, #66527, #2443 ),
 .UNSPECIFIED., .F., .F.,
 ( 4, 2, 2, 2, 4 ),
 ( 0.000000000000000000, 0.001344558393249514153, 0.002689116786499028307, 0.004033675179748542894, 0.005378233572998056614 ),
 .UNSPECIFIED. ) ;
#51447 = DIRECTION ( 'NONE',  ( -1.000000000000000000, 0.000000000000000000, -0.000000000000000000 ) ) ;
#51448 = CARTESIAN_POINT ( 'NONE',  ( -10.01517768586949231, 116.1949999999999932, -6.132527647946036459E-16 ) ) ;
#51449 = VERTEX_POINT ( 'NONE', #22892 ) ;
#51450 =( LENGTH_UNIT ( ) NAMED_UNIT ( * ) SI_UNIT ( .MILLI., .METRE. ) );
#51451 = DIRECTION ( 'NONE',  ( 0.000000000000000000, 1.000000000000000000, 0.000000000000000000 ) ) ;
#51452 = CARTESIAN_POINT ( 'NONE',  ( -74.60500000000000398, 6.826472737025113702, -4.959722759717902107 ) ) ;
#51453 = CARTESIAN_POINT ( 'NONE',  ( 17.00000000000000711, 27.74999999999998224, -3.750000000000000000 ) ) ;
#51454 = ORIENTED_EDGE ( 'NONE', *, *, #34335, .T. ) ;
#51455 = CARTESIAN_POINT ( 'NONE',  ( -9.058813317711337021, 141.1549999999999727, -2.943386871421374895 ) ) ;
#51456 = CARTESIAN_POINT ( 'NONE',  ( -41.49999999999997868, 10.49999999999998224, 3.500000000000000000 ) ) ;
#51457 = SURFACE_STYLE_USAGE ( .BOTH. , #7503 ) ;
#51458 = CARTESIAN_POINT ( 'NONE',  ( 20.04014546381213435, 115.4999999869038163, 10.00000000000000000 ) ) ;
#51459 = ADVANCED_FACE ( 'NONE', ( #55921 ), #2392, .F. ) ;
#51460 =( LENGTH_UNIT ( ) NAMED_UNIT ( * ) SI_UNIT ( .MILLI., .METRE. ) );
#51461 = VERTEX_POINT ( 'NONE', #61517 ) ;
#51462 = DIRECTION ( 'NONE',  ( 1.000000000000000000, 0.000000000000000000, -0.000000000000000000 ) ) ;
#51463 = CARTESIAN_POINT ( 'NONE',  ( -55.94499999999999318, -9.827790563157499189E-16, -8.024999999999991473 ) ) ;
#51464 = ORIENTED_EDGE ( 'NONE', *, *, #33913, .T. ) ;
#51465 = CARTESIAN_POINT ( 'NONE',  ( 2.652578976365602692, 110.9659062983237732, 8.678865135533694541 ) ) ;
#51466 = ADVANCED_FACE ( 'NONE', ( #44389 ), #17627, .T. ) ;
#51467 = DIRECTION ( 'NONE',  ( 0.000000000000000000, -1.000000000000000000, 0.000000000000000000 ) ) ;
#51468 = CARTESIAN_POINT ( 'NONE',  ( -8.921435019309294474E-16, -7.500000000000000888, 1.000000000000000000 ) ) ;
#51469 =( NAMED_UNIT ( * ) SI_UNIT ( $, .STERADIAN. ) SOLID_ANGLE_UNIT ( ) );
#51470 = VERTEX_POINT ( 'NONE', #14059 ) ;
#51471 = CARTESIAN_POINT ( 'NONE',  ( 179.4361977533476136, 0.000000000000000000, 103.7004518695250823 ) ) ;
#51472 = ORIENTED_EDGE ( 'NONE', *, *, #61390, .F. ) ;
#51473 = VECTOR ( 'NONE', #9371, 1000.000000000000000 ) ;
#51474 = CARTESIAN_POINT ( 'NONE',  ( 0.000000000000000000, 2.299999999999999822, 0.000000000000000000 ) ) ;
#51475 = CARTESIAN_POINT ( 'NONE',  ( -103.4049999999999869, -2.607480562269069768, 8.024999999999991473 ) ) ;
#51476 = ORIENTED_EDGE ( 'NONE', *, *, #55194, .T. ) ;
#51477 = CARTESIAN_POINT ( 'NONE',  ( -195.0000000000000000, 0.000000000000000000, 0.000000000000000000 ) ) ;
#51478 = EDGE_CURVE ( 'NONE', #11986, #681, #21223, .T. ) ;
#51479 = CARTESIAN_POINT ( 'NONE',  ( -143.0070736234661695, -8.102448949553172852, -5.886773742842741797 ) ) ;
#51480 = DIRECTION ( 'NONE',  ( -1.000000000000000000, -1.073081856240828566E-16, 0.000000000000000000 ) ) ;
#51481 = CARTESIAN_POINT ( 'NONE',  ( -3.094860106618434248, 143.7949999999999875, 9.525000000000000355 ) ) ;
#51482 = COLOUR_RGB ( '', 0.31764706, 0.68627451, 0.89019608) ;
#51483 = CARTESIAN_POINT ( 'NONE',  ( -71.00707362346615525, -8.102448949553172852, -5.886773742842741797 ) ) ;
#51484 = EDGE_CURVE ( 'NONE', #16813, #41256, #56250, .T. ) ;
#51485 = CARTESIAN_POINT ( 'NONE',  ( -184.0000000000000000, 1.044011396273115718E-15, 8.524999999999977263 ) ) ;
#51486 =( LENGTH_UNIT ( ) NAMED_UNIT ( * ) SI_UNIT ( .MILLI., .METRE. ) );
#51487 = PRESENTATION_LAYER_ASSIGNMENT (  '', '', ( #36970 ) ) ;
#51488 = SURFACE_SIDE_STYLE ('',( #30025 ) ) ;
#51489 = CARTESIAN_POINT ( 'NONE',  ( -120.0549999999999926, -9.827790563157499189E-16, -8.024999999999991473 ) ) ;
#51490 = CARTESIAN_POINT ( 'NONE',  ( -71.49999999999998579, 64.07124727947029896, 7.500000000000000000 ) ) ;
#51491 = SURFACE_STYLE_USAGE ( .BOTH. , #2560 ) ;
#51492 = CARTESIAN_POINT ( 'NONE',  ( -126.7449999999999903, 4.716976649647094177, 6.492361379858945902 ) ) ;
#51493 = CARTESIAN_POINT ( 'NONE',  ( -117.5949999999999847, 2.607480562269072433, 8.024999999999991473 ) ) ;
#51494 = PRESENTATION_STYLE_ASSIGNMENT (( #46966 ) ) ;
#51495 = ORIENTED_EDGE ( 'NONE', *, *, #9987, .T. ) ;
#51496 = DIRECTION ( 'NONE',  ( 1.000000000000000000, 0.000000000000000000, 0.000000000000000000 ) ) ;
#51497 = DIRECTION ( 'NONE',  ( 0.000000000000000000, 0.000000000000000000, 1.000000000000000000 ) ) ;
#51498 = VECTOR ( 'NONE', #53154, 1000.000000000000000 ) ;
#51499 = CARTESIAN_POINT ( 'NONE',  ( -173.0929263765337964, 3.094860106618433360, 9.524999999999991473 ) ) ;
#51500 = CARTESIAN_POINT ( 'NONE',  ( -53.69499999999999318, -8.437984349512085203, 5.166775262442717831E-16 ) ) ;
#51501 = VECTOR ( 'NONE', #24310, 1000.000000000000000 ) ;
#51502 = DIRECTION ( 'NONE',  ( -0.000000000000000000, -1.000000000000000000, 0.000000000000000000 ) ) ;
#51503 = AXIS2_PLACEMENT_3D ( 'NONE', #40922, #29978, #63025 ) ;
#51504 = CYLINDRICAL_SURFACE ( 'NONE', #53724, 4.000000000000000000 ) ;
#51505 = DIRECTION ( 'NONE',  ( -1.000000000000000000, 0.000000000000000000, 0.000000000000000000 ) ) ;
#51506 = VERTEX_POINT ( 'NONE', #25296 ) ;
#51507 = CARTESIAN_POINT ( 'NONE',  ( -85.64292637653379359, -5.598654528085801552, 7.705886871421367523 ) ) ;
#51508 = COLOUR_RGB ( '', 0.66274510, 0.83137255, 0.94901961) ;
#51509 = PRESENTATION_STYLE_ASSIGNMENT (( #24757 ) ) ;
#51510 = FILL_AREA_STYLE_COLOUR ( '', #21446 ) ;
#51511 = ADVANCED_FACE ( 'NONE', ( #40461 ), #56617, .F. ) ;
#51512 = CARTESIAN_POINT ( 'NONE',  ( 71.49999999999998579, 119.9999999999997868, 7.500000000000000000 ) ) ;
#51513 = DIRECTION ( 'NONE',  ( -1.000000000000000000, 0.000000000000000000, 0.000000000000000000 ) ) ;
#51514 = FACE_OUTER_BOUND ( 'NONE', #54461, .T. ) ;
#51515 = STYLED_ITEM ( 'NONE', ( #20877 ), #66640 ) ;
#51516 = SPHERICAL_SURFACE ( 'NONE', #59733, 0.5000000000000000000 ) ;
#51517 = ORIENTED_EDGE ( 'NONE', *, *, #11357, .F. ) ;
#51518 = CARTESIAN_POINT ( 'NONE',  ( 12.25000000000000355, 30.74999999999998579, -4.000000000000000000 ) ) ;
#51519 = SURFACE_STYLE_USAGE ( .BOTH. , #56813 ) ;
#51520 = DIRECTION ( 'NONE',  ( 0.000000000000000000, 0.000000000000000000, 1.000000000000000000 ) ) ;
#51521 = ORIENTED_EDGE ( 'NONE', *, *, #60236, .T. ) ;
#51522 = CARTESIAN_POINT ( 'NONE',  ( -4.716976649647097730, 133.3570736234661638, -6.492361379858953896 ) ) ;
#51523 = CIRCLE ( 'NONE', #21189, 0.5000000000000004441 ) ;
#51524 = FILL_AREA_STYLE ('',( #24774 ) ) ;
#51525 = CARTESIAN_POINT ( 'NONE',  ( 2.607480562269071989, 128.7070736234661865, 8.025000000000002132 ) ) ;
#51526 = VERTEX_POINT ( 'NONE', #46094 ) ;
#51527 = LINE ( 'NONE', #19157, #63055 ) ;
#51528 = CARTESIAN_POINT ( 'NONE',  ( -104.1549999999999869, 7.632228543268600340, 2.479861379858949277 ) ) ;
#51529 = CARTESIAN_POINT ( 'NONE',  ( 34.99999999999992895, 112.9999999999999858, -7.000000000000000000 ) ) ;
#51530 = VECTOR ( 'NONE', #23444, 1000.000000000000000 ) ;
#51531 =( NAMED_UNIT ( * ) SI_UNIT ( $, .STERADIAN. ) SOLID_ANGLE_UNIT ( ) );
#51532 = ORIENTED_EDGE ( 'NONE', *, *, #68968, .T. ) ;
#51533 = CARTESIAN_POINT ( 'NONE',  ( -94.04292637653379927, -9.058813317711329915, -2.943386871421370898 ) ) ;
#51534 = ADVANCED_FACE ( 'NONE', ( #40817 ), #62234, .T. ) ;
#51535 = CARTESIAN_POINT ( 'NONE',  ( 10.00000000000000711, 50.00000000000000000, -54.99999999999998579 ) ) ;
#51536 = EDGE_CURVE ( 'NONE', #36186, #35924, #22444, .T. ) ;
#51537 = CARTESIAN_POINT ( 'NONE',  ( -171.4429263765337907, -1.166476076187852838E-15, -9.524999999999991473 ) ) ;
#51538 = CARTESIAN_POINT ( 'NONE',  ( 75.00000000000000000, -2.215169945516535778E-14, 10.00000000000000000 ) ) ;
#51539 = CARTESIAN_POINT ( 'NONE',  ( -77.24499999999997613, -4.716976649647093289, -6.492361379858945902 ) ) ;
#51540 = VERTEX_POINT ( 'NONE', #21393 ) ;
#51541 =( NAMED_UNIT ( * ) PLANE_ANGLE_UNIT ( ) SI_UNIT ( $, .RADIAN. ) );
#51542 = EDGE_CURVE ( 'NONE', #24428, #58318, #19226, .T. ) ;
#51543 =( LENGTH_UNIT ( ) NAMED_UNIT ( * ) SI_UNIT ( .MILLI., .METRE. ) );
#51544 = AXIS2_PLACEMENT_3D ( 'NONE', #28447, #44705, #13682 ) ;
#51545 = UNCERTAINTY_MEASURE_WITH_UNIT (LENGTH_MEASURE( 1.000000000000000082E-05 ), #11998, 'distance_accuracy_value', 'NONE');
#51546 = ORIENTED_EDGE ( 'NONE', *, *, #28578, .T. ) ;
#51547 = FILL_AREA_STYLE_COLOUR ( '', #3253 ) ;
#51548 = DIRECTION ( 'NONE',  ( 1.000000000000000000, -0.000000000000000000, 0.000000000000000000 ) ) ;
#51549 = EDGE_CURVE ( 'NONE', #60674, #42583, #37004, .T. ) ;
#51550 = AXIS2_PLACEMENT_3D ( 'NONE', #63510, #58233, #10057 ) ;
#51551 =( NAMED_UNIT ( * ) PLANE_ANGLE_UNIT ( ) SI_UNIT ( $, .RADIAN. ) );
#51552 = ORIENTED_EDGE ( 'NONE', *, *, #23588, .T. ) ;
#51553 = PRESENTATION_STYLE_ASSIGNMENT (( #18514 ) ) ;
#51554 = ORIENTED_EDGE ( 'NONE', *, *, #39932, .T. ) ;
#51555 =( GEOMETRIC_REPRESENTATION_CONTEXT ( 3 ) GLOBAL_UNCERTAINTY_ASSIGNED_CONTEXT ( ( #16985 ) ) GLOBAL_UNIT_ASSIGNED_CONTEXT ( ( #41478, #21037, #58003 ) ) REPRESENTATION_CONTEXT ( 'NONE', 'WORKASPACE' ) );
#51556 = ADVANCED_FACE ( 'NONE', ( #48875 ), #30256, .T. ) ;
#51557 = LINE ( 'NONE', #56844, #39246 ) ;
#51558 = CARTESIAN_POINT ( 'NONE',  ( 62.24999999999998579, 33.99999999999999289, -3.750000000000000000 ) ) ;
#51559 = VECTOR ( 'NONE', #19694, 1000.000000000000000 ) ;
#51560 = CARTESIAN_POINT ( 'NONE',  ( -166.7070736234661865, -3.094860106618431139, -9.524999999999991473 ) ) ;
#51561 = DIRECTION ( 'NONE',  ( 0.000000000000000000, 0.000000000000000000, 1.000000000000000000 ) ) ;
#51562 = CARTESIAN_POINT ( 'NONE',  ( -8.102448949553179958, 113.4949999999999761, 5.886773742842747126 ) ) ;
#51563 = MECHANICAL_DESIGN_GEOMETRIC_PRESENTATION_REPRESENTATION (  '', ( #48239 ), #69530 ) ;
#51564 = CARTESIAN_POINT ( 'NONE',  ( -102.2070736234661865, 3.094860106618433360, 9.524999999999991473 ) ) ;
#51565 = CARTESIAN_POINT ( 'NONE',  ( -7.511572993685801073E-16, 2.500000000000000000, 7.000000000000000888 ) ) ;
#51566 = EDGE_CURVE ( 'NONE', #2689, #28436, #68920, .T. ) ;
#51567 = FACE_OUTER_BOUND ( 'NONE', #59052, .T. ) ;
#51568 = VERTEX_POINT ( 'NONE', #575 ) ;
#51569 =( GEOMETRIC_REPRESENTATION_CONTEXT ( 3 ) GLOBAL_UNCERTAINTY_ASSIGNED_CONTEXT ( ( #35599 ) ) GLOBAL_UNIT_ASSIGNED_CONTEXT ( ( #3811, #52410, #41169 ) ) REPRESENTATION_CONTEXT ( 'NONE', 'WORKASPACE' ) );
#51570 = FILL_AREA_STYLE_COLOUR ( '', #9355 ) ;
#51571 = CIRCLE ( 'NONE', #32425, 1.000000000000000888 ) ;
#51572 = FACE_OUTER_BOUND ( 'NONE', #42855, .T. ) ;
#51573 = CARTESIAN_POINT ( 'NONE',  ( 0.000000000000000000, 149.9999999999999716, 0.000000000000000000 ) ) ;
#51574 =( NAMED_UNIT ( * ) SI_UNIT ( $, .STERADIAN. ) SOLID_ANGLE_UNIT ( ) );
#51575 = CARTESIAN_POINT ( 'NONE',  ( -153.3549999999999898, -4.716976649647093289, -6.492361379858945902 ) ) ;
#51576 = DIRECTION ( 'NONE',  ( -0.000000000000000000, -1.000000000000000000, 0.000000000000000000 ) ) ;
#51577 = CARTESIAN_POINT ( 'NONE',  ( -167.9950000000000045, -6.826472737025115478, 4.959722759717900331 ) ) ;
#51578 = STYLED_ITEM ( 'NONE', ( #31400 ), #15038 ) ;
#51579 = CARTESIAN_POINT ( 'NONE',  ( -147.8950000000000102, 6.826472737025115478, 4.959722759717899443 ) ) ;
#51580 = ORIENTED_EDGE ( 'NONE', *, *, #63399, .F. ) ;
#51581 = COLOUR_RGB ( '', 0.09019608, 0.27058824, 0.51372549) ;
#51582 =( LENGTH_UNIT ( ) NAMED_UNIT ( * ) SI_UNIT ( .MILLI., .METRE. ) );
#51583 = LINE ( 'NONE', #13949, #21086 ) ;
#51584 = FILL_AREA_STYLE_COLOUR ( '', #50702 ) ;
#51585 = UNCERTAINTY_MEASURE_WITH_UNIT (LENGTH_MEASURE( 1.000000000000000082E-05 ), #22731, 'distance_accuracy_value', 'NONE');
#51586 = CARTESIAN_POINT ( 'NONE',  ( -66.65499999999998693, -7.632228543268600340, -2.479861379858950166 ) ) ;
#51587 = CARTESIAN_POINT ( 'NONE',  ( 0.000000000000000000, 0.000000000000000000, 2.000000000000000000 ) ) ;
#51589 = CARTESIAN_POINT ( 'NONE',  ( -167.3929263765338078, 8.102448949553176405, 5.886773742842740909 ) ) ;
#51588 = CIRCLE ( 'NONE', #59393, 8.999999999999994671 ) ;
#51590 = CARTESIAN_POINT ( 'NONE',  ( -66.44499999999999318, 0.000000000000000000, 8.024999999999991473 ) ) ;
#51591 = CARTESIAN_POINT ( 'NONE',  ( -9.058813317711338797, 153.4549999999999841, 2.943386871421373563 ) ) ;
#51592 = CYLINDRICAL_SURFACE ( 'NONE', #57853, 1.000000000000000888 ) ;
#51593 = UNCERTAINTY_MEASURE_WITH_UNIT (LENGTH_MEASURE( 1.000000000000000082E-05 ), #5704, 'distance_accuracy_value', 'NONE');
#51594 = CARTESIAN_POINT ( 'NONE',  ( 45.00000000000000000, -1.469576158976824618E-14, -7.000000000000000888 ) ) ;
#51595 = MECHANICAL_DESIGN_GEOMETRIC_PRESENTATION_REPRESENTATION (  '', ( #44906 ), #7803 ) ;
#51596 = DIRECTION ( 'NONE',  ( -0.000000000000000000, -0.000000000000000000, 1.000000000000000000 ) ) ;
#51597 = VECTOR ( 'NONE', #62025, 1000.000000000000000 ) ;
#51598 = FILL_AREA_STYLE ('',( #56883 ) ) ;
#51599 = AXIS2_PLACEMENT_3D ( 'NONE', #39667, #23805, #7976 ) ;
#51600 = FACE_OUTER_BOUND ( 'NONE', #34638, .T. ) ;
#51601 = VERTEX_POINT ( 'NONE', #221 ) ;
#51602 = AXIS2_PLACEMENT_3D ( 'NONE', #66693, #50521, #13919 ) ;
#51603 = ORIENTED_EDGE ( 'NONE', *, *, #55771, .F. ) ;
#51604 = CARTESIAN_POINT ( 'NONE',  ( -60.80707362346617373, 10.01517768586948698, -1.839758294383808966E-15 ) ) ;
#51605 = STYLED_ITEM ( 'NONE', ( #10005 ), #33625 ) ;
#51606 = UNCERTAINTY_MEASURE_WITH_UNIT (LENGTH_MEASURE( 1.000000000000000082E-05 ), #11068, 'distance_accuracy_value', 'NONE');
#51608 = PRESENTATION_LAYER_ASSIGNMENT (  '', '', ( #11181 ) ) ;
#51607 = DIRECTION ( 'NONE',  ( 0.000000000000000000, 1.000000000000000000, 0.000000000000000000 ) ) ;
#51609 = VECTOR ( 'NONE', #46988, 1000.000000000000000 ) ;
#51610 = ADVANCED_FACE ( 'NONE', ( #4511 ), #21752, .T. ) ;
#51612 = SURFACE_SIDE_STYLE ('',( #23242 ) ) ;
#51611 = AXIS2_PLACEMENT_3D ( 'NONE', #40599, #62013, #30010 ) ;
#51613 = CARTESIAN_POINT ( 'NONE',  ( -45.00000000000000711, 9.680295737756338781, 6.198572516085028461 ) ) ;
#51614 = PRESENTATION_LAYER_ASSIGNMENT (  '', '', ( #58401 ) ) ;
#51616 = EDGE_CURVE ( 'NONE', #49241, #10695, #53085, .T. ) ;
#51615 = CARTESIAN_POINT ( 'NONE',  ( -77.30707362346615241, -10.01517768586948698, 6.132527647946031529E-16 ) ) ;
#51617 = ORIENTED_EDGE ( 'NONE', *, *, #587, .T. ) ;
#51618 = ORIENTED_EDGE ( 'NONE', *, *, #51391, .T. ) ;
#51619 = EDGE_CURVE ( 'NONE', #50261, #8395, #47863, .T. ) ;
#51620 = ORIENTED_EDGE ( 'NONE', *, *, #43793, .T. ) ;
#51621 = ADVANCED_FACE ( 'NONE', ( #58690 ), #31955, .T. ) ;
#51622 = CARTESIAN_POINT ( 'NONE',  ( -66.14292637653379359, 5.598654528085800663, -7.705886871421367523 ) ) ;
#51623 = CARTESIAN_POINT ( 'NONE',  ( -1.744870598150812802, 7.000000000000005329, 0.2069669095365387901 ) ) ;
#51624 = ORIENTED_EDGE ( 'NONE', *, *, #17278, .F. ) ;
#51625 = CARTESIAN_POINT ( 'NONE',  ( -180.0570736234661808, 0.000000000000000000, 9.524999999999991473 ) ) ;
#51626 = CARTESIAN_POINT ( 'NONE',  ( -113.2449999999999903, -4.716976649647093289, -6.492361379858945902 ) ) ;
#51627 = VERTEX_POINT ( 'NONE', #2289 ) ;
#51628 = CARTESIAN_POINT ( 'NONE',  ( 74.49999999999998579, 119.9999999999997584, 10.00000000000000000 ) ) ;
#51629 = SURFACE_STYLE_USAGE ( .BOTH. , #57603 ) ;
#51630 = VERTEX_POINT ( 'NONE', #894 ) ;
#51631 = CARTESIAN_POINT ( 'NONE',  ( 2.607480562269076430, 146.7929263765338135, -8.025000000000000355 ) ) ;
#51632 = CARTESIAN_POINT ( 'NONE',  ( -53.64695261562590645, -9.497883372640860244, -3.722847864134625873 ) ) ;
#51633 = FACE_OUTER_BOUND ( 'NONE', #35587, .T. ) ;
#51634 = COLOUR_RGB ( '', 0.40784314, 0.44705882, 0.49803922) ;
#51635 = EDGE_CURVE ( 'NONE', #22849, #51540, #69591, .T. ) ;
#51636 = CARTESIAN_POINT ( 'NONE',  ( 18.25000000000000711, 31.24999999999999289, 4.000000000000000000 ) ) ;
#51637 = SURFACE_SIDE_STYLE ('',( #57250 ) ) ;
#51638 = ORIENTED_EDGE ( 'NONE', *, *, #43442, .F. ) ;
#51639 = CARTESIAN_POINT ( 'NONE',  ( 8.082903768654762899, -1.269775441351268174E-15, 1.082903768654759125 ) ) ;
#51640 = EDGE_LOOP ( 'NONE', ( #26590, #43210, #34064, #24293 ) ) ;
#51641 = FACE_OUTER_BOUND ( 'NONE', #5207, .T. ) ;
#51642 = DIRECTION ( 'NONE',  ( 0.000000000000000000, 0.000000000000000000, -1.000000000000000000 ) ) ;
#51643 = SURFACE_SIDE_STYLE ('',( #18605 ) ) ;
#51644 = CARTESIAN_POINT ( 'NONE',  ( 41.30888752411017606, 107.2690689356287663, -3.464811251346369581 ) ) ;
#51645 = CARTESIAN_POINT ( 'NONE',  ( -123.6549999999999869, -7.632228543268600340, -2.479861379858950166 ) ) ;
#51646 =( NAMED_UNIT ( * ) SI_UNIT ( $, .STERADIAN. ) SOLID_ANGLE_UNIT ( ) );
#51647 =( BOUNDED_CURVE ( )  B_SPLINE_CURVE ( 3, ( #27470, #32403, #1018, #43713 ),
 .UNSPECIFIED., .F., .F. ) 
 B_SPLINE_CURVE_WITH_KNOTS ( ( 4, 4 ),
 ( 1.570796326794896558, 2.351346768814403632 ),
 .UNSPECIFIED. ) 
 CURVE ( )  GEOMETRIC_REPRESENTATION_ITEM ( )  RATIONAL_B_SPLINE_CURVE ( ( 1.000000000000000000, 0.9498695926598446082, 0.9498695926598446082, 1.000000000000000000 ) ) 
 REPRESENTATION_ITEM ( '' )  );
#51648 = CARTESIAN_POINT ( 'NONE',  ( 2.607480562269160362, 141.9070736234661467, -8.024999999999939959 ) ) ;
#51649 = DIRECTION ( 'NONE',  ( -1.000000000000000000, -0.000000000000000000, -0.000000000000000000 ) ) ;
#51650 = CIRCLE ( 'NONE', #53897, 0.5000000000000004441 ) ;
#51651 = CARTESIAN_POINT ( 'NONE',  ( 12.25000000000002132, 7.083454193571968087E-15, 3.750000000000000000 ) ) ;
#51652 = DIRECTION ( 'NONE',  ( 0.000000000000000000, 1.000000000000000000, 0.000000000000000000 ) ) ;
#51653 = VERTEX_POINT ( 'NONE', #50224 ) ;
#51654 = EDGE_LOOP ( 'NONE', ( #60697, #25240, #21025 ) ) ;
#51655 =( NAMED_UNIT ( * ) SI_UNIT ( $, .STERADIAN. ) SOLID_ANGLE_UNIT ( ) );
#51656 = VECTOR ( 'NONE', #6322, 1000.000000000000000 ) ;
#51657 = PLANE ( 'NONE',  #53411 ) ;
#51658 = CARTESIAN_POINT ( 'NONE',  ( 22.75000000000000711, 36.75000000000000000, 3.750000000000000000 ) ) ;
#51659 = CARTESIAN_POINT ( 'NONE',  ( 8.437984349512095861, 114.3070736234661666, 1.550032578732816828E-15 ) ) ;
#51660 = VERTEX_POINT ( 'NONE', #50565 ) ;
#51661 = CARTESIAN_POINT ( 'NONE',  ( -124.5570736234661808, -1.166476076187852838E-15, -9.524999999999991473 ) ) ;
#51662 = CARTESIAN_POINT ( 'NONE',  ( -178.8549999999999898, 4.716976649647094177, 6.492361379858945902 ) ) ;
#51663 = ADVANCED_FACE ( 'NONE', ( #43938 ), #31415, .F. ) ;
#51664 =( NAMED_UNIT ( * ) SI_UNIT ( $, .STERADIAN. ) SOLID_ANGLE_UNIT ( ) );
#51665 = AXIS2_PLACEMENT_3D ( 'NONE', #45464, #23605, #55625 ) ;
#51666 = CARTESIAN_POINT ( 'NONE',  ( -54.35707362346617089, 5.598654528085804216, 7.705886871421366635 ) ) ;
#51667 = MECHANICAL_DESIGN_GEOMETRIC_PRESENTATION_REPRESENTATION (  '', ( #13430 ), #44966 ) ;
#51668 = CARTESIAN_POINT ( 'NONE',  ( -172.4950000000000330, 6.826472737025113702, -4.959722759717902107 ) ) ;
#51669 = EDGE_CURVE ( 'NONE', #35195, #61564, #38202, .T. ) ;
#51670 = PRESENTATION_LAYER_ASSIGNMENT (  '', '', ( #5595 ) ) ;
#51671 = PLANE ( 'NONE',  #57924 ) ;
#51672 = VERTEX_POINT ( 'NONE', #49192 ) ;
#51673 = CARTESIAN_POINT ( 'NONE',  ( -74.83430136428034984, 35.83209040110467214, -9.876238371507287894 ) ) ;
#51674 =( NAMED_UNIT ( * ) SI_UNIT ( $, .STERADIAN. ) SOLID_ANGLE_UNIT ( ) );
#51675 = AXIS2_PLACEMENT_3D ( 'NONE', #68657, #33682, #6582 ) ;
#51676 = DIRECTION ( 'NONE',  ( -1.000000000000000000, -0.000000000000000000, -0.000000000000000000 ) ) ;
#51677 = CARTESIAN_POINT ( 'NONE',  ( -93.50499999999999545, -6.826472737025115478, -4.959722759717899443 ) ) ;
#51678 =( NAMED_UNIT ( * ) SI_UNIT ( $, .STERADIAN. ) SOLID_ANGLE_UNIT ( ) );
#51679 = AXIS2_PLACEMENT_3D ( 'NONE', #63539, #31863, #48100 ) ;
#51680 =( NAMED_UNIT ( * ) SI_UNIT ( $, .STERADIAN. ) SOLID_ANGLE_UNIT ( ) );
#51681 = CARTESIAN_POINT ( 'NONE',  ( -89.39499999999996760, -6.826472737025113702, -4.959722759717900331 ) ) ;
#51682 = CARTESIAN_POINT ( 'NONE',  ( 8.102448949553183510, 125.1049999999999756, -5.886773742842746238 ) ) ;
#51683 = CARTESIAN_POINT ( 'NONE',  ( -65.54499999999998749, -7.632228543268600340, -2.479861379858950166 ) ) ;
#51684 = DIRECTION ( 'NONE',  ( -0.000000000000000000, -0.000000000000000000, -1.000000000000000000 ) ) ;
#51685 =( GEOMETRIC_REPRESENTATION_CONTEXT ( 3 ) GLOBAL_UNCERTAINTY_ASSIGNED_CONTEXT ( ( #48929 ) ) GLOBAL_UNIT_ASSIGNED_CONTEXT ( ( #56602, #8066, #50636 ) ) REPRESENTATION_CONTEXT ( 'NONE', 'WORKASPACE' ) );
#51686 =( LENGTH_UNIT ( ) NAMED_UNIT ( * ) SI_UNIT ( .MILLI., .METRE. ) );
#51687 = PRESENTATION_STYLE_ASSIGNMENT (( #18950 ) ) ;
#51688 = UNCERTAINTY_MEASURE_WITH_UNIT (LENGTH_MEASURE( 1.000000000000000082E-05 ), #62567, 'distance_accuracy_value', 'NONE');
#51689 = AXIS2_PLACEMENT_3D ( 'NONE', #58100, #47594, #69669 ) ;
#51690 = CARTESIAN_POINT ( 'NONE',  ( 0.000000000000000000, 0.000000000000000000, 0.000000000000000000 ) ) ;
#51691 = SURFACE_STYLE_USAGE ( .BOTH. , #30198 ) ;
#51692 = ORIENTED_EDGE ( 'NONE', *, *, #27283, .F. ) ;
#51693 = CARTESIAN_POINT ( 'NONE',  ( -110.0929263765337822, 3.094860106618433360, 9.524999999999991473 ) ) ;
#51694 = CARTESIAN_POINT ( 'NONE',  ( -131.0949999999999989, -2.607480562269071545, -8.024999999999991473 ) ) ;
#51695 = AXIS2_PLACEMENT_3D ( 'NONE', #21831, #41667, #32713 ) ;
#51696 = SURFACE_STYLE_FILL_AREA ( #19674 ) ;
#51697 = EDGE_CURVE ( 'NONE', #43730, #18512, #65113, .T. ) ;
#51699 = SURFACE_STYLE_USAGE ( .BOTH. , #52415 ) ;
#51698 = DIRECTION ( 'NONE',  ( 1.000000000000000000, -4.336808689941999001E-16, 0.000000000000000000 ) ) ;
#51700 = FILL_AREA_STYLE_COLOUR ( '', #13676 ) ;
#51701 = EDGE_LOOP ( 'NONE', ( #5275, #4339, #31628, #18989 ) ) ;
#51702 = VERTEX_POINT ( 'NONE', #66378 ) ;
#51703 = DIRECTION ( 'NONE',  ( 0.000000000000000000, -1.000000000000000000, 0.000000000000000000 ) ) ;
#51704 = CIRCLE ( 'NONE', #57313, 1.000000000000000888 ) ;
#51705 = ADVANCED_FACE ( 'NONE', ( #17860 ), #17929, .T. ) ;
#51706 = CARTESIAN_POINT ( 'NONE',  ( -4.716976649647097730, 147.2429263765338305, -6.492361379858953896 ) ) ;
#51707 = DIRECTION ( 'NONE',  ( -0.000000000000000000, -0.000000000000000000, -1.000000000000000000 ) ) ;
#51708 = FILL_AREA_STYLE_COLOUR ( '', #26243 ) ;
#51709 = PLANE ( 'NONE',  #64450 ) ;
#51710 = ORIENTED_EDGE ( 'NONE', *, *, #48601, .F. ) ;
#51711 = CARTESIAN_POINT ( 'NONE',  ( -131.1550000000000011, 7.632228543268600340, 2.479861379858949277 ) ) ;
#51712 = VERTEX_POINT ( 'NONE', #39685 ) ;
#51713 = CARTESIAN_POINT ( 'NONE',  ( -118.7070736234661581, -3.094860106618431139, -9.524999999999991473 ) ) ;
#51714 = EDGE_CURVE ( 'NONE', #57439, #40317, #34789, .T. ) ;
#51715 = ORIENTED_EDGE ( 'NONE', *, *, #5321, .T. ) ;
#51716 = CARTESIAN_POINT ( 'NONE',  ( 44.43085292287471333, 10.23783787917596122, -3.500000000000000000 ) ) ;
#51717 = CARTESIAN_POINT ( 'NONE',  ( 57.24999999999999289, 27.74999999999998934, -4.000000000000000000 ) ) ;
#51718 = VERTEX_POINT ( 'NONE', #8356 ) ;
#51719 = VECTOR ( 'NONE', #68063, 1000.000000000000000 ) ;
#51720 = VECTOR ( 'NONE', #60493, 1000.000000000000000 ) ;
#51721 = CARTESIAN_POINT ( 'NONE',  ( -195.0000000000000000, 0.000000000000000000, 9.524999999999991473 ) ) ;
#51722 = AXIS2_PLACEMENT_3D ( 'NONE', #26666, #41876, #21769 ) ;
#51723 = CARTESIAN_POINT ( 'NONE',  ( -8.102448949553181734, 142.8949999999999818, -5.886773742842749790 ) ) ;
#51724 = EDGE_LOOP ( 'NONE', ( #62944, #9955, #32158 ) ) ;
#51725 = CARTESIAN_POINT ( 'NONE',  ( 4.750000000000002665, 24.74999999999998579, 3.750000000000000000 ) ) ;
#51726 = CARTESIAN_POINT ( 'NONE',  ( 9.058813317711337021, 148.6549999999999727, 2.943386871421375783 ) ) ;
#51727 = CIRCLE ( 'NONE', #16789, 23.00000000000000000 ) ;
#51728 = CARTESIAN_POINT ( 'NONE',  ( 4.041451884327377897, 1.417096231345241319, 7.000000000000000888 ) ) ;
#51729 = VERTEX_POINT ( 'NONE', #14307 ) ;
#51730 = CARTESIAN_POINT ( 'NONE',  ( -6.826472737025120807, 120.3929263765338220, -4.959722759717907437 ) ) ;
#51731 = DIRECTION ( 'NONE',  ( 1.000000000000000000, 0.000000000000000000, 0.000000000000000000 ) ) ;
#51732 = UNCERTAINTY_MEASURE_WITH_UNIT (LENGTH_MEASURE( 1.000000000000000082E-05 ), #49375, 'distance_accuracy_value', 'NONE');
#51733 = FILL_AREA_STYLE ('',( #25330 ) ) ;
#51734 = VECTOR ( 'NONE', #68833, 1000.000000000000000 ) ;
#51735 =( NAMED_UNIT ( * ) SI_UNIT ( $, .STERADIAN. ) SOLID_ANGLE_UNIT ( ) );
#51736 = EDGE_CURVE ( 'NONE', #38068, #34648, #13441, .T. ) ;
#51737 = SURFACE_SIDE_STYLE ('',( #2069 ) ) ;
#51738 =( NAMED_UNIT ( * ) SI_UNIT ( $, .STERADIAN. ) SOLID_ANGLE_UNIT ( ) );
#51739 = ORIENTED_EDGE ( 'NONE', *, *, #15514, .T. ) ;
#51740 = MECHANICAL_DESIGN_GEOMETRIC_PRESENTATION_REPRESENTATION (  '', ( #49474 ), #45040 ) ;
#51741 = LINE ( 'NONE', #24292, #4856 ) ;
#51742 = ORIENTED_EDGE ( 'NONE', *, *, #14068, .F. ) ;
#51743 = CARTESIAN_POINT ( 'NONE',  ( -58.04292637653379927, -9.058813317711329915, -2.943386871421370898 ) ) ;
#51744 = PRESENTATION_LAYER_ASSIGNMENT (  '', '', ( #30356 ) ) ;
#51745 = CARTESIAN_POINT ( 'NONE',  ( -72.49999999999998579, 119.9999999999997868, 10.00000000000000000 ) ) ;
#51746 = CARTESIAN_POINT ( 'NONE',  ( -45.50000000000000000, 9.708372675170618749, -6.500000000000000000 ) ) ;
#51747 = CARTESIAN_POINT ( 'NONE',  ( -149.6050000000000182, 6.826472737025113702, -4.959722759717902107 ) ) ;
#51748 = ORIENTED_EDGE ( 'NONE', *, *, #10650, .F. ) ;
#51749 = SPHERICAL_SURFACE ( 'NONE', #3637, 0.5000000000000000000 ) ;
#51750 = UNCERTAINTY_MEASURE_WITH_UNIT (LENGTH_MEASURE( 1.000000000000000082E-05 ), #28277, 'distance_accuracy_value', 'NONE');
#51751 = PRESENTATION_LAYER_ASSIGNMENT (  '', '', ( #40515 ) ) ;
#51752 = AXIS2_PLACEMENT_3D ( 'NONE', #51956, #52648, #42138 ) ;
#51753 = FACE_OUTER_BOUND ( 'NONE', #26251, .T. ) ;
#51754 = CARTESIAN_POINT ( 'NONE',  ( -53.81525949776377615, -8.999709270181568854, 5.797011693762002871 ) ) ;
#51755 = CARTESIAN_POINT ( 'NONE',  ( 75.00000000000000000, 19.99999999999997868, 6.000000000000000000 ) ) ;
#51756 = CARTESIAN_POINT ( 'NONE',  ( -10.74999999999999645, -0.9999999999999995559, 6.000000000000001776 ) ) ;
#51757 = VERTEX_POINT ( 'NONE', #62488 ) ;
#51758 = AXIS2_PLACEMENT_3D ( 'NONE', #62127, #35421, #46351 ) ;
#51759 = CARTESIAN_POINT ( 'NONE',  ( 2.999999999999993339, 5.000000000000000000, 24.00402776293822882 ) ) ;
#51760 = ORIENTED_EDGE ( 'NONE', *, *, #21126, .T. ) ;
#51761 = DIRECTION ( 'NONE',  ( 0.000000000000000000, 0.000000000000000000, 1.000000000000000000 ) ) ;
#51762 = CARTESIAN_POINT ( 'NONE',  ( -79.40500000000000114, -2.607480562269069768, 8.024999999999991473 ) ) ;
#51763 = ORIENTED_EDGE ( 'NONE', *, *, #59289, .F. ) ;
#51764 = CARTESIAN_POINT ( 'NONE',  ( 25.75000000000001066, 21.74999999999998224, -3.750000000000000000 ) ) ;
#51765 = ORIENTED_EDGE ( 'NONE', *, *, #11741, .F. ) ;
#51766 =( BOUNDED_SURFACE ( )  B_SPLINE_SURFACE ( 3, 2, ( 
 ( #58058, #68257, #36278 ),
 ( #47543, #57699, #4190 ),
 ( #25667, #20765, #42272 ),
 ( #17812, #44242, #66330 ),
 ( #28685, #43889, #39292 ),
 ( #33974, #12158, #11827 ) ),
 .UNSPECIFIED., .F., .F., .F. ) 
 B_SPLINE_SURFACE_WITH_KNOTS ( ( 4, 2, 4 ),
 ( 3, 3 ),
 ( 0.000000000000000000, 0.7853981633974482790, 1.570796326794896558 ),
 ( 0.000000000000000000, 1.000000000000000000 ),
 .UNSPECIFIED. ) 
 GEOMETRIC_REPRESENTATION_ITEM ( )  RATIONAL_B_SPLINE_SURFACE ( (
 ( 1.000000000000000000, 0.5847102846637692863, 1.000000000000000000),
 ( 1.000000000000000000, 0.5843845446924222919, 1.000000000000000000),
 ( 1.000000000000000000, 0.5995650817083321149, 1.000000000000000000),
 ( 1.000000000000000000, 0.6465434225961957937, 1.000000000000000000),
 ( 1.000000000000000000, 0.6778979487210353705, 1.000000000000000000),
 ( 1.000000000000000000, 0.7071067811865530128, 1.000000000000000000) ) ) 
 REPRESENTATION_ITEM ( '' )  SURFACE ( )  );
#51767 = STYLED_ITEM ( 'NONE', ( #48639 ), #45241 ) ;
#51768 = VECTOR ( 'NONE', #8512, 1000.000000000000000 ) ;
#51769 = CARTESIAN_POINT ( 'NONE',  ( -18.25000000000000711, 31.24999999999999289, 4.000000000000000000 ) ) ;
#51770 = CARTESIAN_POINT ( 'NONE',  ( -8.102448949553181734, 136.8949999999999534, -5.886773742842749790 ) ) ;
#51771 = CARTESIAN_POINT ( 'NONE',  ( -94.94499999999999318, -9.827790563157499189E-16, -8.024999999999991473 ) ) ;
#51772 = MECHANICAL_DESIGN_GEOMETRIC_PRESENTATION_REPRESENTATION (  '', ( #6801 ), #2270 ) ;
#51773 = FACE_OUTER_BOUND ( 'NONE', #54740, .T. ) ;
#51774 = PRESENTATION_LAYER_ASSIGNMENT (  '', '', ( #45075 ) ) ;
#51775 = UNCERTAINTY_MEASURE_WITH_UNIT (LENGTH_MEASURE( 1.000000000000000082E-05 ), #65605, 'distance_accuracy_value', 'NONE');
#51776 =( GEOMETRIC_REPRESENTATION_CONTEXT ( 3 ) GLOBAL_UNCERTAINTY_ASSIGNED_CONTEXT ( ( #24328 ) ) GLOBAL_UNIT_ASSIGNED_CONTEXT ( ( #16512, #16848, #33005 ) ) REPRESENTATION_CONTEXT ( 'NONE', 'WORKASPACE' ) );
#51777 = CARTESIAN_POINT ( 'NONE',  ( -41.00754902350323050, 107.7352920524769786, -3.098114188008660896 ) ) ;
#51778 = EDGE_LOOP ( 'NONE', ( #40467, #36975, #51212, #65832 ) ) ;
#51779 = CARTESIAN_POINT ( 'NONE',  ( -140.3929263765338078, 8.102448949553176405, 5.886773742842740909 ) ) ;
#51780 = SURFACE_SIDE_STYLE ('',( #40902 ) ) ;
#51781 = CARTESIAN_POINT ( 'NONE',  ( -157.4950000000000045, 6.826472737025113702, -4.959722759717902107 ) ) ;
#51782 = CIRCLE ( 'NONE', #4556, 1.000000000000000888 ) ;
#51783 = SURFACE_STYLE_FILL_AREA ( #41253 ) ;
#51784 =( GEOMETRIC_REPRESENTATION_CONTEXT ( 3 ) GLOBAL_UNCERTAINTY_ASSIGNED_CONTEXT ( ( #36338 ) ) GLOBAL_UNIT_ASSIGNED_CONTEXT ( ( #39730, #29482, #23861 ) ) REPRESENTATION_CONTEXT ( 'NONE', 'WORKASPACE' ) );
#51785 = EDGE_CURVE ( 'NONE', #66402, #5542, #22622, .T. ) ;
#51786 = DIRECTION ( 'NONE',  ( 0.000000000000000000, 0.000000000000000000, 1.000000000000000000 ) ) ;
#51787 = CYLINDRICAL_SURFACE ( 'NONE', #1206, 8.025000000000000355 ) ;
#51788 = EDGE_LOOP ( 'NONE', ( #51403, #34044, #40133, #11396 ) ) ;
#51789 = CYLINDRICAL_SURFACE ( 'NONE', #47339, 0.5000000000000004441 ) ;
#51790 = ORIENTED_EDGE ( 'NONE', *, *, #68383, .T. ) ;
#51791 = AXIS2_PLACEMENT_3D ( 'NONE', #13522, #19139, #50828 ) ;
#51792 = DIRECTION ( 'NONE',  ( -1.000000000000000000, 0.000000000000000000, 0.000000000000000000 ) ) ;
#51793 = CARTESIAN_POINT ( 'NONE',  ( 22.75000000000000711, 36.75000000000000000, -3.750000000000000000 ) ) ;
#51794 = SURFACE_STYLE_FILL_AREA ( #35615 ) ;
#51795 = DIRECTION ( 'NONE',  ( 1.000000000000000000, 2.312964634635740689E-15, -0.000000000000000000 ) ) ;
#51796 = CARTESIAN_POINT ( 'NONE',  ( 44.91886116991580735, 9.999999999999980460, 3.201362207699192997 ) ) ;
#51797 = EDGE_CURVE ( 'NONE', #41190, #47531, #4074, .T. ) ;
#51798 = CARTESIAN_POINT ( 'NONE',  ( -7.632228543268607446, 142.6570736234661751, -2.479861379858953718 ) ) ;
#51799 = VERTEX_POINT ( 'NONE', #40365 ) ;
#51800 = CARTESIAN_POINT ( 'NONE',  ( -163.8549999999999898, 4.716976649647094177, 6.492361379858945902 ) ) ;
#51801 = EDGE_CURVE ( 'NONE', #53365, #31566, #57569, .T. ) ;
#51802 = ORIENTED_EDGE ( 'NONE', *, *, #67045, .F. ) ;
#51803 = LINE ( 'NONE', #8877, #510 ) ;
#51805 = ORIENTED_EDGE ( 'NONE', *, *, #8838, .T. ) ;
#51804 = EDGE_CURVE ( 'NONE', #57528, #19277, #2669, .T. ) ;
#51806 =( GEOMETRIC_REPRESENTATION_CONTEXT ( 3 ) GLOBAL_UNCERTAINTY_ASSIGNED_CONTEXT ( ( #41162 ) ) GLOBAL_UNIT_ASSIGNED_CONTEXT ( ( #18197, #66741, #34706 ) ) REPRESENTATION_CONTEXT ( 'NONE', 'WORKASPACE' ) );
#51807 = CYLINDRICAL_SURFACE ( 'NONE', #59564, 9.524999999999991473 ) ;
#51808 = ADVANCED_FACE ( 'NONE', ( #24847 ), #29436, .T. ) ;
#51809 = CARTESIAN_POINT ( 'NONE',  ( -5.598654528085808657, 110.6449999999999960, 7.705886871421373741 ) ) ;
#51810 = ORIENTED_EDGE ( 'NONE', *, *, #30853, .F. ) ;
#51812 = ADVANCED_FACE ( 'NONE', ( #20271 ), #56880, .F. ) ;
#51811 = CARTESIAN_POINT ( 'NONE',  ( 8.102448949553181734, 113.1049999999999898, -5.886773742842746238 ) ) ;
#51813 = CIRCLE ( 'NONE', #5684, 0.5000000000000004441 ) ;
#51814 = CARTESIAN_POINT ( 'NONE',  ( -70.25499999999998124, -4.716976649647092401, 6.492361379858946790 ) ) ;
#51815 = LINE ( 'NONE', #24696, #63270 ) ;
#51816 = PRODUCT ( '13. Bolt M6x45', '13. Bolt M6x45', '', ( #6498 ) ) ;
#51817 = VERTEX_POINT ( 'NONE', #67783 ) ;
#51818 = CARTESIAN_POINT ( 'NONE',  ( -8.102448949553181734, 135.0050000000000239, -5.886773742842749790 ) ) ;
#51819 = UNCERTAINTY_MEASURE_WITH_UNIT (LENGTH_MEASURE( 1.000000000000000082E-05 ), #52654, 'distance_accuracy_value', 'NONE');
#51820 = SURFACE_SIDE_STYLE ('',( #24700 ) ) ;
#51821 = CIRCLE ( 'NONE', #43955, 3.499999999999999556 ) ;
#51822 = CARTESIAN_POINT ( 'NONE',  ( 27.99999999999999289, 34.36176364315826248, -80.00402776293826435 ) ) ;
#51823 = PRESENTATION_LAYER_ASSIGNMENT (  '', '', ( #13582 ) ) ;
#51824 = SURFACE_SIDE_STYLE ('',( #30322 ) ) ;
#51825 = VERTEX_POINT ( 'NONE', #19583 ) ;
#51826 = CARTESIAN_POINT ( 'NONE',  ( -7.499999999999999112, 0.000000000000000000, 0.000000000000000000 ) ) ;
#51827 = CARTESIAN_POINT ( 'NONE',  ( -181.1049999999999898, -6.826472737025115478, 4.959722759717900331 ) ) ;
#51828 = VERTEX_POINT ( 'NONE', #54013 ) ;
#51829 = B_SPLINE_CURVE_WITH_KNOTS ( 'NONE', 3,
 ( #27461, #27794, #49296, #59838, #39116, #48986, #60185, #16613, #37752 ),
 .UNSPECIFIED., .F., .F.,
 ( 4, 2, 1, 2, 4 ),
 ( 0.01084732271231145413, 0.01152005980350376095, 0.01219279689469606777, 0.01353827107708068141, 0.01622921944184991042 ),
 .UNSPECIFIED. ) ;
#51830 = CARTESIAN_POINT ( 'NONE',  ( 8.527945164174102644, 111.3821367850715376, 1.507062088730521499 ) ) ;
#51831 = PRESENTATION_LAYER_ASSIGNMENT (  '', '', ( #36117 ) ) ;
#51832 = DIRECTION ( 'NONE',  ( 1.000000000000000000, 0.000000000000000000, 0.000000000000000000 ) ) ;
#51833 = CARTESIAN_POINT ( 'NONE',  ( -87.14292637653379359, 5.598654528085800663, -7.705886871421367523 ) ) ;
#51834 = ORIENTED_EDGE ( 'NONE', *, *, #36050, .F. ) ;
#51835 = DIRECTION ( 'NONE',  ( -0.000000000000000000, 1.000000000000000000, -0.000000000000000000 ) ) ;
#51836 = CARTESIAN_POINT ( 'NONE',  ( 17.00000000000000711, 24.74999999999997868, -3.750000000000000000 ) ) ;
#51837 = AXIS2_PLACEMENT_3D ( 'NONE', #34039, #325, #1953 ) ;
#51838 = ORIENTED_EDGE ( 'NONE', *, *, #4351, .F. ) ;
#51839 = DIRECTION ( 'NONE',  ( 0.000000000000000000, 0.3420201433256630508, -0.9396926207859105373 ) ) ;
#51840 = CARTESIAN_POINT ( 'NONE',  ( -102.3549999999999898, -4.716976649647093289, -6.492361379858945902 ) ) ;
#51841 = VERTEX_POINT ( 'NONE', #26244 ) ;
#51842 = CARTESIAN_POINT ( 'NONE',  ( 44.28021770739999852, 9.999999999999980460, -3.500000000000000000 ) ) ;
#51843 = AXIS2_PLACEMENT_3D ( 'NONE', #22754, #28336, #12168 ) ;
#51844 = DIRECTION ( 'NONE',  ( 0.000000000000000000, 0.000000000000000000, 1.000000000000000000 ) ) ;
#51845 = CARTESIAN_POINT ( 'NONE',  ( -137.4570736234661865, -9.058813317711329915, 2.943386871421371787 ) ) ;
#51846 = AXIS2_PLACEMENT_3D ( 'NONE', #62051, #34633, #67346 ) ;
#51847 = CARTESIAN_POINT ( 'NONE',  ( -9.058813317711337021, 152.0449999999999875, -2.943386871421374895 ) ) ;
#51848 = CARTESIAN_POINT ( 'NONE',  ( -79.85707362346616378, -5.598654528085803328, -7.705886871421366635 ) ) ;
#51849 = CARTESIAN_POINT ( 'NONE',  ( -93.29292637653493614, 3.094860106599470750, -9.525000000013767121 ) ) ;
#51850 = VERTEX_POINT ( 'NONE', #26574 ) ;
#51851 = FACE_OUTER_BOUND ( 'NONE', #26428, .T. ) ;
#51852 = COLOUR_RGB ( '', 0.66274510, 0.83137255, 0.94901961) ;
#51853 =( NAMED_UNIT ( * ) PLANE_ANGLE_UNIT ( ) SI_UNIT ( $, .RADIAN. ) );
#51854 = STYLED_ITEM ( 'NONE', ( #65038 ), #28085 ) ;
#51855 = FACE_OUTER_BOUND ( 'NONE', #51035, .T. ) ;
#51856 = CARTESIAN_POINT ( 'NONE',  ( -116.6049999999999756, 6.826472737025113702, -4.959722759717902107 ) ) ;
#51857 =( NAMED_UNIT ( * ) SI_UNIT ( $, .STERADIAN. ) SOLID_ANGLE_UNIT ( ) );
#51858 = FACE_OUTER_BOUND ( 'NONE', #53280, .T. ) ;
#51859 = CARTESIAN_POINT ( 'NONE',  ( -128.9950000000000045, -6.826472737025115478, 4.959722759717900331 ) ) ;
#51860 =( GEOMETRIC_REPRESENTATION_CONTEXT ( 3 ) GLOBAL_UNCERTAINTY_ASSIGNED_CONTEXT ( ( #55118 ) ) GLOBAL_UNIT_ASSIGNED_CONTEXT ( ( #28558, #61280, #34212 ) ) REPRESENTATION_CONTEXT ( 'NONE', 'WORKASPACE' ) );
#51861 = DIRECTION ( 'NONE',  ( -1.000000000000000000, 0.000000000000000000, 0.000000000000000000 ) ) ;
#51862 = ORIENTED_EDGE ( 'NONE', *, *, #55440, .T. ) ;
#51863 = FILL_AREA_STYLE_COLOUR ( '', #29071 ) ;
#51864 = COLOUR_RGB ( '', 0.08235294, 0.09019608, 0.10196078) ;
#51866 = MECHANICAL_DESIGN_GEOMETRIC_PRESENTATION_REPRESENTATION (  '', ( #7999 ), #61928 ) ;
#51865 = DIRECTION ( 'NONE',  ( 0.000000000000000000, 0.000000000000000000, 1.000000000000000000 ) ) ;
#51867 = CARTESIAN_POINT ( 'NONE',  ( -172.1929263765337907, -10.01517768586948698, 6.132527647946031529E-16 ) ) ;
#51868 = CARTESIAN_POINT ( 'NONE',  ( 9.568252947146932641, -1.427299755870875986, 0.6386920474458026575 ) ) ;
#51869 = PRESENTATION_STYLE_ASSIGNMENT (( #25805 ) ) ;
#51870 =( GEOMETRIC_REPRESENTATION_CONTEXT ( 3 ) GLOBAL_UNCERTAINTY_ASSIGNED_CONTEXT ( ( #22290 ) ) GLOBAL_UNIT_ASSIGNED_CONTEXT ( ( #43950, #48537, #27355 ) ) REPRESENTATION_CONTEXT ( 'NONE', 'WORKASPACE' ) );
#51871 = ADVANCED_FACE ( 'NONE', ( #64590 ), #5602, .T. ) ;
#51872 = CARTESIAN_POINT ( 'NONE',  ( 71.49999999999998579, 64.07124727947029896, -10.00000000000000000 ) ) ;
#51873 = DIRECTION ( 'NONE',  ( 0.000000000000000000, 0.000000000000000000, 1.000000000000000000 ) ) ;
#51874 = ORIENTED_EDGE ( 'NONE', *, *, #40014, .T. ) ;
#51875 = CARTESIAN_POINT ( 'NONE',  ( -82.64292637653379359, -5.598654528085801552, 7.705886871421367523 ) ) ;
#51876 = EDGE_CURVE ( 'NONE', #43779, #1034, #5128, .T. ) ;
#51877 = MECHANICAL_DESIGN_GEOMETRIC_PRESENTATION_REPRESENTATION (  '', ( #55212 ), #37406 ) ;
#51878 = CARTESIAN_POINT ( 'NONE',  ( -180.1429263765338078, 5.598654528085800663, -7.705886871421367523 ) ) ;
#51879 = CARTESIAN_POINT ( 'NONE',  ( 45.65811388300841855, 10.21937129433612235, -6.000000000000000000 ) ) ;
#51880 = DIRECTION ( 'NONE',  ( 1.000000000000000000, 7.709882115452468306E-16, -0.000000000000000000 ) ) ;
#51881 = CIRCLE ( 'NONE', #21542, 0.5000000000000004441 ) ;
#51882 = CARTESIAN_POINT ( 'NONE',  ( -156.3570736234661922, 5.598654528085804216, 7.705886871421366635 ) ) ;
#51883 = ORIENTED_EDGE ( 'NONE', *, *, #15739, .F. ) ;
#51884 = VECTOR ( 'NONE', #35223, 1000.000000000000000 ) ;
#51885 = DIRECTION ( 'NONE',  ( 0.000000000000000000, -1.000000000000000000, 0.000000000000000000 ) ) ;
#51886 = LINE ( 'NONE', #41696, #47795 ) ;
#51887 = EDGE_CURVE ( 'NONE', #53696, #51899, #58960, .T. ) ;
#51888 = ORIENTED_EDGE ( 'NONE', *, *, #24038, .F. ) ;
#51889 = DIRECTION ( 'NONE',  ( -1.000000000000000000, -0.000000000000000000, -0.000000000000000000 ) ) ;
#51890 = DIRECTION ( 'NONE',  ( 0.000000000000000000, 0.000000000000000000, 1.000000000000000000 ) ) ;
#51891 = CARTESIAN_POINT ( 'NONE',  ( -4.716976649647097730, 130.3570736234661638, -6.492361379858953896 ) ) ;
#51892 = SURFACE_SIDE_STYLE ('',( #8972 ) ) ;
#51893 = MECHANICAL_DESIGN_GEOMETRIC_PRESENTATION_REPRESENTATION (  '', ( #58603 ), #21554 ) ;
#51894 = ORIENTED_EDGE ( 'NONE', *, *, #60913, .F. ) ;
#51896 = EDGE_CURVE ( 'NONE', #8139, #44039, #47248, .T. ) ;
#51895 = LINE ( 'NONE', #56454, #37245 ) ;
#51897 = CARTESIAN_POINT ( 'NONE',  ( -102.2049999999999983, -2.607480562269071545, -8.024999999999991473 ) ) ;
#51898 = COLOUR_RGB ( '', 0.09019608, 0.27058824, 0.51372549) ;
#51899 = VERTEX_POINT ( 'NONE', #10773 ) ;
#51900 =( LENGTH_UNIT ( ) NAMED_UNIT ( * ) SI_UNIT ( .MILLI., .METRE. ) );
#51901 = DIRECTION ( 'NONE',  ( 0.000000000000000000, 1.350863103983176297E-16, 1.000000000000000000 ) ) ;
#51902 = CARTESIAN_POINT ( 'NONE',  ( -58.06841298682653019, -7.714685904994091459, -0.5239124249552955526 ) ) ;
#51903 = EDGE_LOOP ( 'NONE', ( #51186, #60860, #7142, #45771 ) ) ;
#51904 = AXIS2_PLACEMENT_3D ( 'NONE', #59449, #64409, #6346 ) ;
#51905 = CARTESIAN_POINT ( 'NONE',  ( -84.14499999999998181, -4.716976649647092401, 6.492361379858946790 ) ) ;
#51906 = ORIENTED_EDGE ( 'NONE', *, *, #42869, .T. ) ;
#51907 = FACE_OUTER_BOUND ( 'NONE', #47239, .T. ) ;
#51908 = B_SPLINE_CURVE_WITH_KNOTS ( 'NONE', 3,
 ( #27285, #53694, #42857, #26933, #64936, #37226, #48467, #48824, #15415, #10799, #16461, #16792, #843, #26604, #22384, #38264, #32952, #32246, #36872, #58289, #10117, #48125, #53026, #58638, #31544, #7257, #1900 ),
 .UNSPECIFIED., .F., .F.,
 ( 4, 2, 2, 2, 2, 2, 2, 1, 2, 2, 2, 2, 2, 4 ),
 ( 5.946939743265090950E-16, 0.002417576611438273116, 0.003626364917157114988, 0.004835153222875957293, 0.006043941528594800466, 0.007252729834313642772, 0.008461518140032485077, 0.009670306445751328250, 0.01087909475147017142, 0.01208788305718901633, 0.01329667136290785777, 0.01450545966862670268, 0.01692303628006438729, 0.01934061289150207363 ),
 .UNSPECIFIED. ) ;
#51909 = VECTOR ( 'NONE', #59144, 1000.000000000000000 ) ;
#51910 = VECTOR ( 'NONE', #44547, 1000.000000000000000 ) ;
#51911 = DIRECTION ( 'NONE',  ( 0.000000000000000000, 0.000000000000000000, -1.000000000000000000 ) ) ;
#51912 = VERTEX_POINT ( 'NONE', #69503 ) ;
#51913 = DIRECTION ( 'NONE',  ( -1.000000000000000000, 0.000000000000000000, 0.000000000000000000 ) ) ;
#51914 = STYLED_ITEM ( 'NONE', ( #16103 ), #23274 ) ;
#51915 = LINE ( 'NONE', #3673, #23510 ) ;
#51916 = FACE_OUTER_BOUND ( 'NONE', #50600, .T. ) ;
#51917 = EDGE_LOOP ( 'NONE', ( #36912, #53522, #61300 ) ) ;
#51918 = MECHANICAL_DESIGN_GEOMETRIC_PRESENTATION_REPRESENTATION (  '', ( #64245 ), #65421 ) ;
#51919 = VERTEX_POINT ( 'NONE', #64220 ) ;
#51920 = DIRECTION ( 'NONE',  ( -0.000000000000000000, 0.000000000000000000, -1.000000000000000000 ) ) ;
#51921 = CARTESIAN_POINT ( 'NONE',  ( -41.61282686761437333, 107.5028968421555930, 3.982829320873340073 ) ) ;
#51922 = CARTESIAN_POINT ( 'NONE',  ( -168.9570736234661865, 9.058813317711329915, -2.943386871421373119 ) ) ;
#51923 = DIRECTION ( 'NONE',  ( -1.000000000000000000, 0.000000000000000000, 0.000000000000000000 ) ) ;
#51924 = CARTESIAN_POINT ( 'NONE',  ( 3.094860106618435136, 112.2949999999999733, -9.525000000000000355 ) ) ;
#51925 = CARTESIAN_POINT ( 'NONE',  ( -104.4570736234661723, -9.058813317711329915, 2.943386871421371787 ) ) ;
#51926 = EDGE_CURVE ( 'NONE', #69362, #11926, #59535, .T. ) ;
#51927 = MECHANICAL_DESIGN_GEOMETRIC_PRESENTATION_REPRESENTATION (  '', ( #31718 ), #54163 ) ;
#51928 = DIRECTION ( 'NONE',  ( 0.000000000000000000, -1.000000000000000000, 0.000000000000000000 ) ) ;
#51929 = LINE ( 'NONE', #3683, #38136 ) ;
#51930 = ORIENTED_EDGE ( 'NONE', *, *, #32538, .T. ) ;
#51931 = CARTESIAN_POINT ( 'NONE',  ( -23.21231517720797655, 112.9999999999999858, 9.500000000000000000 ) ) ;
#51932 = CARTESIAN_POINT ( 'NONE',  ( 1.000000000000000000, 36.99999999999999289, -3.750000000000000000 ) ) ;
#51934 = CARTESIAN_POINT ( 'NONE',  ( -115.2570736234661695, 5.598654528085800663, -7.705886871421367523 ) ) ;
#51933 = DIRECTION ( 'NONE',  ( 0.000000000000000000, 0.000000000000000000, -1.000000000000000000 ) ) ;
#51935 =( GEOMETRIC_REPRESENTATION_CONTEXT ( 3 ) GLOBAL_UNCERTAINTY_ASSIGNED_CONTEXT ( ( #2518 ) ) GLOBAL_UNIT_ASSIGNED_CONTEXT ( ( #25440, #41656, #57456 ) ) REPRESENTATION_CONTEXT ( 'NONE', 'WORKASPACE' ) );
#51936 = CARTESIAN_POINT ( 'NONE',  ( -151.8549999999999898, 4.716976649647094177, 6.492361379858945902 ) ) ;
#51937 =( NAMED_UNIT ( * ) SI_UNIT ( $, .STERADIAN. ) SOLID_ANGLE_UNIT ( ) );
#51938 = CARTESIAN_POINT ( 'NONE',  ( -0.4067914857153943076, 110.6009882518928720, -9.424011748107126607 ) ) ;
#51939 = MECHANICAL_DESIGN_GEOMETRIC_PRESENTATION_REPRESENTATION (  '', ( #49687 ), #18226 ) ;
#51940 = CARTESIAN_POINT ( 'NONE',  ( -154.4949999999999477, 6.826472737025113702, -4.959722759717902107 ) ) ;
#51941 = CARTESIAN_POINT ( 'NONE',  ( -151.4950000000000045, 6.826472737025113702, -4.959722759717902107 ) ) ;
#51942 = ORIENTED_EDGE ( 'NONE', *, *, #8958, .F. ) ;
#51943 = DIRECTION ( 'NONE',  ( 0.000000000000000000, 0.000000000000000000, 1.000000000000000000 ) ) ;
#51944 = CONICAL_SURFACE ( 'NONE', #58649, 6.999999999999997335, 0.7853981633974500554 ) ;
#51945 = DIRECTION ( 'NONE',  ( -0.000000000000000000, -0.000000000000000000, 1.000000000000000000 ) ) ;
#51946 = CARTESIAN_POINT ( 'NONE',  ( -67.85499999999998977, 4.716976649647094177, 6.492361379858945902 ) ) ;
#51947 = FILL_AREA_STYLE_COLOUR ( '', #28101 ) ;
#51948 = VECTOR ( 'NONE', #60609, 1000.000000000000000 ) ;
#51949 = EDGE_CURVE ( 'NONE', #40929, #33557, #16435, .T. ) ;
#51950 = CARTESIAN_POINT ( 'NONE',  ( -61.19499999999997897, 8.437984349512086979, -1.550032578732815448E-15 ) ) ;
#51951 = EDGE_CURVE ( 'NONE', #29039, #51526, #57288, .T. ) ;
#51952 = CARTESIAN_POINT ( 'NONE',  ( 5.598654528085809545, 152.2549999999999670, -7.705886871421373741 ) ) ;
#51953 = DIRECTION ( 'NONE',  ( -0.000000000000000000, 1.000000000000000000, -0.000000000000000000 ) ) ;
#51954 = MECHANICAL_DESIGN_GEOMETRIC_PRESENTATION_REPRESENTATION (  '', ( #59771 ), #39620 ) ;
#51955 = FACE_BOUND ( 'NONE', #1468, .T. ) ;
#51956 = CARTESIAN_POINT ( 'NONE',  ( 16.00000000000008527, 130.6078173946806942, -43.75000000000001421 ) ) ;
#51957 = DIRECTION ( 'NONE',  ( 0.000000000000000000, -0.000000000000000000, 1.000000000000000000 ) ) ;
#51958 = EDGE_CURVE ( 'NONE', #40174, #41931, #59270, .T. ) ;
#51959 = DIRECTION ( 'NONE',  ( 0.000000000000000000, 0.000000000000000000, 1.000000000000000000 ) ) ;
#51960 = CARTESIAN_POINT ( 'NONE',  ( -178.9429263765338192, 0.000000000000000000, 9.524999999999991473 ) ) ;
#51961 = AXIS2_PLACEMENT_3D ( 'NONE', #35378, #2950, #67036 ) ;
#51962 = CARTESIAN_POINT ( 'NONE',  ( -71.49999999999998579, 64.07124727947029896, 7.500000000000000000 ) ) ;
#51963 = STYLED_ITEM ( 'NONE', ( #51367 ), #22745 ) ;
#51964 = CARTESIAN_POINT ( 'NONE',  ( 26.25000000000001066, 19.24999999999997868, -3.750000000000000000 ) ) ;
#51965 = EDGE_CURVE ( 'NONE', #15803, #45247, #15388, .T. ) ;
#51966 = CYLINDRICAL_SURFACE ( 'NONE', #2474, 13.99999999999999822 ) ;
#51967 = EDGE_LOOP ( 'NONE', ( #69534, #15847, #34577, #21510 ) ) ;
#51968 = VERTEX_POINT ( 'NONE', #32548 ) ;
#51969 = PLANE ( 'NONE',  #11667 ) ;
#51970 = AXIS2_PLACEMENT_3D ( 'NONE', #21533, #52532, #68343 ) ;
#51971 = PRESENTATION_STYLE_ASSIGNMENT (( #9759 ) ) ;
#51972 = STYLED_ITEM ( 'NONE', ( #46584 ), #54871 ) ;
#51973 = EDGE_CURVE ( 'NONE', #57448, #12387, #41499, .T. ) ;
#51974 = DIRECTION ( 'NONE',  ( -1.000000000000000000, 0.000000000000000000, 1.300977106640434891E-16 ) ) ;
#51975 =( LENGTH_UNIT ( ) NAMED_UNIT ( * ) SI_UNIT ( .MILLI., .METRE. ) );
#51976 = ORIENTED_EDGE ( 'NONE', *, *, #62409, .F. ) ;
#51977 = VERTEX_POINT ( 'NONE', #491 ) ;
#51978 = CARTESIAN_POINT ( 'NONE',  ( 27.00000000000001776, 43.00000000000000000, 34.49999999999999289 ) ) ;
#51979 = CIRCLE ( 'NONE', #66583, 8.999999999999994671 ) ;
#51980 = VERTEX_POINT ( 'NONE', #22022 ) ;
#51981 = CARTESIAN_POINT ( 'NONE',  ( -9.058813317711338797, 117.4549999999999841, 2.943386871421373563 ) ) ;
#51982 = DIRECTION ( 'NONE',  ( 1.000000000000000000, 0.000000000000000000, 0.000000000000000000 ) ) ;
#51983 = ORIENTED_EDGE ( 'NONE', *, *, #51407, .F. ) ;
#51984 = CIRCLE ( 'NONE', #21641, 0.4999999999999994449 ) ;
#51985 = B_SPLINE_CURVE_WITH_KNOTS ( 'NONE', 3,
 ( #42341, #62675, #36712, #63397, #4988, #25405 ),
 .UNSPECIFIED., .F., .F.,
 ( 4, 2, 4 ),
 ( 0.004189585287972434971, 0.006269578072783811573, 0.008349570857595188175 ),
 .UNSPECIFIED. ) ;
#51986 =( NAMED_UNIT ( * ) PLANE_ANGLE_UNIT ( ) SI_UNIT ( $, .RADIAN. ) );
#51987 = CARTESIAN_POINT ( 'NONE',  ( -107.0949999999999847, -2.607480562269071545, -8.024999999999991473 ) ) ;
#51988 = ORIENTED_EDGE ( 'NONE', *, *, #55760, .T. ) ;
#51989 = FILL_AREA_STYLE ('',( #21604 ) ) ;
#51990 = CIRCLE ( 'NONE', #30622, 1.000000000000000000 ) ;
#51991 = FILL_AREA_STYLE_COLOUR ( '', #48595 ) ;
#51992 = AXIS2_PLACEMENT_3D ( 'NONE', #19520, #61715, #13198 ) ;
#51993 = DIRECTION ( 'NONE',  ( 0.000000000000000000, 1.000000000000000000, 0.000000000000000000 ) ) ;
#51994 = ORIENTED_EDGE ( 'NONE', *, *, #58778, .F. ) ;
#51995 = CARTESIAN_POINT ( 'NONE',  ( 6.826472737025121695, 140.4929263765338021, -4.959722759717905660 ) ) ;
#51996 = CYLINDRICAL_SURFACE ( 'NONE', #47053, 0.5000000000000004441 ) ;
#51997 = AXIS2_PLACEMENT_3D ( 'NONE', #19007, #60211, #49670 ) ;
#51998 = DIRECTION ( 'NONE',  ( -1.000000000000000000, 0.000000000000000000, 0.000000000000000000 ) ) ;
#51999 = ORIENTED_EDGE ( 'NONE', *, *, #56059, .F. ) ;
#52000 = ORIENTED_EDGE ( 'NONE', *, *, #13785, .F. ) ;
#52001 =( NAMED_UNIT ( * ) SI_UNIT ( $, .STERADIAN. ) SOLID_ANGLE_UNIT ( ) );
#52002 = DIRECTION ( 'NONE',  ( -0.000000000000000000, -0.000000000000000000, -1.000000000000000000 ) ) ;
#52003 = CARTESIAN_POINT ( 'NONE',  ( -139.9429263765337907, 0.000000000000000000, 9.524999999999991473 ) ) ;
#52004 = CARTESIAN_POINT ( 'NONE',  ( 5.196152422706631135, 2.500000000000000000, 9.000000000000001776 ) ) ;
#52005 = MECHANICAL_DESIGN_GEOMETRIC_PRESENTATION_REPRESENTATION (  '', ( #32921 ), #68879 ) ;
#52007 = CARTESIAN_POINT ( 'NONE',  ( -127.1050000000000040, -6.826472737025115478, 4.959722759717900331 ) ) ;
#52006 = VECTOR ( 'NONE', #18487, 1000.000000000000114 ) ;
#52008 =( NAMED_UNIT ( * ) PLANE_ANGLE_UNIT ( ) SI_UNIT ( $, .RADIAN. ) );
#52009 = CARTESIAN_POINT ( 'NONE',  ( 4.716976649647099507, 141.7570736234661410, -6.492361379858953008 ) ) ;
#52010 = CARTESIAN_POINT ( 'NONE',  ( 10.00000000000000888, 43.00000000000000000, -45.61250543006183733 ) ) ;
#52011 = EDGE_CURVE ( 'NONE', #10734, #25093, #43526, .T. ) ;
#52012 = AXIS2_PLACEMENT_3D ( 'NONE', #32583, #61319, #59667 ) ;
#52013 = CARTESIAN_POINT ( 'NONE',  ( -126.1429263765337936, 5.598654528085800663, -7.705886871421367523 ) ) ;
#52014 = PLANE ( 'NONE',  #4713 ) ;
#52015 = CARTESIAN_POINT ( 'NONE',  ( 30.50000000000001066, 16.24999999999997513, 3.750000000000000000 ) ) ;
#52016 = VERTEX_POINT ( 'NONE', #36510 ) ;
#52017 = ORIENTED_EDGE ( 'NONE', *, *, #39651, .F. ) ;
#52018 = CARTESIAN_POINT ( 'NONE',  ( 30.99999999999998579, 5.000000000000000000, -72.00402776293822171 ) ) ;
#52019 = DIRECTION ( 'NONE',  ( 1.000000000000000000, 0.000000000000000000, -0.000000000000000000 ) ) ;
#52020 = CARTESIAN_POINT ( 'NONE',  ( 4.716976649647099507, 114.7570736234661553, -6.492361379858953008 ) ) ;
#52021 = ORIENTED_EDGE ( 'NONE', *, *, #1980, .T. ) ;
#52022 = CARTESIAN_POINT ( 'NONE',  ( 3.000000000000030198, 42.00000000000000000, 89.00000000000000000 ) ) ;
#52023 = CARTESIAN_POINT ( 'NONE',  ( -175.4049999999999727, -2.607480562269069768, 8.024999999999991473 ) ) ;
#52024 = DIRECTION ( 'NONE',  ( -0.000000000000000000, -0.000000000000000000, 1.000000000000000000 ) ) ;
#52025 = AXIS2_PLACEMENT_3D ( 'NONE', #50248, #28051, #603 ) ;
#52026 = SURFACE_STYLE_USAGE ( .BOTH. , #4481 ) ;
#52027 = CARTESIAN_POINT ( 'NONE',  ( -48.95707362346615810, 9.058813317711329915, -2.943386871421373119 ) ) ;
#52028 = VECTOR ( 'NONE', #4918, 1000.000000000000000 ) ;
#52029 = CARTESIAN_POINT ( 'NONE',  ( -177.8950000000000102, 6.826472737025115478, 4.959722759717899443 ) ) ;
#52030 = CARTESIAN_POINT ( 'NONE',  ( 41.61274205743404053, 107.5029750606318402, 3.982828305957055726 ) ) ;
#52031 = EDGE_LOOP ( 'NONE', ( #29827, #20937, #3609, #23525, #41746, #38056, #15127, #56892, #38462, #46900, #46010, #62848, #55785, #68627, #66488, #47151, #26941, #5231, #62350, #62609, #51976, #28467, #31179, #68178, #64556, #55870, #5822, #47175, #238, #25485, #32940, #52710, #38102, #18243 ) ) ;
#52032 =( NAMED_UNIT ( * ) PLANE_ANGLE_UNIT ( ) SI_UNIT ( $, .RADIAN. ) );
#52033 = EDGE_CURVE ( 'NONE', #68810, #31091, #5910, .T. ) ;
#52034 = SURFACE_SIDE_STYLE ('',( #29515 ) ) ;
#52035 = CARTESIAN_POINT ( 'NONE',  ( 7.632228543268607446, 117.1570736234661609, 2.479861379858954606 ) ) ;
#52036 = CARTESIAN_POINT ( 'NONE',  ( -91.70499999999998408, 2.607480562269073321, 8.024999999999991473 ) ) ;
#52037 =( LENGTH_UNIT ( ) NAMED_UNIT ( * ) SI_UNIT ( .MILLI., .METRE. ) );
#52038 = FILL_AREA_STYLE_COLOUR ( '', #64034 ) ;
#52039 = EDGE_CURVE ( 'NONE', #32455, #66131, #12380, .T. ) ;
#52040 = COLOUR_RGB ( '', 0.40784314, 0.44705882, 0.49803922) ;
#52041 = CARTESIAN_POINT ( 'NONE',  ( -92.99499999999999034, -6.826472737025113702, 4.959722759717902107 ) ) ;
#52042 = EDGE_CURVE ( 'NONE', #62231, #3129, #26917, .T. ) ;
#52043 = CARTESIAN_POINT ( 'NONE',  ( -10.01517768586949231, 132.3049999999999500, -6.132527647946036459E-16 ) ) ;
#52044 = CARTESIAN_POINT ( 'NONE',  ( -66.44499999999999318, 0.000000000000000000, 8.024999999999991473 ) ) ;
#52045 = CARTESIAN_POINT ( 'NONE',  ( -75.00000000000000000, 9.708372675170620525, -6.000000000000000000 ) ) ;
#52046 =( NAMED_UNIT ( * ) SI_UNIT ( $, .STERADIAN. ) SOLID_ANGLE_UNIT ( ) );
#52047 = CARTESIAN_POINT ( 'NONE',  ( -33.24616929330141346, -8.228704836123991839, -2.000000000009505285 ) ) ;
#52048 = AXIS2_PLACEMENT_3D ( 'NONE', #58084, #9895, #31310 ) ;
#52049 = CARTESIAN_POINT ( 'NONE',  ( -4.750000000000002665, 24.74999999999998579, 3.750000000000000000 ) ) ;
#52050 = DIRECTION ( 'NONE',  ( 1.000000000000000000, 0.000000000000000000, 0.000000000000000000 ) ) ;
#52051 = ORIENTED_EDGE ( 'NONE', *, *, #58221, .F. ) ;
#52052 = EDGE_CURVE ( 'NONE', #34405, #58037, #17788, .T. ) ;
#52053 = CARTESIAN_POINT ( 'NONE',  ( -109.6429263765338078, -5.598654528085801552, 7.705886871421367523 ) ) ;
#52054 =( BOUNDED_CURVE ( )  B_SPLINE_CURVE ( 2, ( #19053, #68667, #29635, #52504, #52161, #14159, #58116, #41970, #25392, #25725, #14485 ),
 .UNSPECIFIED., .F., .F. ) 
 B_SPLINE_CURVE_WITH_KNOTS ( ( 3, 2, 2, 2, 2, 3 ),
 ( 0.5217391304347703818, 0.5239130434782486301, 0.5260869565217267674, 0.5282608695652050157, 0.5304347826086832640, 0.5326086956521615123 ),
 .UNSPECIFIED. ) 
 CURVE ( )  GEOMETRIC_REPRESENTATION_ITEM ( )  RATIONAL_B_SPLINE_CURVE ( ( 1.000000000000274891, 0.9510565162948785289, 1.000000000000000000, 0.9510565162951535312, 1.000000000000000000, 0.9510565162951535312, 1.000000000000000000, 0.9510565162951535312, 1.000000000000000000, 0.9510565162954335294, 0.9999999999997200018 ) ) 
 REPRESENTATION_ITEM ( '' )  );
#52055 = CARTESIAN_POINT ( 'NONE',  ( -125.0949999999999847, -2.607480562269071545, -8.024999999999991473 ) ) ;
#52056 = PRESENTATION_STYLE_ASSIGNMENT (( #18958 ) ) ;
#52057 = EDGE_CURVE ( 'NONE', #51702, #43100, #22500, .T. ) ;
#52058 =( NAMED_UNIT ( * ) SI_UNIT ( $, .STERADIAN. ) SOLID_ANGLE_UNIT ( ) );
#52060 = DIRECTION ( 'NONE',  ( -0.000000000000000000, -1.000000000000000000, 0.000000000000000000 ) ) ;
#52059 = CARTESIAN_POINT ( 'NONE',  ( -75.00000000000000000, -2.215169945516535778E-14, -9.500000000000000000 ) ) ;
#52061 = CARTESIAN_POINT ( 'NONE',  ( 0.000000000000000000, 2.500000000000000000, 0.000000000000000000 ) ) ;
#52062 = ORIENTED_EDGE ( 'NONE', *, *, #11634, .F. ) ;
#52064 = EDGE_LOOP ( 'NONE', ( #61150, #7997 ) ) ;
#52063 = CIRCLE ( 'NONE', #62118, 0.5000000000000004441 ) ;
#52065 = STYLED_ITEM ( 'NONE', ( #67530 ), #61447 ) ;
#52066 = MECHANICAL_DESIGN_GEOMETRIC_PRESENTATION_REPRESENTATION (  '', ( #20615 ), #29599 ) ;
#52067 = DIRECTION ( 'NONE',  ( -0.000000000000000000, -0.000000000000000000, 1.000000000000000000 ) ) ;
#52068 = CARTESIAN_POINT ( 'NONE',  ( 20.42000000000000526, 0.000000000000000000, -12.50000000000000000 ) ) ;
#52069 = DIRECTION ( 'NONE',  ( -1.000000000000000000, -0.000000000000000000, -0.000000000000000000 ) ) ;
#52070 = FILL_AREA_STYLE ('',( #42249 ) ) ;
#52071 = ORIENTED_EDGE ( 'NONE', *, *, #29555, .T. ) ;
#52072 = CARTESIAN_POINT ( 'NONE',  ( -122.9049999999999727, 2.607480562269069324, -8.024999999999993250 ) ) ;
#52073 = ORIENTED_EDGE ( 'NONE', *, *, #52669, .F. ) ;
#52074 = FILL_AREA_STYLE_COLOUR ( '', #51093 ) ;
#52075 = CARTESIAN_POINT ( 'NONE',  ( -127.8570736234661780, -5.598654528085803328, -7.705886871421366635 ) ) ;
#52076 = VECTOR ( 'NONE', #49052, 1000.000000000000000 ) ;
#52077 = ORIENTED_EDGE ( 'NONE', *, *, #39445, .F. ) ;
#52078 = DIRECTION ( 'NONE',  ( 0.000000000000000000, 0.000000000000000000, -1.000000000000000000 ) ) ;
#52079 = CARTESIAN_POINT ( 'NONE',  ( -45.50000000000000000, -2.024042244987997205E-14, 10.00000000000000000 ) ) ;
#52080 = ORIENTED_EDGE ( 'NONE', *, *, #66895, .F. ) ;
#52081 = PRESENTATION_LAYER_ASSIGNMENT (  '', '', ( #27322 ) ) ;
#52082 = EDGE_CURVE ( 'NONE', #57372, #18616, #69640, .T. ) ;
#52083 = CARTESIAN_POINT ( 'NONE',  ( -87.50000000000000000, -6.499999999999990230, 21.00000000000000000 ) ) ;
#52084 =( BOUNDED_CURVE ( )  B_SPLINE_CURVE ( 2, ( #14438, #57364, #20780, #42289, #20420, #68274, #9549, #30966, #41924, #36297, #20056 ),
 .UNSPECIFIED., .F., .F. ) 
 B_SPLINE_CURVE_WITH_KNOTS ( ( 3, 2, 2, 2, 2, 3 ),
 ( 0.6764705882352943789, 0.6823529411764708286, 0.6882352941176472783, 0.6941176470588237279, 0.7000000000000001776, 0.7058823529411767383 ),
 .UNSPECIFIED. ) 
 CURVE ( )  GEOMETRIC_REPRESENTATION_ITEM ( )  RATIONAL_B_SPLINE_CURVE ( ( 0.9999999999999981126, 0.9510565162951554186, 1.000000000000000000, 0.9510565162951535312, 1.000000000000000000, 0.9510565162951535312, 1.000000000000000000, 0.9510565162951535312, 1.000000000000000000, 0.9510565162951516438, 1.000000000000001776 ) ) 
 REPRESENTATION_ITEM ( '' )  );
#52085 = CARTESIAN_POINT ( 'NONE',  ( 3.094860106618431583, 147.0949999999999704, 9.525000000000000355 ) ) ;
#52086 = DIRECTION ( 'NONE',  ( 0.000000000000000000, 0.000000000000000000, -1.000000000000000000 ) ) ;
#52087 = VECTOR ( 'NONE', #7266, 1000.000000000000000 ) ;
#52088 = ORIENTED_EDGE ( 'NONE', *, *, #96, .T. ) ;
#52089 = SURFACE_STYLE_FILL_AREA ( #35885 ) ;
#52090 = CARTESIAN_POINT ( 'NONE',  ( 9.058813317711337021, 151.6549999999999727, 2.943386871421375783 ) ) ;
#52091 = DIRECTION ( 'NONE',  ( 0.000000000000000000, 0.000000000000000000, 1.000000000000000000 ) ) ;
#52092 = CIRCLE ( 'NONE', #16143, 4.999999999999997335 ) ;
#52093 = ORIENTED_EDGE ( 'NONE', *, *, #16069, .T. ) ;
#52094 = CARTESIAN_POINT ( 'NONE',  ( 4.716976649647099507, 113.6429263765338078, -6.492361379858953008 ) ) ;
#52095 = DIRECTION ( 'NONE',  ( 0.000000000000000000, -1.000000000000000000, 0.000000000000000000 ) ) ;
#52096 = FACE_OUTER_BOUND ( 'NONE', #22998, .T. ) ;
#52097 = CARTESIAN_POINT ( 'NONE',  ( -99.44292637653380496, -1.166476076187852838E-15, -9.524999999999991473 ) ) ;
#52098 = AXIS2_PLACEMENT_3D ( 'NONE', #58466, #10290, #5667 ) ;
#52099 = AXIS2_PLACEMENT_3D ( 'NONE', #56967, #4517, #24585 ) ;
#52100 =( NAMED_UNIT ( * ) SI_UNIT ( $, .STERADIAN. ) SOLID_ANGLE_UNIT ( ) );
#52101 = CARTESIAN_POINT ( 'NONE',  ( 45.59262096826685706, 9.979230606950402205, -6.500000000000001776 ) ) ;
#52102 = EDGE_LOOP ( 'NONE', ( #13463, #23492, #22269, #64146, #64948 ) ) ;
#52103 = CARTESIAN_POINT ( 'NONE',  ( 31.00000000000001421, 43.00000000000000000, 45.61250543006183022 ) ) ;
#52104 = ORIENTED_EDGE ( 'NONE', *, *, #29879, .F. ) ;
#52105 = CARTESIAN_POINT ( 'NONE',  ( -59.54292637653379927, 9.058813317711329915, 2.943386871421369566 ) ) ;
#52106 = CARTESIAN_POINT ( 'NONE',  ( 11.00000000000001776, 42.00000000000000000, -28.00000000000000000 ) ) ;
#52107 = CARTESIAN_POINT ( 'NONE',  ( -4.358330484967983587, -6.451150163859152187, 0.7660251680141582087 ) ) ;
#52108 = CARTESIAN_POINT ( 'NONE',  ( -155.0050000000000239, 6.826472737025116366, 4.959722759717898555 ) ) ;
#52109 = VERTEX_POINT ( 'NONE', #34303 ) ;
#52110 = FILL_AREA_STYLE_COLOUR ( '', #10425 ) ;
#52111 =( NAMED_UNIT ( * ) PLANE_ANGLE_UNIT ( ) SI_UNIT ( $, .RADIAN. ) );
#52112 = CARTESIAN_POINT ( 'NONE',  ( -54.91675365088294569, -8.999709270181570631, 4.695517540642841325 ) ) ;
#52113 = CARTESIAN_POINT ( 'NONE',  ( 74.62643842725375976, 19.76989462323618341, 6.307273367294704336 ) ) ;
#52114 = CARTESIAN_POINT ( 'NONE',  ( 9.827790563157511022E-16, 87.30187232391182306, -8.025000000000000355 ) ) ;
#52115 = ORIENTED_EDGE ( 'NONE', *, *, #50754, .F. ) ;
#52116 = ORIENTED_EDGE ( 'NONE', *, *, #35180, .F. ) ;
#52117 = CARTESIAN_POINT ( 'NONE',  ( 23.15216539473883373, 24.61138016253714156, 27.21282383882673983 ) ) ;
#52118 = CARTESIAN_POINT ( 'NONE',  ( 3.000000000000002665, 38.70020753820971748, -89.00000000000000000 ) ) ;
#52120 = CARTESIAN_POINT ( 'NONE',  ( -62.90499999999997982, 2.607480562269068880, -8.024999999999993250 ) ) ;
#52119 = PRESENTATION_LAYER_ASSIGNMENT (  '', '', ( #47781 ) ) ;
#52121 = VERTEX_POINT ( 'NONE', #6501 ) ;
#52122 = DIRECTION ( 'NONE',  ( 0.000000000000000000, 0.000000000000000000, -1.000000000000000000 ) ) ;
#52123 = EDGE_CURVE ( 'NONE', #24250, #64166, #44970, .T. ) ;
#52124 = PRESENTATION_LAYER_ASSIGNMENT (  '', '', ( #57729 ) ) ;
#52125 = MECHANICAL_DESIGN_GEOMETRIC_PRESENTATION_REPRESENTATION (  '', ( #29595 ), #2631 ) ;
#52126 = CARTESIAN_POINT ( 'NONE',  ( 21.25000000000001066, 24.74999999999998224, -3.750000000000000000 ) ) ;
#52127 = ORIENTED_EDGE ( 'NONE', *, *, #46171, .T. ) ;
#52128 = CIRCLE ( 'NONE', #47527, 3.000000000000000444 ) ;
#52129 = CIRCLE ( 'NONE', #44259, 5.000000000000000888 ) ;
#52130 = ADVANCED_FACE ( 'NONE', ( #11454 ), #22361, .F. ) ;
#52131 = PRESENTATION_STYLE_ASSIGNMENT (( #30624 ) ) ;
#52133 = DIRECTION ( 'NONE',  ( -0.4999999999999998890, 0.000000000000000000, -0.8660254037844385966 ) ) ;
#52132 =( NAMED_UNIT ( * ) PLANE_ANGLE_UNIT ( ) SI_UNIT ( $, .RADIAN. ) );
#52134 = ADVANCED_FACE ( 'NONE', ( #22712 ), #7565, .F. ) ;
#52135 = VECTOR ( 'NONE', #53845, 1000.000000000000000 ) ;
#52136 = CARTESIAN_POINT ( 'NONE',  ( 9.058813317711337021, 147.5449999999999875, 2.943386871421375783 ) ) ;
#52137 = CARTESIAN_POINT ( 'NONE',  ( -100.1949999999999790, 8.437984349512085203, -1.550032578732815448E-15 ) ) ;
#52138 = SURFACE_STYLE_USAGE ( .BOTH. , #68643 ) ;
#52139 = CIRCLE ( 'NONE', #57743, 27.49999999999999645 ) ;
#52140 = DIRECTION ( 'NONE',  ( -0.000000000000000000, 1.000000000000000000, -0.000000000000000000 ) ) ;
#52141 = CIRCLE ( 'NONE', #53237, 5.000000000000004441 ) ;
#52142 = CARTESIAN_POINT ( 'NONE',  ( -71.54292637653379927, 9.058813317711329915, 2.943386871421369566 ) ) ;
#52143 = ORIENTED_EDGE ( 'NONE', *, *, #42538, .F. ) ;
#52144 = CARTESIAN_POINT ( 'NONE',  ( -142.0429263765338135, -9.058813317711329915, -2.943386871421370898 ) ) ;
#52145 = VECTOR ( 'NONE', #67598, 1000.000000000000000 ) ;
#52146 = CARTESIAN_POINT ( 'NONE',  ( -155.2450000000000045, -4.716976649647093289, -6.492361379858945902 ) ) ;
#52147 = DIRECTION ( 'NONE',  ( -0.000000000000000000, 0.000000000000000000, -1.000000000000000000 ) ) ;
#52148 = CONICAL_SURFACE ( 'NONE', #44283, 9.000000000000007105, 0.7853981633974500554 ) ;
#52149 = EDGE_CURVE ( 'NONE', #61605, #14417, #23740, .T. ) ;
#52150 = DIRECTION ( 'NONE',  ( 0.6216216216216174928, -0.7833176619561892373, 0.000000000000000000 ) ) ;
#52151 = CARTESIAN_POINT ( 'NONE',  ( 5.590169943749474513, 0.000000000000000000, 0.000000000000000000 ) ) ;
#52152 = CARTESIAN_POINT ( 'NONE',  ( 0.000000000000000000, -2.500000000000000000, 0.000000000000000000 ) ) ;
#52153 = EDGE_LOOP ( 'NONE', ( #20019, #9430, #57003, #43119, #37781, #22388, #8552, #60601 ) ) ;
#52155 = VERTEX_POINT ( 'NONE', #44210 ) ;
#52154 = AXIS2_PLACEMENT_3D ( 'NONE', #15161, #20032, #58372 ) ;
#52156 =( NAMED_UNIT ( * ) SI_UNIT ( $, .STERADIAN. ) SOLID_ANGLE_UNIT ( ) );
#52157 = AXIS2_PLACEMENT_3D ( 'NONE', #11860, #50886, #17171 ) ;
#52158 = AXIS2_PLACEMENT_3D ( 'NONE', #68423, #53623, #20220 ) ;
#52159 = CARTESIAN_POINT ( 'NONE',  ( -144.2929263765342967, 3.094860106609957917, -9.525000000006148326 ) ) ;
#52160 = CARTESIAN_POINT ( 'NONE',  ( 2.607480562269113733, 118.5929263765338391, 8.024999999999973710 ) ) ;
#52161 = CARTESIAN_POINT ( 'NONE',  ( -110.4570736234661723, -9.058813317711329915, 2.943386871421371787 ) ) ;
#52162 = CARTESIAN_POINT ( 'NONE',  ( -60.70461754965442935, -7.499999999999993783, 2.168404344971008868E-16 ) ) ;
#52163 = ORIENTED_EDGE ( 'NONE', *, *, #34179, .F. ) ;
#52164 = CARTESIAN_POINT ( 'NONE',  ( -161.6049999999999898, 6.826472737025113702, -4.959722759717902107 ) ) ;
#52165 = VECTOR ( 'NONE', #1354, 1000.000000000000000 ) ;
#52166 = ORIENTED_EDGE ( 'NONE', *, *, #46983, .T. ) ;
#52167 = LINE ( 'NONE', #57060, #5437 ) ;
#52168 = LINE ( 'NONE', #31017, #9598 ) ;
#52169 = VERTEX_POINT ( 'NONE', #39614 ) ;
#52170 = VECTOR ( 'NONE', #27620, 1000.000000000000000 ) ;
#52171 = LINE ( 'NONE', #68675, #7958 ) ;
#52172 = EDGE_CURVE ( 'NONE', #15394, #35956, #62901, .T. ) ;
#52173 = LINE ( 'NONE', #69367, #55631 ) ;
#52174 = CARTESIAN_POINT ( 'NONE',  ( -7.632228543268608334, 157.9570736234661581, 2.479861379858952830 ) ) ;
#52175 = VERTEX_POINT ( 'NONE', #54361 ) ;
#52176 = DIRECTION ( 'NONE',  ( 0.000000000000000000, 0.000000000000000000, 1.000000000000000000 ) ) ;
#52177 = CARTESIAN_POINT ( 'NONE',  ( 10.01517768586949408, 124.8049999999999784, 1.839758294383810543E-15 ) ) ;
#52178 = CARTESIAN_POINT ( 'NONE',  ( -69.95499999999998408, -7.632228543268599452, 2.479861379858951054 ) ) ;
#52179 =( LENGTH_UNIT ( ) NAMED_UNIT ( * ) SI_UNIT ( .MILLI., .METRE. ) );
#52180 = ORIENTED_EDGE ( 'NONE', *, *, #5307, .F. ) ;
#52181 = CARTESIAN_POINT ( 'NONE',  ( 10.01517768586949231, 136.8049999999999500, 1.839758294383810543E-15 ) ) ;
#52182 = SURFACE_SIDE_STYLE ('',( #26773 ) ) ;
#52183 = AXIS2_PLACEMENT_3D ( 'NONE', #29893, #51008, #50660 ) ;
#52184 = DIRECTION ( 'NONE',  ( 0.000000000000000000, 0.000000000000000000, 1.000000000000000000 ) ) ;
#52185 = ORIENTED_EDGE ( 'NONE', *, *, #52288, .F. ) ;
#52186 = DIRECTION ( 'NONE',  ( -1.000000000000000000, -0.000000000000000000, -0.000000000000000000 ) ) ;
#52187 = CARTESIAN_POINT ( 'NONE',  ( -178.4050000000000011, -2.607480562269069768, 8.024999999999991473 ) ) ;
#52188 = EDGE_LOOP ( 'NONE', ( #60702, #14541, #46291, #10989 ) ) ;
#52189 = CARTESIAN_POINT ( 'NONE',  ( 31.00000000000001421, 43.00000000000000000, 45.61250543006183022 ) ) ;
#52190 =( BOUNDED_CURVE ( )  B_SPLINE_CURVE ( 2, ( #2514, #24023, #8205, #55688, #56019, #56740, #51119, #24693, #46212, #29987, #67633, #40932, #24355, #7497, #8884, #62352, #35633, #51811, #39895, #28926, #45850, #35278, #57069, #13817, #50764, #19070, #45530, #61302, #3563, #40224, #13113, #67999, #7836, #50413, #40575, #2138, #61990, #18411, #9939, #3934, #68682, #46921, #68331, #15245, #58812, #20112, #37049, #58129, #31361, #10627, #19784, #42674, #42342, #4263, #48290, #32077, #15574, #15927, #4637, #36713, #41620, #52860, #62676, #63036, #52519, #53535, #26093, #20482, #30670, #14880, #63398, #47625, #37409, #35979, #69032, #5320, #20841, #36362, #26763, #25744, #47262, #41278, #14503, #58463, #9608, #57423, #63727, #41989, #64076, #10287, #31720, #53204, #9252, #4989, #31025, #52177, #26442, #25406, #57783, #47972, #69372, #21162, #22562, #49648, #38781, #1392, #64780, #7074, #5664, #683, #28504, #33460, #44420, #22921, #65821, #55247, #27798, #59480, #28140, #39121, #6712, #43031, #16618, #11655, #60510, #10962, #27111, #43710, #49303, #17654, #16284, #1014, #12324, #33125, #344, #33797, #32763, #27466, #59846, #38445, #40559, #11308, #21513, #44064, #48992, #64436, #22215, #65105, #16958, #37760, #60192, #54214, #59137, #54560, #32398, #53865, #6030, #48646, #38083, #21879, #43389, #11999, #6369, #65469, #17320, #54886, #50682, #56991, #13732, #24608, #3115, #46125, #35553, #8117, #39814, #8478, #19345, #56650, #50007, #29194, #35191, #40848, #2424, #61913, #34152, #50337, #29913, #67197, #51032, #18675, #23936, #24282, #44752, #14092, #66870, #55609, #62266, #17976, #60868, #8803, #55947, #13373, #61230, #1745, #18986, #34834, #23255, #51370, #7433, #66145, #2792, #34493, #56287, #45451, #12681, #67548, #28854, #39465, #40153, #2061, #23587, #61547, #40495, #29561, #45099, #66511, #18334, #13040, #45778, #7751, #41895, #25658, #14414, #57693, #58726, #15162, #63988, #37318, #35886, #10198, #30230, #9168, #46846, #63313, #3474, #30583, #62946, #15838, #36633, #9525, #31636, #68947, #53115, #25324, #51726, #57333, #30942, #24975, #63654, #4903, #26354, #58051, #46485, #68596, #4182, #47892, #67911, #52439, #19703, #68250, #9858, #21084, #47176, #42265, #52090, #3841, #69291, #47534, #31274, #20394, #52772, #15495, #20757, #4547, #41199, #42585, #36962, #58373, #62600, #20033, #41530, #26005, #14792, #36269, #27717 ),
 .UNSPECIFIED., .F., .T. ) 
 B_SPLINE_CURVE_WITH_KNOTS ( ( 3, 2, 2, 2, 2, 2, 2, 2, 2, 2, 2, 2, 2, 2, 2, 2, 2, 2, 2, 2, 2, 2, 2, 2, 2, 2, 2, 2, 2, 2, 2, 2, 2, 2, 2, 2, 2, 2, 2, 2, 2, 2, 2, 2, 2, 2, 2, 2, 2, 2, 2, 2, 2, 2, 2, 2, 2, 2, 2, 2, 2, 2, 2, 2, 2, 2, 2, 2, 2, 2, 2, 2, 2, 2, 2, 2, 2, 2, 2, 2, 2, 2, 2, 2, 2, 2, 2, 2, 2, 2, 2, 2, 2, 2, 2, 2, 2, 2, 2, 2, 2, 2, 2, 2, 2, 2, 2, 2, 2, 2, 2, 2, 2, 2, 2, 2, 2, 2, 2, 2, 2, 2, 2, 2, 2, 2, 2, 2, 2, 2, 2, 2, 2, 2, 2, 2, 2, 2, 2, 2, 2, 2, 2, 2, 2, 2, 2, 3 ),
 ( 0.000000000000000000, 0.005882352941176470507, 0.01176470588235294101, 0.01764705882352941152, 0.02352941176470588203, 0.02941176470588234906, 0.03529411764705882304, 0.04117647058823529355, 0.04705882352941176405, 0.05294117647058823456, 0.05882352941176469813, 0.06470588235294118251, 0.07058823529411764608, 0.07647058823529412352, 0.08235294117647058709, 0.08823529411764706454, 0.09411764705882352811, 0.1000000000000000194, 0.1058823529411764691, 0.1117647058823529466, 0.1176470588235293963, 0.1235294117647058876, 0.1294117647058823650, 0.1352941176470588147, 0.1411764705882352922, 0.1470588235294117696, 0.1529411764705882470, 0.1588235294117646967, 0.1647058823529411742, 0.1705882352941176794, 0.1764705882352941291, 0.1823529411764705788, 0.1882352941176470562, 0.1941176470588235337, 0.2000000000000000389, 0.2058823529411764330, 0.2117647058823529382, 0.2176470588235294157, 0.2235294117647058931, 0.2294117647058823428, 0.2352941176470587925, 0.2411764705882352977, 0.2470588235294117752, 0.2529411764705882248, 0.2588235294117647300, 0.2647058823529411797, 0.2705882352941176294, 0.2764705882352941346, 0.2823529411764705843, 0.2882352941176470340, 0.2941176470588235392, 0.2999999999999999889, 0.3058823529411764941, 0.3117647058823529438, 0.3176470588235293935, 0.3235294117647058987, 0.3294117647058823484, 0.3352941176470587981, 0.3411764705882353588, 0.3470588235294116974, 0.3529411764705882582, 0.3588235294117647078, 0.3647058823529411575, 0.3705882352941176627, 0.3764705882352941124, 0.3823529411764705621, 0.3882352941176470673, 0.3941176470588235170, 0.4000000000000000777, 0.4058823529411765274, 0.4117647058823528661, 0.4176470588235294268, 0.4235294117647058765, 0.4294117647058823262, 0.4352941176470588314, 0.4411764705882352811, 0.4470588235294117863, 0.4529411764705882359, 0.4588235294117646856, 0.4647058823529412463, 0.4705882352941175850, 0.4764705882352940347, 0.4823529411764705954, 0.4882352941176470451, 0.4941176470588235503, 0.5000000000000000000, 0.5058823529411764497, 0.5117647058823528994, 0.5176470588235294601, 0.5235294117647059098, 0.5294117647058823595, 0.5352941176470588092, 0.5411764705882352589, 0.5470588235294118196, 0.5529411764705882693, 0.5588235294117647189, 0.5647058823529411686, 0.5705882352941176183, 0.5764705882352940680, 0.5823529411764706287, 0.5882352941176470784, 0.5941176470588235281, 0.5999999999999999778, 0.6058823529411764275, 0.6117647058823529882, 0.6176470588235294379, 0.6235294117647058876, 0.6294117647058823373, 0.6352941176470587870, 0.6411764705882353477, 0.6470588235294117974, 0.6529411764705882470, 0.6588235294117646967, 0.6647058823529411464, 0.6705882352941175961, 0.6764705882352942679, 0.6823529411764707175, 0.6882352941176469452, 0.6941176470588233949, 0.6999999999999998446, 0.7058823529411765163, 0.7117647058823529660, 0.7176470588235294157, 0.7235294117647058654, 0.7294117647058823151, 0.7352941176470588758, 0.7411764705882353255, 0.7470588235294117752, 0.7529411764705882248, 0.7588235294117646745, 0.7647058823529411242, 0.7705882352941176849, 0.7764705882352941346, 0.7823529411764705843, 0.7882352941176470340, 0.7941176470588234837, 0.8000000000000001554, 0.8058823529411766051, 0.8117647058823530548, 0.8176470588235292825, 0.8235294117647057321, 0.8294117647058824039, 0.8352941176470588536, 0.8411764705882353033, 0.8470588235294117530, 0.8529411764705882026, 0.8588235294117646523, 0.8616690633200179139 ),
 .UNSPECIFIED. ) 
 CURVE ( )  GEOMETRIC_REPRESENTATION_ITEM ( )  RATIONAL_B_SPLINE_CURVE ( ( 1.000000000000000000, 0.9510565162951535312, 1.000000000000000000, 0.9510565162951535312, 1.000000000000000000, 0.9510565162951535312, 1.000000000000000000, 0.9510565162951535312, 1.000000000000000000, 0.9510565162951535312, 1.000000000000000000, 0.9510565162951535312, 1.000000000000000000, 0.9510565162951535312, 1.000000000000000000, 0.9510565162951535312, 1.000000000000000000, 0.9510565162951535312, 1.000000000000000000, 0.9510565162951535312, 1.000000000000000000, 0.9510565162951535312, 1.000000000000000000, 0.9510565162951535312, 1.000000000000000000, 0.9510565162951535312, 1.000000000000000000, 0.9510565162951535312, 1.000000000000000000, 0.9510565162951535312, 1.000000000000000000, 0.9510565162951535312, 1.000000000000000000, 0.9510565162951535312, 1.000000000000000000, 0.9510565162951535312, 1.000000000000000000, 0.9510565162951535312, 1.000000000000000000, 0.9510565162951535312, 1.000000000000000000, 0.9510565162951535312, 1.000000000000000000, 0.9510565162951535312, 1.000000000000000000, 0.9510565162951535312, 1.000000000000000000, 0.9510565162951535312, 1.000000000000000000, 0.9510565162951535312, 1.000000000000000000, 0.9510565162951535312, 1.000000000000000000, 0.9510565162951535312, 1.000000000000000000, 0.9510565162951535312, 1.000000000000000000, 0.9510565162951535312, 1.000000000000000000, 0.9510565162951535312, 1.000000000000000000, 0.9510565162951535312, 1.000000000000000000, 0.9510565162951535312, 1.000000000000000000, 0.9510565162951535312, 1.000000000000000000, 0.9510565162951535312, 1.000000000000000000, 0.9510565162951535312, 1.000000000000000000, 0.9510565162951535312, 1.000000000000000000, 0.9510565162951535312, 1.000000000000000000, 0.9510565162951535312, 1.000000000000000000, 0.9510565162951535312, 1.000000000000000000, 0.9510565162951535312, 1.000000000000000000, 0.9510565162951535312, 1.000000000000000000, 0.9510565162951535312, 1.000000000000000000, 0.9510565162951535312, 1.000000000000000000, 0.9510565162951535312, 1.000000000000000000, 0.9510565162951535312, 1.000000000000000000, 0.9510565162951535312, 1.000000000000000000, 0.9510565162951535312, 1.000000000000000000, 0.9510565162951535312, 1.000000000000000000, 0.9510565162951535312, 1.000000000000000000, 0.9510565162951535312, 1.000000000000000000, 0.9510565162951535312, 1.000000000000000000, 0.9510565162951535312, 1.000000000000000000, 0.9510565162951535312, 1.000000000000000000, 0.9510565162951535312, 1.000000000000000000, 0.9510565162951535312, 1.000000000000000000, 0.9510565162951535312, 1.000000000000000000, 0.9510565162951535312, 1.000000000000000000, 0.9510565162951535312, 1.000000000000000000, 0.9510565162951535312, 1.000000000000000000, 0.9510565162951535312, 1.000000000000000000, 0.9510565162951535312, 1.000000000000000000, 0.9510565162951535312, 1.000000000000000000, 0.9510565162951535312, 1.000000000000000000, 0.9510565162951535312, 1.000000000000000000, 0.9510565162951535312, 1.000000000000000000, 0.9510565162951535312, 1.000000000000000000, 0.9510565162951535312, 1.000000000000000000, 0.9510565162951535312, 1.000000000000000000, 0.9510565162951535312, 1.000000000000000000, 0.9510565162951535312, 1.000000000000000000, 0.9510565162951535312, 1.000000000000000000, 0.9510565162951535312, 1.000000000000000000, 0.9510565162951535312, 1.000000000000000000, 0.9510565162951535312, 1.000000000000000000, 0.9510565162951535312, 1.000000000000000000, 0.9510565162951535312, 1.000000000000000000, 0.9510565162951535312, 1.000000000000000000, 0.9510565162951535312, 1.000000000000000000, 0.9510565162951535312, 1.000000000000000000, 0.9510565162951535312, 1.000000000000000000, 0.9510565162951535312, 1.000000000000000000, 0.9510565162951535312, 1.000000000000000000, 0.9510565162951535312, 1.000000000000000000, 0.9510565162951535312, 1.000000000000000000, 0.9510565162951535312, 1.000000000000000000, 0.9510565162951535312, 1.000000000000000000, 0.9510565162951535312, 1.000000000000000000, 0.9510565162951535312, 1.000000000000000000, 0.9510565162951535312, 1.000000000000000000, 0.9510565162951535312, 1.000000000000000000, 0.9510565162951535312, 1.000000000000000000, 0.9510565162951535312, 1.000000000000000000, 0.9510565162951535312, 1.000000000000000000, 0.9510565162951535312, 1.000000000000000000, 0.9510565162951535312, 1.000000000000000000, 0.9510565162951535312, 1.000000000000000000, 0.9510565162951535312, 1.000000000000000000, 0.9510565162951535312, 1.000000000000000000, 0.9510565162951535312, 1.000000000000000000, 0.9510565162951535312, 1.000000000000000000, 0.9510565162951535312, 1.000000000000000000, 0.9510565162951535312, 1.000000000000000000, 0.9510565162951535312, 1.000000000000000000, 0.9510565162951535312, 1.000000000000000000, 0.9510565162951535312, 1.000000000000000000, 0.9510565162951535312, 1.000000000000000000, 0.9510565162951535312, 1.000000000000000000, 0.9510565162951535312, 1.000000000000000000, 0.9510565162951535312, 1.000000000000000000, 0.9510565162951535312, 1.000000000000000000, 0.9510565162951535312, 1.000000000000000000, 0.9510565162951535312, 1.000000000000000000, 0.9510565162951535312, 1.000000000000000000, 0.9510565162951535312, 1.000000000000000000, 0.9510565162951535312, 1.000000000000000000, 0.9510565162951535312, 1.000000000000000000, 0.9510565162951535312, 1.000000000000000000, 0.9510565162951535312, 1.000000000000000000, 0.9510565162951535312, 1.000000000000000000, 0.9510565162951535312, 1.000000000000000000, 0.9510565162951535312, 1.000000000000000000, 0.9510565162951535312, 1.000000000000000000, 0.9510565162951535312, 1.000000000000000000, 0.9510565162951535312, 1.000000000000000000, 0.9510565162951535312, 1.000000000000000000, 0.9510565162951535312, 1.000000000000000000, 0.9510565162951535312, 1.000000000000000000, 0.9510565162951535312, 1.000000000000000000, 0.9510565162951535312, 1.000000000000000000, 0.9510565162951535312, 1.000000000000000000, 0.9510565162951535312, 1.000000000000000000, 0.9510565162951535312, 1.000000000000000000, 0.9510565162951535312, 1.000000000000000000, 0.9510565162951535312, 1.000000000000000000, 0.9510565162951535312, 1.000000000000000000, 0.9510565162951535312, 1.000000000000000000, 0.9510565162951535312, 1.000000000000000000, 0.9510565162951535312, 1.000000000000000000, 0.9510565162951535312, 1.000000000000000000, 0.9510565162951535312, 1.000000000000000000, 0.9510565162951535312, 1.000000000000000000, 0.9510565162951535312, 1.000000000000000000, 0.9510565162951535312, 1.000000000000000000, 0.9510565162951535312, 1.000000000000000000, 0.9510565162951535312, 1.000000000000000000, 0.9510565162951535312, 1.000000000000000000, 0.9763240417800694848, 0.9755541358147066244 ) ) 
 REPRESENTATION_ITEM ( '' )  );
#52191 = COLOUR_RGB ( '', 0.08235294, 0.09019608, 0.10196078) ;
#52192 =( NAMED_UNIT ( * ) SI_UNIT ( $, .STERADIAN. ) SOLID_ANGLE_UNIT ( ) );
#52193 = MECHANICAL_DESIGN_GEOMETRIC_PRESENTATION_REPRESENTATION (  '', ( #35351 ), #3821 ) ;
#52194 = ORIENTED_EDGE ( 'NONE', *, *, #45624, .F. ) ;
#52195 = CARTESIAN_POINT ( 'NONE',  ( 0.000000000000000000, 121.0570736234661524, -8.025000000000000355 ) ) ;
#52196 = ORIENTED_EDGE ( 'NONE', *, *, #9246, .F. ) ;
#52197 =( GEOMETRIC_REPRESENTATION_CONTEXT ( 3 ) GLOBAL_UNCERTAINTY_ASSIGNED_CONTEXT ( ( #61634 ) ) GLOBAL_UNIT_ASSIGNED_CONTEXT ( ( #31344, #62663, #14863 ) ) REPRESENTATION_CONTEXT ( 'NONE', 'WORKASPACE' ) );
#52198 = FILL_AREA_STYLE ('',( #19811 ) ) ;
#52199 = CARTESIAN_POINT ( 'NONE',  ( -92.30499999999999261, 8.437984349512085203, -1.550032578732815448E-15 ) ) ;
#52200 = ORIENTED_EDGE ( 'NONE', *, *, #16087, .T. ) ;
#52201 = SURFACE_STYLE_FILL_AREA ( #3963 ) ;
#52202 = ADVANCED_FACE ( 'NONE', ( #27610 ), #817, .F. ) ;
#52203 = DIRECTION ( 'NONE',  ( -1.000000000000000000, 0.000000000000000000, 0.000000000000000000 ) ) ;
#52204 = CARTESIAN_POINT ( 'NONE',  ( -142.2570736234661695, 5.598654528085800663, -7.705886871421367523 ) ) ;
#52205 = CARTESIAN_POINT ( 'NONE',  ( 12.25000000000000533, 28.24999999999998224, -4.000000000000000000 ) ) ;
#52206 = CARTESIAN_POINT ( 'NONE',  ( 3.094860106618435136, 151.2949999999999875, -9.525000000000000355 ) ) ;
#52207 = CARTESIAN_POINT ( 'NONE',  ( -74.90707362346616094, -3.094860106618429807, 9.524999999999991473 ) ) ;
#52208 = AXIS2_PLACEMENT_3D ( 'NONE', #17274, #27068, #37714 ) ;
#52209 = VERTEX_POINT ( 'NONE', #36049 ) ;
#52210 = DIRECTION ( 'NONE',  ( -0.000000000000000000, -1.000000000000000000, -0.000000000000000000 ) ) ;
#52211 = CARTESIAN_POINT ( 'NONE',  ( -15.00000000000000000, -10.90871211463571022, -5.000000000000000000 ) ) ;
#52213 = DIRECTION ( 'NONE',  ( 0.000000000000000000, 0.000000000000000000, -1.000000000000000000 ) ) ;
#52212 = SURFACE_STYLE_USAGE ( .BOTH. , #46959 ) ;
#52214 = CIRCLE ( 'NONE', #21866, 5.500000000000001776 ) ;
#52215 = CARTESIAN_POINT ( 'NONE',  ( -118.8549999999999898, 4.716976649647094177, 6.492361379858945902 ) ) ;
#52216 = EDGE_CURVE ( 'NONE', #69517, #54457, #2181, .T. ) ;
#52217 = LINE ( 'NONE', #45571, #34743 ) ;
#52218 = CARTESIAN_POINT ( 'NONE',  ( 9.058813317711338797, 120.8449999999999847, -2.943386871421372675 ) ) ;
#52219 = CARTESIAN_POINT ( 'NONE',  ( -130.1950000000000216, 8.437984349512085203, -1.550032578732815448E-15 ) ) ;
#52220 = AXIS2_PLACEMENT_3D ( 'NONE', #64688, #27010, #31972 ) ;
#52221 = AXIS2_PLACEMENT_3D ( 'NONE', #59569, #32855, #11388 ) ;
#52222 = EDGE_CURVE ( 'NONE', #10363, #2682, #55059, .T. ) ;
#52223 = VERTEX_POINT ( 'NONE', #2929 ) ;
#52224 = SURFACE_STYLE_FILL_AREA ( #9296 ) ;
#52225 = DIRECTION ( 'NONE',  ( -1.000000000000000000, 0.000000000000000000, 0.000000000000000000 ) ) ;
#52226 = EDGE_CURVE ( 'NONE', #38982, #51395, #24732, .T. ) ;
#52227 = EDGE_LOOP ( 'NONE', ( #60097, #13890, #36073, #52196 ) ) ;
#52228 = DIRECTION ( 'NONE',  ( -1.000000000000000000, 0.000000000000000000, 0.000000000000000000 ) ) ;
#52229 = CARTESIAN_POINT ( 'NONE',  ( -172.4929263765338305, -8.102448949553172852, 5.886773742842742685 ) ) ;
#52230 = CARTESIAN_POINT ( 'NONE',  ( -181.1949999999999648, 8.437984349512085203, -1.550032578732815448E-15 ) ) ;
#52231 = EDGE_CURVE ( 'NONE', #30878, #65754, #18805, .T. ) ;
#52232 = AXIS2_PLACEMENT_3D ( 'NONE', #8283, #36054, #52249 ) ;
#52233 = DIRECTION ( 'NONE',  ( 0.000000000000000000, 0.000000000000000000, 1.000000000000000000 ) ) ;
#52234 = CIRCLE ( 'NONE', #40992, 5.000000000000000000 ) ;
#52235 = FACE_OUTER_BOUND ( 'NONE', #61727, .T. ) ;
#52236 = CARTESIAN_POINT ( 'NONE',  ( 0.000000000000000000, 136.0570736234661808, -8.025000000000000355 ) ) ;
#52237 = ORIENTED_EDGE ( 'NONE', *, *, #44874, .T. ) ;
#52238 = CARTESIAN_POINT ( 'NONE',  ( -86.09292637653378222, 3.094860106618433360, 9.524999999999991473 ) ) ;
#52239 = CONTEXT_DEPENDENT_SHAPE_REPRESENTATION ( #64848, #34496 ) ;
#52240 = AXIS2_PLACEMENT_3D ( 'NONE', #16008, #5063, #17041 ) ;
#52241 = CYLINDRICAL_SURFACE ( 'NONE', #56557, 0.5000000000000004441 ) ;
#52242 = CARTESIAN_POINT ( 'NONE',  ( -166.7929263765339840, -3.094860106614799378, 9.525000000002631140 ) ) ;
#52243 = CIRCLE ( 'NONE', #62355, 0.2500000000000002220 ) ;
#52244 = DIRECTION ( 'NONE',  ( -0.000000000000000000, 1.000000000000000000, -0.000000000000000000 ) ) ;
#52245 = CARTESIAN_POINT ( 'NONE',  ( 179.4361977533490347, 14.00000000000000000, 103.7004518695263044 ) ) ;
#52246 = PLANE ( 'NONE',  #6961 ) ;
#52247 = ORIENTED_EDGE ( 'NONE', *, *, #67147, .T. ) ;
#52248 = DIRECTION ( 'NONE',  ( 0.000000000000000000, 0.000000000000000000, 1.000000000000000000 ) ) ;
#52249 = DIRECTION ( 'NONE',  ( 0.000000000000000000, -1.000000000000000000, 0.000000000000000000 ) ) ;
#52250 = SURFACE_SIDE_STYLE ('',( #35704 ) ) ;
#52251 = VERTEX_POINT ( 'NONE', #24091 ) ;
#52252 = CARTESIAN_POINT ( 'NONE',  ( -110.9929263765338163, 8.102448949553172852, -5.886773742842744461 ) ) ;
#52253 = DIRECTION ( 'NONE',  ( 0.000000000000000000, 1.000000000000000000, -0.000000000000000000 ) ) ;
#52254 = CARTESIAN_POINT ( 'NONE',  ( 0.000000000000000000, 130.0570736234661524, -8.025000000000000355 ) ) ;
#52255 = PRESENTATION_LAYER_ASSIGNMENT (  '', '', ( #11798 ) ) ;
#52256 = VERTEX_POINT ( 'NONE', #45238 ) ;
#52257 = CARTESIAN_POINT ( 'NONE',  ( -30.38025804287905629, -8.499999999999996447, 0.06931351858032895608 ) ) ;
#52258 = CARTESIAN_POINT ( 'NONE',  ( -100.7049999999999699, 2.607480562269072433, 8.024999999999991473 ) ) ;
#52259 =( LENGTH_UNIT ( ) NAMED_UNIT ( * ) SI_UNIT ( .MILLI., .METRE. ) );
#52260 = ORIENTED_EDGE ( 'NONE', *, *, #18809, .T. ) ;
#52261 = CARTESIAN_POINT ( 'NONE',  ( -37.71575249473459479, -12.64783167710381129, 1.172152365681724095 ) ) ;
#52262 = CIRCLE ( 'NONE', #26362, 0.2500000000000002220 ) ;
#52263 = CARTESIAN_POINT ( 'NONE',  ( -104.6070736234661780, -8.102448949553174629, 5.886773742842742685 ) ) ;
#52264 =( LENGTH_UNIT ( ) NAMED_UNIT ( * ) SI_UNIT ( .MILLI., .METRE. ) );
#52265 = CARTESIAN_POINT ( 'NONE',  ( 29.00000000000000000, 34.80256050929376954, -80.00402776293826435 ) ) ;
#52266 =( GEOMETRIC_REPRESENTATION_CONTEXT ( 3 ) GLOBAL_UNCERTAINTY_ASSIGNED_CONTEXT ( ( #32040 ) ) GLOBAL_UNIT_ASSIGNED_CONTEXT ( ( #12933, #8005, #9060 ) ) REPRESENTATION_CONTEXT ( 'NONE', 'WORKASPACE' ) );
#52267 = ORIENTED_EDGE ( 'NONE', *, *, #68375, .T. ) ;
#52268 = PRESENTATION_LAYER_ASSIGNMENT (  '', '', ( #23028 ) ) ;
#52269 = CARTESIAN_POINT ( 'NONE',  ( 6.062177826491070398, 3.500000000000002665, 0.000000000000000000 ) ) ;
#52270 = CARTESIAN_POINT ( 'NONE',  ( -67.79499999999998749, 2.607480562269068880, -8.024999999999993250 ) ) ;
#52271 = VERTEX_POINT ( 'NONE', #8618 ) ;
#52272 = DIRECTION ( 'NONE',  ( -0.000000000000000000, -0.000000000000000000, -1.000000000000000000 ) ) ;
#52273 = DIRECTION ( 'NONE',  ( 0.000000000000000000, 1.000000000000000000, 0.000000000000000000 ) ) ;
#52274 = UNCERTAINTY_MEASURE_WITH_UNIT (LENGTH_MEASURE( 1.000000000000000082E-05 ), #4181, 'distance_accuracy_value', 'NONE');
#52275 = EDGE_LOOP ( 'NONE', ( #16011, #12970 ) ) ;
#52276 = CARTESIAN_POINT ( 'NONE',  ( 34.99999999999992895, 110.4999999999999858, 10.00000000000000000 ) ) ;
#52277 = CARTESIAN_POINT ( 'NONE',  ( -72.50000000000000000, 35.92875272052971525, 10.00000000000000000 ) ) ;
#52278 = CARTESIAN_POINT ( 'NONE',  ( -75.00000000000000000, -2.215169945516535778E-14, 6.500000000000000000 ) ) ;
#52279 = ORIENTED_EDGE ( 'NONE', *, *, #28091, .T. ) ;
#52280 = FACE_BOUND ( 'NONE', #38342, .T. ) ;
#52282 = ORIENTED_EDGE ( 'NONE', *, *, #44751, .F. ) ;
#52281 = EDGE_CURVE ( 'NONE', #35268, #246, #68391, .T. ) ;
#52283 = FILL_AREA_STYLE_COLOUR ( '', #903 ) ;
#52284 = DIRECTION ( 'NONE',  ( 1.000000000000000000, 1.073081856240828566E-16, 0.000000000000000000 ) ) ;
#52285 = CARTESIAN_POINT ( 'NONE',  ( 15.98999599679679839, 146.9999999999999716, 7.000000000000000000 ) ) ;
#52286 = CARTESIAN_POINT ( 'NONE',  ( -167.4570736234661865, -9.058813317711329915, 2.943386871421371787 ) ) ;
#52287 = CARTESIAN_POINT ( 'NONE',  ( 3.094860106618435136, 121.2949999999999733, -9.525000000000000355 ) ) ;
#52288 = EDGE_CURVE ( 'NONE', #26176, #49404, #35963, .T. ) ;
#52289 = CARTESIAN_POINT ( 'NONE',  ( -107.0070736234661837, -8.102448949553172852, -5.886773742842741797 ) ) ;
#52290 = ADVANCED_FACE ( 'NONE', ( #14579 ), #3998, .F. ) ;
#52291 = SURFACE_SIDE_STYLE ('',( #20598 ) ) ;
#52292 = COLOUR_RGB ( '', 0.40784314, 0.44705882, 0.49803922) ;
#52293 = DIRECTION ( 'NONE',  ( 0.000000000000000000, -1.000000000000000000, 0.000000000000000000 ) ) ;
#52294 = ORIENTED_EDGE ( 'NONE', *, *, #26170, .T. ) ;
#52295 = CYLINDRICAL_SURFACE ( 'NONE', #10457, 0.5000000000000004441 ) ;
#52296 = EDGE_CURVE ( 'NONE', #39801, #53553, #41000, .T. ) ;
#52297 = CARTESIAN_POINT ( 'NONE',  ( -82.34292637653379643, -9.058813317711329915, 2.943386871421371787 ) ) ;
#52298 = FACE_OUTER_BOUND ( 'NONE', #24414, .T. ) ;
#52299 = CARTESIAN_POINT ( 'NONE',  ( -147.8050000000000068, -8.437984349512085203, 5.166775262442717831E-16 ) ) ;
#52300 = EDGE_CURVE ( 'NONE', #68529, #55377, #2586, .T. ) ;
#52301 = DIRECTION ( 'NONE',  ( 0.000000000000000000, 0.000000000000000000, -1.000000000000000000 ) ) ;
#52302 = CARTESIAN_POINT ( 'NONE',  ( -4.877232780471185691, 110.9397655174076078, -7.675753971875499460 ) ) ;
#52303 = CARTESIAN_POINT ( 'NONE',  ( -156.2949999999999591, -2.607480562269069768, 8.024999999999991473 ) ) ;
#52304 = EDGE_CURVE ( 'NONE', #18998, #42152, #8616, .T. ) ;
#52305 = CARTESIAN_POINT ( 'NONE',  ( -151.1949999999999932, 8.437984349512086979, -1.550032578732815448E-15 ) ) ;
#52306 = ORIENTED_EDGE ( 'NONE', *, *, #61045, .F. ) ;
#52307 = COLOUR_RGB ( '', 0.66274510, 0.83137255, 0.94901961) ;
#52308 = CARTESIAN_POINT ( 'NONE',  ( -64.94292637653380496, 0.000000000000000000, 9.524999999999991473 ) ) ;
#52309 = AXIS2_PLACEMENT_3D ( 'NONE', #30520, #53052, #4846 ) ;
#52310 = EDGE_CURVE ( 'NONE', #6197, #33800, #38304, .T. ) ;
#52311 = UNCERTAINTY_MEASURE_WITH_UNIT (LENGTH_MEASURE( 1.000000000000000082E-05 ), #21671, 'distance_accuracy_value', 'NONE');
#52312 = CARTESIAN_POINT ( 'NONE',  ( -60.50499999999998124, -6.826472737025115478, -4.959722759717899443 ) ) ;
#52313 = CARTESIAN_POINT ( 'NONE',  ( -40.19857555756883016, -13.54303449714841534, 2.705192303963718015 ) ) ;
#52314 = VECTOR ( 'NONE', #40263, 1000.000000000000000 ) ;
#52315 = CARTESIAN_POINT ( 'NONE',  ( -60.89499999999998892, 6.826472737025115478, 4.959722759717899443 ) ) ;
#52316 = CARTESIAN_POINT ( 'NONE',  ( 8.102448949553181734, 154.5049999999999670, 5.886773742842750679 ) ) ;
#52317 = DIRECTION ( 'NONE',  ( 1.000000000000000000, 0.000000000000000000, 0.000000000000000000 ) ) ;
#52318 = AXIS2_PLACEMENT_3D ( 'NONE', #43739, #40426, #34433 ) ;
#52319 = DIRECTION ( 'NONE',  ( 0.000000000000000000, 0.000000000000000000, -1.000000000000000000 ) ) ;
#52320 = UNCERTAINTY_MEASURE_WITH_UNIT (LENGTH_MEASURE( 1.000000000000000082E-05 ), #40269, 'distance_accuracy_value', 'NONE');
#52321 = CARTESIAN_POINT ( 'NONE',  ( -153.1429263765338078, 5.598654528085800663, -7.705886871421367523 ) ) ;
#52322 = CARTESIAN_POINT ( 'NONE',  ( -5.512442546754645178, 110.6161587570711191, 7.633710229764736788 ) ) ;
#52323 = CARTESIAN_POINT ( 'NONE',  ( -177.4429263765338192, -1.166476076187852838E-15, -9.524999999999991473 ) ) ;
#52324 = CIRCLE ( 'NONE', #30950, 8.000000000000007105 ) ;
#52325 = LINE ( 'NONE', #25211, #32665 ) ;
#52326 = CIRCLE ( 'NONE', #55662, 0.2500000000000002220 ) ;
#52327 = CARTESIAN_POINT ( 'NONE',  ( -11.24540022918535698, 52.49282396394303873, -2.000000000000000000 ) ) ;
#52328 = ORIENTED_EDGE ( 'NONE', *, *, #68478, .F. ) ;
#52329 = VERTEX_POINT ( 'NONE', #11019 ) ;
#52330 = FILL_AREA_STYLE ('',( #4800 ) ) ;
#52332 = CYLINDRICAL_SURFACE ( 'NONE', #43978, 0.2500000000000002220 ) ;
#52331 = AXIS2_PLACEMENT_3D ( 'NONE', #24604, #30579, #61907 ) ;
#52333 = EDGE_CURVE ( 'NONE', #7256, #11976, #61835, .T. ) ;
#52334 = FACE_OUTER_BOUND ( 'NONE', #31493, .T. ) ;
#52335 = CARTESIAN_POINT ( 'NONE',  ( 7.794228634059945371, -2.500000000000000000, 4.500000000000000888 ) ) ;
#52336 = CARTESIAN_POINT ( 'NONE',  ( -77.60707362346613536, -8.102448949553174629, 5.886773742842742685 ) ) ;
#52337 = ORIENTED_EDGE ( 'NONE', *, *, #32910, .F. ) ;
#52338 = EDGE_LOOP ( 'NONE', ( #11562, #29754, #47739, #38471 ) ) ;
#52339 = DIRECTION ( 'NONE',  ( 0.000000000000000000, 0.000000000000000000, 1.000000000000000000 ) ) ;
#52340 = CARTESIAN_POINT ( 'NONE',  ( -195.0000000000000000, 0.000000000000000000, 9.524999999999991473 ) ) ;
#52341 = DIRECTION ( 'NONE',  ( -0.000000000000000000, -0.000000000000000000, -1.000000000000000000 ) ) ;
#52342 = VERTEX_POINT ( 'NONE', #42059 ) ;
#52343 = CARTESIAN_POINT ( 'NONE',  ( -5.598654528085808657, 114.7549999999999812, 7.705886871421373741 ) ) ;
#52344 = DIRECTION ( 'NONE',  ( -0.000000000000000000, -0.000000000000000000, 1.000000000000000000 ) ) ;
#52345 = CARTESIAN_POINT ( 'NONE',  ( 0.000000000000000000, 154.9999999999999716, 0.000000000000000000 ) ) ;
#52346 = CARTESIAN_POINT ( 'NONE',  ( -101.8449999999999847, -7.632228543268599452, 2.479861379858951054 ) ) ;
#52347 = ORIENTED_EDGE ( 'NONE', *, *, #27948, .T. ) ;
#52348 = CARTESIAN_POINT ( 'NONE',  ( 23.67688240327908389, 27.44010416289936316, -27.18999999999999062 ) ) ;
#52349 = CARTESIAN_POINT ( 'NONE',  ( 21.50000000000000711, 21.99999999999998224, 3.750000000000000000 ) ) ;
#52350 =( NAMED_UNIT ( * ) SI_UNIT ( $, .STERADIAN. ) SOLID_ANGLE_UNIT ( ) );
#52351 = CARTESIAN_POINT ( 'NONE',  ( -65.49999999999997158, -2.024042244987997205E-14, -12.00000000000000000 ) ) ;
#52352 = VERTEX_POINT ( 'NONE', #58185 ) ;
#52353 = CARTESIAN_POINT ( 'NONE',  ( 6.826472737025121695, 158.4929263765337737, -4.959722759717905660 ) ) ;
#52354 = COLOUR_RGB ( '', 0.72549020, 0.75294118, 0.79215686) ;
#52355 = PLANE ( 'NONE',  #15455 ) ;
#52356 = EDGE_CURVE ( 'NONE', #19997, #42076, #46183, .T. ) ;
#52357 = VERTEX_POINT ( 'NONE', #63110 ) ;
#52358 = CARTESIAN_POINT ( 'NONE',  ( 19.89974874213240597, 114.9999999999999574, -10.00000000000001421 ) ) ;
#52359 = ORIENTED_EDGE ( 'NONE', *, *, #59547, .T. ) ;
#52360 = CARTESIAN_POINT ( 'NONE',  ( 7.632228543268608334, 128.3429263765338249, -2.479861379858951942 ) ) ;
#52361 = AXIS2_PLACEMENT_3D ( 'NONE', #50089, #46219, #24701 ) ;
#52362 = COLOUR_RGB ( '', 0.08235294, 0.09019608, 0.10196078) ;
#52363 =( LENGTH_UNIT ( ) NAMED_UNIT ( * ) SI_UNIT ( .MILLI., .METRE. ) );
#52364 = CARTESIAN_POINT ( 'NONE',  ( -124.5549999999999926, 0.000000000000000000, 8.024999999999991473 ) ) ;
#52365 =( LENGTH_UNIT ( ) NAMED_UNIT ( * ) SI_UNIT ( .MILLI., .METRE. ) );
#52366 =( LENGTH_UNIT ( ) NAMED_UNIT ( * ) SI_UNIT ( .MILLI., .METRE. ) );
#52367 = FACE_OUTER_BOUND ( 'NONE', #30071, .T. ) ;
#52368 = ADVANCED_FACE ( 'NONE', ( #4709 ), #51, .F. ) ;
#52369 = CARTESIAN_POINT ( 'NONE',  ( 0.000000000000000000, 115.4999999999999574, 16.00000000000000000 ) ) ;
#52370 = CARTESIAN_POINT ( 'NONE',  ( -6.021969435454501252, 7.569642976165948056, 0.6362876910938565223 ) ) ;
#52371 = CARTESIAN_POINT ( 'NONE',  ( 3.999798566743335115, 8.867945265733711224, 11.56480034751363917 ) ) ;
#52372 = ORIENTED_EDGE ( 'NONE', *, *, #13188, .F. ) ;
#52373 = ORIENTED_EDGE ( 'NONE', *, *, #35314, .T. ) ;
#52374 = DIRECTION ( 'NONE',  ( 1.000000000000000000, 1.224646799147353454E-16, 0.000000000000000000 ) ) ;
#52375 = CARTESIAN_POINT ( 'NONE',  ( 44.99999999999998579, 119.9999999999999716, -7.500000000000000000 ) ) ;
#52376 = CARTESIAN_POINT ( 'NONE',  ( 57.24999999999999289, 28.24999999999998934, -3.750000000000000000 ) ) ;
#52377 = DIRECTION ( 'NONE',  ( -1.000000000000000000, -4.336808689941999001E-16, 0.000000000000000000 ) ) ;
#52379 = ORIENTED_EDGE ( 'NONE', *, *, #57297, .T. ) ;
#52378 = CIRCLE ( 'NONE', #11924, 4.999999999999997335 ) ;
#52380 = CARTESIAN_POINT ( 'NONE',  ( -153.8929263765338078, -8.102448949553174629, -5.886773742842741797 ) ) ;
#52381 = CARTESIAN_POINT ( 'NONE',  ( -174.3549999999999898, -4.716976649647093289, -6.492361379858945902 ) ) ;
#52382 = CARTESIAN_POINT ( 'NONE',  ( 69.99999999999998579, 37.00000000000000000, 3.750000000000000000 ) ) ;
#52383 = FACE_OUTER_BOUND ( 'NONE', #68632, .T. ) ;
#52384 = CARTESIAN_POINT ( 'NONE',  ( -46.85707362346616378, -5.598654528085803328, -7.705886871421366635 ) ) ;
#52385 = ADVANCED_FACE ( 'NONE', ( #68393 ), #19159, .T. ) ;
#52386 =( GEOMETRIC_REPRESENTATION_CONTEXT ( 3 ) GLOBAL_UNCERTAINTY_ASSIGNED_CONTEXT ( ( #9346 ) ) GLOBAL_UNIT_ASSIGNED_CONTEXT ( ( #18697, #61570, #24305 ) ) REPRESENTATION_CONTEXT ( 'NONE', 'WORKASPACE' ) );
#52387 = CARTESIAN_POINT ( 'NONE',  ( -174.1449999999999818, -4.716976649647092401, 6.492361379858946790 ) ) ;
#52388 = CIRCLE ( 'NONE', #36649, 0.2500000000000002220 ) ;
#52389 = ORIENTED_EDGE ( 'NONE', *, *, #63228, .F. ) ;
#52390 = DIRECTION ( 'NONE',  ( 0.000000000000000000, 0.000000000000000000, 1.000000000000000000 ) ) ;
#52391 = DIRECTION ( 'NONE',  ( 0.000000000000000000, 0.000000000000000000, -1.000000000000000000 ) ) ;
#52392 = ADVANCED_FACE ( 'NONE', ( #20187 ), #55111, .T. ) ;
#52393 = CARTESIAN_POINT ( 'NONE',  ( -10.66860548474816639, 11.73595285652921305, -2.518653182310350402 ) ) ;
#52394 = CARTESIAN_POINT ( 'NONE',  ( -89.45499999999999829, 7.632228543268599452, -2.479861379858951942 ) ) ;
#52395 = SURFACE_SIDE_STYLE ('',( #4492 ) ) ;
#52396 = PRESENTATION_STYLE_ASSIGNMENT (( #9821 ) ) ;
#52397 = CARTESIAN_POINT ( 'NONE',  ( -91.34499999999998465, 7.632228543268599452, -2.479861379858951942 ) ) ;
#52398 = CARTESIAN_POINT ( 'NONE',  ( -3.094860106618434248, 126.9049999999999869, 9.525000000000000355 ) ) ;
#52399 = CARTESIAN_POINT ( 'NONE',  ( -69.44499999999999318, 0.000000000000000000, 8.024999999999991473 ) ) ;
#52400 = DIRECTION ( 'NONE',  ( -0.000000000000000000, 1.000000000000000000, -0.000000000000000000 ) ) ;
#52401 = FILL_AREA_STYLE_COLOUR ( '', #18007 ) ;
#52402 = DIRECTION ( 'NONE',  ( -1.000000000000000000, 0.000000000000000000, 0.000000000000000000 ) ) ;
#52403 = UNCERTAINTY_MEASURE_WITH_UNIT (LENGTH_MEASURE( 1.000000000000000082E-05 ), #26838, 'distance_accuracy_value', 'NONE');
#52404 = DIRECTION ( 'NONE',  ( -0.000000000000000000, 0.000000000000000000, 1.000000000000000000 ) ) ;
#52405 = AXIS2_PLACEMENT_3D ( 'NONE', #36513, #2039, #34126 ) ;
#52406 = EDGE_LOOP ( 'NONE', ( #32135, #44061, #48848, #60337, #38374 ) ) ;
#52407 = CARTESIAN_POINT ( 'NONE',  ( -100.9429263765338050, 0.000000000000000000, 9.524999999999991473 ) ) ;
#52408 = PRODUCT ( '14. Nut M6', '14. Nut M6', '', ( #23386 ) ) ;
#52409 = CARTESIAN_POINT ( 'NONE',  ( -126.8949999999999818, 6.826472737025116366, 4.959722759717898555 ) ) ;
#52410 =( NAMED_UNIT ( * ) PLANE_ANGLE_UNIT ( ) SI_UNIT ( $, .RADIAN. ) );
#52411 = AXIS2_PLACEMENT_3D ( 'NONE', #14011, #61821, #13653 ) ;
#52412 = SURFACE_SIDE_STYLE ('',( #21395 ) ) ;
#52413 = AXIS2_PLACEMENT_3D ( 'NONE', #22047, #21005, #5844 ) ;
#52415 = SURFACE_SIDE_STYLE ('',( #3090 ) ) ;
#52414 = CARTESIAN_POINT ( 'NONE',  ( 2.607480562268992941, 135.9070736234661751, -8.025000000000060751 ) ) ;
#52416 = CARTESIAN_POINT ( 'NONE',  ( 98.00000000000000000, 14.00000000000000000, 0.000000000000000000 ) ) ;
#52417 = VERTEX_POINT ( 'NONE', #43454 ) ;
#52418 = ORIENTED_EDGE ( 'NONE', *, *, #10508, .T. ) ;
#52419 = CARTESIAN_POINT ( 'NONE',  ( -175.1070736234661638, 8.102448949553172852, -5.886773742842744461 ) ) ;
#52420 = EDGE_CURVE ( 'NONE', #20391, #56887, #56219, .T. ) ;
#52421 = DIRECTION ( 'NONE',  ( 0.000000000000000000, 0.000000000000000000, 1.000000000000000000 ) ) ;
#52422 =( NAMED_UNIT ( * ) PLANE_ANGLE_UNIT ( ) SI_UNIT ( $, .RADIAN. ) );
#52423 = ORIENTED_EDGE ( 'NONE', *, *, #56530, .T. ) ;
#52424 = CARTESIAN_POINT ( 'NONE',  ( -118.1049999999999898, -6.826472737025113702, 4.959722759717902107 ) ) ;
#52425 = VERTEX_POINT ( 'NONE', #48712 ) ;
#52426 = SURFACE_STYLE_FILL_AREA ( #25645 ) ;
#52427 = CIRCLE ( 'NONE', #6343, 0.5000000000000004441 ) ;
#52428 = CARTESIAN_POINT ( 'NONE',  ( -122.6070736234661780, -8.102448949553172852, 5.886773742842742685 ) ) ;
#52429 = VERTEX_POINT ( 'NONE', #7138 ) ;
#52430 = DIRECTION ( 'NONE',  ( 0.000000000000000000, 0.000000000000000000, 1.000000000000000000 ) ) ;
#52431 = DIRECTION ( 'NONE',  ( 0.000000000000000000, 0.000000000000000000, 1.000000000000000000 ) ) ;
#52432 = ORIENTED_EDGE ( 'NONE', *, *, #67061, .F. ) ;
#52433 = SURFACE_STYLE_FILL_AREA ( #30937 ) ;
#52434 = CARTESIAN_POINT ( 'NONE',  ( -8.102448949553181734, 145.8949999999999534, -5.886773742842749790 ) ) ;
#52435 = PRODUCT_DEFINITION ( 'UNKNOWN', '', #1144, #37556 ) ;
#52436 = EDGE_LOOP ( 'NONE', ( #31723, #9933, #11101 ) ) ;
#52437 = ADVANCED_FACE ( 'NONE', ( #22980 ), #6093, .F. ) ;
#52438 = CARTESIAN_POINT ( 'NONE',  ( -5.196152422706633800, -9.000000000000005329, 7.500000000000000000 ) ) ;
#52439 = CARTESIAN_POINT ( 'NONE',  ( -8.102448949553179958, 150.6049999999999898, 5.886773742842747126 ) ) ;
#52440 = DIRECTION ( 'NONE',  ( 1.000000000000000000, 0.000000000000000000, 0.000000000000000000 ) ) ;
#52441 = DIRECTION ( 'NONE',  ( 0.000000000000000000, 1.000000000000000000, 0.000000000000000000 ) ) ;
#52442 = ORIENTED_EDGE ( 'NONE', *, *, #1046, .F. ) ;
#52443 = CARTESIAN_POINT ( 'NONE',  ( -6.826472737025120807, 126.9929263765338163, 4.959722759717906548 ) ) ;
#52444 = DIRECTION ( 'NONE',  ( -0.000000000000000000, 1.000000000000000000, -0.000000000000000000 ) ) ;
#52445 = UNCERTAINTY_MEASURE_WITH_UNIT (LENGTH_MEASURE( 1.000000000000000082E-05 ), #68711, 'distance_accuracy_value', 'NONE');
#52446 = DIRECTION ( 'NONE',  ( -1.000000000000000000, 0.000000000000000000, 0.000000000000000000 ) ) ;
#52447 = ADVANCED_FACE ( 'NONE', ( #12054 ), #27176, .T. ) ;
#52448 = DIRECTION ( 'NONE',  ( 1.000000000000000000, 0.000000000000000000, -1.300977106640434891E-16 ) ) ;
#52449 = FILL_AREA_STYLE ('',( #9869 ) ) ;
#52450 = ADVANCED_FACE ( 'NONE', ( #39179 ), #34895, .T. ) ;
#52451 = ORIENTED_EDGE ( 'NONE', *, *, #33898, .T. ) ;
#52452 = CARTESIAN_POINT ( 'NONE',  ( 41.25890975875731215, 107.3519676386824813, 3.442113426143906807 ) ) ;
#52453 = EDGE_LOOP ( 'NONE', ( #24283, #20944, #1426, #15991 ) ) ;
#52454 = CARTESIAN_POINT ( 'NONE',  ( -59.09292637653378222, 3.094860106618433360, 9.524999999999991473 ) ) ;
#52455 = DIRECTION ( 'NONE',  ( 0.000000000000000000, 0.000000000000000000, 1.000000000000000000 ) ) ;
#52456 = CARTESIAN_POINT ( 'NONE',  ( -154.7049999999999841, 2.607480562269073321, 8.024999999999991473 ) ) ;
#52457 = ORIENTED_EDGE ( 'NONE', *, *, #17978, .T. ) ;
#52458 = UNCERTAINTY_MEASURE_WITH_UNIT (LENGTH_MEASURE( 1.000000000000000082E-05 ), #27915, 'distance_accuracy_value', 'NONE');
#52459 = EDGE_CURVE ( 'NONE', #68594, #50928, #51782, .T. ) ;
#52460 = DIRECTION ( 'NONE',  ( -0.000000000000000000, -0.000000000000000000, -1.000000000000000000 ) ) ;
#52461 = CARTESIAN_POINT ( 'NONE',  ( -55.81907424270178808, -8.628515624790351168, 6.048998428371599623 ) ) ;
#52462 = CARTESIAN_POINT ( 'NONE',  ( -70.79292637653379927, -3.094860106618429807, 9.524999999999991473 ) ) ;
#52463 = DIRECTION ( 'NONE',  ( -1.000000000000000000, -0.000000000000000000, -0.000000000000000000 ) ) ;
#52464 = ORIENTED_EDGE ( 'NONE', *, *, #1933, .F. ) ;
#52466 = EDGE_CURVE ( 'NONE', #4737, #49912, #22627, .T. ) ;
#52465 = ORIENTED_EDGE ( 'NONE', *, *, #18041, .T. ) ;
#52467 = CARTESIAN_POINT ( 'NONE',  ( 22.70708736557406482, 27.11529135480144248, 27.31808320068521923 ) ) ;
#52468 = MECHANICAL_DESIGN_GEOMETRIC_PRESENTATION_REPRESENTATION (  '', ( #50181 ), #4087 ) ;
#52469 = CARTESIAN_POINT ( 'NONE',  ( -71.00499999999996703, 6.826472737025116366, 4.959722759717898555 ) ) ;
#52470 = VERTEX_POINT ( 'NONE', #28205 ) ;
#52472 = VECTOR ( 'NONE', #55626, 1000.000000000000000 ) ;
#52471 = CARTESIAN_POINT ( 'NONE',  ( 22.00000000000002132, 50.00000000000000000, 60.00000000000000711 ) ) ;
#52474 = EDGE_CURVE ( 'NONE', #37003, #66069, #38510, .T. ) ;
#52473 = VECTOR ( 'NONE', #65645, 1000.000000000000000 ) ;
#52475 = CARTESIAN_POINT ( 'NONE',  ( -60.00000000000000000, -2.024042244987997205E-14, -7.500000000000000000 ) ) ;
#52476 = DIRECTION ( 'NONE',  ( 1.000000000000000000, -0.000000000000000000, 0.000000000000000000 ) ) ;
#52477 = VERTEX_POINT ( 'NONE', #49367 ) ;
#52478 = DIRECTION ( 'NONE',  ( -0.000000000000000000, -1.000000000000000000, -0.000000000000000000 ) ) ;
#52479 = EDGE_CURVE ( 'NONE', #50347, #58968, #60576, .T. ) ;
#52480 = DIRECTION ( 'NONE',  ( -1.000000000000000000, -0.000000000000000000, -0.000000000000000000 ) ) ;
#52482 = DIRECTION ( 'NONE',  ( -1.000000000000000000, 0.000000000000000000, 0.000000000000000000 ) ) ;
#52481 =( BOUNDED_CURVE ( )  B_SPLINE_CURVE ( 2, ( #56007, #35262, #8188, #34555, #51798, #34220, #18728, #55674, #7823, #29637, #7486 ),
 .UNSPECIFIED., .F., .F. ) 
 B_SPLINE_CURVE_WITH_KNOTS ( ( 3, 2, 2, 2, 2, 3 ),
 ( 0.6470588235294115753, 0.6529411764705880250, 0.6588235294117644747, 0.6647058823529409244, 0.6705882352941173741, 0.6764705882352939348 ),
 .UNSPECIFIED. ) 
 CURVE ( )  GEOMETRIC_REPRESENTATION_ITEM ( )  RATIONAL_B_SPLINE_CURVE ( ( 1.000000000000001776, 0.9510565162951516438, 1.000000000000000000, 0.9510565162951535312, 1.000000000000000000, 0.9510565162951535312, 1.000000000000000000, 0.9510565162951535312, 1.000000000000000000, 0.9510565162951554186, 0.9999999999999981126 ) ) 
 REPRESENTATION_ITEM ( '' )  );
#52484 = CARTESIAN_POINT ( 'NONE',  ( 66.24999999999998579, 33.74999999999999289, 3.750000000000000000 ) ) ;
#52483 = DIRECTION ( 'NONE',  ( 0.7071067811865472397, 0.000000000000000000, -0.7071067811865477948 ) ) ;
#52485 = STYLED_ITEM ( 'NONE', ( #37417 ), #40490 ) ;
#52486 = CARTESIAN_POINT ( 'NONE',  ( 8.102448949553181734, 147.3950000000000102, 5.886773742842750679 ) ) ;
#52487 = CARTESIAN_POINT ( 'NONE',  ( -101.3949999999999676, -6.826472737025115478, -4.959722759717899443 ) ) ;
#52488 = LINE ( 'NONE', #58773, #4962 ) ;
#52489 = CARTESIAN_POINT ( 'NONE',  ( 20.71231517720798010, 149.9999999999999716, -10.00000000000000000 ) ) ;
#52490 = UNCERTAINTY_MEASURE_WITH_UNIT (LENGTH_MEASURE( 1.000000000000000082E-05 ), #61780, 'distance_accuracy_value', 'NONE');
#52491 = DIRECTION ( 'NONE',  ( -0.000000000000000000, -0.000000000000000000, -1.000000000000000000 ) ) ;
#52492 = CIRCLE ( 'NONE', #33994, 0.2500000000000002220 ) ;
#52493 = ORIENTED_EDGE ( 'NONE', *, *, #68539, .T. ) ;
#52494 = CARTESIAN_POINT ( 'NONE',  ( -134.2429263765338305, 5.598654528085804216, 7.705886871421366635 ) ) ;
#52495 = FACE_OUTER_BOUND ( 'NONE', #57319, .T. ) ;
#52496 = CARTESIAN_POINT ( 'NONE',  ( -152.8449999999999989, -7.632228543268599452, 2.479861379858951054 ) ) ;
#52497 =( LENGTH_UNIT ( ) NAMED_UNIT ( * ) SI_UNIT ( .MILLI., .METRE. ) );
#52498 = CARTESIAN_POINT ( 'NONE',  ( -132.4429263765338192, -1.166476076187852838E-15, -9.524999999999991473 ) ) ;
#52499 = ORIENTED_EDGE ( 'NONE', *, *, #9476, .F. ) ;
#52500 = EDGE_LOOP ( 'NONE', ( #17671, #62096, #59486, #7236 ) ) ;
#52501 = CARTESIAN_POINT ( 'NONE',  ( 109.0067032876572171, 14.00000000000000000, 19.20378738324562917 ) ) ;
#52502 = DIRECTION ( 'NONE',  ( 0.000000000000000000, -1.000000000000000000, 0.000000000000000000 ) ) ;
#52503 = CARTESIAN_POINT ( 'NONE',  ( -45.00000000000000000, 8.545765431912348831, 5.556277950132127330 ) ) ;
#52504 = CARTESIAN_POINT ( 'NONE',  ( -110.6070736234661638, -8.102448949553174629, 5.886773742842742685 ) ) ;
#52505 = DIRECTION ( 'NONE',  ( 0.000000000000000000, 0.000000000000000000, 1.000000000000000000 ) ) ;
#52506 = CIRCLE ( 'NONE', #4142, 0.5000000000000004441 ) ;
#52507 = ORIENTED_EDGE ( 'NONE', *, *, #21290, .F. ) ;
#52508 = CARTESIAN_POINT ( 'NONE',  ( -149.1549999999999727, 7.632228543268600340, 2.479861379858949277 ) ) ;
#52509 = ORIENTED_EDGE ( 'NONE', *, *, #68734, .F. ) ;
#52510 = CARTESIAN_POINT ( 'NONE',  ( 5.356721384544675502, 4.721886399977926807, 0.1324414877861175011 ) ) ;
#52511 = FILL_AREA_STYLE ('',( #9601 ) ) ;
#52512 = ORIENTED_EDGE ( 'NONE', *, *, #45166, .F. ) ;
#52513 = DIRECTION ( 'NONE',  ( 0.000000000000000000, -1.000000000000000000, 1.734723475976805615E-16 ) ) ;
#52514 = CARTESIAN_POINT ( 'NONE',  ( -58.40707362346616094, 3.094860106618428031, -9.524999999999993250 ) ) ;
#52515 = CARTESIAN_POINT ( 'NONE',  ( -9.058813317711337021, 125.0449999999999875, -2.943386871421374895 ) ) ;
#52516 = VERTEX_POINT ( 'NONE', #49712 ) ;
#52517 = EDGE_CURVE ( 'NONE', #40740, #15615, #44478, .T. ) ;
#52518 = PRESENTATION_STYLE_ASSIGNMENT (( #9251 ) ) ;
#52519 = CARTESIAN_POINT ( 'NONE',  ( -9.058813317711337021, 120.1549999999999869, -2.943386871421374895 ) ) ;
#52520 = CARTESIAN_POINT ( 'NONE',  ( -68.30499999999999261, 8.437984349512086979, -1.550032578732815448E-15 ) ) ;
#52521 = CARTESIAN_POINT ( 'NONE',  ( 71.74137931034481142, 36.89918356738973415, 9.500000000000000000 ) ) ;
#52522 = EDGE_LOOP ( 'NONE', ( #16606, #55678, #10275, #6278 ) ) ;
#52523 = CARTESIAN_POINT ( 'NONE',  ( -8.102448949553181734, 138.0049999999999670, -5.886773742842749790 ) ) ;
#52524 = UNCERTAINTY_MEASURE_WITH_UNIT (LENGTH_MEASURE( 1.000000000000000082E-05 ), #29775, 'distance_accuracy_value', 'NONE');
#52525 = ADVANCED_FACE ( 'NONE', ( #62659 ), #29265, .F. ) ;
#52526 = CARTESIAN_POINT ( 'NONE',  ( 3.499999999999999112, 33.74999999999998579, -3.750000000000000000 ) ) ;
#52527 = AXIS2_PLACEMENT_3D ( 'NONE', #60437, #12244, #1976 ) ;
#52528 = ADVANCED_FACE ( 'NONE', ( #41262 ), #13438, .T. ) ;
#52529 = CARTESIAN_POINT ( 'NONE',  ( 7.249999999999999112, 9.031770143711729009E-16, 1.000000000000000000 ) ) ;
#52530 = ORIENTED_EDGE ( 'NONE', *, *, #24839, .T. ) ;
#52531 = DIRECTION ( 'NONE',  ( 0.000000000000000000, -1.000000000000000000, 0.000000000000000000 ) ) ;
#52532 = DIRECTION ( 'NONE',  ( 7.080503983578803083E-17, 1.000000000000000000, 0.000000000000000000 ) ) ;
#52533 = CYLINDRICAL_SURFACE ( 'NONE', #40660, 0.2500000000000002220 ) ;
#52534 = CARTESIAN_POINT ( 'NONE',  ( -181.8549999999999898, 4.716976649647094177, 6.492361379858945902 ) ) ;
#52535 = VERTEX_POINT ( 'NONE', #23650 ) ;
#52536 = CARTESIAN_POINT ( 'NONE',  ( 7.789749869348521649, 111.5987935625219052, -3.257487185497865312 ) ) ;
#52537 = CARTESIAN_POINT ( 'NONE',  ( 41.49999999999998579, 106.9282032302754999, -4.000000000000000000 ) ) ;
#52538 =( NAMED_UNIT ( * ) PLANE_ANGLE_UNIT ( ) SI_UNIT ( $, .RADIAN. ) );
#52539 = VERTEX_POINT ( 'NONE', #7819 ) ;
#52540 = DIRECTION ( 'NONE',  ( 0.000000000000000000, 0.000000000000000000, -1.000000000000000000 ) ) ;
#52541 = CARTESIAN_POINT ( 'NONE',  ( 48.74999999999999289, 24.74999999999998579, -4.000000000000000000 ) ) ;
#52542 = ORIENTED_EDGE ( 'NONE', *, *, #44406, .T. ) ;
#52543 = EDGE_CURVE ( 'NONE', #9166, #50552, #3180, .T. ) ;
#52544 = DIRECTION ( 'NONE',  ( 0.000000000000000000, 0.000000000000000000, 1.000000000000000000 ) ) ;
#52545 = CARTESIAN_POINT ( 'NONE',  ( -95.45499999999998408, 7.632228543268599452, -2.479861379858951942 ) ) ;
#52546 = VERTEX_POINT ( 'NONE', #45834 ) ;
#52547 = FILL_AREA_STYLE ('',( #15273 ) ) ;
#52548 = CARTESIAN_POINT ( 'NONE',  ( -15.98999599679679839, 146.9999999999999716, 7.500000000000000000 ) ) ;
#52549 = CARTESIAN_POINT ( 'NONE',  ( -133.4070736234661751, 3.094860106618428031, -9.524999999999993250 ) ) ;
#52550 = SURFACE_STYLE_USAGE ( .BOTH. , #57098 ) ;
#52551 = CARTESIAN_POINT ( 'NONE',  ( 5.598654528085809545, 148.1450000000000102, -7.705886871421373741 ) ) ;
#52552 = CARTESIAN_POINT ( 'NONE',  ( -77.60707362346613536, -8.102448949553172852, 5.886773742842742685 ) ) ;
#52553 = EDGE_LOOP ( 'NONE', ( #65896, #67284, #68649, #22681 ) ) ;
#52554 = CARTESIAN_POINT ( 'NONE',  ( 75.00000000000000000, -2.215169945516535778E-14, 6.999999999999999112 ) ) ;
#52555 = CARTESIAN_POINT ( 'NONE',  ( 0.000000000000000000, 0.000000000000000000, 0.000000000000000000 ) ) ;
#52556 = AXIS2_PLACEMENT_3D ( 'NONE', #39724, #6620, #50260 ) ;
#52558 = DIRECTION ( 'NONE',  ( 0.000000000000000000, 0.000000000000000000, -1.000000000000000000 ) ) ;
#52557 =( NAMED_UNIT ( * ) PLANE_ANGLE_UNIT ( ) SI_UNIT ( $, .RADIAN. ) );
#52559 = CIRCLE ( 'NONE', #27785, 5.000000000000000000 ) ;
#52560 = CARTESIAN_POINT ( 'NONE',  ( -107.1549999999999869, 7.632228543268600340, 2.479861379858949277 ) ) ;
#52562 = EDGE_CURVE ( 'NONE', #51718, #18409, #30291, .T. ) ;
#52561 = CARTESIAN_POINT ( 'NONE',  ( 48.25000000000000000, 21.99999999999998579, -4.000000000000000000 ) ) ;
#52563 = CARTESIAN_POINT ( 'NONE',  ( -3.094860106618432471, 124.5949999999999704, -9.525000000000000355 ) ) ;
#52564 = CARTESIAN_POINT ( 'NONE',  ( -125.0949999999999847, -2.607480562269071545, -8.024999999999991473 ) ) ;
#52565 = CARTESIAN_POINT ( 'NONE',  ( -60.99999999999998579, 50.00000000000000000, 7.500000000000000000 ) ) ;
#52566 = ADVANCED_FACE ( 'NONE', ( #56721 ), #18725, .F. ) ;
#52567 = FACE_OUTER_BOUND ( 'NONE', #15341, .T. ) ;
#52568 = CARTESIAN_POINT ( 'NONE',  ( -118.3429263765338106, -9.058813317711329915, 2.943386871421371787 ) ) ;
#52569 = ORIENTED_EDGE ( 'NONE', *, *, #39881, .T. ) ;
#52570 = CARTESIAN_POINT ( 'NONE',  ( -159.4429263765338192, -1.166476076187852838E-15, -9.524999999999991473 ) ) ;
#52571 = SURFACE_STYLE_FILL_AREA ( #9992 ) ;
#52572 = SURFACE_SIDE_STYLE ('',( #19837 ) ) ;
#52573 = VECTOR ( 'NONE', #43165, 999.9999999999998863 ) ;
#52574 = DIRECTION ( 'NONE',  ( 1.000000000000000000, 0.000000000000000000, 0.000000000000000000 ) ) ;
#52575 = DIRECTION ( 'NONE',  ( 0.000000000000000000, 0.000000000000000000, 1.000000000000000000 ) ) ;
#52576 = CARTESIAN_POINT ( 'NONE',  ( -83.49999999999998579, 4.336808689942018722E-16, -0.000000000000000000 ) ) ;
#52577 = CARTESIAN_POINT ( 'NONE',  ( -48.50000000000000000, 13.41640786499872284, -7.500000000000000000 ) ) ;
#52578 = EDGE_LOOP ( 'NONE', ( #64192, #34545, #44643, #43198 ) ) ;
#52579 = CARTESIAN_POINT ( 'NONE',  ( -87.14292637653379359, 5.598654528085800663, -7.705886871421367523 ) ) ;
#52580 = CONTEXT_DEPENDENT_SHAPE_REPRESENTATION ( #19021, #23257 ) ;
#52581 = CARTESIAN_POINT ( 'NONE',  ( -195.0000000000000000, 0.000000000000000000, 9.524999999999991473 ) ) ;
#52582 = CARTESIAN_POINT ( 'NONE',  ( 21.50000000000000711, 22.24999999999998224, -4.000000000000000000 ) ) ;
#52583 = CYLINDRICAL_SURFACE ( 'NONE', #15, 3.000000000000000444 ) ;
#52584 =( LENGTH_UNIT ( ) NAMED_UNIT ( * ) SI_UNIT ( .MILLI., .METRE. ) );
#52585 = CARTESIAN_POINT ( 'NONE',  ( -175.8549999999999898, 4.716976649647094177, 6.492361379858945902 ) ) ;
#52586 = ORIENTED_EDGE ( 'NONE', *, *, #30975, .F. ) ;
#52587 = DIRECTION ( 'NONE',  ( 0.000000000000000000, 1.000000000000000000, -0.000000000000000000 ) ) ;
#52589 = EDGE_CURVE ( 'NONE', #24627, #48545, #13110, .T. ) ;
#52588 = DIRECTION ( 'NONE',  ( -1.000000000000000000, 0.000000000000000000, 0.000000000000000000 ) ) ;
#52590 =( NAMED_UNIT ( * ) PLANE_ANGLE_UNIT ( ) SI_UNIT ( $, .RADIAN. ) );
#52591 = EDGE_LOOP ( 'NONE', ( #56474, #49436, #17199, #31053 ) ) ;
#52592 = CARTESIAN_POINT ( 'NONE',  ( 5.603568002170370654, -1.515110734050476804, 8.294335516573690725 ) ) ;
#52593 =( NAMED_UNIT ( * ) PLANE_ANGLE_UNIT ( ) SI_UNIT ( $, .RADIAN. ) );
#52594 = CARTESIAN_POINT ( 'NONE',  ( 4.716976649647099507, 144.7570736234661410, -6.492361379858953008 ) ) ;
#52595 =( BOUNDED_CURVE ( )  B_SPLINE_CURVE ( 3, ( #40334, #24137, #50193, #2262 ),
 .UNSPECIFIED., .F., .F. ) 
 B_SPLINE_CURVE_WITH_KNOTS ( ( 4, 4 ),
 ( 3.141592653589793116, 4.712388980384689674 ),
 .UNSPECIFIED. ) 
 CURVE ( )  GEOMETRIC_REPRESENTATION_ITEM ( )  RATIONAL_B_SPLINE_CURVE ( ( 1.000000000000000000, 0.8047378541243649375, 0.8047378541243649375, 1.000000000000000000 ) ) 
 REPRESENTATION_ITEM ( '' )  );
#52596 = EDGE_LOOP ( 'NONE', ( #8985, #58182 ) ) ;
#52597 = CIRCLE ( 'NONE', #57040, 2.500000000000002220 ) ;
#52598 = DIRECTION ( 'NONE',  ( 0.000000000000000000, 0.000000000000000000, -1.000000000000000000 ) ) ;
#52599 = CARTESIAN_POINT ( 'NONE',  ( -101.0049999999999812, 6.826472737025115478, 4.959722759717899443 ) ) ;
#52600 = UNCERTAINTY_MEASURE_WITH_UNIT (LENGTH_MEASURE( 1.000000000000000082E-05 ), #22081, 'distance_accuracy_value', 'NONE');
#52601 = FILL_AREA_STYLE ('',( #36452 ) ) ;
#52602 = VERTEX_POINT ( 'NONE', #10270 ) ;
#52603 = MECHANICAL_DESIGN_GEOMETRIC_PRESENTATION_REPRESENTATION (  '', ( #5359 ), #47001 ) ;
#52604 = CARTESIAN_POINT ( 'NONE',  ( -23.71231517720798010, 117.4999999999999716, -7.500000000000000000 ) ) ;
#52605 = EDGE_CURVE ( 'NONE', #50571, #59291, #63856, .T. ) ;
#52606 = DIRECTION ( 'NONE',  ( 0.000000000000000000, 0.000000000000000000, -1.000000000000000000 ) ) ;
#52607 = CARTESIAN_POINT ( 'NONE',  ( -32.95000823261079859, -9.007918291183415249, 4.145374715402367904 ) ) ;
#52608 = VERTEX_POINT ( 'NONE', #57406 ) ;
#52609 = CARTESIAN_POINT ( 'NONE',  ( -4.041451884327381450, -7.000000000000002665, 1.082903768654759791 ) ) ;
#52610 = CARTESIAN_POINT ( 'NONE',  ( -71.09499999999999886, -2.607480562269071545, -8.024999999999991473 ) ) ;
#52611 = ORIENTED_EDGE ( 'NONE', *, *, #22161, .F. ) ;
#52612 = CARTESIAN_POINT ( 'NONE',  ( 44.99999999999977973, 149.9999999999999716, 9.500000000000000000 ) ) ;
#52613 = DIRECTION ( 'NONE',  ( -1.000000000000000000, 0.000000000000000000, 0.000000000000000000 ) ) ;
#52614 = VERTEX_POINT ( 'NONE', #64056 ) ;
#52615 = DIRECTION ( 'NONE',  ( -1.000000000000000000, 0.000000000000000000, 0.000000000000000000 ) ) ;
#52616 = SURFACE_STYLE_FILL_AREA ( #9707 ) ;
#52617 = VECTOR ( 'NONE', #6412, 1000.000000000000000 ) ;
#52618 = EDGE_CURVE ( 'NONE', #67222, #7479, #41601, .T. ) ;
#52619 = CARTESIAN_POINT ( 'NONE',  ( 8.000000000000030198, 0.000000000000000000, -32.00402776293825013 ) ) ;
#52620 = ORIENTED_EDGE ( 'NONE', *, *, #30377, .F. ) ;
#52621 = FILL_AREA_STYLE ('',( #26544 ) ) ;
#52622 = EDGE_LOOP ( 'NONE', ( #31531, #25328 ) ) ;
#52623 = DIRECTION ( 'NONE',  ( 1.224646799147353207E-16, 1.000000000000000000, -0.000000000000000000 ) ) ;
#52624 = FILL_AREA_STYLE_COLOUR ( '', #68998 ) ;
#52625 = DIRECTION ( 'NONE',  ( 0.000000000000000000, 0.000000000000000000, 1.000000000000000000 ) ) ;
#52626 = CARTESIAN_POINT ( 'NONE',  ( -164.0070736234661695, -8.102448949553172852, -5.886773742842741797 ) ) ;
#52627 = CARTESIAN_POINT ( 'NONE',  ( 8.102448949553179958, 123.3949999999999818, 5.886773742842750679 ) ) ;
#52628 = CARTESIAN_POINT ( 'NONE',  ( -102.8070736234661666, 10.01517768586948698, -1.839758294383808571E-15 ) ) ;
#52629 =( LENGTH_UNIT ( ) NAMED_UNIT ( * ) SI_UNIT ( .MILLI., .METRE. ) );
#52630 = CARTESIAN_POINT ( 'NONE',  ( -65.00707362346616947, -8.102448949553174629, -5.886773742842741797 ) ) ;
#52631 = ORIENTED_EDGE ( 'NONE', *, *, #17446, .F. ) ;
#52632 = SURFACE_SIDE_STYLE ('',( #36481 ) ) ;
#52634 = PLANE ( 'NONE',  #54866 ) ;
#52633 = CARTESIAN_POINT ( 'NONE',  ( -18.25000000000000711, 31.24999999999999289, -3.750000000000000000 ) ) ;
#52635 = CARTESIAN_POINT ( 'NONE',  ( -141.6550000000000011, -7.632228543268600340, -2.479861379858950166 ) ) ;
#52636 =( NAMED_UNIT ( * ) SI_UNIT ( $, .STERADIAN. ) SOLID_ANGLE_UNIT ( ) );
#52637 = DIRECTION ( 'NONE',  ( 0.000000000000000000, 0.000000000000000000, 1.000000000000000000 ) ) ;
#52638 = CARTESIAN_POINT ( 'NONE',  ( -152.0949999999999420, -2.607480562269071545, -8.024999999999991473 ) ) ;
#52639 = AXIS2_PLACEMENT_3D ( 'NONE', #33113, #59467, #6700 ) ;
#52640 = CARTESIAN_POINT ( 'NONE',  ( -134.9949999999999477, -6.826472737025113702, 4.959722759717902107 ) ) ;
#52641 = ORIENTED_EDGE ( 'NONE', *, *, #59558, .T. ) ;
#52642 = PRESENTATION_LAYER_ASSIGNMENT (  '', '', ( #859 ) ) ;
#52643 = FACE_OUTER_BOUND ( 'NONE', #22343, .T. ) ;
#52644 = DIRECTION ( 'NONE',  ( 1.000000000000000000, 0.000000000000000000, 0.000000000000000000 ) ) ;
#52645 = CARTESIAN_POINT ( 'NONE',  ( -66.35499999999998977, -4.716976649647093289, -6.492361379858945902 ) ) ;
#52646 = DIRECTION ( 'NONE',  ( -0.2413793103448194644, 0.9704308468600220117, 0.000000000000000000 ) ) ;
#52647 = CARTESIAN_POINT ( 'NONE',  ( -10.01517768586949231, 156.3049999999999500, -6.132527647946036459E-16 ) ) ;
#52648 = DIRECTION ( 'NONE',  ( 1.091455702833321811E-16, -1.000000000000000000, 2.220446049250313081E-16 ) ) ;
#52649 = CIRCLE ( 'NONE', #63869, 0.5000000000000004441 ) ;
#52650 = DIRECTION ( 'NONE',  ( 0.000000000000000000, 0.000000000000000000, -1.000000000000000000 ) ) ;
#52651 = DIRECTION ( 'NONE',  ( -1.000000000000000000, -0.000000000000000000, -0.000000000000000000 ) ) ;
#52652 = DIRECTION ( 'NONE',  ( 0.000000000000000000, 0.000000000000000000, -1.000000000000000000 ) ) ;
#52653 = EDGE_CURVE ( 'NONE', #16376, #59091, #9230, .T. ) ;
#52654 =( LENGTH_UNIT ( ) NAMED_UNIT ( * ) SI_UNIT ( .MILLI., .METRE. ) );
#52655 = EDGE_LOOP ( 'NONE', ( #44320, #19096, #11823, #38097 ) ) ;
#52656 = ORIENTED_EDGE ( 'NONE', *, *, #61139, .F. ) ;
#52657 = SURFACE_SIDE_STYLE ('',( #4082 ) ) ;
#52658 = CARTESIAN_POINT ( 'NONE',  ( 3.409440450231733699, -1.719598803866701386, -7.000000000000002665 ) ) ;
#52659 = EDGE_CURVE ( 'NONE', #9871, #59451, #39498, .T. ) ;
#52660 = EDGE_CURVE ( 'NONE', #69671, #5028, #24835, .T. ) ;
#52661 = VECTOR ( 'NONE', #53730, 1000.000000000000000 ) ;
#52662 = CARTESIAN_POINT ( 'NONE',  ( -20.35573775503900151, 114.9974703310426634, 9.999999999999998224 ) ) ;
#52663 = CARTESIAN_POINT ( 'NONE',  ( 4.250000000000001776, 22.24999999999998579, -3.750000000000000000 ) ) ;
#52664 = ORIENTED_EDGE ( 'NONE', *, *, #60106, .T. ) ;
#52666 = EDGE_LOOP ( 'NONE', ( #30603, #7371, #10714, #62012 ) ) ;
#52665 = AXIS2_PLACEMENT_3D ( 'NONE', #38807, #13065, #28533 ) ;
#52667 = CARTESIAN_POINT ( 'NONE',  ( -65.50000000000000000, -1.956686671034892874E-14, -6.500000000000000000 ) ) ;
#52668 = FACE_OUTER_BOUND ( 'NONE', #204, .T. ) ;
#52669 = EDGE_CURVE ( 'NONE', #23306, #25927, #19207, .T. ) ;
#52670 = CARTESIAN_POINT ( 'NONE',  ( -20.71231517720798365, 149.5697028012963301, 10.00000000000000000 ) ) ;
#52671 = ORIENTED_EDGE ( 'NONE', *, *, #59335, .T. ) ;
#52672 = CARTESIAN_POINT ( 'NONE',  ( 3.094860106618431583, 118.2049999999999699, 9.525000000000000355 ) ) ;
#52673 = ORIENTED_EDGE ( 'NONE', *, *, #49747, .F. ) ;
#52674 = ADVANCED_FACE ( 'NONE', ( #25723 ), #68665, .T. ) ;
#52675 = VECTOR ( 'NONE', #52430, 1000.000000000000000 ) ;
#52676 = ADVANCED_FACE ( 'NONE', ( #63376 ), #66389, .F. ) ;
#52677 = CARTESIAN_POINT ( 'NONE',  ( -45.00000000000000000, 1.044011396273118676E-15, -8.525000000000000355 ) ) ;
#52678 = CARTESIAN_POINT ( 'NONE',  ( -101.6949999999999790, -8.437984349512085203, 5.166775262442717831E-16 ) ) ;
#52679 = ORIENTED_EDGE ( 'NONE', *, *, #21523, .F. ) ;
#52680 = AXIS2_PLACEMENT_3D ( 'NONE', #16040, #54320, #58924 ) ;
#52681 = CARTESIAN_POINT ( 'NONE',  ( -8.594831491281922808, 110.4999999999999858, 4.199347284499536315 ) ) ;
#52682 = CARTESIAN_POINT ( 'NONE',  ( -53.54292637653379217, 9.058813317711329915, 2.943386871421369566 ) ) ;
#52683 = EDGE_CURVE ( 'NONE', #23192, #29467, #34717, .T. ) ;
#52684 = DIRECTION ( 'NONE',  ( -1.000000000000000000, 0.000000000000000000, 0.000000000000000000 ) ) ;
#52685 = EDGE_LOOP ( 'NONE', ( #4214, #10134, #7442, #14401 ) ) ;
#52686 = CARTESIAN_POINT ( 'NONE',  ( -9.827790563157511022E-16, 157.4429263765338192, 8.025000000000000355 ) ) ;
#52687 = DIRECTION ( 'NONE',  ( 0.000000000000000000, 1.000000000000000000, -0.000000000000000000 ) ) ;
#52688 = AXIS2_PLACEMENT_3D ( 'NONE', #484, #61010, #33594 ) ;
#52689 = STYLED_ITEM ( 'NONE', ( #22252 ), #66698 ) ;
#52690 = DIRECTION ( 'NONE',  ( 0.000000000000000000, 0.000000000000000000, -1.000000000000000000 ) ) ;
#52691 = EDGE_LOOP ( 'NONE', ( #27737, #1101, #67915, #66061 ) ) ;
#52692 = CARTESIAN_POINT ( 'NONE',  ( 20.86748625714523087, 115.0277251398784273, -10.00000000000000000 ) ) ;
#52693 = ORIENTED_EDGE ( 'NONE', *, *, #6261, .T. ) ;
#52694 = CARTESIAN_POINT ( 'NONE',  ( -60.00000000000000000, -2.024042244987997205E-14, -12.00000000000000000 ) ) ;
#52695 = SURFACE_SIDE_STYLE ('',( #19625 ) ) ;
#52696 = MECHANICAL_DESIGN_GEOMETRIC_PRESENTATION_REPRESENTATION (  '', ( #3164 ), #31325 ) ;
#52697 = CARTESIAN_POINT ( 'NONE',  ( -70.75000000000000000, -0.9999999999999995559, 24.00000000000000000 ) ) ;
#52698 = VECTOR ( 'NONE', #7534, 1000.000000000000000 ) ;
#52699 = CARTESIAN_POINT ( 'NONE',  ( 71.50000000000000000, 35.92875272052971525, 10.00000000000000000 ) ) ;
#52700 = CARTESIAN_POINT ( 'NONE',  ( -74.10730706101928433, 9.343722028457024820, 6.169771923672650260 ) ) ;
#52701 = DIRECTION ( 'NONE',  ( -1.000000000000000000, -0.000000000000000000, -0.000000000000000000 ) ) ;
#52702 = CARTESIAN_POINT ( 'NONE',  ( 0.000000000000000000, 119.9429263765338050, -8.025000000000000355 ) ) ;
#52703 = CARTESIAN_POINT ( 'NONE',  ( 2.999999999999997335, 5.000000000000000000, 72.00402776293822171 ) ) ;
#52704 = ORIENTED_EDGE ( 'NONE', *, *, #52222, .T. ) ;
#52705 = ORIENTED_EDGE ( 'NONE', *, *, #33168, .F. ) ;
#52706 = DIRECTION ( 'NONE',  ( -0.000000000000000000, -0.000000000000000000, -1.000000000000000000 ) ) ;
#52707 = FACE_OUTER_BOUND ( 'NONE', #60177, .T. ) ;
#52708 = CARTESIAN_POINT ( 'NONE',  ( -182.0929263765338249, 3.094860106619032880, 9.524999999999554490 ) ) ;
#52709 = SURFACE_STYLE_USAGE ( .BOTH. , #36573 ) ;
#52710 = ORIENTED_EDGE ( 'NONE', *, *, #47488, .F. ) ;
#52711 = CARTESIAN_POINT ( 'NONE',  ( -22.50000000000000711, 34.24999999999999289, -3.750000000000000000 ) ) ;
#52712 = CARTESIAN_POINT ( 'NONE',  ( -166.5550000000000068, 0.000000000000000000, 8.024999999999991473 ) ) ;
#52713 = CARTESIAN_POINT ( 'NONE',  ( 15.98999599679679839, 117.9999999999999716, 7.500000000000000000 ) ) ;
#52714 =( LENGTH_UNIT ( ) NAMED_UNIT ( * ) SI_UNIT ( .MILLI., .METRE. ) );
#52715 = CARTESIAN_POINT ( 'NONE',  ( -50.15707362346616094, -9.058813317711329915, -2.943386871421370898 ) ) ;
#52716 = CARTESIAN_POINT ( 'NONE',  ( -180.2949999999999591, -2.607480562269069768, 8.024999999999991473 ) ) ;
#52717 = ORIENTED_EDGE ( 'NONE', *, *, #37853, .F. ) ;
#52718 = CARTESIAN_POINT ( 'NONE',  ( 8.690363669209107300, 2.947848588679142789, 0.1381979515792646496 ) ) ;
#52720 = DIRECTION ( 'NONE',  ( 1.000000000000000000, 0.000000000000000000, 0.000000000000000000 ) ) ;
#52719 = AXIS2_PLACEMENT_3D ( 'NONE', #12374, #12038, #7120 ) ;
#52721 = FILL_AREA_STYLE ('',( #69570 ) ) ;
#52722 = CARTESIAN_POINT ( 'NONE',  ( -94.40500000000000114, -2.607480562269069768, 8.024999999999991473 ) ) ;
#52723 = SURFACE_STYLE_FILL_AREA ( #25609 ) ;
#52724 = DIRECTION ( 'NONE',  ( 0.000000000000000000, 0.000000000000000000, 1.000000000000000000 ) ) ;
#52725 = FACE_OUTER_BOUND ( 'NONE', #11501, .T. ) ;
#52726 = AXIS2_PLACEMENT_3D ( 'NONE', #37167, #31831, #54330 ) ;
#52727 = CARTESIAN_POINT ( 'NONE',  ( -88.49499999999999034, 6.826472737025113702, -4.959722759717902107 ) ) ;
#52728 = CARTESIAN_POINT ( 'NONE',  ( 8.102448949553181734, 127.5049999999999812, 5.886773742842750679 ) ) ;
#52729 = CARTESIAN_POINT ( 'NONE',  ( -60.29499999999999460, -2.607480562269069768, 8.024999999999991473 ) ) ;
#52730 = CARTESIAN_POINT ( 'NONE',  ( -75.00000000000000000, 8.553246373267512581, -6.928940927505454539 ) ) ;
#52731 = AXIS2_PLACEMENT_3D ( 'NONE', #63496, #63824, #36802 ) ;
#52732 = CARTESIAN_POINT ( 'NONE',  ( -170.8429263765337964, 9.058813317711329915, -2.943386871421373119 ) ) ;
#52733 = SURFACE_STYLE_FILL_AREA ( #9828 ) ;
#52734 = MECHANICAL_DESIGN_GEOMETRIC_PRESENTATION_REPRESENTATION (  '', ( #4382 ), #48286 ) ;
#52735 =( LENGTH_UNIT ( ) NAMED_UNIT ( * ) SI_UNIT ( .MILLI., .METRE. ) );
#52736 = VECTOR ( 'NONE', #26510, 1000.000000000000000 ) ;
#52737 =( NAMED_UNIT ( * ) SI_UNIT ( $, .STERADIAN. ) SOLID_ANGLE_UNIT ( ) );
#52738 = ORIENTED_EDGE ( 'NONE', *, *, #36248, .F. ) ;
#52739 = FILL_AREA_STYLE ('',( #9135 ) ) ;
#52740 = PRESENTATION_LAYER_ASSIGNMENT (  '', '', ( #57181 ) ) ;
#52741 = EDGE_CURVE ( 'NONE', #35195, #529, #24175, .T. ) ;
#52742 = FACE_OUTER_BOUND ( 'NONE', #54813, .T. ) ;
#52743 = EDGE_CURVE ( 'NONE', #13980, #618, #61116, .T. ) ;
#52745 = LINE ( 'NONE', #26323, #5655 ) ;
#52744 = DIRECTION ( 'NONE',  ( -1.000000000000000000, -0.000000000000000000, -0.000000000000000000 ) ) ;
#52746 = FACE_OUTER_BOUND ( 'NONE', #54, .T. ) ;
#52747 = ORIENTED_EDGE ( 'NONE', *, *, #6993, .T. ) ;
#52748 = ORIENTED_EDGE ( 'NONE', *, *, #47634, .F. ) ;
#52749 = CARTESIAN_POINT ( 'NONE',  ( 18.25000000000000711, 33.74999999999999289, -3.750000000000000000 ) ) ;
#52750 = LINE ( 'NONE', #45604, #2686 ) ;
#52751 = AXIS2_PLACEMENT_3D ( 'NONE', #39674, #45988, #61095 ) ;
#52752 = EDGE_CURVE ( 'NONE', #42499, #1545, #15813, .T. ) ;
#52753 = APPLICATION_CONTEXT ( 'automotive_design' ) ;
#52754 = CYLINDRICAL_SURFACE ( 'NONE', #7125, 9.524999999999991473 ) ;
#52755 = DIRECTION ( 'NONE',  ( -0.000000000000000000, -1.000000000000000000, -0.000000000000000000 ) ) ;
#52756 = EDGE_LOOP ( 'NONE', ( #11666, #52849, #26519, #6636 ) ) ;
#52757 = CARTESIAN_POINT ( 'NONE',  ( -117.9549999999999841, -7.632228543268599452, 2.479861379858951054 ) ) ;
#52758 = EDGE_LOOP ( 'NONE', ( #56381, #15874, #49372, #43460 ) ) ;
#52759 = CARTESIAN_POINT ( 'NONE',  ( 45.50000000000000000, 10.69371294336137801, 3.999999999999999112 ) ) ;
#52760 = CARTESIAN_POINT ( 'NONE',  ( 8.437984349512095861, 129.3070736234661524, 1.550032578732816828E-15 ) ) ;
#52761 = ORIENTED_EDGE ( 'NONE', *, *, #35340, .T. ) ;
#52762 = FACE_OUTER_BOUND ( 'NONE', #18540, .T. ) ;
#52763 = CARTESIAN_POINT ( 'NONE',  ( 7.766391886667106448, 1.733608113333017453, 0.5482146608018618750 ) ) ;
#52764 = VERTEX_POINT ( 'NONE', #59456 ) ;
#52765 = EDGE_CURVE ( 'NONE', #60632, #66255, #23155, .T. ) ;
#52766 = COLOUR_RGB ( '', 0.09019608, 0.27058824, 0.51372549) ;
#52767 = AXIS2_PLACEMENT_3D ( 'NONE', #42103, #57888, #4369 ) ;
#52768 = CARTESIAN_POINT ( 'NONE',  ( 5.598654528085805993, 150.2449999999999761, 7.705886871421374629 ) ) ;
#52769 = DIRECTION ( 'NONE',  ( 0.000000000000000000, -1.000000000000000000, 0.000000000000000000 ) ) ;
#52770 = ORIENTED_EDGE ( 'NONE', *, *, #52814, .F. ) ;
#52771 = LINE ( 'NONE', #62265, #61102 ) ;
#52772 = CARTESIAN_POINT ( 'NONE',  ( 0.000000000000000000, 152.5550000000000068, -9.525000000000000355 ) ) ;
#52773 = CARTESIAN_POINT ( 'NONE',  ( -136.1070736234661922, 8.102448949553172852, -5.886773742842744461 ) ) ;
#52774 = STYLED_ITEM ( 'NONE', ( #51494 ), #44058 ) ;
#52775 = EDGE_CURVE ( 'NONE', #3199, #55926, #20299, .T. ) ;
#52776 = CARTESIAN_POINT ( 'NONE',  ( 12.72792206135785698, 115.4999999999999574, -10.50000000000000000 ) ) ;
#52777 = VERTEX_POINT ( 'NONE', #61442 ) ;
#52778 = CARTESIAN_POINT ( 'NONE',  ( -6.826472737025120807, 123.9929263765338163, 4.959722759717906548 ) ) ;
#52779 = LINE ( 'NONE', #20762, #5330 ) ;
#52780 =( NAMED_UNIT ( * ) PLANE_ANGLE_UNIT ( ) SI_UNIT ( $, .RADIAN. ) );
#52781 = FACE_OUTER_BOUND ( 'NONE', #18965, .T. ) ;
#52782 = LINE ( 'NONE', #3850, #36267 ) ;
#52783 = CARTESIAN_POINT ( 'NONE',  ( 45.50000000000000000, 9.639620389971918613, -6.500000000000000000 ) ) ;
#52784 = ORIENTED_EDGE ( 'NONE', *, *, #52589, .F. ) ;
#52785 = AXIS2_PLACEMENT_3D ( 'NONE', #18348, #67212, #18999 ) ;
#52786 = FACE_OUTER_BOUND ( 'NONE', #37292, .T. ) ;
#52787 = EDGE_LOOP ( 'NONE', ( #6536, #5746, #57219, #32238 ) ) ;
#52788 = CARTESIAN_POINT ( 'NONE',  ( -58.19292637653381206, -10.01517768586948698, 6.132527647946031529E-16 ) ) ;
#52789 = CONICAL_SURFACE ( 'NONE', #65095, 5.499999999999976907, 0.7853981633974300713 ) ;
#52790 =( NAMED_UNIT ( * ) PLANE_ANGLE_UNIT ( ) SI_UNIT ( $, .RADIAN. ) );
#52791 = CARTESIAN_POINT ( 'NONE',  ( -24.21231517720798010, 113.4999999999999858, 7.500000000000000000 ) ) ;
#52792 = CARTESIAN_POINT ( 'NONE',  ( -157.2549999999999955, -4.716976649647092401, 6.492361379858946790 ) ) ;
#52793 = ORIENTED_EDGE ( 'NONE', *, *, #12952, .F. ) ;
#52794 = FILL_AREA_STYLE_COLOUR ( '', #67705 ) ;
#52795 =( BOUNDED_CURVE ( )  B_SPLINE_CURVE ( 3, ( #33933, #6492, #44884, #66289 ),
 .UNSPECIFIED., .F., .F. ) 
 B_SPLINE_CURVE_WITH_KNOTS ( ( 4, 4 ),
 ( 1.570796326794894116, 3.141592653589793116 ),
 .UNSPECIFIED. ) 
 CURVE ( )  GEOMETRIC_REPRESENTATION_ITEM ( )  RATIONAL_B_SPLINE_CURVE ( ( 1.000000000000000000, 0.8047378541243643824, 0.8047378541243643824, 1.000000000000000000 ) ) 
 REPRESENTATION_ITEM ( '' )  );
#52796 = CARTESIAN_POINT ( 'NONE',  ( -9.250000000000003553, 27.74999999999998934, -3.750000000000000000 ) ) ;
#52797 = MECHANICAL_DESIGN_GEOMETRIC_PRESENTATION_REPRESENTATION (  '', ( #6714 ), #55005 ) ;
#52798 = DIRECTION ( 'NONE',  ( 1.000000000000000000, 0.000000000000000000, 0.000000000000000000 ) ) ;
#52799 = CARTESIAN_POINT ( 'NONE',  ( -69.89292637653379359, -8.102448949553174629, -5.886773742842741797 ) ) ;
#52800 = ORIENTED_EDGE ( 'NONE', *, *, #68319, .T. ) ;
#52801 = AXIS2_PLACEMENT_3D ( 'NONE', #25975, #63957, #11187 ) ;
#52802 = ORIENTED_EDGE ( 'NONE', *, *, #38505, .T. ) ;
#52803 = CARTESIAN_POINT ( 'NONE',  ( -1.000000000000028644, 0.000000000000000000, 0.000000000000000000 ) ) ;
#52804 = DIRECTION ( 'NONE',  ( 1.000000000000000000, 0.000000000000000000, 0.000000000000000000 ) ) ;
#52805 = CARTESIAN_POINT ( 'NONE',  ( -67.25499999999998124, -4.716976649647092401, 6.492361379858946790 ) ) ;
#52806 = ORIENTED_EDGE ( 'NONE', *, *, #58778, .T. ) ;
#52807 = CARTESIAN_POINT ( 'NONE',  ( 22.00000000000002132, 43.00000000000000000, 75.00000000000000000 ) ) ;
#52808 = CARTESIAN_POINT ( 'NONE',  ( 30.25000000000000711, 18.74999999999997868, -3.750000000000000000 ) ) ;
#52809 = CIRCLE ( 'NONE', #32526, 0.2500000000000002220 ) ;
#52810 = CARTESIAN_POINT ( 'NONE',  ( -166.5570736234661808, -1.166476076187852838E-15, -9.524999999999991473 ) ) ;
#52811 = DIRECTION ( 'NONE',  ( 0.000000000000000000, 0.000000000000000000, 1.000000000000000000 ) ) ;
#52812 = COLOUR_RGB ( '', 0.72549020, 0.75294118, 0.79215686) ;
#52813 = VERTEX_POINT ( 'NONE', #13262 ) ;
#52814 = EDGE_CURVE ( 'NONE', #38619, #57494, #56271, .T. ) ;
#52815 = DIRECTION ( 'NONE',  ( 0.000000000000000000, 0.000000000000000000, -1.000000000000000000 ) ) ;
#52816 =( NAMED_UNIT ( * ) PLANE_ANGLE_UNIT ( ) SI_UNIT ( $, .RADIAN. ) );
#52818 = CARTESIAN_POINT ( 'NONE',  ( 7.632228543268607446, 126.1570736234661467, 2.479861379858954606 ) ) ;
#52817 = DIRECTION ( 'NONE',  ( -1.000000000000000000, 0.000000000000000000, 0.000000000000000000 ) ) ;
#52819 = CARTESIAN_POINT ( 'NONE',  ( -121.7949999999999875, 2.607480562269069324, -8.024999999999993250 ) ) ;
#52820 = CARTESIAN_POINT ( 'NONE',  ( 3.094860106618431583, 144.0949999999999704, 9.525000000000000355 ) ) ;
#52821 = CARTESIAN_POINT ( 'NONE',  ( -101.0949999999999989, -2.607480562269071545, -8.024999999999991473 ) ) ;
#52822 = CARTESIAN_POINT ( 'NONE',  ( -15.00000000000000000, 8.000000000000000000, -3.500000000000017764 ) ) ;
#52823 = DIRECTION ( 'NONE',  ( 0.000000000000000000, -1.000000000000000000, 0.000000000000000000 ) ) ;
#52824 = AXIS2_PLACEMENT_3D ( 'NONE', #450, #33220, #22309 ) ;
#52825 = CARTESIAN_POINT ( 'NONE',  ( -43.75000000000000000, 0.000000000000000000, -7.000000000000000000 ) ) ;
#52827 = ORIENTED_EDGE ( 'NONE', *, *, #47577, .F. ) ;
#52826 = AXIS2_PLACEMENT_3D ( 'NONE', #22180, #64747, #10593 ) ;
#52828 = CARTESIAN_POINT ( 'NONE',  ( -138.2929263765338419, 3.094860106618428031, -9.524999999999993250 ) ) ;
#52829 =( NAMED_UNIT ( * ) PLANE_ANGLE_UNIT ( ) SI_UNIT ( $, .RADIAN. ) );
#52830 = CARTESIAN_POINT ( 'NONE',  ( -195.0000000000000000, 0.000000000000000000, 9.524999999999991473 ) ) ;
#52831 = CARTESIAN_POINT ( 'NONE',  ( -161.8449999999999989, -7.632228543268599452, 2.479861379858951054 ) ) ;
#52832 = ADVANCED_FACE ( 'NONE', ( #41086 ), #41787, .T. ) ;
#52833 = ADVANCED_FACE ( 'NONE', ( #14679 ), #52332, .T. ) ;
#52834 = SURFACE_STYLE_USAGE ( .BOTH. , #38671 ) ;
#52835 =( GEOMETRIC_REPRESENTATION_CONTEXT ( 3 ) GLOBAL_UNCERTAINTY_ASSIGNED_CONTEXT ( ( #63128 ) ) GLOBAL_UNIT_ASSIGNED_CONTEXT ( ( #5209, #10521, #35860 ) ) REPRESENTATION_CONTEXT ( 'NONE', 'WORKASPACE' ) );
#52836 = AXIS2_PLACEMENT_3D ( 'NONE', #33775, #68983, #31309 ) ;
#52837 = CARTESIAN_POINT ( 'NONE',  ( -133.6429263765338078, -5.598654528085801552, 7.705886871421367523 ) ) ;
#52838 = VERTEX_POINT ( 'NONE', #29805 ) ;
#52839 = ORIENTED_EDGE ( 'NONE', *, *, #32218, .F. ) ;
#52840 = AXIS2_PLACEMENT_3D ( 'NONE', #3918, #2850, #40562 ) ;
#52841 = CYLINDRICAL_SURFACE ( 'NONE', #43172, 0.2500000000000002220 ) ;
#52842 = EDGE_CURVE ( 'NONE', #51825, #47861, #25219, .T. ) ;
#52843 = CARTESIAN_POINT ( 'NONE',  ( -45.00000000000000000, 8.745397170020954292, 6.877347455810014054 ) ) ;
#52844 = VECTOR ( 'NONE', #27258, 1000.000000000000000 ) ;
#52845 = EDGE_CURVE ( 'NONE', #55122, #45002, #68488, .T. ) ;
#52846 = FACE_OUTER_BOUND ( 'NONE', #22537, .T. ) ;
#52847 = EDGE_LOOP ( 'NONE', ( #42115, #1317 ) ) ;
#52848 = CARTESIAN_POINT ( 'NONE',  ( -152.0049999999999955, 6.826472737025115478, 4.959722759717899443 ) ) ;
#52849 = ORIENTED_EDGE ( 'NONE', *, *, #18407, .F. ) ;
#52850 = LINE ( 'NONE', #4980, #14450 ) ;
#52851 =( LENGTH_UNIT ( ) NAMED_UNIT ( * ) SI_UNIT ( .MILLI., .METRE. ) );
#52852 = ORIENTED_EDGE ( 'NONE', *, *, #40619, .T. ) ;
#52853 = COLOUR_RGB ( '', 0.31764706, 0.68627451, 0.89019608) ;
#52854 = EDGE_CURVE ( 'NONE', #29473, #42106, #4609, .T. ) ;
#52855 =( NAMED_UNIT ( * ) SI_UNIT ( $, .STERADIAN. ) SOLID_ANGLE_UNIT ( ) );
#52856 = CARTESIAN_POINT ( 'NONE',  ( 65.49999999999997158, 2.470600640510325396E-15, -12.00000000000000000 ) ) ;
#52857 = CARTESIAN_POINT ( 'NONE',  ( -8.102448949553181734, 119.4949999999999903, 5.886773742842747126 ) ) ;
#52858 = FACE_OUTER_BOUND ( 'NONE', #21008, .T. ) ;
#52859 = ORIENTED_EDGE ( 'NONE', *, *, #28967, .T. ) ;
#52860 = CARTESIAN_POINT ( 'NONE',  ( -3.094860106618432471, 119.7049999999999983, -9.525000000000000355 ) ) ;
#52861 = CARTESIAN_POINT ( 'NONE',  ( -60.05499999999998550, -9.827790563157499189E-16, -8.024999999999991473 ) ) ;
#52862 = EDGE_CURVE ( 'NONE', #15154, #30495, #1500, .T. ) ;
#52863 = ORIENTED_EDGE ( 'NONE', *, *, #35742, .F. ) ;
#52864 = CARTESIAN_POINT ( 'NONE',  ( -9.058813317711337021, 150.1549999999999727, -2.943386871421374895 ) ) ;
#52865 = AXIS2_PLACEMENT_3D ( 'NONE', #25282, #52724, #25957 ) ;
#52866 = CARTESIAN_POINT ( 'NONE',  ( 30.99999999999999289, 5.000000000000000000, 37.00402776293829277 ) ) ;
#52867 = DIRECTION ( 'NONE',  ( -0.000000000000000000, -0.000000000000000000, -1.000000000000000000 ) ) ;
#52868 = CARTESIAN_POINT ( 'NONE',  ( -4.750000000000000000, 0.000000000000000000, 0.7500000000000000000 ) ) ;
#52869 = ORIENTED_EDGE ( 'NONE', *, *, #35919, .T. ) ;
#52870 =( NAMED_UNIT ( * ) SI_UNIT ( $, .STERADIAN. ) SOLID_ANGLE_UNIT ( ) );
#52871 = DIRECTION ( 'NONE',  ( 0.000000000000000000, 0.000000000000000000, 1.000000000000000000 ) ) ;
#52872 = CARTESIAN_POINT ( 'NONE',  ( -195.0000000000000000, 1.166476076187852838E-15, -9.524999999999991473 ) ) ;
#52873 = CARTESIAN_POINT ( 'NONE',  ( -183.3549999999999898, -4.716976649647093289, -6.492361379858945902 ) ) ;
#52874 = VERTEX_POINT ( 'NONE', #40376 ) ;
#52875 = CARTESIAN_POINT ( 'NONE',  ( -54.73148258177910463, -9.107254030097815090, -2.000000000000000000 ) ) ;
#52876 = DIRECTION ( 'NONE',  ( -1.000000000000000000, 0.000000000000000000, 0.000000000000000000 ) ) ;
#52877 = MECHANICAL_DESIGN_GEOMETRIC_PRESENTATION_REPRESENTATION (  '', ( #39373 ), #13523 ) ;
#52878 = ORIENTED_EDGE ( 'NONE', *, *, #49490, .F. ) ;
#52879 = FACE_OUTER_BOUND ( 'NONE', #60261, .T. ) ;
#52880 = DIRECTION ( 'NONE',  ( 1.000000000000000000, 0.000000000000000000, 0.000000000000000000 ) ) ;
#52881 = ORIENTED_EDGE ( 'NONE', *, *, #51136, .T. ) ;
#52882 = DIRECTION ( 'NONE',  ( 1.000000000000000000, 0.000000000000000000, 0.000000000000000000 ) ) ;
#52883 =( LENGTH_UNIT ( ) NAMED_UNIT ( * ) SI_UNIT ( .MILLI., .METRE. ) );
#52884 = CARTESIAN_POINT ( 'NONE',  ( -98.60499999999997556, 6.826472737025113702, -4.959722759717902107 ) ) ;
#52885 = ORIENTED_EDGE ( 'NONE', *, *, #60826, .T. ) ;
#52886 = DIRECTION ( 'NONE',  ( 0.000000000000000000, 0.000000000000000000, -1.000000000000000000 ) ) ;
#52887 = CARTESIAN_POINT ( 'NONE',  ( -130.5570736234661808, -1.166476076187852838E-15, -9.524999999999991473 ) ) ;
#52888 = AXIS2_PLACEMENT_3D ( 'NONE', #66042, #16856, #38329 ) ;
#52889 = CARTESIAN_POINT ( 'NONE',  ( 0.000000000000000000, 151.4449999999999932, -9.525000000000000355 ) ) ;
#52890 = CARTESIAN_POINT ( 'NONE',  ( -76.40707362346614673, 3.094860106618428031, -9.524999999999993250 ) ) ;
#52891 = ADVANCED_FACE ( 'NONE', ( #46372 ), #51268, .F. ) ;
#52892 = ORIENTED_EDGE ( 'NONE', *, *, #38156, .T. ) ;
#52893 = SURFACE_STYLE_FILL_AREA ( #32436 ) ;
#52894 = CARTESIAN_POINT ( 'NONE',  ( -17.51869064886620109, -11.19266561951042149, -4.331441116418161208 ) ) ;
#52895 =( NAMED_UNIT ( * ) SI_UNIT ( $, .STERADIAN. ) SOLID_ANGLE_UNIT ( ) );
#52896 = CARTESIAN_POINT ( 'NONE',  ( -113.9049999999999869, 2.607480562269068880, -8.024999999999993250 ) ) ;
#52897 = LINE ( 'NONE', #65060, #34804 ) ;
#52898 = CARTESIAN_POINT ( 'NONE',  ( 5.598654528085805993, 120.2449999999999903, 7.705886871421374629 ) ) ;
#52899 = CARTESIAN_POINT ( 'NONE',  ( -121.9449999999999932, -9.827790563157499189E-16, -8.024999999999991473 ) ) ;
#52900 = CARTESIAN_POINT ( 'NONE',  ( -9.827790563157511022E-16, 124.4429263765338192, 8.025000000000000355 ) ) ;
#52901 = VECTOR ( 'NONE', #23064, 1000.000000000000000 ) ;
#52902 = EDGE_CURVE ( 'NONE', #36693, #39699, #24885, .T. ) ;
#52903 = ORIENTED_EDGE ( 'NONE', *, *, #32115, .F. ) ;
#52904 = CARTESIAN_POINT ( 'NONE',  ( -163.9429263765338192, 0.000000000000000000, 9.524999999999991473 ) ) ;
#52905 = DIRECTION ( 'NONE',  ( 1.000000000000000000, 0.000000000000000000, 0.000000000000000000 ) ) ;
#52906 = EDGE_CURVE ( 'NONE', #43714, #65168, #6920, .T. ) ;
#52907 = ADVANCED_FACE ( 'NONE', ( #56889 ), #53594, .T. ) ;
#52908 = CARTESIAN_POINT ( 'NONE',  ( -8.437984349512095861, 148.8070736234661240, -5.166775262442723748E-16 ) ) ;
#52909 = CARTESIAN_POINT ( 'NONE',  ( -21.02379604162874926, 114.4999999999999574, -10.00000000000000000 ) ) ;
#52910 = CYLINDRICAL_SURFACE ( 'NONE', #6964, 0.5000000000000004441 ) ;
#52911 = ORIENTED_EDGE ( 'NONE', *, *, #24077, .F. ) ;
#52912 = CONICAL_SURFACE ( 'NONE', #36094, 9.000000000000000000, 0.7853981633974500554 ) ;
#52913 = CARTESIAN_POINT ( 'NONE',  ( -72.89292637653380780, -8.102448949553172852, -5.886773742842741797 ) ) ;
#52914 = CARTESIAN_POINT ( 'NONE',  ( 39.24999999999999289, 15.99999999999997691, -3.750000000000000000 ) ) ;
#52915 = FILL_AREA_STYLE ('',( #26156 ) ) ;
#52916 = ADVANCED_FACE ( 'NONE', ( #49559 ), #61015, .F. ) ;
#52917 = STYLED_ITEM ( 'NONE', ( #19655 ), #12452 ) ;
#52918 = CARTESIAN_POINT ( 'NONE',  ( 0.000000000000000000, 152.9429263765338192, -8.025000000000000355 ) ) ;
#52919 = CARTESIAN_POINT ( 'NONE',  ( 8.437984349512095861, 147.3070736234662093, 1.550032578732816828E-15 ) ) ;
#52920 = CARTESIAN_POINT ( 'NONE',  ( 45.00000000000000000, -1.469576158976824618E-14, 6.999999999999999112 ) ) ;
#52921 = EDGE_CURVE ( 'NONE', #12616, #69397, #8026, .T. ) ;
#52922 = AXIS2_PLACEMENT_3D ( 'NONE', #25288, #9483, #24245 ) ;
#52923 = CARTESIAN_POINT ( 'NONE',  ( -175.1050000000000182, -6.826472737025113702, 4.959722759717902107 ) ) ;
#52924 = VERTEX_POINT ( 'NONE', #7224 ) ;
#52925 = CARTESIAN_POINT ( 'NONE',  ( -11.74999999999999645, -0.9999999999999995559, 6.000000000000001776 ) ) ;
#52926 = CARTESIAN_POINT ( 'NONE',  ( 4.500000000000002665, 22.24999999999998579, -3.750000000000000000 ) ) ;
#52927 = AXIS2_PLACEMENT_3D ( 'NONE', #10271, #21498, #64416 ) ;
#52928 = DIRECTION ( 'NONE',  ( 0.000000000000000000, -1.000000000000000000, -8.673617379884034486E-16 ) ) ;
#52929 = ORIENTED_EDGE ( 'NONE', *, *, #8102, .F. ) ;
#52930 = CARTESIAN_POINT ( 'NONE',  ( 93.00000000000000000, 5.000000000000000000, 0.000000000000000000 ) ) ;
#52931 = AXIS2_PLACEMENT_3D ( 'NONE', #46017, #47066, #3369 ) ;
#52932 = CARTESIAN_POINT ( 'NONE',  ( -6.826472737025120807, 139.5070736234661126, -4.959722759717907437 ) ) ;
#52933 = VERTEX_POINT ( 'NONE', #22707 ) ;
#52934 = CARTESIAN_POINT ( 'NONE',  ( -32.76851741822840580, -9.107254030101904263, -2.000000000000000000 ) ) ;
#52935 = CARTESIAN_POINT ( 'NONE',  ( -91.40499999999998693, -2.607480562269069768, 8.024999999999991473 ) ) ;
#52936 =( GEOMETRIC_REPRESENTATION_CONTEXT ( 3 ) GLOBAL_UNCERTAINTY_ASSIGNED_CONTEXT ( ( #15212 ) ) GLOBAL_UNIT_ASSIGNED_CONTEXT ( ( #29633, #40560, #13799 ) ) REPRESENTATION_CONTEXT ( 'NONE', 'WORKASPACE' ) );
#52937 = ORIENTED_EDGE ( 'NONE', *, *, #60899, .F. ) ;
#52938 = LINE ( 'NONE', #30761, #46767 ) ;
#52939 = SURFACE_SIDE_STYLE ('',( #31805 ) ) ;
#52940 = ADVANCED_FACE ( 'NONE', ( #54355 ), #38225, .T. ) ;
#52941 = CYLINDRICAL_SURFACE ( 'NONE', #33336, 5.000000000000011546 ) ;
#52942 =( GEOMETRIC_REPRESENTATION_CONTEXT ( 3 ) GLOBAL_UNCERTAINTY_ASSIGNED_CONTEXT ( ( #9591 ) ) GLOBAL_UNIT_ASSIGNED_CONTEXT ( ( #46047, #2711, #8034 ) ) REPRESENTATION_CONTEXT ( 'NONE', 'WORKASPACE' ) );
#52943 = ORIENTED_EDGE ( 'NONE', *, *, #2660, .T. ) ;
#52944 = ADVANCED_FACE ( 'NONE', ( #49451 ), #23384, .F. ) ;
#52945 = CARTESIAN_POINT ( 'NONE',  ( -75.44499999999997897, 0.000000000000000000, 8.024999999999991473 ) ) ;
#52946 = ORIENTED_EDGE ( 'NONE', *, *, #42157, .F. ) ;
#52947 = DIRECTION ( 'NONE',  ( 0.000000000000000000, 0.000000000000000000, 1.000000000000000000 ) ) ;
#52948 = SURFACE_SIDE_STYLE ('',( #58213 ) ) ;
#52949 = ORIENTED_EDGE ( 'NONE', *, *, #436, .T. ) ;
#52950 = CARTESIAN_POINT ( 'NONE',  ( -69.74999999999998579, -4.000000000000000000, 24.00000000000000000 ) ) ;
#52951 = DIRECTION ( 'NONE',  ( 0.000000000000000000, 1.000000000000000000, 0.000000000000000000 ) ) ;
#52952 = STYLED_ITEM ( 'NONE', ( #47681 ), #6101 ) ;
#52953 = VECTOR ( 'NONE', #33817, 1000.000000000000000 ) ;
#52954 = CARTESIAN_POINT ( 'NONE',  ( -75.00000000000000000, 9.708372675170616972, 6.000000000000000888 ) ) ;
#52955 = EDGE_LOOP ( 'NONE', ( #46649, #22296, #64183, #46601 ) ) ;
#52956 =( NAMED_UNIT ( * ) PLANE_ANGLE_UNIT ( ) SI_UNIT ( $, .RADIAN. ) );
#52957 = ORIENTED_EDGE ( 'NONE', *, *, #57598, .F. ) ;
#52958 = DIRECTION ( 'NONE',  ( 0.000000000000000000, -0.000000000000000000, 1.000000000000000000 ) ) ;
#52959 = DIRECTION ( 'NONE',  ( -1.000000000000000000, 0.000000000000000000, 0.000000000000000000 ) ) ;
#52960 = CARTESIAN_POINT ( 'NONE',  ( -41.72783051798697329, 107.4000574072428833, 3.999999999999999112 ) ) ;
#52961 = CARTESIAN_POINT ( 'NONE',  ( -157.1070736234661354, 8.102448949553171076, -5.886773742842744461 ) ) ;
#52962 = CIRCLE ( 'NONE', #30473, 13.99999999999999822 ) ;
#52963 = CARTESIAN_POINT ( 'NONE',  ( 8.102448949553181734, 123.9949999999999903, -5.886773742842746238 ) ) ;
#52964 = CARTESIAN_POINT ( 'NONE',  ( -106.8570736234661780, -5.598654528085803328, -7.705886871421366635 ) ) ;
#52965 = VECTOR ( 'NONE', #18498, 1000.000000000000000 ) ;
#52966 = PRODUCT_DEFINITION_SHAPE ( 'NONE', 'NONE',  #69694 ) ;
#52967 = ORIENTED_EDGE ( 'NONE', *, *, #58282, .T. ) ;
#52968 = DIRECTION ( 'NONE',  ( 1.000000000000000000, -0.000000000000000000, 0.000000000000000000 ) ) ;
#52969 = DIRECTION ( 'NONE',  ( -1.000000000000000000, 1.156482317317866203E-15, 0.000000000000000000 ) ) ;
#52970 = DIRECTION ( 'NONE',  ( -0.000000000000000000, -0.000000000000000000, 1.000000000000000000 ) ) ;
#52971 = CARTESIAN_POINT ( 'NONE',  ( -143.3050000000000068, 8.437984349512085203, -1.550032578732815448E-15 ) ) ;
#52972 = EDGE_CURVE ( 'NONE', #64724, #12513, #1233, .T. ) ;
#52973 = CARTESIAN_POINT ( 'NONE',  ( -157.0449999999999875, 7.632228543268600340, 2.479861379858949277 ) ) ;
#52974 = CARTESIAN_POINT ( 'NONE',  ( -135.2949999999999875, -2.607480562269069768, 8.024999999999991473 ) ) ;
#52975 = AXIS2_PLACEMENT_3D ( 'NONE', #58198, #10022, #31442 ) ;
#52976 = VERTEX_POINT ( 'NONE', #50477 ) ;
#52977 = MECHANICAL_DESIGN_GEOMETRIC_PRESENTATION_REPRESENTATION (  '', ( #36117 ), #23738 ) ;
#52978 = DIRECTION ( 'NONE',  ( -0.000000000000000000, -0.000000000000000000, -1.000000000000000000 ) ) ;
#52979 = DIRECTION ( 'NONE',  ( 0.000000000000000000, 0.000000000000000000, 1.000000000000000000 ) ) ;
#52980 = EDGE_CURVE ( 'NONE', #31555, #28627, #54694, .T. ) ;
#52981 = UNCERTAINTY_MEASURE_WITH_UNIT (LENGTH_MEASURE( 1.000000000000000082E-05 ), #22403, 'distance_accuracy_value', 'NONE');
#52982 = CARTESIAN_POINT ( 'NONE',  ( -58.10499999999999687, -6.826472737025115478, 4.959722759717900331 ) ) ;
#52983 =( NAMED_UNIT ( * ) SI_UNIT ( $, .STERADIAN. ) SOLID_ANGLE_UNIT ( ) );
#52984 = MECHANICAL_DESIGN_GEOMETRIC_PRESENTATION_REPRESENTATION (  '', ( #9150 ), #40646 ) ;
#52985 = EDGE_CURVE ( 'NONE', #12752, #51919, #56687, .T. ) ;
#52986 = CARTESIAN_POINT ( 'NONE',  ( 5.598654528085805993, 160.3549999999999898, 7.705886871421374629 ) ) ;
#52987 = SURFACE_STYLE_FILL_AREA ( #36838 ) ;
#52988 = AXIS2_PLACEMENT_3D ( 'NONE', #32794, #17998, #21902 ) ;
#52989 = UNCERTAINTY_MEASURE_WITH_UNIT (LENGTH_MEASURE( 1.000000000000000082E-05 ), #64024, 'distance_accuracy_value', 'NONE');
#52990 = CARTESIAN_POINT ( 'NONE',  ( 41.50000000000001421, 26.00000000000000711, 23.99999999999998934 ) ) ;
#52991 = CARTESIAN_POINT ( 'NONE',  ( -18.25000000000000711, 33.74999999999999289, -4.000000000000000000 ) ) ;
#52992 = VECTOR ( 'NONE', #31561, 1000.000000000000000 ) ;
#52993 = DIRECTION ( 'NONE',  ( 0.000000000000000000, -1.000000000000000000, 0.000000000000000000 ) ) ;
#52994 = CARTESIAN_POINT ( 'NONE',  ( -32.56443198605217049, -8.762778093183483108, -2.500000000007921219 ) ) ;
#52995 = CIRCLE ( 'NONE', #27154, 0.5000000000000004441 ) ;
#52996 = EDGE_CURVE ( 'NONE', #46653, #29207, #12129, .T. ) ;
#52997 = SURFACE_SIDE_STYLE ('',( #31514 ) ) ;
#52998 = SURFACE_SIDE_STYLE ('',( #824 ) ) ;
#52999 = DIRECTION ( 'NONE',  ( 0.000000000000000000, -0.000000000000000000, 1.000000000000000000 ) ) ;
#53000 = DIRECTION ( 'NONE',  ( 0.000000000000000000, 1.000000000000000000, 0.000000000000000000 ) ) ;
#53001 = ORIENTED_EDGE ( 'NONE', *, *, #47798, .F. ) ;
#53002 = ORIENTED_EDGE ( 'NONE', *, *, #41490, .T. ) ;
#53003 = FACE_OUTER_BOUND ( 'NONE', #41871, .T. ) ;
#53004 = STYLED_ITEM ( 'NONE', ( #65447 ), #60410 ) ;
#53005 = CARTESIAN_POINT ( 'NONE',  ( 4.716976649647099507, 114.7570736234661553, -6.492361379858953008 ) ) ;
#53006 = AXIS2_PLACEMENT_3D ( 'NONE', #45941, #39984, #56461 ) ;
#53007 = AXIS2_PLACEMENT_3D ( 'NONE', #10759, #53655, #49441 ) ;
#53008 = PRESENTATION_STYLE_ASSIGNMENT (( #10098 ) ) ;
#53009 =( NAMED_UNIT ( * ) SI_UNIT ( $, .STERADIAN. ) SOLID_ANGLE_UNIT ( ) );
#53010 =( NAMED_UNIT ( * ) PLANE_ANGLE_UNIT ( ) SI_UNIT ( $, .RADIAN. ) );
#53011 = VERTEX_POINT ( 'NONE', #51177 ) ;
#53012 = COLOUR_RGB ( '', 0.09019608, 0.27058824, 0.51372549) ;
#53013 = EDGE_LOOP ( 'NONE', ( #3422, #35965, #22924, #19012 ) ) ;
#53014 = DIRECTION ( 'NONE',  ( 0.000000000000000000, -0.000000000000000000, 1.000000000000000000 ) ) ;
#53015 = DIRECTION ( 'NONE',  ( -0.000000000000000000, -1.000000000000000000, -0.000000000000000000 ) ) ;
#53016 = DIRECTION ( 'NONE',  ( 1.000000000000000000, 0.000000000000000000, -0.000000000000000000 ) ) ;
#53017 = ORIENTED_EDGE ( 'NONE', *, *, #38580, .F. ) ;
#53018 = CARTESIAN_POINT ( 'NONE',  ( -9.058813317711338797, 120.4549999999999983, 2.943386871421373563 ) ) ;
#53019 = EDGE_LOOP ( 'NONE', ( #51862, #38177 ) ) ;
#53020 =( GEOMETRIC_REPRESENTATION_CONTEXT ( 3 ) GLOBAL_UNCERTAINTY_ASSIGNED_CONTEXT ( ( #42764 ) ) GLOBAL_UNIT_ASSIGNED_CONTEXT ( ( #6882, #44227, #6191 ) ) REPRESENTATION_CONTEXT ( 'NONE', 'WORKASPACE' ) );
#53021 =( GEOMETRIC_REPRESENTATION_CONTEXT ( 3 ) GLOBAL_UNCERTAINTY_ASSIGNED_CONTEXT ( ( #66518 ) ) GLOBAL_UNIT_ASSIGNED_CONTEXT ( ( #38352, #1295, #17234 ) ) REPRESENTATION_CONTEXT ( 'NONE', 'WORKASPACE' ) );
#53022 = DIRECTION ( 'NONE',  ( 0.000000000000000000, 0.000000000000000000, -1.000000000000000000 ) ) ;
#53023 = CARTESIAN_POINT ( 'NONE',  ( -100.7950000000000017, 2.607480562269068880, -8.024999999999993250 ) ) ;
#53024 = VERTEX_POINT ( 'NONE', #18473 ) ;
#53025 = MECHANICAL_DESIGN_GEOMETRIC_PRESENTATION_REPRESENTATION (  '', ( #32787 ), #1273 ) ;
#53026 = CARTESIAN_POINT ( 'NONE',  ( 3.871746768188337740, 154.1452054115613350, -8.351915511153046978 ) ) ;
#53027 = LINE ( 'NONE', #37589, #40803 ) ;
#53028 = UNCERTAINTY_MEASURE_WITH_UNIT (LENGTH_MEASURE( 1.000000000000000082E-05 ), #57161, 'distance_accuracy_value', 'NONE');
#53029 = ORIENTED_EDGE ( 'NONE', *, *, #18036, .F. ) ;
#53030 = CARTESIAN_POINT ( 'NONE',  ( 2.607480562269076430, 155.7929263765337566, -8.025000000000000355 ) ) ;
#53031 = SURFACE_STYLE_USAGE ( .BOTH. , #31191 ) ;
#53032 = AXIS2_PLACEMENT_3D ( 'NONE', #23307, #33182, #32828 ) ;
#53033 = DIRECTION ( 'NONE',  ( -1.000000000000000000, -0.000000000000000000, -0.000000000000000000 ) ) ;
#53034 = AXIS2_PLACEMENT_3D ( 'NONE', #35315, #50446, #50119 ) ;
#53035 = CARTESIAN_POINT ( 'NONE',  ( 3.000000000000002665, 37.76051491742381216, -89.34202014332566932 ) ) ;
#53036 = ORIENTED_EDGE ( 'NONE', *, *, #41029, .T. ) ;
#53037 = CARTESIAN_POINT ( 'NONE',  ( 7.632228543268607446, 128.0429263765338135, 2.479861379858954606 ) ) ;
#53038 =( NAMED_UNIT ( * ) PLANE_ANGLE_UNIT ( ) SI_UNIT ( $, .RADIAN. ) );
#53039 = CARTESIAN_POINT ( 'NONE',  ( -32.87190215642332447, -9.152876382972353397, 4.262533829682994657 ) ) ;
#53040 = CARTESIAN_POINT ( 'NONE',  ( 32.00000000000001421, 14.00000000000000000, 34.49999999999998579 ) ) ;
#53041 =( LENGTH_UNIT ( ) NAMED_UNIT ( * ) SI_UNIT ( .MILLI., .METRE. ) );
#53042 = CIRCLE ( 'NONE', #3578, 15.00000000000000000 ) ;
#53043 = LINE ( 'NONE', #4837, #62064 ) ;
#53044 = FACE_OUTER_BOUND ( 'NONE', #6462, .T. ) ;
#53045 = LINE ( 'NONE', #69225, #55084 ) ;
#53046 = DIRECTION ( 'NONE',  ( -0.000000000000000000, -0.000000000000000000, 1.000000000000000000 ) ) ;
#53047 = EDGE_LOOP ( 'NONE', ( #21121, #42150 ) ) ;
#53048 = AXIS2_PLACEMENT_3D ( 'NONE', #12422, #51134, #7848 ) ;
#53049 = VERTEX_POINT ( 'NONE', #61360 ) ;
#53050 =( NAMED_UNIT ( * ) SI_UNIT ( $, .STERADIAN. ) SOLID_ANGLE_UNIT ( ) );
#53051 = CARTESIAN_POINT ( 'NONE',  ( -170.0070736234661410, -8.102448949553174629, -5.886773742842741797 ) ) ;
#53052 = DIRECTION ( 'NONE',  ( 0.000000000000000000, 0.000000000000000000, 1.000000000000000000 ) ) ;
#53053 = ORIENTED_EDGE ( 'NONE', *, *, #19136, .F. ) ;
#53054 = SURFACE_STYLE_USAGE ( .BOTH. , #5184 ) ;
#53055 = CARTESIAN_POINT ( 'NONE',  ( -165.9549999999999841, -7.632228543268599452, 2.479861379858951054 ) ) ;
#53056 = DIRECTION ( 'NONE',  ( 0.000000000000000000, 0.000000000000000000, -1.000000000000000000 ) ) ;
#53057 = CARTESIAN_POINT ( 'NONE',  ( -147.9570736234661581, 9.058813317711329915, -2.943386871421373119 ) ) ;
#53058 = EDGE_CURVE ( 'NONE', #4457, #11295, #33873, .T. ) ;
#53059 = CARTESIAN_POINT ( 'NONE',  ( -180.5949999999999704, 2.607480562269073321, 8.024999999999991473 ) ) ;
#53060 =( GEOMETRIC_REPRESENTATION_CONTEXT ( 3 ) GLOBAL_UNCERTAINTY_ASSIGNED_CONTEXT ( ( #15125 ) ) GLOBAL_UNIT_ASSIGNED_CONTEXT ( ( #41508, #10859, #43603 ) ) REPRESENTATION_CONTEXT ( 'NONE', 'WORKASPACE' ) );
#53061 = CARTESIAN_POINT ( 'NONE',  ( -170.3949999999999818, -6.826472737025113702, -4.959722759717900331 ) ) ;
#53062 = EDGE_LOOP ( 'NONE', ( #23914, #5071, #4901, #27647 ) ) ;
#53063 = CARTESIAN_POINT ( 'NONE',  ( -87.50000000000000000, -8.499999999999989342, 0.000000000000000000 ) ) ;
#53064 = AXIS2_PLACEMENT_3D ( 'NONE', #22224, #28146, #66156 ) ;
#53065 = CARTESIAN_POINT ( 'NONE',  ( -0.2278693232858663154, -2.499999999999997780, 9.000000000000003553 ) ) ;
#53066 = CARTESIAN_POINT ( 'NONE',  ( -10.25993137369353470, 11.89347840174322002, 1.624321976435927573 ) ) ;
#53067 = CARTESIAN_POINT ( 'NONE',  ( -81.80499999999996419, -8.437984349512085203, 5.166775262442717831E-16 ) ) ;
#53068 = DIRECTION ( 'NONE',  ( 1.000000000000000000, 0.000000000000000000, 0.000000000000000000 ) ) ;
#53069 = CARTESIAN_POINT ( 'NONE',  ( -168.6570736234661751, 9.058813317711329915, 2.943386871421369566 ) ) ;
#53070 = CIRCLE ( 'NONE', #10394, 5.500000000000005329 ) ;
#53071 = EDGE_CURVE ( 'NONE', #57942, #12184, #2334, .T. ) ;
#53072 = CARTESIAN_POINT ( 'NONE',  ( -90.89499999999999602, 6.826472737025115478, 4.959722759717899443 ) ) ;
#53073 = CARTESIAN_POINT ( 'NONE',  ( 3.094860106618431583, 124.2049999999999841, 9.525000000000000355 ) ) ;
#53074 = ADVANCED_FACE ( 'NONE', ( #30732 ), #46277, .T. ) ;
#53075 = CARTESIAN_POINT ( 'NONE',  ( 20.05205915161432628, 114.9999999999999858, -10.44837816993549495 ) ) ;
#53076 = CARTESIAN_POINT ( 'NONE',  ( -172.4070736234662604, 3.094860106616344808, -9.525000000001510259 ) ) ;
#53078 = EDGE_CURVE ( 'NONE', #16885, #58121, #10311, .T. ) ;
#53077 = COLOUR_RGB ( '', 0.40784314, 0.44705882, 0.49803922) ;
#53079 = CARTESIAN_POINT ( 'NONE',  ( 57.74999999999998579, 30.99999999999999289, -3.750000000000000000 ) ) ;
#53080 = UNCERTAINTY_MEASURE_WITH_UNIT (LENGTH_MEASURE( 1.000000000000000082E-05 ), #16989, 'distance_accuracy_value', 'NONE');
#53081 = CARTESIAN_POINT ( 'NONE',  ( -4.041451884327380562, -1.417096231345237545, -7.000000000000003553 ) ) ;
#53082 =( LENGTH_UNIT ( ) NAMED_UNIT ( * ) SI_UNIT ( .MILLI., .METRE. ) );
#53083 = EDGE_LOOP ( 'NONE', ( #44346, #65217, #52863, #58192 ) ) ;
#53084 = EDGE_CURVE ( 'NONE', #25644, #51899, #45589, .T. ) ;
#53085 = LINE ( 'NONE', #4876, #32516 ) ;
#53086 = EDGE_CURVE ( 'NONE', #28375, #35982, #68056, .T. ) ;
#53087 = PRESENTATION_LAYER_ASSIGNMENT (  '', '', ( #55280 ) ) ;
#53088 = AXIS2_PLACEMENT_3D ( 'NONE', #69148, #52968, #46699 ) ;
#53089 = CARTESIAN_POINT ( 'NONE',  ( 32.00000000000001421, 15.00000000000000000, 36.49999999999999289 ) ) ;
#53090 = ORIENTED_EDGE ( 'NONE', *, *, #55402, .T. ) ;
#53091 = EDGE_LOOP ( 'NONE', ( #54109, #6932, #46895, #36284 ) ) ;
#53092 = CARTESIAN_POINT ( 'NONE',  ( -15.00000000000000000, -10.90871211463571200, 5.000000000000000000 ) ) ;
#53093 = CARTESIAN_POINT ( 'NONE',  ( -175.4070736234663173, 3.094860106616942108, -9.525000000001076828 ) ) ;
#53094 = UNCERTAINTY_MEASURE_WITH_UNIT (LENGTH_MEASURE( 1.000000000000000082E-05 ), #61105, 'distance_accuracy_value', 'NONE');
#53095 = TOROIDAL_SURFACE ( 'NONE', #62052, 18.99999999999998934, 1.000000000000000000 ) ;
#53096 = DIRECTION ( 'NONE',  ( 0.000000000000000000, 0.000000000000000000, -1.000000000000000000 ) ) ;
#53097 = SURFACE_SIDE_STYLE ('',( #11202 ) ) ;
#53098 = CIRCLE ( 'NONE', #32917, 0.5000000000000006661 ) ;
#53099 = CARTESIAN_POINT ( 'NONE',  ( 51.99999999999998579, 1.797044900979284448E-15, 10.50000000000000000 ) ) ;
#53100 = CARTESIAN_POINT ( 'NONE',  ( -8.021777294149472937, -2.499999999999994227, 4.105874159530730871 ) ) ;
#53101 = ORIENTED_EDGE ( 'NONE', *, *, #64031, .T. ) ;
#53102 = CARTESIAN_POINT ( 'NONE',  ( -121.1050000000000040, -6.826472737025113702, 4.959722759717902107 ) ) ;
#53103 = VERTEX_POINT ( 'NONE', #39955 ) ;
#53104 = PRESENTATION_STYLE_ASSIGNMENT (( #47165 ) ) ;
#53105 = DIRECTION ( 'NONE',  ( -1.000000000000000000, -0.000000000000000000, -0.000000000000000000 ) ) ;
#53106 = ORIENTED_EDGE ( 'NONE', *, *, #64017, .F. ) ;
#53107 = CARTESIAN_POINT ( 'NONE',  ( 59.00000000000000000, 11.99999999999999822, -3.499999999999999556 ) ) ;
#53108 = ORIENTED_EDGE ( 'NONE', *, *, #20171, .F. ) ;
#53109 = TOROIDAL_SURFACE ( 'NONE', #17225, 13.49999999999999822, 0.5000000000000000000 ) ;
#53110 = CIRCLE ( 'NONE', #41949, 0.9999999999999997780 ) ;
#53111 = DIRECTION ( 'NONE',  ( -1.000000000000000000, -0.000000000000000000, -0.000000000000000000 ) ) ;
#53112 = CARTESIAN_POINT ( 'NONE',  ( 8.102448949553183510, 153.9950000000000045, -5.886773742842746238 ) ) ;
#53113 = ORIENTED_EDGE ( 'NONE', *, *, #12536, .T. ) ;
#53114 = MECHANICAL_DESIGN_GEOMETRIC_PRESENTATION_REPRESENTATION (  '', ( #47532 ), #13788 ) ;
#53115 = CARTESIAN_POINT ( 'NONE',  ( 5.598654528085805993, 148.3549999999999898, 7.705886871421374629 ) ) ;
#53116 = PRESENTATION_STYLE_ASSIGNMENT (( #53776 ) ) ;
#53117 = CARTESIAN_POINT ( 'NONE',  ( -130.1929263765337907, -10.01517768586948698, 6.132527647946031529E-16 ) ) ;
#53118 = VERTEX_POINT ( 'NONE', #52236 ) ;
#53119 = CARTESIAN_POINT ( 'NONE',  ( 7.632228543268608334, 122.3429263765338249, -2.479861379858951942 ) ) ;
#53120 = DIRECTION ( 'NONE',  ( -1.000000000000000000, -0.000000000000000000, -0.000000000000000000 ) ) ;
#53121 = UNCERTAINTY_MEASURE_WITH_UNIT (LENGTH_MEASURE( 1.000000000000000082E-05 ), #67493, 'distance_accuracy_value', 'NONE');
#53122 = FACE_OUTER_BOUND ( 'NONE', #50433, .T. ) ;
#53123 = MECHANICAL_DESIGN_GEOMETRIC_PRESENTATION_REPRESENTATION (  '', ( #261 ), #56456 ) ;
#53124 = CARTESIAN_POINT ( 'NONE',  ( -98.39292637653380780, 8.102448949553176405, 5.886773742842740909 ) ) ;
#53125 = LINE ( 'NONE', #48566, #42277 ) ;
#53126 = VERTEX_POINT ( 'NONE', #13515 ) ;
#53127 = AXIS2_PLACEMENT_3D ( 'NONE', #64698, #64340, #26349 ) ;
#53128 = FACE_OUTER_BOUND ( 'NONE', #10893, .T. ) ;
#53129 = ORIENTED_EDGE ( 'NONE', *, *, #17662, .F. ) ;
#53130 = CARTESIAN_POINT ( 'NONE',  ( -53.84292637653378932, 9.058813317711329915, -2.943386871421373119 ) ) ;
#53131 = CARTESIAN_POINT ( 'NONE',  ( 0.000000000000000000, -2.500000000000000000, 0.000000000000000000 ) ) ;
#53132 = CARTESIAN_POINT ( 'NONE',  ( -5.705565085145812176, -4.117671386636407860, 0.02778322089669425093 ) ) ;
#53133 = CARTESIAN_POINT ( 'NONE',  ( -150.2049999999999841, -2.607480562269071545, -8.024999999999991473 ) ) ;
#53134 = STYLED_ITEM ( 'NONE', ( #16299 ), #35839 ) ;
#53135 = UNCERTAINTY_MEASURE_WITH_UNIT (LENGTH_MEASURE( 1.000000000000000082E-05 ), #36484, 'distance_accuracy_value', 'NONE');
#53136 = PRESENTATION_LAYER_ASSIGNMENT (  '', '', ( #44182 ) ) ;
#53137 = CARTESIAN_POINT ( 'NONE',  ( 44.99999999999998579, 119.9999999999999716, 10.00000000000000000 ) ) ;
#53138 = DIRECTION ( 'NONE',  ( 0.000000000000000000, 0.000000000000000000, -1.000000000000000000 ) ) ;
#53139 = DIRECTION ( 'NONE',  ( 0.000000000000000000, 0.000000000000000000, -1.000000000000000000 ) ) ;
#53140 = ORIENTED_EDGE ( 'NONE', *, *, #53690, .T. ) ;
#53141 = ORIENTED_EDGE ( 'NONE', *, *, #45557, .T. ) ;
#53142 = CARTESIAN_POINT ( 'NONE',  ( 22.91109586540972032, 27.27678992330844920, 27.25908479965321263 ) ) ;
#53143 = DIRECTION ( 'NONE',  ( -1.000000000000000000, 0.000000000000000000, 0.000000000000000000 ) ) ;
#53144 = COLOUR_RGB ( '', 0.08235294, 0.09019608, 0.10196078) ;
#53145 = CARTESIAN_POINT ( 'NONE',  ( -66.05499999999999261, -9.827790563157499189E-16, -8.024999999999991473 ) ) ;
#53146 = VERTEX_POINT ( 'NONE', #57124 ) ;
#53147 = CARTESIAN_POINT ( 'NONE',  ( -26.79538245034556709, -8.499999999999996447, 1.000000000000000000 ) ) ;
#53148 = ADVANCED_FACE ( 'NONE', ( #34986 ), #19132, .F. ) ;
#53149 = CARTESIAN_POINT ( 'NONE',  ( -55.00000000000000000, -2.024042244987997205E-14, 11.50000000000003020 ) ) ;
#53150 = DIRECTION ( 'NONE',  ( 0.000000000000000000, 0.000000000000000000, -1.000000000000000000 ) ) ;
#53152 = EDGE_CURVE ( 'NONE', #32986, #24001, #56878, .T. ) ;
#53151 = ORIENTED_EDGE ( 'NONE', *, *, #37464, .T. ) ;
#53153 = AXIS2_PLACEMENT_3D ( 'NONE', #49248, #64727, #42976 ) ;
#53154 = DIRECTION ( 'NONE',  ( -0.000000000000000000, -1.000000000000000000, -0.000000000000000000 ) ) ;
#53155 = SURFACE_STYLE_FILL_AREA ( #37360 ) ;
#53156 = FILL_AREA_STYLE ('',( #20441 ) ) ;
#53157 = DIRECTION ( 'NONE',  ( 0.000000000000000000, 0.000000000000000000, 1.000000000000000000 ) ) ;
#53158 = EDGE_CURVE ( 'NONE', #16845, #10966, #56088, .T. ) ;
#53159 = CARTESIAN_POINT ( 'NONE',  ( -119.9949999999999903, -6.826472737025113702, 4.959722759717902107 ) ) ;
#53160 = CARTESIAN_POINT ( 'NONE',  ( -3.094860106618432471, 151.5949999999999989, -9.525000000000000355 ) ) ;
#53161 = CARTESIAN_POINT ( 'NONE',  ( -87.29500000000000171, -2.607480562269069768, 8.024999999999991473 ) ) ;
#53162 = EDGE_CURVE ( 'NONE', #22486, #23656, #58616, .T. ) ;
#53163 = CARTESIAN_POINT ( 'NONE',  ( 12.34222745343792127, 115.4999999999999574, 10.18181818181818166 ) ) ;
#53164 = CIRCLE ( 'NONE', #19397, 1.000000000000000888 ) ;
#53165 = FACE_OUTER_BOUND ( 'NONE', #63212, .T. ) ;
#53166 = UNCERTAINTY_MEASURE_WITH_UNIT (LENGTH_MEASURE( 1.000000000000000082E-05 ), #69092, 'distance_accuracy_value', 'NONE');
#53167 = FACE_OUTER_BOUND ( 'NONE', #38287, .T. ) ;
#53168 = CIRCLE ( 'NONE', #16123, 1.000000000000000888 ) ;
#53169 = ORIENTED_EDGE ( 'NONE', *, *, #51076, .F. ) ;
#53170 = EDGE_CURVE ( 'NONE', #6589, #26613, #51881, .T. ) ;
#53171 = CARTESIAN_POINT ( 'NONE',  ( -136.3429263765337964, -9.058813317711329915, 2.943386871421371787 ) ) ;
#53172 = CARTESIAN_POINT ( 'NONE',  ( -37.50000000000000000, 58.31681314173471975, 6.349999999999996092 ) ) ;
#53173 = CARTESIAN_POINT ( 'NONE',  ( -151.0449999999999875, 7.632228543268600340, 2.479861379858949277 ) ) ;
#53174 = CARTESIAN_POINT ( 'NONE',  ( -0.7098155475105580869, 7.000000000000003553, 0.02753250691854559548 ) ) ;
#53175 = COLOUR_RGB ( '', 0.40784314, 0.44705882, 0.49803922) ;
#53176 = FACE_OUTER_BOUND ( 'NONE', #68326, .T. ) ;
#53177 = VERTEX_POINT ( 'NONE', #8612 ) ;
#53178 = ORIENTED_EDGE ( 'NONE', *, *, #69683, .T. ) ;
#53179 = PRESENTATION_LAYER_ASSIGNMENT (  '', '', ( #13849 ) ) ;
#53180 = CARTESIAN_POINT ( 'NONE',  ( 60.99999999999998579, 50.00000000000000000, -7.000000000000000000 ) ) ;
#53181 = AXIS2_PLACEMENT_3D ( 'NONE', #39045, #12250, #28064 ) ;
#53182 = AXIS2_PLACEMENT_3D ( 'NONE', #67529, #18658, #28838 ) ;
#53183 = CARTESIAN_POINT ( 'NONE',  ( -4.716976649647097730, 117.2429263765338163, -6.492361379858953896 ) ) ;
#53184 = CARTESIAN_POINT ( 'NONE',  ( -7.499999999999999112, 6.123233995736765296E-16, -4.999999999999999112 ) ) ;
#53185 = DIRECTION ( 'NONE',  ( 0.000000000000000000, 0.000000000000000000, -1.000000000000000000 ) ) ;
#53186 = CARTESIAN_POINT ( 'NONE',  ( 0.000000000000000000, 36.75000000000000000, 3.750000000000000000 ) ) ;
#53187 = TOROIDAL_SURFACE ( 'NONE', #11593, 14.49999999999999822, 0.5000000000000000000 ) ;
#53188 = ORIENTED_EDGE ( 'NONE', *, *, #40293, .F. ) ;
#53189 = CARTESIAN_POINT ( 'NONE',  ( -154.5550000000000068, 0.000000000000000000, 8.024999999999991473 ) ) ;
#53190 = CIRCLE ( 'NONE', #52099, 0.5000000000000004441 ) ;
#53191 = ORIENTED_EDGE ( 'NONE', *, *, #66881, .T. ) ;
#53192 = CARTESIAN_POINT ( 'NONE',  ( -195.0000000000000000, 1.166476076187852838E-15, -9.524999999999991473 ) ) ;
#53193 = FILL_AREA_STYLE ('',( #43022 ) ) ;
#53194 = ORIENTED_EDGE ( 'NONE', *, *, #49397, .F. ) ;
#53195 = DIRECTION ( 'NONE',  ( -1.000000000000000000, -0.000000000000000000, -0.000000000000000000 ) ) ;
#53196 = FACE_OUTER_BOUND ( 'NONE', #36807, .T. ) ;
#53197 = CARTESIAN_POINT ( 'NONE',  ( -9.058813317711337021, 119.0449999999999875, -2.943386871421374895 ) ) ;
#53198 = CARTESIAN_POINT ( 'NONE',  ( 0.08961394468541400427, 42.48853604202994916, -74.70442749311222030 ) ) ;
#53199 = EDGE_CURVE ( 'NONE', #1408, #49241, #40635, .T. ) ;
#53200 = VECTOR ( 'NONE', #23207, 1000.000000000000000 ) ;
#53201 = EDGE_LOOP ( 'NONE', ( #34809, #19524, #26118, #61915 ) ) ;
#53202 =( GEOMETRIC_REPRESENTATION_CONTEXT ( 3 ) GLOBAL_UNCERTAINTY_ASSIGNED_CONTEXT ( ( #25676 ) ) GLOBAL_UNIT_ASSIGNED_CONTEXT ( ( #28297, #11805, #44566 ) ) REPRESENTATION_CONTEXT ( 'NONE', 'WORKASPACE' ) );
#53203 =( NAMED_UNIT ( * ) SI_UNIT ( $, .STERADIAN. ) SOLID_ANGLE_UNIT ( ) );
#53204 = CARTESIAN_POINT ( 'NONE',  ( 3.094860106618431583, 124.2049999999999841, 9.525000000000000355 ) ) ;
#53205 = CARTESIAN_POINT ( 'NONE',  ( -63.95499999999998408, -7.632228543268599452, 2.479861379858951054 ) ) ;
#53206 = LINE ( 'NONE', #69375, #23944 ) ;
#53207 = VERTEX_POINT ( 'NONE', #24086 ) ;
#53208 = CARTESIAN_POINT ( 'NONE',  ( 3.094860106618435136, 146.4050000000000011, -9.525000000000000355 ) ) ;
#53209 = UNCERTAINTY_MEASURE_WITH_UNIT (LENGTH_MEASURE( 1.000000000000000082E-05 ), #9470, 'distance_accuracy_value', 'NONE');
#53210 = DIRECTION ( 'NONE',  ( -1.000000000000000000, 0.000000000000000000, 0.000000000000000000 ) ) ;
#53211 = CARTESIAN_POINT ( 'NONE',  ( 10.00000000000002309, 43.00000000000000000, 90.00000000000000000 ) ) ;
#53212 = CARTESIAN_POINT ( 'NONE',  ( 13.75000000000000355, 28.24999999999998934, -3.750000000000000000 ) ) ;
#53213 = DIRECTION ( 'NONE',  ( -0.000000000000000000, -0.000000000000000000, -1.000000000000000000 ) ) ;
#53214 = VERTEX_POINT ( 'NONE', #62045 ) ;
#53215 = AXIS2_PLACEMENT_3D ( 'NONE', #52749, #4522, #32304 ) ;
#53216 = LINE ( 'NONE', #26457, #68844 ) ;
#53217 = CARTESIAN_POINT ( 'NONE',  ( -180.5049999999999670, -6.826472737025115478, -4.959722759717899443 ) ) ;
#53218 = ORIENTED_EDGE ( 'NONE', *, *, #37853, .T. ) ;
#53219 = CARTESIAN_POINT ( 'NONE',  ( -87.35707362346617799, 5.598654528085804216, 7.705886871421366635 ) ) ;
#53220 = VECTOR ( 'NONE', #28160, 1000.000000000000000 ) ;
#53221 = LINE ( 'NONE', #47644, #66065 ) ;
#53222 = SURFACE_STYLE_FILL_AREA ( #57801 ) ;
#53223 = ORIENTED_EDGE ( 'NONE', *, *, #577, .F. ) ;
#53224 =( LENGTH_UNIT ( ) NAMED_UNIT ( * ) SI_UNIT ( .MILLI., .METRE. ) );
#53225 = EDGE_LOOP ( 'NONE', ( #14123, #15505, #45939, #47509 ) ) ;
#53226 = EDGE_CURVE ( 'NONE', #9250, #66411, #67008, .T. ) ;
#53227 = CYLINDRICAL_SURFACE ( 'NONE', #68491, 0.5000000000000004441 ) ;
#53228 = CARTESIAN_POINT ( 'NONE',  ( -96.65499999999998693, -7.632228543268600340, -2.479861379858950166 ) ) ;
#53230 = ORIENTED_EDGE ( 'NONE', *, *, #15492, .T. ) ;
#53229 = AXIS2_PLACEMENT_3D ( 'NONE', #5727, #16346, #32458 ) ;
#53231 = EDGE_CURVE ( 'NONE', #56901, #1286, #61689, .T. ) ;
#53232 = FILL_AREA_STYLE_COLOUR ( '', #20448 ) ;
#53233 = CARTESIAN_POINT ( 'NONE',  ( -128.3070736234661524, -10.01517768586948698, 6.132527647946031529E-16 ) ) ;
#53234 =( NAMED_UNIT ( * ) SI_UNIT ( $, .STERADIAN. ) SOLID_ANGLE_UNIT ( ) );
#53235 = CARTESIAN_POINT ( 'NONE',  ( 5.598654528085809545, 151.1449999999999818, -7.705886871421373741 ) ) ;
#53236 = CARTESIAN_POINT ( 'NONE',  ( -61.85707362346616378, -5.598654528085803328, -7.705886871421366635 ) ) ;
#53237 = AXIS2_PLACEMENT_3D ( 'NONE', #65994, #32961, #59309 ) ;
#53238 = EDGE_CURVE ( 'NONE', #31454, #27359, #14944, .T. ) ;
#53239 = FILL_AREA_STYLE ('',( #48682 ) ) ;
#53240 = PRESENTATION_LAYER_ASSIGNMENT (  '', '', ( #42029 ) ) ;
#53241 = VERTEX_POINT ( 'NONE', #4701 ) ;
#53242 = SURFACE_STYLE_USAGE ( .BOTH. , #5356 ) ;
#53243 = FILL_AREA_STYLE ('',( #27153 ) ) ;
#53245 = CARTESIAN_POINT ( 'NONE',  ( 1.000000000000000888, 1.224646799147365780E-16, 4.000000000000000000 ) ) ;
#53244 = CYLINDRICAL_SURFACE ( 'NONE', #58294, 5.000000000000004441 ) ;
#53246 = CIRCLE ( 'NONE', #16048, 0.5000000000000004441 ) ;
#53247 = AXIS2_PLACEMENT_3D ( 'NONE', #35774, #42148, #46006 ) ;
#53248 = CARTESIAN_POINT ( 'NONE',  ( -114.2049999999999699, -2.607480562269071545, -8.024999999999991473 ) ) ;
#53249 = CARTESIAN_POINT ( 'NONE',  ( 10.01517768586949231, 120.6949999999999790, 1.839758294383810543E-15 ) ) ;
#53250 = CARTESIAN_POINT ( 'NONE',  ( -114.7449999999999903, 4.716976649647094177, 6.492361379858945902 ) ) ;
#53251 = ADVANCED_FACE ( 'NONE', ( #58181 ), #46977, .T. ) ;
#53252 = CIRCLE ( 'NONE', #3784, 3.499999999999999556 ) ;
#53253 = DIRECTION ( 'NONE',  ( -0.000000000000000000, -0.000000000000000000, -1.000000000000000000 ) ) ;
#53254 = TOROIDAL_SURFACE ( 'NONE', #52157, 0.7500000000000000000, 0.2500000000000000000 ) ;
#53255 = CYLINDRICAL_SURFACE ( 'NONE', #17763, 0.5000000000000004441 ) ;
#53256 = AXIS2_PLACEMENT_3D ( 'NONE', #59773, #38371, #58746 ) ;
#53257 = ORIENTED_EDGE ( 'NONE', *, *, #50517, .F. ) ;
#53258 = EDGE_CURVE ( 'NONE', #33018, #32747, #9999, .T. ) ;
#53259 = CARTESIAN_POINT ( 'NONE',  ( -162.1429263765338362, 5.598654528085800663, -7.705886871421367523 ) ) ;
#53260 = FACE_OUTER_BOUND ( 'NONE', #45149, .T. ) ;
#53261 = PRESENTATION_LAYER_ASSIGNMENT (  '', '', ( #27346 ) ) ;
#53262 = DIRECTION ( 'NONE',  ( 0.000000000000000000, 1.000000000000000000, 0.000000000000000000 ) ) ;
#53264 = DIRECTION ( 'NONE',  ( -0.000000000000000000, 1.000000000000000000, -0.000000000000000000 ) ) ;
#53263 = AXIS2_PLACEMENT_3D ( 'NONE', #31879, #5143, #26587 ) ;
#53265 = SURFACE_STYLE_USAGE ( .BOTH. , #32133 ) ;
#53266 = FILL_AREA_STYLE_COLOUR ( '', #28280 ) ;
#53267 = ORIENTED_EDGE ( 'NONE', *, *, #33357, .T. ) ;
#53268 = CARTESIAN_POINT ( 'NONE',  ( -74.54292637653379927, 9.058813317711329915, 2.943386871421369566 ) ) ;
#53269 = DIRECTION ( 'NONE',  ( 0.9704308468600219006, 0.2413793103448194921, 0.000000000000000000 ) ) ;
#53270 = CARTESIAN_POINT ( 'NONE',  ( 48.81081081081080697, 14.09971791521132900, 9.500000000000000000 ) ) ;
#53271 = DIRECTION ( 'NONE',  ( -0.7681514953298232973, 0.000000000000000000, 0.6402681315062906942 ) ) ;
#53272 = DIRECTION ( 'NONE',  ( 0.000000000000000000, 0.000000000000000000, -1.000000000000000000 ) ) ;
#53273 = CARTESIAN_POINT ( 'NONE',  ( -178.1049999999999613, -6.826472737025113702, 4.959722759717902107 ) ) ;
#53274 = ORIENTED_EDGE ( 'NONE', *, *, #12713, .F. ) ;
#53275 = CARTESIAN_POINT ( 'NONE',  ( -74.50000000000000000, 36.50926243676796190, -10.00000000000000000 ) ) ;
#53276 = CARTESIAN_POINT ( 'NONE',  ( -181.7070736234662149, -3.094860106618727347, -9.524999999999778311 ) ) ;
#53277 = CARTESIAN_POINT ( 'NONE',  ( -7.632228543268608334, 145.9570736234661581, 2.479861379858952830 ) ) ;
#53278 = AXIS2_PLACEMENT_3D ( 'NONE', #25853, #10044, #57530 ) ;
#53279 = EDGE_CURVE ( 'NONE', #11259, #62586, #123, .T. ) ;
#53280 = EDGE_LOOP ( 'NONE', ( #21877, #24952, #43275, #33960, #55282, #764 ) ) ;
#53281 = CARTESIAN_POINT ( 'NONE',  ( 34.99999999999992895, 109.9999999999999858, 10.00000000000000000 ) ) ;
#53282 = CARTESIAN_POINT ( 'NONE',  ( -96.65499999999998693, -7.632228543268600340, -2.479861379858950166 ) ) ;
#53283 = MECHANICAL_DESIGN_GEOMETRIC_PRESENTATION_REPRESENTATION (  '', ( #13951 ), #25147 ) ;
#53284 = UNCERTAINTY_MEASURE_WITH_UNIT (LENGTH_MEASURE( 1.000000000000000082E-05 ), #23336, 'distance_accuracy_value', 'NONE');
#53285 = ORIENTED_EDGE ( 'NONE', *, *, #27475, .F. ) ;
#53286 = CARTESIAN_POINT ( 'NONE',  ( 23.21231517720797655, 117.4999999999999716, 7.500000000000000000 ) ) ;
#53287 = CYLINDRICAL_SURFACE ( 'NONE', #18152, 1.000000000000000888 ) ;
#53288 = CYLINDRICAL_SURFACE ( 'NONE', #38939, 22.00000000000001421 ) ;
#53289 = DIRECTION ( 'NONE',  ( -0.7071067811865425767, 0.000000000000000000, -0.7071067811865525687 ) ) ;
#53290 = ORIENTED_EDGE ( 'NONE', *, *, #45998, .F. ) ;
#53291 = DIRECTION ( 'NONE',  ( -0.000000000000000000, -0.000000000000000000, 1.000000000000000000 ) ) ;
#53292 = CARTESIAN_POINT ( 'NONE',  ( -69.74499999999999034, 4.716976649647094177, 6.492361379858945902 ) ) ;
#53293 = ORIENTED_EDGE ( 'NONE', *, *, #50050, .T. ) ;
#53294 = CARTESIAN_POINT ( 'NONE',  ( -75.75000000000000000, -3.000000000000000000, 19.00000000000000000 ) ) ;
#53295 = CIRCLE ( 'NONE', #40970, 1.000000000000000888 ) ;
#53296 = PRODUCT_DEFINITION ( 'UNKNOWN', '', #50630, #2925 ) ;
#53297 = AXIS2_PLACEMENT_3D ( 'NONE', #45024, #38715, #60449 ) ;
#53298 = EDGE_CURVE ( 'NONE', #22897, #5819, #39544, .T. ) ;
#53299 = CARTESIAN_POINT ( 'NONE',  ( -121.1070736234661922, 8.102448949553172852, -5.886773742842744461 ) ) ;
#53300 = CARTESIAN_POINT ( 'NONE',  ( -125.0070736234661979, -8.102448949553174629, -5.886773742842741797 ) ) ;
#53301 = ADVANCED_FACE ( 'NONE', ( #64136 ), #48353, .T. ) ;
#53302 = ORIENTED_EDGE ( 'NONE', *, *, #1303, .F. ) ;
#53303 = LINE ( 'NONE', #25499, #65051 ) ;
#53304 = PRESENTATION_STYLE_ASSIGNMENT (( #42784 ) ) ;
#53305 = ADVANCED_FACE ( 'NONE', ( #15633 ), #52910, .F. ) ;
#53307 =( NAMED_UNIT ( * ) PLANE_ANGLE_UNIT ( ) SI_UNIT ( $, .RADIAN. ) );
#53306 = TOROIDAL_SURFACE ( 'NONE', #7247, 13.49999999999999822, 0.5000000000000000000 ) ;
#53308 = DIRECTION ( 'NONE',  ( 0.000000000000000000, -0.000000000000000000, 1.000000000000000000 ) ) ;
#53309 = ORIENTED_EDGE ( 'NONE', *, *, #66111, .F. ) ;
#53310 = EDGE_CURVE ( 'NONE', #19358, #50943, #65368, .T. ) ;
#53311 = DIRECTION ( 'NONE',  ( -9.376883653928687363E-17, 1.000000000000000000, -0.000000000000000000 ) ) ;
#53312 = ORIENTED_EDGE ( 'NONE', *, *, #10343, .F. ) ;
#53313 = LINE ( 'NONE', #42795, #25460 ) ;
#53314 = CIRCLE ( 'NONE', #54379, 1.000000000000000888 ) ;
#53315 = AXIS2_PLACEMENT_3D ( 'NONE', #756, #20923, #37494 ) ;
#53316 = CARTESIAN_POINT ( 'NONE',  ( -162.2070736234661865, 3.094860106618433360, 9.524999999999991473 ) ) ;
#53317 = CARTESIAN_POINT ( 'NONE',  ( 9.058813317711337021, 120.5449999999999875, 2.943386871421375783 ) ) ;
#53318 = CARTESIAN_POINT ( 'NONE',  ( -91.40707362346616094, 3.094860106618428031, -9.524999999999993250 ) ) ;
#53319 = EDGE_CURVE ( 'NONE', #39971, #23974, #54615, .T. ) ;
#53320 = CARTESIAN_POINT ( 'NONE',  ( 40.99999999999998579, 107.7459666924148252, -3.499999999999999556 ) ) ;
#53321 = VERTEX_POINT ( 'NONE', #34214 ) ;
#53322 = CARTESIAN_POINT ( 'NONE',  ( -44.99999999999977973, 146.9999999999999716, 7.500000000000000000 ) ) ;
#53323 = ADVANCED_FACE ( 'NONE', ( #33514 ), #22268, .T. ) ;
#53325 = FACE_BOUND ( 'NONE', #68171, .T. ) ;
#53324 = LINE ( 'NONE', #10748, #62648 ) ;
#53326 = DIRECTION ( 'NONE',  ( 0.000000000000000000, 0.000000000000000000, -1.000000000000000000 ) ) ;
#53327 = CIRCLE ( 'NONE', #20722, 1.000000000000000888 ) ;
#53328 = CARTESIAN_POINT ( 'NONE',  ( -137.7549999999999955, 4.716976649647091513, -6.492361379858946790 ) ) ;
#53329 = DIRECTION ( 'NONE',  ( -0.000000000000000000, -1.000000000000000000, 0.000000000000000000 ) ) ;
#53330 = DIRECTION ( 'NONE',  ( -0.000000000000000000, 1.000000000000000000, -0.000000000000000000 ) ) ;
#53331 = CARTESIAN_POINT ( 'NONE',  ( -158.8449999999999989, -7.632228543268599452, 2.479861379858951054 ) ) ;
#53332 = AXIS2_PLACEMENT_3D ( 'NONE', #24052, #66624, #33565 ) ;
#53333 = CARTESIAN_POINT ( 'NONE',  ( -141.4449999999999932, 0.000000000000000000, 8.024999999999991473 ) ) ;
#53334 = ORIENTED_EDGE ( 'NONE', *, *, #13091, .F. ) ;
#53335 = CARTESIAN_POINT ( 'NONE',  ( -180.0570736234661808, 0.000000000000000000, 9.524999999999991473 ) ) ;
#53336 = DIRECTION ( 'NONE',  ( -0.000000000000000000, -0.000000000000000000, 1.000000000000000000 ) ) ;
#53337 = FILL_AREA_STYLE ('',( #4402 ) ) ;
#53338 = MECHANICAL_DESIGN_GEOMETRIC_PRESENTATION_REPRESENTATION (  '', ( #31964 ), #48840 ) ;
#53339 = CARTESIAN_POINT ( 'NONE',  ( -56.15499999999997982, 7.632228543268600340, 2.479861379858949277 ) ) ;
#53340 = SURFACE_STYLE_USAGE ( .BOTH. , #48782 ) ;
#53341 = FACE_OUTER_BOUND ( 'NONE', #5908, .T. ) ;
#53342 = CYLINDRICAL_SURFACE ( 'NONE', #33188, 8.000000000000014211 ) ;
#53343 = CARTESIAN_POINT ( 'NONE',  ( -5.196152422706636465, -1.107695154586737063, 9.000000000000001776 ) ) ;
#53344 = EDGE_CURVE ( 'NONE', #38783, #20552, #29407, .T. ) ;
#53345 = DIRECTION ( 'NONE',  ( -1.000000000000000000, -1.010476424756490132E-16, -2.775557561562891351E-17 ) ) ;
#53346 = AXIS2_PLACEMENT_3D ( 'NONE', #67154, #18942, #55906 ) ;
#53347 = CARTESIAN_POINT ( 'NONE',  ( 0.000000000000000000, 33.74999999999999289, 3.750000000000000000 ) ) ;
#53348 = CARTESIAN_POINT ( 'NONE',  ( -89.15707362346617515, -9.058813317711329915, -2.943386871421370898 ) ) ;
#53349 = CARTESIAN_POINT ( 'NONE',  ( 57.00000000000000000, 16.00000000000000000, -60.00402776293825724 ) ) ;
#53350 = MECHANICAL_DESIGN_GEOMETRIC_PRESENTATION_REPRESENTATION (  '', ( #41017 ), #15170 ) ;
#53351 = CYLINDRICAL_SURFACE ( 'NONE', #42043, 1.000000000000000000 ) ;
#53352 = CYLINDRICAL_SURFACE ( 'NONE', #16071, 8.000000000000014211 ) ;
#53354 = ORIENTED_EDGE ( 'NONE', *, *, #65439, .T. ) ;
#53353 = STYLED_ITEM ( 'NONE', ( #53104 ), #48973 ) ;
#53355 = AXIS2_PLACEMENT_3D ( 'NONE', #61512, #66113, #7035 ) ;
#53356 = CARTESIAN_POINT ( 'NONE',  ( 7.399999999999989697, 11.99999999999999289, -4.000000000000000000 ) ) ;
#53357 = CARTESIAN_POINT ( 'NONE',  ( -7.632228543268608334, 112.9570736234661581, 2.479861379858952830 ) ) ;
#53358 = CARTESIAN_POINT ( 'NONE',  ( -20.77797364267480518, 115.1388508835393907, 10.00000000000000000 ) ) ;
#53359 = DIRECTION ( 'NONE',  ( 1.000000000000000000, 0.000000000000000000, -0.000000000000000000 ) ) ;
#53360 =( LENGTH_UNIT ( ) NAMED_UNIT ( * ) SI_UNIT ( .MILLI., .METRE. ) );
#53361 = ORIENTED_EDGE ( 'NONE', *, *, #17349, .T. ) ;
#53362 = VERTEX_POINT ( 'NONE', #22619 ) ;
#53363 = CARTESIAN_POINT ( 'NONE',  ( 7.999999999999998224, 5.000000000000000000, -37.00402776293825724 ) ) ;
#53364 = DIRECTION ( 'NONE',  ( 0.000000000000000000, 0.000000000000000000, -1.000000000000000000 ) ) ;
#53365 = VERTEX_POINT ( 'NONE', #6427 ) ;
#53366 = CARTESIAN_POINT ( 'NONE',  ( 5.598654528085809545, 122.2549999999999955, -7.705886871421373741 ) ) ;
#53367 = CARTESIAN_POINT ( 'NONE',  ( 3.109477999331718312, 1.987149502472170370, -9.000000000000005329 ) ) ;
#53368 = ORIENTED_EDGE ( 'NONE', *, *, #55366, .T. ) ;
#53369 = TOROIDAL_SURFACE ( 'NONE', #62345, 13.50000000000000178, 0.5000000000000000000 ) ;
#53370 = CARTESIAN_POINT ( 'NONE',  ( 66.24999999999998579, 33.74999999999999289, -4.000000000000000000 ) ) ;
#53371 = CARTESIAN_POINT ( 'NONE',  ( -98.69499999999999318, -8.437984349512085203, 5.166775262442717831E-16 ) ) ;
#53372 = ORIENTED_EDGE ( 'NONE', *, *, #65370, .F. ) ;
#53373 = AXIS2_PLACEMENT_3D ( 'NONE', #57779, #40927, #45845 ) ;
#53374 = DIRECTION ( 'NONE',  ( 0.000000000000000000, 1.000000000000000000, 0.000000000000000000 ) ) ;
#53375 = CARTESIAN_POINT ( 'NONE',  ( -7.500000000000000000, 0.000000000000000000, 0.7500000000000000000 ) ) ;
#53376 = EDGE_CURVE ( 'NONE', #20808, #19090, #57491, .T. ) ;
#53377 = VECTOR ( 'NONE', #34702, 1000.000000000000000 ) ;
#53378 = EDGE_LOOP ( 'NONE', ( #14957, #2266, #42662, #61220 ) ) ;
#53379 = CARTESIAN_POINT ( 'NONE',  ( 0.000000000000000000, 158.9429263765338192, -8.025000000000000355 ) ) ;
#53380 =( NAMED_UNIT ( * ) SI_UNIT ( $, .STERADIAN. ) SOLID_ANGLE_UNIT ( ) );
#53381 = FACE_OUTER_BOUND ( 'NONE', #59992, .T. ) ;
#53382 = EDGE_CURVE ( 'NONE', #60182, #4086, #11439, .T. ) ;
#53383 = CARTESIAN_POINT ( 'NONE',  ( 8.750000000000001776, 24.74999999999998579, -4.000000000000000000 ) ) ;
#53384 = CARTESIAN_POINT ( 'NONE',  ( 19.98198699191933869, 115.0278726071232711, -9.999999999996266098 ) ) ;
#53385 = ORIENTED_EDGE ( 'NONE', *, *, #15302, .F. ) ;
#53386 =( LENGTH_UNIT ( ) NAMED_UNIT ( * ) SI_UNIT ( .MILLI., .METRE. ) );
#53387 = CYLINDRICAL_SURFACE ( 'NONE', #8843, 0.4999999999999995004 ) ;
#53388 = CYLINDRICAL_SURFACE ( 'NONE', #36720, 9.524999999999991473 ) ;
#53389 = CARTESIAN_POINT ( 'NONE',  ( 57.00000000000000000, 0.000000000000000000, -79.00402776293826435 ) ) ;
#53390 = CARTESIAN_POINT ( 'NONE',  ( 45.07697505292422591, 10.02565835097472480, -6.500000000000000000 ) ) ;
#53391 = STYLED_ITEM ( 'NONE', ( #3583 ), #27767 ) ;
#53392 = CIRCLE ( 'NONE', #7294, 0.2500000000000002220 ) ;
#53393 = DIRECTION ( 'NONE',  ( 0.000000000000000000, -1.000000000000000000, 0.000000000000000000 ) ) ;
#53394 = LINE ( 'NONE', #33568, #5805 ) ;
#53395 = LINE ( 'NONE', #20687, #10175 ) ;
#53396 = CARTESIAN_POINT ( 'NONE',  ( -4.134715136431658777, 153.9646786816057045, 8.000580966448437081 ) ) ;
#53397 = ORIENTED_EDGE ( 'NONE', *, *, #67033, .T. ) ;
#53398 = ORIENTED_EDGE ( 'NONE', *, *, #31392, .T. ) ;
#53399 = DIRECTION ( 'NONE',  ( 1.000000000000000000, 0.000000000000000000, 0.000000000000000000 ) ) ;
#53400 = CARTESIAN_POINT ( 'NONE',  ( -16.72057948583355369, 65.79671608775228719, 5.561181121879805289 ) ) ;
#53401 = EDGE_CURVE ( 'NONE', #20703, #52602, #10359, .T. ) ;
#53402 = CARTESIAN_POINT ( 'NONE',  ( 0.000000000000000000, 110.5549999999999926, -9.525000000000000355 ) ) ;
#53404 = FILL_AREA_STYLE ('',( #65323 ) ) ;
#53403 = PRESENTATION_LAYER_ASSIGNMENT (  '', '', ( #42203 ) ) ;
#53405 = ORIENTED_EDGE ( 'NONE', *, *, #49250, .F. ) ;
#53406 = CARTESIAN_POINT ( 'NONE',  ( -167.9050000000000011, 2.607480562269068880, -8.024999999999993250 ) ) ;
#53407 = DIRECTION ( 'NONE',  ( 0.000000000000000000, 0.000000000000000000, -1.000000000000000000 ) ) ;
#53408 = CARTESIAN_POINT ( 'NONE',  ( 32.00000000000001421, 43.00000000000000000, 36.49999999999999289 ) ) ;
#53409 = CARTESIAN_POINT ( 'NONE',  ( -180.1450000000000102, -4.716976649647092401, 6.492361379858946790 ) ) ;
#53410 = AXIS2_PLACEMENT_3D ( 'NONE', #25225, #8374, #46024 ) ;
#53411 = AXIS2_PLACEMENT_3D ( 'NONE', #63593, #68532, #10136 ) ;
#53412 = CARTESIAN_POINT ( 'NONE',  ( -170.0949999999999989, -2.607480562269071545, -8.024999999999991473 ) ) ;
#53413 = ORIENTED_EDGE ( 'NONE', *, *, #32891, .F. ) ;
#53414 = FILL_AREA_STYLE_COLOUR ( '', #40325 ) ;
#53415 = CARTESIAN_POINT ( 'NONE',  ( -40.24243276991634843, -11.80832556086091856, 3.294024383991729366 ) ) ;
#53416 = CARTESIAN_POINT ( 'NONE',  ( -81.05499999999999261, -9.827790563157499189E-16, -8.024999999999991473 ) ) ;
#53417 = DIRECTION ( 'NONE',  ( -1.000000000000000000, -0.000000000000000000, -0.000000000000000000 ) ) ;
#53418 = CARTESIAN_POINT ( 'NONE',  ( 23.49527607712185073, 27.44009427658185984, 27.19000446309344809 ) ) ;
#53419 = CARTESIAN_POINT ( 'NONE',  ( -74.98971658424945019, 36.00805210434474901, -9.715834439412292411 ) ) ;
#53420 = AXIS2_PLACEMENT_3D ( 'NONE', #48276, #5653, #37749 ) ;
#53421 = CARTESIAN_POINT ( 'NONE',  ( -84.29499999999998749, -2.607480562269069768, 8.024999999999991473 ) ) ;
#53422 = CARTESIAN_POINT ( 'NONE',  ( -8.102448949553181734, 135.6049999999999613, 5.886773742842747126 ) ) ;
#53423 = ADVANCED_FACE ( 'NONE', ( #49360 ), #58498, .T. ) ;
#53424 = CARTESIAN_POINT ( 'NONE',  ( 7.766025168014160762, -0.5488498361408512549, 0.7660251680141582087 ) ) ;
#53425 = LINE ( 'NONE', #58336, #66300 ) ;
#53426 = DIRECTION ( 'NONE',  ( -0.000000000000000000, -1.000000000000000000, 0.000000000000000000 ) ) ;
#53427 = ADVANCED_FACE ( 'NONE', ( #11360 ), #64831, .F. ) ;
#53428 = COLOUR_RGB ( '', 0.40784314, 0.44705882, 0.49803922) ;
#53429 = ORIENTED_EDGE ( 'NONE', *, *, #19201, .T. ) ;
#53430 = CARTESIAN_POINT ( 'NONE',  ( -9.827790563157511022E-16, 133.4429263765338192, 8.025000000000000355 ) ) ;
#53431 = DIRECTION ( 'NONE',  ( 0.000000000000000000, 0.000000000000000000, -1.000000000000000000 ) ) ;
#53433 = DIRECTION ( 'NONE',  ( -1.040834085586083310E-14, 0.000000000000000000, -1.000000000000000000 ) ) ;
#53432 = SURFACE_SIDE_STYLE ('',( #22446 ) ) ;
#53434 = CARTESIAN_POINT ( 'NONE',  ( 1.000000000000000000, 0.9999999999999991118, -80.00402776293826435 ) ) ;
#53435 = ORIENTED_EDGE ( 'NONE', *, *, #5531, .F. ) ;
#53436 = EDGE_LOOP ( 'NONE', ( #48958, #1890, #15868, #52806 ) ) ;
#53437 = DIRECTION ( 'NONE',  ( 1.000000000000000000, 0.000000000000000000, 0.000000000000000000 ) ) ;
#53438 = DIRECTION ( 'NONE',  ( 0.000000000000000000, 1.000000000000000000, 0.000000000000000000 ) ) ;
#53439 = FILL_AREA_STYLE_COLOUR ( '', #18016 ) ;
#53440 = CARTESIAN_POINT ( 'NONE',  ( 69.74999999999998579, 36.75000000000000000, 4.000000000000000000 ) ) ;
#53441 = SURFACE_STYLE_FILL_AREA ( #65711 ) ;
#53442 = ORIENTED_EDGE ( 'NONE', *, *, #61615, .T. ) ;
#53443 = CARTESIAN_POINT ( 'NONE',  ( -121.4049999999999869, -2.607480562269069768, 8.024999999999991473 ) ) ;
#53444 = ORIENTED_EDGE ( 'NONE', *, *, #48035, .F. ) ;
#53445 = AXIS2_PLACEMENT_3D ( 'NONE', #9579, #3901, #9219 ) ;
#53446 = CARTESIAN_POINT ( 'NONE',  ( -2.451748578458123784E-13, 110.8535625161535592, 9.171437483846442973 ) ) ;
#53447 = ORIENTED_EDGE ( 'NONE', *, *, #45868, .T. ) ;
#53448 = DIRECTION ( 'NONE',  ( 0.000000000000000000, 2.430666987508117145E-16, -1.000000000000000000 ) ) ;
#53449 = ORIENTED_EDGE ( 'NONE', *, *, #49830, .T. ) ;
#53450 = ADVANCED_FACE ( 'NONE', ( #60567 ), #47449, .F. ) ;
#53451 = AXIS2_PLACEMENT_3D ( 'NONE', #24817, #9370, #3686 ) ;
#53452 = DIRECTION ( 'NONE',  ( -7.703719777548941223E-32, 1.000000000000000000, 0.000000000000000000 ) ) ;
#53453 = CARTESIAN_POINT ( 'NONE',  ( -1.166476076187854022E-15, 152.9449999999999932, 9.525000000000000355 ) ) ;
#53454 = ORIENTED_EDGE ( 'NONE', *, *, #68375, .F. ) ;
#53455 = CARTESIAN_POINT ( 'NONE',  ( -117.9570736234661723, 9.058813317711329915, -2.943386871421373119 ) ) ;
#53456 =( NAMED_UNIT ( * ) PLANE_ANGLE_UNIT ( ) SI_UNIT ( $, .RADIAN. ) );
#53457 = DIRECTION ( 'NONE',  ( -0.000000000000000000, -0.000000000000000000, 1.000000000000000000 ) ) ;
#53458 = EDGE_LOOP ( 'NONE', ( #27776, #56218 ) ) ;
#53459 = CARTESIAN_POINT ( 'NONE',  ( 2.607480562269071989, 121.5929263765338249, 8.025000000000002132 ) ) ;
#53460 = CARTESIAN_POINT ( 'NONE',  ( 45.44163888576682808, 10.14721296192225886, -3.260160134650228247 ) ) ;
#53461 = DIRECTION ( 'NONE',  ( 0.000000000000000000, 0.000000000000000000, -1.000000000000000000 ) ) ;
#53462 = VECTOR ( 'NONE', #20025, 1000.000000000000000 ) ;
#53463 = ADVANCED_FACE ( 'NONE', ( #17015 ), #19314, .T. ) ;
#53464 = ORIENTED_EDGE ( 'NONE', *, *, #46667, .T. ) ;
#53465 = CIRCLE ( 'NONE', #15291, 0.5000000000000004441 ) ;
#53466 = CARTESIAN_POINT ( 'NONE',  ( 1.000000000000000000, 0.9999999999999991118, -79.00402776293826435 ) ) ;
#53467 = ORIENTED_EDGE ( 'NONE', *, *, #26138, .F. ) ;
#53468 = PRESENTATION_STYLE_ASSIGNMENT (( #65028 ) ) ;
#53469 =( GEOMETRIC_REPRESENTATION_CONTEXT ( 3 ) GLOBAL_UNCERTAINTY_ASSIGNED_CONTEXT ( ( #67043 ) ) GLOBAL_UNIT_ASSIGNED_CONTEXT ( ( #13061, #66893, #39841 ) ) REPRESENTATION_CONTEXT ( 'NONE', 'WORKASPACE' ) );
#53470 = DIRECTION ( 'NONE',  ( -1.000000000000000000, 0.000000000000000000, -0.000000000000000000 ) ) ;
#53471 = CARTESIAN_POINT ( 'NONE',  ( -147.0549999999999784, -9.827790563157499189E-16, -8.024999999999991473 ) ) ;
#53472 = EDGE_CURVE ( 'NONE', #46653, #27901, #44196, .T. ) ;
#53473 = CARTESIAN_POINT ( 'NONE',  ( -175.8570736234661638, -5.598654528085803328, -7.705886871421366635 ) ) ;
#53474 = VECTOR ( 'NONE', #11910, 1000.000000000000000 ) ;
#53475 = EDGE_CURVE ( 'NONE', #52256, #43138, #26048, .T. ) ;
#53476 = VECTOR ( 'NONE', #12740, 1000.000000000000000 ) ;
#53477 = DIRECTION ( 'NONE',  ( -0.000000000000000000, -0.000000000000000000, -1.000000000000000000 ) ) ;
#53478 =( NAMED_UNIT ( * ) PLANE_ANGLE_UNIT ( ) SI_UNIT ( $, .RADIAN. ) );
#53479 = CARTESIAN_POINT ( 'NONE',  ( 48.25000000000000000, 22.24999999999998579, 3.750000000000000000 ) ) ;
#53480 = ORIENTED_EDGE ( 'NONE', *, *, #25650, .T. ) ;
#53481 = ORIENTED_EDGE ( 'NONE', *, *, #32025, .T. ) ;
#53482 = DIRECTION ( 'NONE',  ( -1.000000000000000000, -0.000000000000000000, -0.000000000000000000 ) ) ;
#53483 = EDGE_CURVE ( 'NONE', #59464, #42883, #51097, .T. ) ;
#53484 = CARTESIAN_POINT ( 'NONE',  ( -148.9429263765338192, 0.000000000000000000, 9.524999999999991473 ) ) ;
#53485 = CARTESIAN_POINT ( 'NONE',  ( -59.75499999999998835, 4.716976649647091513, -6.492361379858946790 ) ) ;
#53486 = ORIENTED_EDGE ( 'NONE', *, *, #19610, .T. ) ;
#53487 = FACE_OUTER_BOUND ( 'NONE', #16563, .T. ) ;
#53488 = CYLINDRICAL_SURFACE ( 'NONE', #15003, 0.2500000000000002220 ) ;
#53489 = DIRECTION ( 'NONE',  ( 0.000000000000000000, 0.000000000000000000, 1.000000000000000000 ) ) ;
#53490 = DIRECTION ( 'NONE',  ( 0.000000000000000000, 0.000000000000000000, -1.000000000000000000 ) ) ;
#53491 = VERTEX_POINT ( 'NONE', #30286 ) ;
#53492 = CARTESIAN_POINT ( 'NONE',  ( -60.00000000000000000, -2.024042244987997205E-14, -7.000000000000000888 ) ) ;
#53493 = DIRECTION ( 'NONE',  ( 0.000000000000000000, -1.000000000000000000, 0.000000000000000000 ) ) ;
#53494 = SURFACE_STYLE_USAGE ( .BOTH. , #1339 ) ;
#53495 = FACE_OUTER_BOUND ( 'NONE', #3551, .T. ) ;
#53496 = AXIS2_PLACEMENT_3D ( 'NONE', #67466, #40084, #30161 ) ;
#53497 = CARTESIAN_POINT ( 'NONE',  ( -109.9449999999999932, -9.827790563157499189E-16, -8.024999999999991473 ) ) ;
#53498 = CARTESIAN_POINT ( 'NONE',  ( 8.102448949553181734, 153.3950000000000387, 5.886773742842750679 ) ) ;
#53499 = CARTESIAN_POINT ( 'NONE',  ( -89.09499999999998465, -2.607480562269071545, -8.024999999999991473 ) ) ;
#53500 = CARTESIAN_POINT ( 'NONE',  ( 2.999999999999996447, 0.000000000000000000, -37.00402776293829277 ) ) ;
#53501 = CIRCLE ( 'NONE', #38920, 0.2500000000000002220 ) ;
#53502 = CIRCLE ( 'NONE', #16428, 1.000000000000000888 ) ;
#53503 = DIRECTION ( 'NONE',  ( -1.000000000000000000, -0.000000000000000000, -0.000000000000000000 ) ) ;
#53504 =( BOUNDED_CURVE ( )  B_SPLINE_CURVE ( 2, ( #8107, #51022, #2783, #41191, #29551, #24601, #62592, #45769, #2412, #57323, #7744 ),
 .UNSPECIFIED., .F., .F. ) 
 B_SPLINE_CURVE_WITH_KNOTS ( ( 3, 2, 2, 2, 2, 3 ),
 ( 0.08695652173912844785, 0.08913043478260665453, 0.09130434782608486122, 0.09347826086956306790, 0.09565217391304127459, 0.09782608695651948127 ),
 .UNSPECIFIED. ) 
 CURVE ( )  GEOMETRIC_REPRESENTATION_ITEM ( )  RATIONAL_B_SPLINE_CURVE ( ( 1.000000000000044631, 0.9510565162951089002, 1.000000000000000000, 0.9510565162951535312, 1.000000000000000000, 0.9510565162951535312, 1.000000000000000000, 0.9510565162951535312, 1.000000000000000000, 0.9510565162952044904, 0.9999999999999490408 ) ) 
 REPRESENTATION_ITEM ( '' )  );
#53505 = CARTESIAN_POINT ( 'NONE',  ( -167.1570736234661751, -9.058813317711329915, -2.943386871421370898 ) ) ;
#53506 = DIRECTION ( 'NONE',  ( 0.000000000000000000, 1.000000000000000000, 0.000000000000000000 ) ) ;
#53507 = ORIENTED_EDGE ( 'NONE', *, *, #8981, .F. ) ;
#53508 = CARTESIAN_POINT ( 'NONE',  ( -130.9429263765338192, 0.000000000000000000, 9.524999999999991473 ) ) ;
#53509 = CARTESIAN_POINT ( 'NONE',  ( -149.6949999999999648, -8.437984349512085203, 5.166775262442717831E-16 ) ) ;
#53510 = COLOUR_RGB ( '', 0.08235294, 0.09019608, 0.10196078) ;
#53511 = COLOUR_RGB ( '', 0.09019608, 0.27058824, 0.51372549) ;
#53512 = DIRECTION ( 'NONE',  ( -1.000000000000000000, -0.000000000000000000, -0.000000000000000000 ) ) ;
#53513 = FILL_AREA_STYLE ('',( #64757 ) ) ;
#53514 = ORIENTED_EDGE ( 'NONE', *, *, #56720, .F. ) ;
#53515 = EDGE_LOOP ( 'NONE', ( #58788, #25832, #2297, #64073 ) ) ;
#53516 = DIRECTION ( 'NONE',  ( 0.000000000000000000, 0.000000000000000000, 1.000000000000000000 ) ) ;
#53517 = CARTESIAN_POINT ( 'NONE',  ( -8.437984349512095861, 117.6929263765338050, -5.166775262442723748E-16 ) ) ;
#53518 = CARTESIAN_POINT ( 'NONE',  ( -45.87416991466958649, 9.273068908601562299, 6.223864456579077498 ) ) ;
#53519 = DIRECTION ( 'NONE',  ( 1.000000000000000000, 0.000000000000000000, 0.000000000000000000 ) ) ;
#53520 = CARTESIAN_POINT ( 'NONE',  ( -57.58629378005753097, -7.761720733523303828, -0.7755720678496390574 ) ) ;
#53521 = CARTESIAN_POINT ( 'NONE',  ( -150.7429263765338021, -5.598654528085803328, -7.705886871421366635 ) ) ;
#53522 = ORIENTED_EDGE ( 'NONE', *, *, #59076, .T. ) ;
#53523 = CARTESIAN_POINT ( 'NONE',  ( -152.4550000000000125, 7.632228543268599452, -2.479861379858951942 ) ) ;
#53524 = ORIENTED_EDGE ( 'NONE', *, *, #48628, .T. ) ;
#53525 = FACE_OUTER_BOUND ( 'NONE', #54042, .T. ) ;
#53526 = ORIENTED_EDGE ( 'NONE', *, *, #25782, .F. ) ;
#53527 = ADVANCED_FACE ( 'NONE', ( #25043 ), #32792, .T. ) ;
#53528 = DIRECTION ( 'NONE',  ( -0.000000000000000000, -0.000000000000000000, -1.000000000000000000 ) ) ;
#53529 = CARTESIAN_POINT ( 'NONE',  ( 8.102448949553183510, 123.9949999999999903, -5.886773742842746238 ) ) ;
#53530 = DIRECTION ( 'NONE',  ( 0.000000000000000000, -1.000000000000000000, 0.000000000000000000 ) ) ;
#53531 = EDGE_CURVE ( 'NONE', #27999, #64410, #56344, .T. ) ;
#53532 = VERTEX_POINT ( 'NONE', #40555 ) ;
#53533 = EDGE_CURVE ( 'NONE', #23645, #42007, #23999, .T. ) ;
#53534 = CARTESIAN_POINT ( 'NONE',  ( -95.90707362346724096, -3.094860106600548111, 9.525000000012983747 ) ) ;
#53535 = CARTESIAN_POINT ( 'NONE',  ( -10.01517768586949408, 120.3049999999999784, -6.132527647946036459E-16 ) ) ;
#53536 = CARTESIAN_POINT ( 'NONE',  ( -63.80499999999998550, -8.437984349512086979, 5.166775262442717831E-16 ) ) ;
#53537 = CARTESIAN_POINT ( 'NONE',  ( -122.9950000000000045, -6.826472737025115478, 4.959722759717900331 ) ) ;
#53538 = DIRECTION ( 'NONE',  ( -0.000000000000000000, -1.000000000000000000, 0.000000000000000000 ) ) ;
#53539 = VERTEX_POINT ( 'NONE', #29625 ) ;
#53540 = CARTESIAN_POINT ( 'NONE',  ( 5.598654528085809545, 152.2549999999999670, -7.705886871421373741 ) ) ;
#53541 = EDGE_CURVE ( 'NONE', #6283, #49290, #50769, .T. ) ;
#53542 = DIRECTION ( 'NONE',  ( 1.000000000000000000, 0.000000000000000000, 0.000000000000000000 ) ) ;
#53543 = CARTESIAN_POINT ( 'NONE',  ( 7.999999999999992895, 0.000000000000000000, 24.00402776293826079 ) ) ;
#53544 = EDGE_CURVE ( 'NONE', #1454, #56729, #42984, .T. ) ;
#53545 = STYLED_ITEM ( 'NONE', ( #33375 ), #2964 ) ;
#53546 = EDGE_CURVE ( 'NONE', #35999, #43029, #35043, .T. ) ;
#53547 = DIRECTION ( 'NONE',  ( 0.000000000000000000, 0.000000000000000000, 1.000000000000000000 ) ) ;
#53548 = COLOUR_RGB ( '', 0.72549020, 0.75294118, 0.79215686) ;
#53549 = ORIENTED_EDGE ( 'NONE', *, *, #23830, .F. ) ;
#53550 = FILL_AREA_STYLE ('',( #20494 ) ) ;
#53551 = CARTESIAN_POINT ( 'NONE',  ( -170.6050000000000182, 6.826472737025113702, -4.959722759717902107 ) ) ;
#53553 = VERTEX_POINT ( 'NONE', #24336 ) ;
#53552 = EDGE_CURVE ( 'NONE', #26603, #4250, #2847, .T. ) ;
#53554 = CARTESIAN_POINT ( 'NONE',  ( 2.056319983864932865, 111.9482313798679769, -7.829595205988900908 ) ) ;
#53555 =( NAMED_UNIT ( * ) SI_UNIT ( $, .STERADIAN. ) SOLID_ANGLE_UNIT ( ) );
#53556 = EDGE_CURVE ( 'NONE', #46319, #20411, #39247, .T. ) ;
#53557 = PRESENTATION_STYLE_ASSIGNMENT (( #38108 ) ) ;
#53558 = EDGE_LOOP ( 'NONE', ( #18151, #20828, #68961, #35232 ) ) ;
#53559 = CARTESIAN_POINT ( 'NONE',  ( -129.0570736234661808, 0.000000000000000000, 9.524999999999991473 ) ) ;
#53560 = FACE_OUTER_BOUND ( 'NONE', #40682, .T. ) ;
#53561 = CARTESIAN_POINT ( 'NONE',  ( -98.00500000000000966, 6.826472737025116366, 4.959722759717898555 ) ) ;
#53562 = ORIENTED_EDGE ( 'NONE', *, *, #22573, .T. ) ;
#53563 = CARTESIAN_POINT ( 'NONE',  ( -6.062177826491070398, 2.500000000000000000, -3.499999999999998224 ) ) ;
#53564 = CARTESIAN_POINT ( 'NONE',  ( -130.1070736234661922, 8.102448949553171076, -5.886773742842744461 ) ) ;
#53565 = SURFACE_STYLE_FILL_AREA ( #42712 ) ;
#53566 = DIRECTION ( 'NONE',  ( 1.000000000000000000, 0.000000000000000000, 0.000000000000000000 ) ) ;
#53567 = CARTESIAN_POINT ( 'NONE',  ( -68.60707362346614957, -8.102448949553172852, 5.886773742842742685 ) ) ;
#53568 = DIRECTION ( 'NONE',  ( 0.000000000000000000, -1.000000000000000000, 0.000000000000000000 ) ) ;
#53569 = ORIENTED_EDGE ( 'NONE', *, *, #39985, .F. ) ;
#53570 =( LENGTH_UNIT ( ) NAMED_UNIT ( * ) SI_UNIT ( .MILLI., .METRE. ) );
#53571 = PRESENTATION_LAYER_ASSIGNMENT (  '', '', ( #54660 ) ) ;
#53572 =( LENGTH_UNIT ( ) NAMED_UNIT ( * ) SI_UNIT ( .MILLI., .METRE. ) );
#53573 = CARTESIAN_POINT ( 'NONE',  ( -110.6049999999999898, 6.826472737025113702, -4.959722759717902107 ) ) ;
#53574 = CARTESIAN_POINT ( 'NONE',  ( 9.058813317711337021, 123.5449999999999875, 2.943386871421375783 ) ) ;
#53575 = CARTESIAN_POINT ( 'NONE',  ( -113.8449999999999847, -7.632228543268599452, 2.479861379858951054 ) ) ;
#53576 =( LENGTH_UNIT ( ) NAMED_UNIT ( * ) SI_UNIT ( .MILLI., .METRE. ) );
#53577 = EDGE_CURVE ( 'NONE', #20521, #17573, #44091, .T. ) ;
#53579 = FILL_AREA_STYLE_COLOUR ( '', #67344 ) ;
#53578 =( LENGTH_UNIT ( ) NAMED_UNIT ( * ) SI_UNIT ( .MILLI., .METRE. ) );
#53580 = ORIENTED_EDGE ( 'NONE', *, *, #32459, .T. ) ;
#53581 = CARTESIAN_POINT ( 'NONE',  ( -158.6929263765338192, 10.01517768586948698, -1.839758294383808571E-15 ) ) ;
#53582 =( NAMED_UNIT ( * ) PLANE_ANGLE_UNIT ( ) SI_UNIT ( $, .RADIAN. ) );
#53583 = CARTESIAN_POINT ( 'NONE',  ( -171.8949999999999534, 6.826472737025116366, 4.959722759717898555 ) ) ;
#53584 = CIRCLE ( 'NONE', #23261, 13.99999999999999822 ) ;
#53585 = B_SPLINE_CURVE_WITH_KNOTS ( 'NONE', 3,
 ( #21242, #42773, #5404, #16370, #59217, #27199, #59575, #11392 ),
 .UNSPECIFIED., .F., .F.,
 ( 4, 2, 2, 4 ),
 ( 0.01462827986756859780, 0.01731435831274189333, 0.01865739753532854109, 0.02000043675791518885 ),
 .UNSPECIFIED. ) ;
#53586 = AXIS2_PLACEMENT_3D ( 'NONE', #37771, #12015, #16297 ) ;
#53587 = FACE_OUTER_BOUND ( 'NONE', #40986, .T. ) ;
#53588 = CARTESIAN_POINT ( 'NONE',  ( -41.21370884129409973, -11.98618176148272241, 3.233652621117119708 ) ) ;
#53589 = DIRECTION ( 'NONE',  ( 1.000000000000000000, 0.000000000000000000, 0.000000000000000000 ) ) ;
#53590 = DIRECTION ( 'NONE',  ( -1.000000000000000000, 0.000000000000000000, 0.000000000000000000 ) ) ;
#53591 = VERTEX_POINT ( 'NONE', #35610 ) ;
#53592 = CARTESIAN_POINT ( 'NONE',  ( -79.94292637653380496, 0.000000000000000000, 9.524999999999991473 ) ) ;
#53593 = LINE ( 'NONE', #59546, #16134 ) ;
#53594 =( BOUNDED_SURFACE ( )  B_SPLINE_SURFACE ( 1, 2, ( 
 ( #8703, #24858, #14319, #5824, #58972, #143, #27264, #10443, #42484, #59645, #31525, #5462, #37206, #54368, #26252, #26583, #59278, #43535, #48108, #54023, #47784, #69186, #64228, #10783, #48802, #26914, #53357, #64920, #69511, #6189, #48452, #37909, #11462, #36854, #32934, #502, #37572, #20643, #53005, #47422, #4802, #16770, #32227, #11106, #16086, #38243, #22032, #68845, #15726, #32557, #63550, #42156, #15396, #21673, #64600, #43192, #58268, #10094, #20986, #63877, #58617, #31874, #5138, #16446, #21314, #42836, #53676, #23397, #28302, #55056, #6512, #7238, #45251, #2223, #28669, #1887, #44571, #50497, #34316, #23753, #17798, #49810, #12146, #55769, #38600, #49463, #44905, #12848, #66311, #27622, #49135, #18138, #17471, #830, #17128, #22368, #50164, #39274, #23076, #65627, #13186, #7575, #59997, #60339, #33611, #39974, #65966, #33279, #66675, #12493, #39622, #60676, #18490, #29005, #61375, #38940, #61030, #43867, #34644, #65275, #56103, #11809, #54707, #27955, #1189, #22723, #44222, #6880, #1552, #33953, #55413, #51525, #35363, #24427, #3646, #8628, #56819, #56453, #57139, #25479, #52254, #8971, #51891, #24775, #30751, #14592, #4011, #67716, #30058, #62067, #36059, #18815, #29729, #25143, #62756, #46656, #7920, #29363, #68075, #67358, #50842, #67025, #2597, #30389, #19510, #3287, #45932, #63122, #57501, #40298, #40655, #13897, #20200, #46294, #41009, #41701, #14962, #8287, #9327, #19858, #24102, #46993, #62430, #14245, #35709, #36445, #41351, #68405, #45608, #61705, #13536, #35004, #19154, #51195, #2939, #31438, #48725, #64153, #16357, #69442, #10699, #37832, #20917, #52932, #428, #42073, #16009, #47706, #64846, #36784, #37130, #61, #53937, #58538, #64513, #58195, #10018, #5064, #21231, #59205, #37489, #63804, #5742, #10371, #16694, #58893, #48371, #21958, #47337, #43465, #11028, #48039, #31097, #63475, #57865, #9689, #32152, #27186, #52594, #31797, #53606, #4341, #25825, #42758, #68766, #21594, #53277, #26517, #5393, #4720, #20558, #32475, #15326, #26169, #26833, #69109, #42416, #15650, #43107, #55684, #65546, #65190, #27542, #22285, #12406, #33864, #66225, #44490, #55328, #65895, #1100, #17722, #12758, #49068, #7153, #49726, #60268, #7495, #50079, #17392, #6108, #752, #60588, #44145, #28923, #22995, #11733, #38857, #22641, #17042, #59562, #27872, #44820, #12069, #11383, #23664, #54964, #45170, #49378, #28581, #66589, #38523, #33533, #32847, #6789, #28217, #18050, #59916, #1466, #39536, #54638, #1809, #50409, #39193, #23324, #60939, #34230, #2133, #38159, #54290, #6446, #43787, #33200, #46571, #67993, #29279, #52174, #24688, #8200, #46208, #50761, #19430, #62348, #35274, #29648, #13109, #19066, #18740, #61297, #3930, #67630 ),
 ( #40222, #62673, #3559, #19780, #40928, #35974, #14171, #41275, #51809, #9248, #2510, #35630, #24019, #57065, #18406, #8881, #57420, #25401, #40571, #30305, #34564, #30667, #29983, #56016, #25061, #67276, #61988, #3196, #13452, #7832, #14498, #46918, #39891, #8550, #45526, #66946, #61626, #34918, #56365, #45846, #51116, #2860, #24352, #13813, #56736, #51448, #4985, #64070, #26435, #31355, #47968, #43027, #57780, #15923, #10283, #20836, #16280, #10622, #47620, #36358, #9605, #21158, #4632, #59133, #53197, #41982, #69027, #52857, #25740, #20109, #58125, #5316, #26087, #41614, #53862, #15571, #5659, #9935, #37404, #27107, #47259, #63724, #63031, #42338, #37043, #26761, #68677, #31716, #55171, #15241, #58806, #10956, #58460, #69368, #42668, #32073, #32394, #53529, #48284, #36709, #31021, #21509, #64430, #37754, #52515, #68328, #14874, #4260, #20477, #63394, #49644, #22916, #65465, #59842, #43384, #49298, #48988, #21875, #34146, #6707, #28136, #44059, #32758, #33455, #11650, #1011, #22210, #54209, #43706, #17315, #679, #23251, #33790, #50004, #1387, #66142, #44416, #28497, #12320, #39460, #65817, #60863, #54556, #17649, #39118, #60187, #12677, #27795, #60507, #16953, #16614, #33120, #7069, #1743, #59474, #55605, #54883, #38440, #55242, #11303, #44748, #17972, #38777, #6366, #64775, #22556, #65099, #38077, #7428, #48641, #340, #11995, #6025, #27463, #40149, #29558, #2419, #13036, #23932, #67193, #29190, #3470, #14088, #30227, #51366, #46480, #8474, #8801, #62260, #19699, #39808, #56647, #28851, #29908, #67905, #35883, #51027, #3112, #45094, #41196, #40492, #66507, #35549, #8113, #2788, #13727, #45446, #23583, #56987, #57329, #62596, #18982, #18328, #14410, #50334, #66866, #2056, #56283, #55944, #61226, #34489, #24605, #46121, #51723, #35187, #67542, #19341, #61543, #40841, #24971, #7749, #50677, #61908, #24277, #18671, #13370, #45774, #34830, #46842, #31631, #15156, #69611, #63650, #52434, #58047, #41890, #36265, #30580, #68593, #15834, #36630, #52085, #64339, #26000, #16187, #20388, #26348, #37665, #57690, #4543, #3836, #63308, #9853, #37313, #9519, #42261, #10542, #25653, #58721, #58368, #31268, #26679, #52768, #9165, #36957, #69287, #21420, #68248, #42938, #31979, #68943, #25320, #62942, #20029, #14787, #5235, #15490, #21081, #47529, #41528, #53453, #48204, #47173, #42580, #30938, #4179, #20751, #53112, #47888, #4899, #10193, #63984, #250, #59381, #11215, #53772, #59062, #38693, #16872, #22125, #32662, #65380, #65014, #43619, #16535, #919, #44323, #1289, #22470, #43966, #59748, #22825, #54797, #65721, #33029, #38346, #48902, #6606, #21783, #54118, #17228, #33371, #60094, #10879, #5573, #11911, #27371, #27019, #43296, #48554, #28050 ) ),
 .UNSPECIFIED., .F., .F., .F. ) 
 B_SPLINE_SURFACE_WITH_KNOTS ( ( 2, 2 ),
 ( 3, 2, 2, 2, 2, 2, 2, 2, 2, 2, 2, 2, 2, 2, 2, 2, 2, 2, 2, 2, 2, 2, 2, 2, 2, 2, 2, 2, 2, 2, 2, 2, 2, 2, 2, 2, 2, 2, 2, 2, 2, 2, 2, 2, 2, 2, 2, 2, 2, 2, 2, 2, 2, 2, 2, 2, 2, 2, 2, 2, 2, 2, 2, 2, 2, 2, 2, 2, 2, 2, 2, 2, 2, 2, 2, 2, 2, 2, 2, 2, 2, 2, 2, 2, 2, 2, 2, 2, 2, 2, 2, 2, 2, 2, 2, 2, 2, 2, 2, 2, 2, 2, 2, 2, 2, 2, 2, 2, 2, 2, 2, 2, 2, 2, 2, 2, 2, 2, 2, 2, 2, 2, 2, 2, 2, 2, 2, 2, 2, 2, 2, 2, 2, 2, 2, 2, 2, 2, 2, 2, 2, 2, 2, 2, 2, 2, 2, 2, 2, 2, 2, 2, 2, 2, 2, 2, 2, 2, 2, 2, 2, 2, 2, 2, 2, 2, 2, 2, 2, 2, 3 ),
 ( 0.000000000000000000, 1.000000000000000000 ),
 ( 0.000000000000000000, 0.005882352941176470507, 0.01176470588235294101, 0.01764705882352941152, 0.02352941176470588203, 0.02941176470588235253, 0.03529411764705882304, 0.04117647058823529355, 0.04705882352941176405, 0.05294117647058823456, 0.05882352941176470507, 0.06470588235294118251, 0.07058823529411764608, 0.07647058823529412352, 0.08235294117647058709, 0.08823529411764706454, 0.09411764705882352811, 0.1000000000000000056, 0.1058823529411764691, 0.1117647058823529466, 0.1176470588235294101, 0.1235294117647058876, 0.1294117647058823650, 0.1352941176470588147, 0.1411764705882352922, 0.1470588235294117696, 0.1529411764705882470, 0.1588235294117646967, 0.1647058823529411742, 0.1705882352941176516, 0.1764705882352941291, 0.1823529411764705788, 0.1882352941176470562, 0.1941176470588235337, 0.2000000000000000111, 0.2058823529411764608, 0.2117647058823529382, 0.2176470588235294157, 0.2235294117647058931, 0.2294117647058823428, 0.2352941176470588203, 0.2411764705882352977, 0.2470588235294117752, 0.2529411764705882248, 0.2588235294117647300, 0.2647058823529411797, 0.2705882352941176294, 0.2764705882352941346, 0.2823529411764705843, 0.2882352941176470340, 0.2941176470588235392, 0.2999999999999999889, 0.3058823529411764941, 0.3117647058823529438, 0.3176470588235293935, 0.3235294117647058987, 0.3294117647058823484, 0.3352941176470587981, 0.3411764705882353033, 0.3470588235294117530, 0.3529411764705882582, 0.3588235294117647078, 0.3647058823529411575, 0.3705882352941176627, 0.3764705882352941124, 0.3823529411764705621, 0.3882352941176470673, 0.3941176470588235170, 0.4000000000000000222, 0.4058823529411764719, 0.4117647058823529216, 0.4176470588235294268, 0.4235294117647058765, 0.4294117647058823262, 0.4352941176470588314, 0.4411764705882352811, 0.4470588235294117863, 0.4529411764705882359, 0.4588235294117646856, 0.4647058823529411908, 0.4705882352941176405, 0.4764705882352940902, 0.4823529411764705954, 0.4882352941176470451, 0.4941176470588235503, 0.5000000000000000000, 0.5058823529411764497, 0.5117647058823528994, 0.5176470588235294601, 0.5235294117647059098, 0.5294117647058823595, 0.5352941176470588092, 0.5411764705882352589, 0.5470588235294118196, 0.5529411764705882693, 0.5588235294117647189, 0.5647058823529411686, 0.5705882352941176183, 0.5764705882352940680, 0.5823529411764706287, 0.5882352941176470784, 0.5941176470588235281, 0.5999999999999999778, 0.6058823529411764275, 0.6117647058823529882, 0.6176470588235294379, 0.6235294117647058876, 0.6294117647058823373, 0.6352941176470587870, 0.6411764705882353477, 0.6470588235294117974, 0.6529411764705882470, 0.6588235294117646967, 0.6647058823529411464, 0.6705882352941175961, 0.6764705882352941568, 0.6823529411764706065, 0.6882352941176470562, 0.6941176470588235059, 0.6999999999999999556, 0.7058823529411765163, 0.7117647058823529660, 0.7176470588235294157, 0.7235294117647058654, 0.7294117647058823151, 0.7352941176470588758, 0.7411764705882353255, 0.7470588235294117752, 0.7529411764705882248, 0.7588235294117646745, 0.7647058823529411242, 0.7705882352941176849, 0.7764705882352941346, 0.7823529411764705843, 0.7882352941176470340, 0.7941176470588234837, 0.8000000000000000444, 0.8058823529411764941, 0.8117647058823529438, 0.8176470588235293935, 0.8235294117647058432, 0.8294117647058824039, 0.8352941176470588536, 0.8411764705882353033, 0.8470588235294117530, 0.8529411764705882026, 0.8588235294117646523, 0.8647058823529412130, 0.8705882352941176627, 0.8764705882352941124, 0.8823529411764705621, 0.8882352941176470118, 0.8941176470588235725, 0.9000000000000000222, 0.9058823529411764719, 0.9117647058823529216, 0.9176470588235293713, 0.9235294117647059320, 0.9294117647058823817, 0.9352941176470588314, 0.9411764705882352811, 0.9470588235294117307, 0.9529411764705881804, 0.9588235294117647411, 0.9647058823529411908, 0.9705882352941176405, 0.9764705882352940902, 0.9823529411764705399, 0.9882352941176471006, 0.9941176470588235503, 1.000000000000000000 ),
 .UNSPECIFIED. ) 
 GEOMETRIC_REPRESENTATION_ITEM ( )  RATIONAL_B_SPLINE_SURFACE ( (
 ( 1.000000000000000000, 0.9510565162951535312, 1.000000000000000000, 0.9510565162951535312, 1.000000000000000000, 0.9510565162951535312, 1.000000000000000000, 0.9510565162951535312, 1.000000000000000000, 0.9510565162951535312, 1.000000000000000000, 0.9510565162951535312, 1.000000000000000000, 0.9510565162951535312, 1.000000000000000000, 0.9510565162951535312, 1.000000000000000000, 0.9510565162951535312, 1.000000000000000000, 0.9510565162951535312, 1.000000000000000000, 0.9510565162951535312, 1.000000000000000000, 0.9510565162951535312, 1.000000000000000000, 0.9510565162951535312, 1.000000000000000000, 0.9510565162951535312, 1.000000000000000000, 0.9510565162951535312, 1.000000000000000000, 0.9510565162951535312, 1.000000000000000000, 0.9510565162951535312, 1.000000000000000000, 0.9510565162951535312, 1.000000000000000000, 0.9510565162951535312, 1.000000000000000000, 0.9510565162951535312, 1.000000000000000000, 0.9510565162951535312, 1.000000000000000000, 0.9510565162951535312, 1.000000000000000000, 0.9510565162951535312, 1.000000000000000000, 0.9510565162951535312, 1.000000000000000000, 0.9510565162951535312, 1.000000000000000000, 0.9510565162951535312, 1.000000000000000000, 0.9510565162951535312, 1.000000000000000000, 0.9510565162951535312, 1.000000000000000000, 0.9510565162951535312, 1.000000000000000000, 0.9510565162951535312, 1.000000000000000000, 0.9510565162951535312, 1.000000000000000000, 0.9510565162951535312, 1.000000000000000000, 0.9510565162951535312, 1.000000000000000000, 0.9510565162951535312, 1.000000000000000000, 0.9510565162951535312, 1.000000000000000000, 0.9510565162951535312, 1.000000000000000000, 0.9510565162951535312, 1.000000000000000000, 0.9510565162951535312, 1.000000000000000000, 0.9510565162951535312, 1.000000000000000000, 0.9510565162951535312, 1.000000000000000000, 0.9510565162951535312, 1.000000000000000000, 0.9510565162951535312, 1.000000000000000000, 0.9510565162951535312, 1.000000000000000000, 0.9510565162951535312, 1.000000000000000000, 0.9510565162951535312, 1.000000000000000000, 0.9510565162951535312, 1.000000000000000000, 0.9510565162951535312, 1.000000000000000000, 0.9510565162951535312, 1.000000000000000000, 0.9510565162951535312, 1.000000000000000000, 0.9510565162951535312, 1.000000000000000000, 0.9510565162951535312, 1.000000000000000000, 0.9510565162951535312, 1.000000000000000000, 0.9510565162951535312, 1.000000000000000000, 0.9510565162951535312, 1.000000000000000000, 0.9510565162951535312, 1.000000000000000000, 0.9510565162951535312, 1.000000000000000000, 0.9510565162951535312, 1.000000000000000000, 0.9510565162951535312, 1.000000000000000000, 0.9510565162951535312, 1.000000000000000000, 0.9510565162951535312, 1.000000000000000000, 0.9510565162951535312, 1.000000000000000000, 0.9510565162951535312, 1.000000000000000000, 0.9510565162951535312, 1.000000000000000000, 0.9510565162951535312, 1.000000000000000000, 0.9510565162951535312, 1.000000000000000000, 0.9510565162951535312, 1.000000000000000000, 0.9510565162951535312, 1.000000000000000000, 0.9510565162951535312, 1.000000000000000000, 0.9510565162951535312, 1.000000000000000000, 0.9510565162951535312, 1.000000000000000000, 0.9510565162951535312, 1.000000000000000000, 0.9510565162951535312, 1.000000000000000000, 0.9510565162951535312, 1.000000000000000000, 0.9510565162951535312, 1.000000000000000000, 0.9510565162951535312, 1.000000000000000000, 0.9510565162951535312, 1.000000000000000000, 0.9510565162951535312, 1.000000000000000000, 0.9510565162951535312, 1.000000000000000000, 0.9510565162951535312, 1.000000000000000000, 0.9510565162951535312, 1.000000000000000000, 0.9510565162951535312, 1.000000000000000000, 0.9510565162951535312, 1.000000000000000000, 0.9510565162951535312, 1.000000000000000000, 0.9510565162951535312, 1.000000000000000000, 0.9510565162951535312, 1.000000000000000000, 0.9510565162951535312, 1.000000000000000000, 0.9510565162951535312, 1.000000000000000000, 0.9510565162951535312, 1.000000000000000000, 0.9510565162951535312, 1.000000000000000000, 0.9510565162951535312, 1.000000000000000000, 0.9510565162951535312, 1.000000000000000000, 0.9510565162951535312, 1.000000000000000000, 0.9510565162951535312, 1.000000000000000000, 0.9510565162951535312, 1.000000000000000000, 0.9510565162951535312, 1.000000000000000000, 0.9510565162951535312, 1.000000000000000000, 0.9510565162951535312, 1.000000000000000000, 0.9510565162951535312, 1.000000000000000000, 0.9510565162951535312, 1.000000000000000000, 0.9510565162951535312, 1.000000000000000000, 0.9510565162951535312, 1.000000000000000000, 0.9510565162951535312, 1.000000000000000000, 0.9510565162951535312, 1.000000000000000000, 0.9510565162951535312, 1.000000000000000000, 0.9510565162951535312, 1.000000000000000000, 0.9510565162951535312, 1.000000000000000000, 0.9510565162951535312, 1.000000000000000000, 0.9510565162951535312, 1.000000000000000000, 0.9510565162951535312, 1.000000000000000000, 0.9510565162951535312, 1.000000000000000000, 0.9510565162951535312, 1.000000000000000000, 0.9510565162951535312, 1.000000000000000000, 0.9510565162951535312, 1.000000000000000000, 0.9510565162951535312, 1.000000000000000000, 0.9510565162951535312, 1.000000000000000000, 0.9510565162951535312, 1.000000000000000000, 0.9510565162951535312, 1.000000000000000000, 0.9510565162951535312, 1.000000000000000000, 0.9510565162951535312, 1.000000000000000000, 0.9510565162951535312, 1.000000000000000000, 0.9510565162951535312, 1.000000000000000000, 0.9510565162951535312, 1.000000000000000000, 0.9510565162951535312, 1.000000000000000000, 0.9510565162951535312, 1.000000000000000000, 0.9510565162951535312, 1.000000000000000000, 0.9510565162951535312, 1.000000000000000000, 0.9510565162951535312, 1.000000000000000000, 0.9510565162951535312, 1.000000000000000000, 0.9510565162951535312, 1.000000000000000000, 0.9510565162951535312, 1.000000000000000000, 0.9510565162951535312, 1.000000000000000000, 0.9510565162951535312, 1.000000000000000000, 0.9510565162951535312, 1.000000000000000000, 0.9510565162951535312, 1.000000000000000000, 0.9510565162951535312, 1.000000000000000000, 0.9510565162951535312, 1.000000000000000000, 0.9510565162951535312, 1.000000000000000000, 0.9510565162951535312, 1.000000000000000000, 0.9510565162951535312, 1.000000000000000000, 0.9510565162951535312, 1.000000000000000000, 0.9510565162951535312, 1.000000000000000000, 0.9510565162951535312, 1.000000000000000000, 0.9510565162951535312, 1.000000000000000000, 0.9510565162951535312, 1.000000000000000000, 0.9510565162951535312, 1.000000000000000000, 0.9510565162951535312, 1.000000000000000000, 0.9510565162951535312, 1.000000000000000000, 0.9510565162951535312, 1.000000000000000000, 0.9510565162951535312, 1.000000000000000000, 0.9510565162951535312, 1.000000000000000000, 0.9510565162951535312, 1.000000000000000000, 0.9510565162951535312, 1.000000000000000000, 0.9510565162951535312, 1.000000000000000000, 0.9510565162951535312, 1.000000000000000000, 0.9510565162951535312, 1.000000000000000000, 0.9510565162951535312, 1.000000000000000000, 0.9510565162951535312, 1.000000000000000000, 0.9510565162951535312, 1.000000000000000000, 0.9510565162951535312, 1.000000000000000000, 0.9510565162951535312, 1.000000000000000000, 0.9510565162951535312, 1.000000000000000000, 0.9510565162951535312, 1.000000000000000000, 0.9510565162951535312, 1.000000000000000000, 0.9510565162951535312, 1.000000000000000000, 0.9510565162951535312, 1.000000000000000000, 0.9510565162951535312, 1.000000000000000000, 0.9510565162951535312, 1.000000000000000000, 0.9510565162951535312, 1.000000000000000000, 0.9510565162951535312, 1.000000000000000000, 0.9510565162951535312, 1.000000000000000000),
 ( 1.000000000000000000, 0.9510565162951535312, 1.000000000000000000, 0.9510565162951535312, 1.000000000000000000, 0.9510565162951535312, 1.000000000000000000, 0.9510565162951535312, 1.000000000000000000, 0.9510565162951535312, 1.000000000000000000, 0.9510565162951535312, 1.000000000000000000, 0.9510565162951535312, 1.000000000000000000, 0.9510565162951535312, 1.000000000000000000, 0.9510565162951535312, 1.000000000000000000, 0.9510565162951535312, 1.000000000000000000, 0.9510565162951535312, 1.000000000000000000, 0.9510565162951535312, 1.000000000000000000, 0.9510565162951535312, 1.000000000000000000, 0.9510565162951535312, 1.000000000000000000, 0.9510565162951535312, 1.000000000000000000, 0.9510565162951535312, 1.000000000000000000, 0.9510565162951535312, 1.000000000000000000, 0.9510565162951535312, 1.000000000000000000, 0.9510565162951535312, 1.000000000000000000, 0.9510565162951535312, 1.000000000000000000, 0.9510565162951535312, 1.000000000000000000, 0.9510565162951535312, 1.000000000000000000, 0.9510565162951535312, 1.000000000000000000, 0.9510565162951535312, 1.000000000000000000, 0.9510565162951535312, 1.000000000000000000, 0.9510565162951535312, 1.000000000000000000, 0.9510565162951535312, 1.000000000000000000, 0.9510565162951535312, 1.000000000000000000, 0.9510565162951535312, 1.000000000000000000, 0.9510565162951535312, 1.000000000000000000, 0.9510565162951535312, 1.000000000000000000, 0.9510565162951535312, 1.000000000000000000, 0.9510565162951535312, 1.000000000000000000, 0.9510565162951535312, 1.000000000000000000, 0.9510565162951535312, 1.000000000000000000, 0.9510565162951535312, 1.000000000000000000, 0.9510565162951535312, 1.000000000000000000, 0.9510565162951535312, 1.000000000000000000, 0.9510565162951535312, 1.000000000000000000, 0.9510565162951535312, 1.000000000000000000, 0.9510565162951535312, 1.000000000000000000, 0.9510565162951535312, 1.000000000000000000, 0.9510565162951535312, 1.000000000000000000, 0.9510565162951535312, 1.000000000000000000, 0.9510565162951535312, 1.000000000000000000, 0.9510565162951535312, 1.000000000000000000, 0.9510565162951535312, 1.000000000000000000, 0.9510565162951535312, 1.000000000000000000, 0.9510565162951535312, 1.000000000000000000, 0.9510565162951535312, 1.000000000000000000, 0.9510565162951535312, 1.000000000000000000, 0.9510565162951535312, 1.000000000000000000, 0.9510565162951535312, 1.000000000000000000, 0.9510565162951535312, 1.000000000000000000, 0.9510565162951535312, 1.000000000000000000, 0.9510565162951535312, 1.000000000000000000, 0.9510565162951535312, 1.000000000000000000, 0.9510565162951535312, 1.000000000000000000, 0.9510565162951535312, 1.000000000000000000, 0.9510565162951535312, 1.000000000000000000, 0.9510565162951535312, 1.000000000000000000, 0.9510565162951535312, 1.000000000000000000, 0.9510565162951535312, 1.000000000000000000, 0.9510565162951535312, 1.000000000000000000, 0.9510565162951535312, 1.000000000000000000, 0.9510565162951535312, 1.000000000000000000, 0.9510565162951535312, 1.000000000000000000, 0.9510565162951535312, 1.000000000000000000, 0.9510565162951535312, 1.000000000000000000, 0.9510565162951535312, 1.000000000000000000, 0.9510565162951535312, 1.000000000000000000, 0.9510565162951535312, 1.000000000000000000, 0.9510565162951535312, 1.000000000000000000, 0.9510565162951535312, 1.000000000000000000, 0.9510565162951535312, 1.000000000000000000, 0.9510565162951535312, 1.000000000000000000, 0.9510565162951535312, 1.000000000000000000, 0.9510565162951535312, 1.000000000000000000, 0.9510565162951535312, 1.000000000000000000, 0.9510565162951535312, 1.000000000000000000, 0.9510565162951535312, 1.000000000000000000, 0.9510565162951535312, 1.000000000000000000, 0.9510565162951535312, 1.000000000000000000, 0.9510565162951535312, 1.000000000000000000, 0.9510565162951535312, 1.000000000000000000, 0.9510565162951535312, 1.000000000000000000, 0.9510565162951535312, 1.000000000000000000, 0.9510565162951535312, 1.000000000000000000, 0.9510565162951535312, 1.000000000000000000, 0.9510565162951535312, 1.000000000000000000, 0.9510565162951535312, 1.000000000000000000, 0.9510565162951535312, 1.000000000000000000, 0.9510565162951535312, 1.000000000000000000, 0.9510565162951535312, 1.000000000000000000, 0.9510565162951535312, 1.000000000000000000, 0.9510565162951535312, 1.000000000000000000, 0.9510565162951535312, 1.000000000000000000, 0.9510565162951535312, 1.000000000000000000, 0.9510565162951535312, 1.000000000000000000, 0.9510565162951535312, 1.000000000000000000, 0.9510565162951535312, 1.000000000000000000, 0.9510565162951535312, 1.000000000000000000, 0.9510565162951535312, 1.000000000000000000, 0.9510565162951535312, 1.000000000000000000, 0.9510565162951535312, 1.000000000000000000, 0.9510565162951535312, 1.000000000000000000, 0.9510565162951535312, 1.000000000000000000, 0.9510565162951535312, 1.000000000000000000, 0.9510565162951535312, 1.000000000000000000, 0.9510565162951535312, 1.000000000000000000, 0.9510565162951535312, 1.000000000000000000, 0.9510565162951535312, 1.000000000000000000, 0.9510565162951535312, 1.000000000000000000, 0.9510565162951535312, 1.000000000000000000, 0.9510565162951535312, 1.000000000000000000, 0.9510565162951535312, 1.000000000000000000, 0.9510565162951535312, 1.000000000000000000, 0.9510565162951535312, 1.000000000000000000, 0.9510565162951535312, 1.000000000000000000, 0.9510565162951535312, 1.000000000000000000, 0.9510565162951535312, 1.000000000000000000, 0.9510565162951535312, 1.000000000000000000, 0.9510565162951535312, 1.000000000000000000, 0.9510565162951535312, 1.000000000000000000, 0.9510565162951535312, 1.000000000000000000, 0.9510565162951535312, 1.000000000000000000, 0.9510565162951535312, 1.000000000000000000, 0.9510565162951535312, 1.000000000000000000, 0.9510565162951535312, 1.000000000000000000, 0.9510565162951535312, 1.000000000000000000, 0.9510565162951535312, 1.000000000000000000, 0.9510565162951535312, 1.000000000000000000, 0.9510565162951535312, 1.000000000000000000, 0.9510565162951535312, 1.000000000000000000, 0.9510565162951535312, 1.000000000000000000, 0.9510565162951535312, 1.000000000000000000, 0.9510565162951535312, 1.000000000000000000, 0.9510565162951535312, 1.000000000000000000, 0.9510565162951535312, 1.000000000000000000, 0.9510565162951535312, 1.000000000000000000, 0.9510565162951535312, 1.000000000000000000, 0.9510565162951535312, 1.000000000000000000, 0.9510565162951535312, 1.000000000000000000, 0.9510565162951535312, 1.000000000000000000, 0.9510565162951535312, 1.000000000000000000, 0.9510565162951535312, 1.000000000000000000, 0.9510565162951535312, 1.000000000000000000, 0.9510565162951535312, 1.000000000000000000, 0.9510565162951535312, 1.000000000000000000, 0.9510565162951535312, 1.000000000000000000, 0.9510565162951535312, 1.000000000000000000, 0.9510565162951535312, 1.000000000000000000, 0.9510565162951535312, 1.000000000000000000, 0.9510565162951535312, 1.000000000000000000, 0.9510565162951535312, 1.000000000000000000, 0.9510565162951535312, 1.000000000000000000, 0.9510565162951535312, 1.000000000000000000, 0.9510565162951535312, 1.000000000000000000, 0.9510565162951535312, 1.000000000000000000, 0.9510565162951535312, 1.000000000000000000, 0.9510565162951535312, 1.000000000000000000, 0.9510565162951535312, 1.000000000000000000, 0.9510565162951535312, 1.000000000000000000, 0.9510565162951535312, 1.000000000000000000, 0.9510565162951535312, 1.000000000000000000, 0.9510565162951535312, 1.000000000000000000, 0.9510565162951535312, 1.000000000000000000, 0.9510565162951535312, 1.000000000000000000, 0.9510565162951535312, 1.000000000000000000, 0.9510565162951535312, 1.000000000000000000) ) ) 
 REPRESENTATION_ITEM ( '' )  SURFACE ( )  );
#53595 =( NAMED_UNIT ( * ) SI_UNIT ( $, .STERADIAN. ) SOLID_ANGLE_UNIT ( ) );
#53596 = CARTESIAN_POINT ( 'NONE',  ( 23.71231517720798010, 117.4999999999999716, -9.500000000000000000 ) ) ;
#53597 = CIRCLE ( 'NONE', #42410, 1.000000000000000888 ) ;
#53598 = CARTESIAN_POINT ( 'NONE',  ( -183.6549999999999727, -7.632228543268600340, -2.479861379858950166 ) ) ;
#53599 = ADVANCED_FACE ( 'NONE', ( #57049 ), #51789, .F. ) ;
#53600 = ORIENTED_EDGE ( 'NONE', *, *, #21912, .T. ) ;
#53601 = SPHERICAL_SURFACE ( 'NONE', #27974, 1.000000000000000000 ) ;
#53602 = FACE_OUTER_BOUND ( 'NONE', #22394, .T. ) ;
#53603 = DIRECTION ( 'NONE',  ( -0.000000000000000000, -0.000000000000000000, -1.000000000000000000 ) ) ;
#53604 = SURFACE_STYLE_USAGE ( .BOTH. , #26832 ) ;
#53605 = FACE_OUTER_BOUND ( 'NONE', #20933, .T. ) ;
#53606 = CARTESIAN_POINT ( 'NONE',  ( 0.000000000000000000, 145.0570736234661524, -8.025000000000000355 ) ) ;
#53607 = EDGE_CURVE ( 'NONE', #29847, #737, #64674, .T. ) ;
#53608 = ORIENTED_EDGE ( 'NONE', *, *, #22312, .F. ) ;
#53609 = CARTESIAN_POINT ( 'NONE',  ( 12.25000000000000355, 30.99999999999998579, -3.750000000000000000 ) ) ;
#53610 = CARTESIAN_POINT ( 'NONE',  ( -94.85499999999998977, 4.716976649647094177, 6.492361379858945902 ) ) ;
#53611 = LINE ( 'NONE', #69447, #25217 ) ;
#53612 = VERTEX_POINT ( 'NONE', #21754 ) ;
#53613 = FILL_AREA_STYLE ('',( #65199 ) ) ;
#53614 = CARTESIAN_POINT ( 'NONE',  ( 1.804495846578303864, 51.08602766979955589, 2.000000000000000000 ) ) ;
#53615 = CARTESIAN_POINT ( 'NONE',  ( -71.50000000000000000, 35.92875272052971525, 7.500000000000000000 ) ) ;
#53616 = ADVANCED_FACE ( 'NONE', ( #16161 ), #65355, .F. ) ;
#53617 = DIRECTION ( 'NONE',  ( 0.000000000000000000, 1.000000000000000000, 0.000000000000000000 ) ) ;
#53618 = EDGE_LOOP ( 'NONE', ( #55837, #59140, #13025, #38275 ) ) ;
#53619 =( NAMED_UNIT ( * ) PLANE_ANGLE_UNIT ( ) SI_UNIT ( $, .RADIAN. ) );
#53620 = CARTESIAN_POINT ( 'NONE',  ( -73.64499999999998181, 4.716976649647091513, -6.492361379858946790 ) ) ;
#53621 = ORIENTED_EDGE ( 'NONE', *, *, #58396, .F. ) ;
#53622 = DIRECTION ( 'NONE',  ( 0.000000000000000000, 0.000000000000000000, 1.000000000000000000 ) ) ;
#53623 = DIRECTION ( 'NONE',  ( -0.000000000000000000, 0.000000000000000000, -1.000000000000000000 ) ) ;
#53624 = ADVANCED_FACE ( 'NONE', ( #6260 ), #38318, .F. ) ;
#53625 = ORIENTED_EDGE ( 'NONE', *, *, #24839, .F. ) ;
#53626 = DIRECTION ( 'NONE',  ( 0.000000000000000000, 0.000000000000000000, -1.000000000000000000 ) ) ;
#53627 =( GEOMETRIC_REPRESENTATION_CONTEXT ( 3 ) GLOBAL_UNCERTAINTY_ASSIGNED_CONTEXT ( ( #34796 ) ) GLOBAL_UNIT_ASSIGNED_CONTEXT ( ( #67458, #14005, #25574 ) ) REPRESENTATION_CONTEXT ( 'NONE', 'WORKASPACE' ) );
#53628 = AXIS2_PLACEMENT_3D ( 'NONE', #52376, #10137, #25594 ) ;
#53629 = DIRECTION ( 'NONE',  ( -0.000000000000000000, -0.000000000000000000, 1.000000000000000000 ) ) ;
#53630 = CARTESIAN_POINT ( 'NONE',  ( -121.4049999999999869, -2.607480562269069768, 8.024999999999991473 ) ) ;
#53631 = ORIENTED_EDGE ( 'NONE', *, *, #18451, .F. ) ;
#53632 = MECHANICAL_DESIGN_GEOMETRIC_PRESENTATION_REPRESENTATION (  '', ( #16609 ), #4145 ) ;
#53633 = CARTESIAN_POINT ( 'NONE',  ( -10.39230484541326938, 1.107695154586735509, -1.661048719744147042E-15 ) ) ;
#53634 = EDGE_LOOP ( 'NONE', ( #27856, #45539, #7132, #6100 ) ) ;
#53635 = PLANE ( 'NONE',  #13991 ) ;
#53636 = LINE ( 'NONE', #49094, #31117 ) ;
#53637 = CARTESIAN_POINT ( 'NONE',  ( -159.6570736234661751, 9.058813317711329915, 2.943386871421369566 ) ) ;
#53638 = CARTESIAN_POINT ( 'NONE',  ( -9.058813317711338797, 125.3449999999999847, 2.943386871421373563 ) ) ;
#53639 = CARTESIAN_POINT ( 'NONE',  ( -93.65707362346617515, 9.058813317711329915, 2.943386871421369566 ) ) ;
#53640 = ORIENTED_EDGE ( 'NONE', *, *, #34901, .F. ) ;
#53641 = FILL_AREA_STYLE_COLOUR ( '', #5970 ) ;
#53642 = STYLED_ITEM ( 'NONE', ( #33927 ), #67425 ) ;
#53643 = CARTESIAN_POINT ( 'NONE',  ( -52.00000000000000000, -1.926070501056209087E-14, 12.00000000000000000 ) ) ;
#53644 = LINE ( 'NONE', #48769, #11894 ) ;
#53645 = CARTESIAN_POINT ( 'NONE',  ( -139.1049999999999898, -6.826472737025115478, 4.959722759717900331 ) ) ;
#53646 =( LENGTH_UNIT ( ) NAMED_UNIT ( * ) SI_UNIT ( .MILLI., .METRE. ) );
#53647 = DIRECTION ( 'NONE',  ( 0.000000000000000000, 0.000000000000000000, -1.000000000000000000 ) ) ;
#53648 = CARTESIAN_POINT ( 'NONE',  ( 40.78947368421051323, 108.1536491499103363, 3.000000000000000000 ) ) ;
#53649 = CARTESIAN_POINT ( 'NONE',  ( -142.7949999999999875, 2.607480562269068880, -8.024999999999993250 ) ) ;
#53650 = CARTESIAN_POINT ( 'NONE',  ( -140.2450000000000045, -4.716976649647093289, -6.492361379858945902 ) ) ;
#53651 = ORIENTED_EDGE ( 'NONE', *, *, #63152, .T. ) ;
#53652 = ADVANCED_FACE ( 'NONE', ( #46901 ), #65699, .T. ) ;
#53653 = LINE ( 'NONE', #1159, #69579 ) ;
#53654 = CARTESIAN_POINT ( 'NONE',  ( 179.4361977533490347, 13.00000000000000178, 103.7004518695263044 ) ) ;
#53655 = DIRECTION ( 'NONE',  ( -0.000000000000000000, -0.000000000000000000, 1.000000000000000000 ) ) ;
#53656 = UNCERTAINTY_MEASURE_WITH_UNIT (LENGTH_MEASURE( 1.000000000000000082E-05 ), #15595, 'distance_accuracy_value', 'NONE');
#53657 = CARTESIAN_POINT ( 'NONE',  ( -53.75499999999999545, 4.716976649647091513, -6.492361379858946790 ) ) ;
#53658 = FILL_AREA_STYLE_COLOUR ( '', #22569 ) ;
#53659 = EDGE_CURVE ( 'NONE', #20313, #36746, #67526, .T. ) ;
#53660 = CARTESIAN_POINT ( 'NONE',  ( 0.000000000000000000, 161.5550000000000068, -9.525000000000000355 ) ) ;
#53661 = CARTESIAN_POINT ( 'NONE',  ( -155.0070736234661979, -8.102448949553174629, -5.886773742842741797 ) ) ;
#53662 = PRODUCT_DEFINITION_CONTEXT ( 'detailed design', #52753, 'design' ) ;
#53663 = CARTESIAN_POINT ( 'NONE',  ( -104.6929263765337907, 10.01517768586948698, -1.839758294383808571E-15 ) ) ;
#53664 = DIRECTION ( 'NONE',  ( -5.551115123125782702E-17, 0.9285714285714283811, 0.3711537444790456441 ) ) ;
#53665 = CARTESIAN_POINT ( 'NONE',  ( -152.6929263765337907, 10.01517768586948698, -1.839758294383808966E-15 ) ) ;
#53666 = CIRCLE ( 'NONE', #17741, 0.5000000000000004441 ) ;
#53667 = CARTESIAN_POINT ( 'NONE',  ( -90.05707362346616662, 0.000000000000000000, 9.524999999999991473 ) ) ;
#53668 = CARTESIAN_POINT ( 'NONE',  ( 31.00000000000000000, 42.00000000000000000, -79.00402776293826435 ) ) ;
#53669 = AXIS2_PLACEMENT_3D ( 'NONE', #34580, #51467, #12784 ) ;
#53670 = EDGE_CURVE ( 'NONE', #41380, #31338, #27022, .T. ) ;
#53671 = CARTESIAN_POINT ( 'NONE',  ( -76.94292637653380496, 0.000000000000000000, 9.524999999999991473 ) ) ;
#53672 = EDGE_CURVE ( 'NONE', #40899, #3817, #34032, .T. ) ;
#53673 = EDGE_LOOP ( 'NONE', ( #15082, #65282, #1959 ) ) ;
#53674 = DIRECTION ( 'NONE',  ( -0.000000000000000000, 1.000000000000000000, -0.000000000000000000 ) ) ;
#53675 = COLOUR_RGB ( '', 0.08235294, 0.09019608, 0.10196078) ;
#53676 = CARTESIAN_POINT ( 'NONE',  ( -7.632228543268608334, 118.9570736234661581, 2.479861379858952830 ) ) ;
#53677 = EDGE_CURVE ( 'NONE', #40049, #12184, #59633, .T. ) ;
#53678 =( NAMED_UNIT ( * ) SI_UNIT ( $, .STERADIAN. ) SOLID_ANGLE_UNIT ( ) );
#53679 = CARTESIAN_POINT ( 'NONE',  ( 22.29422224269975672, 26.00000000000000355, -27.50000000000000711 ) ) ;
#53680 = VECTOR ( 'NONE', #11704, 1000.000000000000000 ) ;
#53681 = PLANE ( 'NONE',  #7209 ) ;
#53682 = EDGE_CURVE ( 'NONE', #44352, #44514, #13255, .T. ) ;
#53683 = VERTEX_POINT ( 'NONE', #23149 ) ;
#53684 = VERTEX_POINT ( 'NONE', #17543 ) ;
#53685 = DIRECTION ( 'NONE',  ( -0.000000000000000000, -1.000000000000000000, -0.000000000000000000 ) ) ;
#53686 = DIRECTION ( 'NONE',  ( -0.000000000000000000, 0.000000000000000000, -1.000000000000000000 ) ) ;
#53687 = ORIENTED_EDGE ( 'NONE', *, *, #67691, .T. ) ;
#53688 = CARTESIAN_POINT ( 'NONE',  ( -5.598654528085806881, 131.8549999999999898, -7.705886871421374629 ) ) ;
#53689 = CARTESIAN_POINT ( 'NONE',  ( 10.00000000000000711, 50.00000000000000000, -60.00000000000000000 ) ) ;
#53690 = EDGE_CURVE ( 'NONE', #26112, #41724, #5699, .T. ) ;
#53691 = SURFACE_STYLE_FILL_AREA ( #37223 ) ;
#53692 = CARTESIAN_POINT ( 'NONE',  ( -97.34499999999998465, 7.632228543268599452, -2.479861379858951942 ) ) ;
#53693 = ORIENTED_EDGE ( 'NONE', *, *, #49662, .F. ) ;
#53694 = CARTESIAN_POINT ( 'NONE',  ( 6.962805267914501606, 153.0662478080784012, 4.200845087328706207 ) ) ;
#53695 = EDGE_CURVE ( 'NONE', #61842, #22693, #3404, .T. ) ;
#53696 = VERTEX_POINT ( 'NONE', #66744 ) ;
#53697 = CARTESIAN_POINT ( 'NONE',  ( 8.437984349512095861, 152.1929263765338192, 1.550032578732817026E-15 ) ) ;
#53698 = FILL_AREA_STYLE ('',( #32250 ) ) ;
#53699 = CYLINDRICAL_SURFACE ( 'NONE', #66611, 1.000000000000000000 ) ;
#53700 =( LENGTH_UNIT ( ) NAMED_UNIT ( * ) SI_UNIT ( .MILLI., .METRE. ) );
#53701 = FACE_OUTER_BOUND ( 'NONE', #12398, .T. ) ;
#53702 = ORIENTED_EDGE ( 'NONE', *, *, #20842, .T. ) ;
#53703 = CARTESIAN_POINT ( 'NONE',  ( 10.42000000000000526, 0.000000000000000000, 12.50000000000000000 ) ) ;
#53704 = DIRECTION ( 'NONE',  ( 0.000000000000000000, 0.000000000000000000, 1.000000000000000000 ) ) ;
#53705 = FACE_OUTER_BOUND ( 'NONE', #35556, .T. ) ;
#53706 = CIRCLE ( 'NONE', #53756, 15.00000000000000000 ) ;
#53707 = CARTESIAN_POINT ( 'NONE',  ( -8.750000000000001776, 25.24999999999998934, -3.750000000000000000 ) ) ;
#53708 = CARTESIAN_POINT ( 'NONE',  ( -2.139492287038055877E-14, 27.74999999999994316, 4.000000000000000000 ) ) ;
#53709 = SPHERICAL_SURFACE ( 'NONE', #25027, 0.2500000000000000000 ) ;
#53710 = CARTESIAN_POINT ( 'NONE',  ( -54.49999999999999289, -1.956686671034893189E-14, 6.500000000000000000 ) ) ;
#53711 = CARTESIAN_POINT ( 'NONE',  ( 24.00000000000000355, 36.75000000000000000, -4.000000000000000000 ) ) ;
#53712 = CARTESIAN_POINT ( 'NONE',  ( -8.253986449296890626, 153.4602809114455511, -1.986321737243838648 ) ) ;
#53713 = ORIENTED_EDGE ( 'NONE', *, *, #54397, .F. ) ;
#53714 = MECHANICAL_DESIGN_GEOMETRIC_PRESENTATION_REPRESENTATION (  '', ( #3097 ), #24480 ) ;
#53715 = ORIENTED_EDGE ( 'NONE', *, *, #43019, .T. ) ;
#53716 = PLANE ( 'NONE',  #1346 ) ;
#53717 = LINE ( 'NONE', #65321, #59020 ) ;
#53718 = CARTESIAN_POINT ( 'NONE',  ( -171.0570736234661808, 0.000000000000000000, 9.524999999999991473 ) ) ;
#53719 = SURFACE_STYLE_USAGE ( .BOTH. , #63926 ) ;
#53720 = ORIENTED_EDGE ( 'NONE', *, *, #30059, .T. ) ;
#53721 = CARTESIAN_POINT ( 'NONE',  ( -165.3549999999999898, -4.716976649647093289, -6.492361379858945902 ) ) ;
#53722 = CARTESIAN_POINT ( 'NONE',  ( -22.25000000000000711, 33.99999999999999289, 4.000000000000000000 ) ) ;
#53723 = CARTESIAN_POINT ( 'NONE',  ( -170.6949999999999932, -8.437984349512085203, 5.166775262442717831E-16 ) ) ;
#53724 = AXIS2_PLACEMENT_3D ( 'NONE', #3265, #24752, #46276 ) ;
#53725 = CARTESIAN_POINT ( 'NONE',  ( -164.6949999999999932, -8.437984349512086979, 5.166775262442717831E-16 ) ) ;
#53726 = ORIENTED_EDGE ( 'NONE', *, *, #41649, .F. ) ;
#53727 = STYLED_ITEM ( 'NONE', ( #55075 ), #1109 ) ;
#53728 = EDGE_CURVE ( 'NONE', #20856, #42614, #50568, .T. ) ;
#53729 = CARTESIAN_POINT ( 'NONE',  ( -89.24292637653380211, 5.598654528085804216, 7.705886871421366635 ) ) ;
#53730 = DIRECTION ( 'NONE',  ( -0.000000000000000000, -0.000000000000000000, -1.000000000000000000 ) ) ;
#53731 = CARTESIAN_POINT ( 'NONE',  ( -14.17503136354020477, 10.93867306445503651, -4.934238260594468350 ) ) ;
#53732 = CARTESIAN_POINT ( 'NONE',  ( -83.75499999999998124, 4.716976649647091513, -6.492361379858946790 ) ) ;
#53733 = DIRECTION ( 'NONE',  ( 0.000000000000000000, 0.000000000000000000, -1.000000000000000000 ) ) ;
#53734 = CARTESIAN_POINT ( 'NONE',  ( -195.0000000000000000, 0.000000000000000000, 9.524999999999991473 ) ) ;
#53736 = PLANE ( 'NONE',  #41611 ) ;
#53735 = AXIS2_PLACEMENT_3D ( 'NONE', #28802, #39755, #1688 ) ;
#53737 = CARTESIAN_POINT ( 'NONE',  ( -78.74499999999997613, 4.716976649647094177, 6.492361379858945902 ) ) ;
#53738 = CARTESIAN_POINT ( 'NONE',  ( -9.058813317711338797, 141.4549999999999841, 2.943386871421373563 ) ) ;
#53739 = CARTESIAN_POINT ( 'NONE',  ( 6.767634268437467959, -2.278113600022081631, 0.1324414877861178896 ) ) ;
#53740 = CARTESIAN_POINT ( 'NONE',  ( 0.7098900097155632638, -7.000000000000000888, -2.373649839567916678E-14 ) ) ;
#53741 = CARTESIAN_POINT ( 'NONE',  ( -72.50000000000001421, 35.92875272052971525, -10.00000000000000000 ) ) ;
#53742 = UNCERTAINTY_MEASURE_WITH_UNIT (LENGTH_MEASURE( 1.000000000000000082E-05 ), #37382, 'distance_accuracy_value', 'NONE');
#53743 =( LENGTH_UNIT ( ) NAMED_UNIT ( * ) SI_UNIT ( .MILLI., .METRE. ) );
#53744 = ORIENTED_EDGE ( 'NONE', *, *, #36160, .T. ) ;
#53745 = EDGE_CURVE ( 'NONE', #42007, #54981, #50227, .T. ) ;
#53746 = PRESENTATION_STYLE_ASSIGNMENT (( #21058 ) ) ;
#53747 = EDGE_CURVE ( 'NONE', #27816, #20613, #2292, .T. ) ;
#53748 = AXIS2_PLACEMENT_3D ( 'NONE', #65137, #34519, #7781 ) ;
#53749 = ADVANCED_FACE ( 'NONE', ( #60073 ), #40044, .F. ) ;
#53750 = CARTESIAN_POINT ( 'NONE',  ( 179.4098300562505415, 0.000000000000000000, 0.000000000000000000 ) ) ;
#53751 = DIRECTION ( 'NONE',  ( -0.000000000000000000, -0.000000000000000000, -1.000000000000000000 ) ) ;
#53752 = ADVANCED_FACE ( 'NONE', ( #49537 ), #61890, .F. ) ;
#53753 = DIRECTION ( 'NONE',  ( -1.000000000000000000, -0.000000000000000000, -0.000000000000000000 ) ) ;
#53754 = CARTESIAN_POINT ( 'NONE',  ( 1.000000000000000000, 43.00000000000000000, 35.50000000000000000 ) ) ;
#53755 = ORIENTED_EDGE ( 'NONE', *, *, #22327, .F. ) ;
#53756 = AXIS2_PLACEMENT_3D ( 'NONE', #48635, #15568, #21868 ) ;
#53757 = ORIENTED_EDGE ( 'NONE', *, *, #66891, .T. ) ;
#53758 = PLANE ( 'NONE',  #15013 ) ;
#53759 = SURFACE_STYLE_FILL_AREA ( #22110 ) ;
#53760 = VECTOR ( 'NONE', #26614, 1000.000000000000000 ) ;
#53761 = CYLINDRICAL_SURFACE ( 'NONE', #62941, 1.000000000000000888 ) ;
#53762 = DIRECTION ( 'NONE',  ( 0.000000000000000000, 0.000000000000000000, 1.000000000000000000 ) ) ;
#53763 = CARTESIAN_POINT ( 'NONE',  ( -69.20707362346617231, 3.094860106618433360, 9.524999999999991473 ) ) ;
#53764 = ADVANCED_FACE ( 'NONE', ( #22799 ), #17206, .F. ) ;
#53765 = ORIENTED_EDGE ( 'NONE', *, *, #47730, .T. ) ;
#53766 = CARTESIAN_POINT ( 'NONE',  ( -108.3549999999999898, -4.716976649647093289, -6.492361379858945902 ) ) ;
#53767 = ORIENTED_EDGE ( 'NONE', *, *, #45101, .F. ) ;
#53768 = ORIENTED_EDGE ( 'NONE', *, *, #14311, .F. ) ;
#53769 = CARTESIAN_POINT ( 'NONE',  ( 0.000000000000000000, 0.000000000000000000, 0.000000000000000000 ) ) ;
#53770 = ORIENTED_EDGE ( 'NONE', *, *, #8349, .F. ) ;
#53771 = CARTESIAN_POINT ( 'NONE',  ( 9.566487832665400148, 1.863712308906143811, 1.430357023834058161 ) ) ;
#53772 = CARTESIAN_POINT ( 'NONE',  ( -10.01517768586949231, 155.1949999999999648, -6.132527647946036459E-16 ) ) ;
#53773 = FILL_AREA_STYLE ('',( #48205 ) ) ;
#53774 = VERTEX_POINT ( 'NONE', #12208 ) ;
#53775 = FACE_OUTER_BOUND ( 'NONE', #52691, .T. ) ;
#53776 = SURFACE_STYLE_USAGE ( .BOTH. , #10546 ) ;
#53777 = DIRECTION ( 'NONE',  ( 0.000000000000000000, 0.000000000000000000, -1.000000000000000000 ) ) ;
#53778 = EDGE_LOOP ( 'NONE', ( #51429, #8467, #48676 ) ) ;
#53779 = CARTESIAN_POINT ( 'NONE',  ( -2.607480562269075097, 124.2929263765337993, 8.025000000000000355 ) ) ;
#53780 = CARTESIAN_POINT ( 'NONE',  ( 39.24999999999999289, 16.24999999999997513, 3.750000000000000000 ) ) ;
#53781 = CARTESIAN_POINT ( 'NONE',  ( -75.46465235827693618, 36.01723441224693545, -9.608246556350810152 ) ) ;
#53782 = AXIS2_PLACEMENT_3D ( 'NONE', #24554, #46428, #57997 ) ;
#53783 = CARTESIAN_POINT ( 'NONE',  ( 2.607480562269051116, 124.5929263765338106, 8.025000000000016342 ) ) ;
#53784 = DIRECTION ( 'NONE',  ( -1.000000000000000000, 0.000000000000000000, 0.000000000000000000 ) ) ;
#53785 = ADVANCED_FACE ( 'NONE', ( #33684 ), #6955, .T. ) ;
#53786 = ORIENTED_EDGE ( 'NONE', *, *, #36940, .F. ) ;
#53787 = DIRECTION ( 'NONE',  ( -1.000000000000000000, 0.000000000000000000, -0.000000000000000000 ) ) ;
#53788 = ORIENTED_EDGE ( 'NONE', *, *, #60487, .T. ) ;
#53789 = CARTESIAN_POINT ( 'NONE',  ( -52.79292637653378506, -3.094860106618429807, 9.524999999999991473 ) ) ;
#53790 = DIRECTION ( 'NONE',  ( 1.000000000000000000, 0.000000000000000000, 0.000000000000000000 ) ) ;
#53791 = CARTESIAN_POINT ( 'NONE',  ( 74.50000000000000000, -2.135340797662720349E-14, 6.999999999999999112 ) ) ;
#53792 = CARTESIAN_POINT ( 'NONE',  ( -140.1550000000000011, 7.632228543268600340, 2.479861379858949277 ) ) ;
#53793 = PRESENTATION_STYLE_ASSIGNMENT (( #65032 ) ) ;
#53794 = EDGE_CURVE ( 'NONE', #2846, #43100, #40729, .T. ) ;
#53795 = UNCERTAINTY_MEASURE_WITH_UNIT (LENGTH_MEASURE( 1.000000000000000082E-05 ), #32214, 'distance_accuracy_value', 'NONE');
#53796 = AXIS2_PLACEMENT_3D ( 'NONE', #59024, #64651, #52391 ) ;
#53797 = FILL_AREA_STYLE ('',( #33060 ) ) ;
#53798 = CARTESIAN_POINT ( 'NONE',  ( 40.78947371891847240, 108.1536491252660568, 3.151596837137058404 ) ) ;
#53799 = EDGE_LOOP ( 'NONE', ( #45676, #50361, #33527, #30295, #14831 ) ) ;
#53800 = EDGE_LOOP ( 'NONE', ( #30237, #34612, #27101, #11046 ) ) ;
#53801 = CARTESIAN_POINT ( 'NONE',  ( -190.0000000000000000, 0.000000000000000000, 0.000000000000000000 ) ) ;
#53802 = CIRCLE ( 'NONE', #23466, 110.0000000000000142 ) ;
#53803 = SURFACE_STYLE_USAGE ( .BOTH. , #20427 ) ;
#53804 = CARTESIAN_POINT ( 'NONE',  ( -57.65499999999998693, -7.632228543268600340, -2.479861379858950166 ) ) ;
#53805 = ORIENTED_EDGE ( 'NONE', *, *, #51478, .F. ) ;
#53806 =( LENGTH_UNIT ( ) NAMED_UNIT ( * ) SI_UNIT ( .MILLI., .METRE. ) );
#53807 = DIRECTION ( 'NONE',  ( -1.000000000000000000, 0.000000000000000000, 0.000000000000000000 ) ) ;
#53808 = CARTESIAN_POINT ( 'NONE',  ( 0.000000000000000000, 154.9999999999999716, 0.000000000000000000 ) ) ;
#53809 = PLANE ( 'NONE',  #16721 ) ;
#53810 = PRESENTATION_LAYER_ASSIGNMENT (  '', '', ( #14494 ) ) ;
#53811 = VECTOR ( 'NONE', #54462, 1000.000000000000000 ) ;
#53812 = CARTESIAN_POINT ( 'NONE',  ( -75.46551724137930250, 63.49197145334878201, -10.00000000000000000 ) ) ;
#53813 = DIRECTION ( 'NONE',  ( 0.000000000000000000, 0.000000000000000000, 1.000000000000000000 ) ) ;
#53814 = MECHANICAL_DESIGN_GEOMETRIC_PRESENTATION_REPRESENTATION (  '', ( #67277 ), #62792 ) ;
#53815 = EDGE_LOOP ( 'NONE', ( #56098, #60333, #41426, #11405 ) ) ;
#53816 = FACE_OUTER_BOUND ( 'NONE', #8470, .T. ) ;
#53817 = DIRECTION ( 'NONE',  ( 0.000000000000000000, 0.000000000000000000, 1.000000000000000000 ) ) ;
#53818 = CARTESIAN_POINT ( 'NONE',  ( 108.3664351561509562, 14.00000000000000000, -18.43563588791579377 ) ) ;
#53819 = AXIS2_PLACEMENT_3D ( 'NONE', #13165, #34622, #2202 ) ;
#53820 = FILL_AREA_STYLE ('',( #42985 ) ) ;
#53821 = CARTESIAN_POINT ( 'NONE',  ( -106.6449999999999960, 4.716976649647091513, -6.492361379858946790 ) ) ;
#53822 = CARTESIAN_POINT ( 'NONE',  ( -5.598654528085808657, 111.7549999999999955, 7.705886871421373741 ) ) ;
#53823 = CARTESIAN_POINT ( 'NONE',  ( -84.44499999999999318, 0.000000000000000000, 8.024999999999991473 ) ) ;
#53824 = EDGE_CURVE ( 'NONE', #32384, #7642, #25541, .T. ) ;
#53825 = STYLED_ITEM ( 'NONE', ( #68729 ), #14964 ) ;
#53826 = CARTESIAN_POINT ( 'NONE',  ( 6.999798566743344885, 2.607462097171131976, -12.22502112111942196 ) ) ;
#53827 = DIRECTION ( 'NONE',  ( 0.000000000000000000, 0.000000000000000000, 1.000000000000000000 ) ) ;
#53828 = UNCERTAINTY_MEASURE_WITH_UNIT (LENGTH_MEASURE( 1.000000000000000082E-05 ), #15468, 'distance_accuracy_value', 'NONE');
#53829 = CIRCLE ( 'NONE', #11145, 0.5000000000000004441 ) ;
#53830 = FACE_OUTER_BOUND ( 'NONE', #25649, .T. ) ;
#53831 = ORIENTED_EDGE ( 'NONE', *, *, #67769, .T. ) ;
#53832 = EDGE_CURVE ( 'NONE', #55926, #32866, #62490, .T. ) ;
#53833 = CARTESIAN_POINT ( 'NONE',  ( -133.3429263765337964, -9.058813317711329915, 2.943386871421371787 ) ) ;
#53834 = SURFACE_STYLE_FILL_AREA ( #25708 ) ;
#53835 = CARTESIAN_POINT ( 'NONE',  ( -150.7449999999999761, 4.716976649647094177, 6.492361379858945902 ) ) ;
#53836 = AXIS2_PLACEMENT_3D ( 'NONE', #33079, #27418, #5980 ) ;
#53837 = EDGE_CURVE ( 'NONE', #8600, #49132, #63002, .T. ) ;
#53838 = FILL_AREA_STYLE_COLOUR ( '', #66637 ) ;
#53839 =( NAMED_UNIT ( * ) PLANE_ANGLE_UNIT ( ) SI_UNIT ( $, .RADIAN. ) );
#53840 = ORIENTED_EDGE ( 'NONE', *, *, #32891, .T. ) ;
#53841 = ORIENTED_EDGE ( 'NONE', *, *, #67338, .F. ) ;
#53842 = PRESENTATION_LAYER_ASSIGNMENT (  '', '', ( #19032 ) ) ;
#53843 = STYLED_ITEM ( 'NONE', ( #67047 ), #58874 ) ;
#53844 = PLANE ( 'NONE',  #56111 ) ;
#53845 = DIRECTION ( 'NONE',  ( -0.000000000000000000, 1.000000000000000000, -0.000000000000000000 ) ) ;
#53846 = CIRCLE ( 'NONE', #23513, 9.525000000000000355 ) ;
#53847 = CARTESIAN_POINT ( 'NONE',  ( 9.827790563157511022E-16, 87.30187232391182306, -8.025000000000000355 ) ) ;
#53848 = CARTESIAN_POINT ( 'NONE',  ( -45.00000000000000000, 8.380821545698690755, 5.549835146672248420 ) ) ;
#53850 = EDGE_CURVE ( 'NONE', #16782, #43736, #52325, .T. ) ;
#53849 = PRESENTATION_STYLE_ASSIGNMENT (( #17305 ) ) ;
#53851 = EDGE_LOOP ( 'NONE', ( #54958, #46432, #38771, #8574 ) ) ;
#53852 = CARTESIAN_POINT ( 'NONE',  ( -155.4549999999999841, 7.632228543268599452, -2.479861379858951942 ) ) ;
#53853 = ORIENTED_EDGE ( 'NONE', *, *, #39642, .F. ) ;
#53854 = FILL_AREA_STYLE ('',( #59128 ) ) ;
#53855 = CARTESIAN_POINT ( 'NONE',  ( -141.2070736234666697, 3.094860106627038032, 9.524999999993740474 ) ) ;
#53856 = ORIENTED_EDGE ( 'NONE', *, *, #47139, .T. ) ;
#53857 = AXIS2_PLACEMENT_3D ( 'NONE', #11082, #21287, #37543 ) ;
#53858 = VECTOR ( 'NONE', #33301, 1000.000000000000000 ) ;
#53859 = DIRECTION ( 'NONE',  ( -0.000000000000000000, -0.000000000000000000, -1.000000000000000000 ) ) ;
#53860 = PRESENTATION_STYLE_ASSIGNMENT (( #31354 ) ) ;
#53861 = AXIS2_PLACEMENT_3D ( 'NONE', #56808, #58186, #31426 ) ;
#53862 = CARTESIAN_POINT ( 'NONE',  ( 9.058813317711337021, 120.5449999999999875, 2.943386871421375783 ) ) ;
#53863 = PRESENTATION_LAYER_ASSIGNMENT (  '', '', ( #58338 ) ) ;
#53864 = VERTEX_POINT ( 'NONE', #68139 ) ;
#53865 = CARTESIAN_POINT ( 'NONE',  ( 10.01517768586949408, 133.8049999999999784, 1.839758294383810543E-15 ) ) ;
#53866 = CARTESIAN_POINT ( 'NONE',  ( -61.70499999999997698, 2.607480562269072433, 8.024999999999991473 ) ) ;
#53867 = CARTESIAN_POINT ( 'NONE',  ( -121.9449999999999932, -9.827790563157499189E-16, -8.024999999999991473 ) ) ;
#53868 = CIRCLE ( 'NONE', #29144, 5.000000000000000000 ) ;
#53869 = DIRECTION ( 'NONE',  ( -0.000000000000000000, -0.000000000000000000, 1.000000000000000000 ) ) ;
#53870 = B_SPLINE_CURVE_WITH_KNOTS ( 'NONE', 3,
 ( #65009, #54115, #49210, #915, #54463, #38690, #32657, #12583 ),
 .UNSPECIFIED., .F., .F.,
 ( 4, 2, 2, 4 ),
 ( 2.544316211736544463E-07, 0.002094919859796806009, 0.003142252573884622008, 0.004189585287972438440 ),
 .UNSPECIFIED. ) ;
#53871 = ORIENTED_EDGE ( 'NONE', *, *, #39756, .F. ) ;
#53872 = CARTESIAN_POINT ( 'NONE',  ( 3.094860106618431583, 148.2050000000000125, 9.525000000000000355 ) ) ;
#53873 = CARTESIAN_POINT ( 'NONE',  ( 57.00000000000000000, 0.9999999999999991118, -60.00402776293827145 ) ) ;
#53874 = UNCERTAINTY_MEASURE_WITH_UNIT (LENGTH_MEASURE( 1.000000000000000082E-05 ), #15944, 'distance_accuracy_value', 'NONE');
#53875 = SURFACE_STYLE_FILL_AREA ( #691 ) ;
#53876 = DIRECTION ( 'NONE',  ( 0.000000000000000000, 0.000000000000000000, -1.000000000000000000 ) ) ;
#53877 = DIRECTION ( 'NONE',  ( -1.000000000000000000, -0.000000000000000000, -0.000000000000000000 ) ) ;
#53878 = EDGE_LOOP ( 'NONE', ( #14711, #33047, #68143, #1710 ) ) ;
#53879 = VECTOR ( 'NONE', #56695, 1000.000000000000000 ) ;
#53880 = DIRECTION ( 'NONE',  ( -1.000000000000000000, 1.224646799147349509E-16, 0.000000000000000000 ) ) ;
#53881 = CARTESIAN_POINT ( 'NONE',  ( -172.7049999999999841, 2.607480562269073321, 8.024999999999991473 ) ) ;
#53882 = VERTEX_POINT ( 'NONE', #25893 ) ;
#53883 = DIRECTION ( 'NONE',  ( -0.000000000000000000, -1.000000000000000000, -0.000000000000000000 ) ) ;
#53884 = UNCERTAINTY_MEASURE_WITH_UNIT (LENGTH_MEASURE( 1.000000000000000082E-05 ), #50006, 'distance_accuracy_value', 'NONE');
#53885 = COLOUR_RGB ( '', 0.72549020, 0.75294118, 0.79215686) ;
#53886 = SURFACE_STYLE_USAGE ( .BOTH. , #58833 ) ;
#53887 = ORIENTED_EDGE ( 'NONE', *, *, #47398, .F. ) ;
#53888 = STYLED_ITEM ( 'NONE', ( #61182 ), #69187 ) ;
#53889 = SURFACE_STYLE_USAGE ( .BOTH. , #42368 ) ;
#53890 = CARTESIAN_POINT ( 'NONE',  ( -83.15499999999998693, 7.632228543268600340, 2.479861379858949277 ) ) ;
#53891 = ORIENTED_EDGE ( 'NONE', *, *, #16794, .F. ) ;
#53892 = CARTESIAN_POINT ( 'NONE',  ( 24.21231517720798010, 113.4999999999999858, -7.500000000000000000 ) ) ;
#53893 = VECTOR ( 'NONE', #65917, 1000.000000000000000 ) ;
#53894 = PRESENTATION_LAYER_ASSIGNMENT (  '', '', ( #41581 ) ) ;
#53895 =( BOUNDED_CURVE ( )  B_SPLINE_CURVE ( 2, ( #30096, #25183, #19553, #57543, #46700, #36104, #19893, #41391, #48896, #15485, #15150 ),
 .UNSPECIFIED., .F., .F. ) 
 B_SPLINE_CURVE_WITH_KNOTS ( ( 3, 2, 2, 2, 2, 3 ),
 ( 0.5543478260869435514, 0.5565217391304217998, 0.5586956521739000481, 0.5608695652173781854, 0.5630434782608564337, 0.5652173913043346820 ),
 .UNSPECIFIED. ) 
 CURVE ( )  GEOMETRIC_REPRESENTATION_ITEM ( )  RATIONAL_B_SPLINE_CURVE ( ( 1.000000000000292433, 0.9510565162948610984, 1.000000000000000000, 0.9510565162951535312, 1.000000000000000000, 0.9510565162951535312, 1.000000000000000000, 0.9510565162951535312, 1.000000000000000000, 0.9510565162954485174, 0.9999999999997050137 ) ) 
 REPRESENTATION_ITEM ( '' )  );
#53896 = CARTESIAN_POINT ( 'NONE',  ( -70.10707362346617799, 8.102448949553171076, -5.886773742842744461 ) ) ;
#53897 = AXIS2_PLACEMENT_3D ( 'NONE', #18015, #55655, #39865 ) ;
#53898 = ORIENTED_EDGE ( 'NONE', *, *, #35035, .F. ) ;
#53899 = DIRECTION ( 'NONE',  ( -1.000000000000000000, 0.000000000000000000, 0.000000000000000000 ) ) ;
#53900 = FACE_OUTER_BOUND ( 'NONE', #51967, .T. ) ;
#53901 = CARTESIAN_POINT ( 'NONE',  ( -101.9049999999999869, 2.607480562269068880, -8.024999999999993250 ) ) ;
#53902 = CARTESIAN_POINT ( 'NONE',  ( -1.166476076187854022E-15, 131.9449999999999932, 9.525000000000000355 ) ) ;
#53903 = CARTESIAN_POINT ( 'NONE',  ( -119.8449999999999989, -7.632228543268599452, 2.479861379858951054 ) ) ;
#53904 = EDGE_CURVE ( 'NONE', #21935, #42181, #20274, .T. ) ;
#53905 = STYLED_ITEM ( 'NONE', ( #42238 ), #20977 ) ;
#53906 = VECTOR ( 'NONE', #49283, 1000.000000000000000 ) ;
#53907 = LINE ( 'NONE', #27511, #16828 ) ;
#53908 = STYLED_ITEM ( 'NONE', ( #44399 ), #34243 ) ;
#53910 =( NAMED_UNIT ( * ) SI_UNIT ( $, .STERADIAN. ) SOLID_ANGLE_UNIT ( ) );
#53909 = CARTESIAN_POINT ( 'NONE',  ( -32.76851741822989084, -9.107254030102708953, -2.000000000007038370 ) ) ;
#53911 = AXIS2_PLACEMENT_3D ( 'NONE', #65696, #63367, #27685 ) ;
#53912 = CARTESIAN_POINT ( 'NONE',  ( -164.8429263765337964, 9.058813317711329915, -2.943386871421373119 ) ) ;
#53913 = CARTESIAN_POINT ( 'NONE',  ( -177.1450000000000102, -4.716976649647092401, 6.492361379858946790 ) ) ;
#53914 = VECTOR ( 'NONE', #27944, 1000.000000000000000 ) ;
#53915 = EDGE_CURVE ( 'NONE', #8408, #64066, #41703, .T. ) ;
#53916 = SURFACE_STYLE_USAGE ( .BOTH. , #4696 ) ;
#53917 = EDGE_CURVE ( 'NONE', #40178, #17236, #65263, .T. ) ;
#53918 = COLOUR_RGB ( '', 0.31764706, 0.68627451, 0.89019608) ;
#53919 = CARTESIAN_POINT ( 'NONE',  ( 0.000000000000000000, 0.000000000000000000, 0.000000000000000000 ) ) ;
#53920 = EDGE_LOOP ( 'NONE', ( #57885, #17031, #24379, #63882 ) ) ;
#53921 = CARTESIAN_POINT ( 'NONE',  ( 2.000000000000015099, 26.00000000000000355, 20.49999999999999645 ) ) ;
#53922 = DIRECTION ( 'NONE',  ( 0.000000000000000000, -1.000000000000000000, 0.000000000000000000 ) ) ;
#53923 = ORIENTED_EDGE ( 'NONE', *, *, #56829, .F. ) ;
#53924 = ADVANCED_FACE ( 'NONE', ( #31161 ), #19220, .F. ) ;
#53925 = CARTESIAN_POINT ( 'NONE',  ( -73.94292637653379074, 0.000000000000000000, 9.524999999999991473 ) ) ;
#53926 = CIRCLE ( 'NONE', #41615, 1.000000000000000888 ) ;
#53927 = PLANE ( 'NONE',  #475 ) ;
#53928 = DIRECTION ( 'NONE',  ( -1.000000000000000000, -0.000000000000000000, -0.000000000000000000 ) ) ;
#53929 = EDGE_CURVE ( 'NONE', #54030, #11506, #46003, .T. ) ;
#53930 = DIRECTION ( 'NONE',  ( 0.000000000000000000, 0.000000000000000000, -1.000000000000000000 ) ) ;
#53931 = CARTESIAN_POINT ( 'NONE',  ( -180.3549999999999898, -4.716976649647093289, -6.492361379858945902 ) ) ;
#53932 = ORIENTED_EDGE ( 'NONE', *, *, #67944, .F. ) ;
#53934 = FACE_OUTER_BOUND ( 'NONE', #25102, .T. ) ;
#53933 = ADVANCED_BREP_SHAPE_REPRESENTATION ( '', ( #27320, #42840 ), #60796 ) ;
#53935 = CARTESIAN_POINT ( 'NONE',  ( 35.99999999999999289, 5.000000000000000000, -72.00402776293825013 ) ) ;
#53936 = SURFACE_STYLE_USAGE ( .BOTH. , #11382 ) ;
#53937 = CARTESIAN_POINT ( 'NONE',  ( 4.716976649647096842, 140.8570736234661638, 6.492361379858953896 ) ) ;
#53938 = VERTEX_POINT ( 'NONE', #62140 ) ;
#53939 = AXIS2_PLACEMENT_3D ( 'NONE', #45746, #67162, #61869 ) ;
#53940 = CARTESIAN_POINT ( 'NONE',  ( 0.000000000000000000, 137.9429263765338192, -8.025000000000000355 ) ) ;
#53941 = CARTESIAN_POINT ( 'NONE',  ( -94.25499999999999545, -4.716976649647092401, 6.492361379858946790 ) ) ;
#53942 = UNCERTAINTY_MEASURE_WITH_UNIT (LENGTH_MEASURE( 1.000000000000000082E-05 ), #29352, 'distance_accuracy_value', 'NONE');
#53943 = SURFACE_SIDE_STYLE ('',( #42765 ) ) ;
#53944 = ORIENTED_EDGE ( 'NONE', *, *, #16630, .T. ) ;
#53945 = FILL_AREA_STYLE_COLOUR ( '', #41174 ) ;
#53946 = SURFACE_STYLE_USAGE ( .BOTH. , #52939 ) ;
#53947 = DIRECTION ( 'NONE',  ( -0.000000000000000000, 1.000000000000000000, -0.000000000000000000 ) ) ;
#53948 = PRESENTATION_STYLE_ASSIGNMENT (( #10711 ) ) ;
#53949 = MECHANICAL_DESIGN_GEOMETRIC_PRESENTATION_REPRESENTATION (  '', ( #64050 ), #2219 ) ;
#53950 = ORIENTED_EDGE ( 'NONE', *, *, #48798, .F. ) ;
#53951 = CARTESIAN_POINT ( 'NONE',  ( -60.59499999999997755, 2.607480562269073321, 8.024999999999991473 ) ) ;
#53953 = EDGE_LOOP ( 'NONE', ( #8409, #2683, #43446, #57770 ) ) ;
#53952 = COLOUR_RGB ( '', 0.31764706, 0.68627451, 0.89019608) ;
#53954 = LINE ( 'NONE', #21976, #16015 ) ;
#53955 = CARTESIAN_POINT ( 'NONE',  ( -49.34292637653378222, -9.058813317711329915, 2.943386871421371787 ) ) ;
#53956 = CARTESIAN_POINT ( 'NONE',  ( -126.0570736234661808, 0.000000000000000000, 9.524999999999991473 ) ) ;
#53957 = AXIS2_PLACEMENT_3D ( 'NONE', #16436, #37904, #59635 ) ;
#53958 = ORIENTED_EDGE ( 'NONE', *, *, #45924, .T. ) ;
#53959 = SURFACE_SIDE_STYLE ('',( #83 ) ) ;
#53960 = VECTOR ( 'NONE', #11721, 1000.000000000000000 ) ;
#53961 = ORIENTED_EDGE ( 'NONE', *, *, #43143, .F. ) ;
#53962 = FACE_OUTER_BOUND ( 'NONE', #28398, .T. ) ;
#53963 = CARTESIAN_POINT ( 'NONE',  ( -74.99999999999998579, 36.00000000000000711, -41.30495168499704306 ) ) ;
#53964 = CARTESIAN_POINT ( 'NONE',  ( -115.2549999999999955, -4.716976649647092401, 6.492361379858946790 ) ) ;
#53965 = VERTEX_POINT ( 'NONE', #13965 ) ;
#53966 = FILL_AREA_STYLE ('',( #27573 ) ) ;
#53967 = PRESENTATION_LAYER_ASSIGNMENT (  '', '', ( #57347 ) ) ;
#53968 = ORIENTED_EDGE ( 'NONE', *, *, #30799, .F. ) ;
#53969 = FACE_BOUND ( 'NONE', #65359, .T. ) ;
#53971 = VECTOR ( 'NONE', #18548, 1000.000000000000000 ) ;
#53970 = DIRECTION ( 'NONE',  ( -1.000000000000000000, -0.000000000000000000, -0.000000000000000000 ) ) ;
#53972 = CARTESIAN_POINT ( 'NONE',  ( -158.4570736234661581, -9.058813317711329915, 2.943386871421371787 ) ) ;
#53973 = AXIS2_PLACEMENT_3D ( 'NONE', #43935, #65344, #17197 ) ;
#53974 = CARTESIAN_POINT ( 'NONE',  ( 8.102448949553181734, 135.9949999999999477, -5.886773742842746238 ) ) ;
#53975 = CARTESIAN_POINT ( 'NONE',  ( -94.70707362346618652, -3.094860106618431139, -9.524999999999991473 ) ) ;
#53976 = AXIS2_PLACEMENT_3D ( 'NONE', #23909, #63535, #46359 ) ;
#53977 = DIRECTION ( 'NONE',  ( 0.000000000000000000, 0.000000000000000000, 1.000000000000000000 ) ) ;
#53978 = ORIENTED_EDGE ( 'NONE', *, *, #17080, .F. ) ;
#53979 =( GEOMETRIC_REPRESENTATION_CONTEXT ( 3 ) GLOBAL_UNCERTAINTY_ASSIGNED_CONTEXT ( ( #41773 ) ) GLOBAL_UNIT_ASSIGNED_CONTEXT ( ( #63525, #69164, #44198 ) ) REPRESENTATION_CONTEXT ( 'NONE', 'WORKASPACE' ) );
#53980 = DIRECTION ( 'NONE',  ( 0.000000000000000000, 0.000000000000000000, -1.000000000000000000 ) ) ;
#53982 = PRESENTATION_STYLE_ASSIGNMENT (( #106 ) ) ;
#53981 = FILL_AREA_STYLE ('',( #28630 ) ) ;
#53983 = CARTESIAN_POINT ( 'NONE',  ( 72.50000000000000000, 14.49137674618942562, 9.500000000000000000 ) ) ;
#53984 = B_SPLINE_CURVE_WITH_KNOTS ( 'NONE', 3,
 ( #46204, #30662, #25056, #67989 ),
 .UNSPECIFIED., .F., .F.,
 ( 4, 4 ),
 ( 0.000000000000000000, 1.000000000000000000 ),
 .UNSPECIFIED. ) ;
#53985 = CARTESIAN_POINT ( 'NONE',  ( -142.5549999999999784, 0.000000000000000000, 8.024999999999991473 ) ) ;
#53986 = LINE ( 'NONE', #47385, #55483 ) ;
#53987 =( NAMED_UNIT ( * ) PLANE_ANGLE_UNIT ( ) SI_UNIT ( $, .RADIAN. ) );
#53988 = CARTESIAN_POINT ( 'NONE',  ( 53.24999999999999289, 27.74999999999998579, -3.750000000000000000 ) ) ;
#53989 = CARTESIAN_POINT ( 'NONE',  ( -148.3449999999999989, 7.632228543268599452, -2.479861379858951942 ) ) ;
#53990 = ADVANCED_FACE ( 'NONE', ( #30466 ), #35436, .F. ) ;
#53991 = CARTESIAN_POINT ( 'NONE',  ( -134.0949999999999704, -2.607480562269071545, -8.024999999999991473 ) ) ;
#53992 = ORIENTED_EDGE ( 'NONE', *, *, #43869, .F. ) ;
#53993 = EDGE_CURVE ( 'NONE', #27227, #22912, #9146, .T. ) ;
#53994 =( BOUNDED_CURVE ( )  B_SPLINE_CURVE ( 2, ( #23857, #17579, #60779, #18240, #22836, #23184, #29104, #50597, #45363, #28777, #44674 ),
 .UNSPECIFIED., .F., .F. ) 
 B_SPLINE_CURVE_WITH_KNOTS ( ( 3, 2, 2, 2, 2, 3 ),
 ( 0.05882352941176476058, 0.06470588235294123802, 0.07058823529411770159, 0.07647058823529419291, 0.08235294117647065648, 0.08823529411764713393 ),
 .UNSPECIFIED. ) 
 CURVE ( )  GEOMETRIC_REPRESENTATION_ITEM ( )  RATIONAL_B_SPLINE_CURVE ( ( 0.9999999999999995559, 0.9510565162951539753, 1.000000000000000000, 0.9510565162951535312, 1.000000000000000000, 0.9510565162951535312, 1.000000000000000000, 0.9510565162951535312, 1.000000000000000000, 0.9510565162951529761, 1.000000000000000666 ) ) 
 REPRESENTATION_ITEM ( '' )  );
#53995 = SURFACE_STYLE_FILL_AREA ( #11787 ) ;
#53996 = DIRECTION ( 'NONE',  ( 1.000000000000000000, 0.000000000000000000, 0.000000000000000000 ) ) ;
#53997 = MECHANICAL_DESIGN_GEOMETRIC_PRESENTATION_REPRESENTATION (  '', ( #9075 ), #48430 ) ;
#53999 = COLOUR_RGB ( '', 0.72549020, 0.75294118, 0.79215686) ;
#53998 = DIRECTION ( 'NONE',  ( 0.000000000000000000, 0.000000000000000000, -1.000000000000000000 ) ) ;
#54000 = CARTESIAN_POINT ( 'NONE',  ( -51.95499999999996987, -7.632228543268599452, 2.479861379858951054 ) ) ;
#54001 = CARTESIAN_POINT ( 'NONE',  ( 0.000000000000000000, 0.9999999999999991118, -79.00402776293826435 ) ) ;
#54002 = CARTESIAN_POINT ( 'NONE',  ( -62.54499999999998749, -7.632228543268600340, -2.479861379858950166 ) ) ;
#54003 = LINE ( 'NONE', #65254, #21965 ) ;
#54004 = CARTESIAN_POINT ( 'NONE',  ( -102.6570736234661751, 9.058813317711329915, 2.943386871421369566 ) ) ;
#54005 = CARTESIAN_POINT ( 'NONE',  ( -7.731910350068054619E-16, -6.500000000000000888, 21.00000000000000000 ) ) ;
#54006 = VECTOR ( 'NONE', #11722, 1000.000000000000000 ) ;
#54007 = EDGE_CURVE ( 'NONE', #44668, #53049, #64593, .T. ) ;
#54008 = CARTESIAN_POINT ( 'NONE',  ( -106.0429263765337993, -9.058813317711329915, -2.943386871421370898 ) ) ;
#54009 = DIRECTION ( 'NONE',  ( 5.551115123125782702E-17, -0.9591247405308764851, -0.2829836251474255326 ) ) ;
#54010 = CARTESIAN_POINT ( 'NONE',  ( -41.49999999999997868, 9.999999999999978684, 3.500000000000000000 ) ) ;
#54011 = AXIS2_PLACEMENT_3D ( 'NONE', #54773, #49888, #45330 ) ;
#54012 = EDGE_CURVE ( 'NONE', #1406, #3527, #45131, .T. ) ;
#54013 = CARTESIAN_POINT ( 'NONE',  ( 26.00000000000001066, 21.74999999999998224, -3.750000000000000000 ) ) ;
#54014 = FILL_AREA_STYLE_COLOUR ( '', #23637 ) ;
#54015 = MECHANICAL_DESIGN_GEOMETRIC_PRESENTATION_REPRESENTATION (  '', ( #57397 ), #20327 ) ;
#54016 = ORIENTED_EDGE ( 'NONE', *, *, #43429, .F. ) ;
#54017 = PRESENTATION_LAYER_ASSIGNMENT (  '', '', ( #23640 ) ) ;
#54018 =( NAMED_UNIT ( * ) PLANE_ANGLE_UNIT ( ) SI_UNIT ( $, .RADIAN. ) );
#54019 = DIRECTION ( 'NONE',  ( -0.000000000000000000, -0.000000000000000000, 1.000000000000000000 ) ) ;
#54020 = ORIENTED_EDGE ( 'NONE', *, *, #50131, .T. ) ;
#54021 = PLANE ( 'NONE',  #40925 ) ;
#54022 = CIRCLE ( 'NONE', #9114, 0.2500000000000002220 ) ;
#54023 = CARTESIAN_POINT ( 'NONE',  ( 2.607480562269076430, 111.9070736234661751, -8.025000000000000355 ) ) ;
#54024 = CARTESIAN_POINT ( 'NONE',  ( 3.409623619629276625, -7.000000000000002665, 0.7804846576204699238 ) ) ;
#54025 = FACE_OUTER_BOUND ( 'NONE', #52655, .T. ) ;
#54026 =( NAMED_UNIT ( * ) SI_UNIT ( $, .STERADIAN. ) SOLID_ANGLE_UNIT ( ) );
#54027 = ORIENTED_EDGE ( 'NONE', *, *, #42064, .T. ) ;
#54028 = ORIENTED_EDGE ( 'NONE', *, *, #69580, .F. ) ;
#54029 =( NAMED_UNIT ( * ) SI_UNIT ( $, .STERADIAN. ) SOLID_ANGLE_UNIT ( ) );
#54030 = VERTEX_POINT ( 'NONE', #69506 ) ;
#54031 = CARTESIAN_POINT ( 'NONE',  ( -10.01517768586949231, 129.3050000000000068, -6.132527647946036459E-16 ) ) ;
#54032 = DIRECTION ( 'NONE',  ( -0.000000000000000000, 0.000000000000000000, 1.000000000000000000 ) ) ;
#54033 = LINE ( 'NONE', #5838, #46392 ) ;
#54034 = AXIS2_PLACEMENT_3D ( 'NONE', #44803, #67607, #2487 ) ;
#54035 = CARTESIAN_POINT ( 'NONE',  ( 45.50000000000000000, -1.469576158976824618E-14, 10.00000000000000000 ) ) ;
#54036 = CARTESIAN_POINT ( 'NONE',  ( -89.24499999999999034, -4.716976649647093289, -6.492361379858945902 ) ) ;
#54037 = ORIENTED_EDGE ( 'NONE', *, *, #15768, .F. ) ;
#54038 = ADVANCED_FACE ( 'NONE', ( #21308 ), #11457, .T. ) ;
#54039 = FILL_AREA_STYLE ('',( #43211 ) ) ;
#54040 = AXIS2_PLACEMENT_3D ( 'NONE', #55776, #1561, #34324 ) ;
#54041 = CARTESIAN_POINT ( 'NONE',  ( -71.50000000000000000, 35.92875272052971525, -7.500000000000000000 ) ) ;
#54042 = EDGE_LOOP ( 'NONE', ( #25002, #64105, #54921, #20342 ) ) ;
#54043 = CARTESIAN_POINT ( 'NONE',  ( -175.0429263765338135, -9.058813317711329915, -2.943386871421370898 ) ) ;
#54044 = PLANE ( 'NONE',  #37082 ) ;
#54045 = CARTESIAN_POINT ( 'NONE',  ( 7.766025168014160762, -0.5488498361408512549, 0.7660251680141582087 ) ) ;
#54046 = FILL_AREA_STYLE ('',( #42866 ) ) ;
#54047 = VERTEX_POINT ( 'NONE', #10085 ) ;
#54048 = CIRCLE ( 'NONE', #5737, 0.9999999999999995559 ) ;
#54049 = FACE_OUTER_BOUND ( 'NONE', #29491, .T. ) ;
#54050 = ORIENTED_EDGE ( 'NONE', *, *, #47547, .F. ) ;
#54051 = DIRECTION ( 'NONE',  ( 0.000000000000000000, 0.000000000000000000, -1.000000000000000000 ) ) ;
#54052 = LINE ( 'NONE', #43222, #43679 ) ;
#54053 = CARTESIAN_POINT ( 'NONE',  ( -195.0000000000000000, 0.000000000000000000, 0.000000000000000000 ) ) ;
#54054 = FILL_AREA_STYLE_COLOUR ( '', #45683 ) ;
#54055 = FACE_OUTER_BOUND ( 'NONE', #43127, .T. ) ;
#54056 = COLOUR_RGB ( '', 0.31764706, 0.68627451, 0.89019608) ;
#54057 = VECTOR ( 'NONE', #34308, 1000.000000000000000 ) ;
#54058 = CARTESIAN_POINT ( 'NONE',  ( -69.14292637653379359, 5.598654528085800663, -7.705886871421367523 ) ) ;
#54059 = CARTESIAN_POINT ( 'NONE',  ( -72.49999999999998579, 63.67479433117734544, -10.00000000000000000 ) ) ;
#54060 = CARTESIAN_POINT ( 'NONE',  ( -7.514523004098856873, 153.7576610836294151, 4.578433682763812129 ) ) ;
#54061 = VERTEX_POINT ( 'NONE', #53671 ) ;
#54062 = VECTOR ( 'NONE', #30367, 1000.000000000000000 ) ;
#54063 = CARTESIAN_POINT ( 'NONE',  ( 74.99999999999998579, 50.00000000000000000, -7.500000000000000000 ) ) ;
#54064 = EDGE_CURVE ( 'NONE', #49536, #55848, #6868, .T. ) ;
#54065 =( LENGTH_UNIT ( ) NAMED_UNIT ( * ) SI_UNIT ( .MILLI., .METRE. ) );
#54066 = ORIENTED_EDGE ( 'NONE', *, *, #41307, .F. ) ;
#54067 = CARTESIAN_POINT ( 'NONE',  ( -173.9049999999999727, 2.607480562269068880, -8.024999999999993250 ) ) ;
#54068 = ADVANCED_FACE ( 'NONE', ( #37198 ), #48795, .T. ) ;
#54069 = CARTESIAN_POINT ( 'NONE',  ( -15.00000000000000000, 8.000000000000000000, 4.000000000000000000 ) ) ;
#54070 = CARTESIAN_POINT ( 'NONE',  ( -147.3570736234661638, 5.598654528085804216, 7.705886871421366635 ) ) ;
#54071 = CIRCLE ( 'NONE', #61905, 7.000000000000001776 ) ;
#54072 = CARTESIAN_POINT ( 'NONE',  ( -172.9449999999999932, -9.827790563157499189E-16, -8.024999999999991473 ) ) ;
#54073 = CARTESIAN_POINT ( 'NONE',  ( -168.1449999999999818, -4.716976649647092401, 6.492361379858946790 ) ) ;
#54074 =( GEOMETRIC_REPRESENTATION_CONTEXT ( 3 ) GLOBAL_UNCERTAINTY_ASSIGNED_CONTEXT ( ( #41874 ) ) GLOBAL_UNIT_ASSIGNED_CONTEXT ( ( #22624, #43093, #59901 ) ) REPRESENTATION_CONTEXT ( 'NONE', 'WORKASPACE' ) );
#54075 = ORIENTED_EDGE ( 'NONE', *, *, #28737, .F. ) ;
#54076 = CARTESIAN_POINT ( 'NONE',  ( 10.00000000000000178, 43.00000000000000000, -90.00000000000000000 ) ) ;
#54077 = ADVANCED_FACE ( 'NONE', ( #58963 ), #22025, .T. ) ;
#54078 = DIRECTION ( 'NONE',  ( 1.000000000000000000, 0.000000000000000000, 0.000000000000000000 ) ) ;
#54079 =( LENGTH_UNIT ( ) NAMED_UNIT ( * ) SI_UNIT ( .MILLI., .METRE. ) );
#54080 = CARTESIAN_POINT ( 'NONE',  ( -82.40500000000000114, -2.607480562269069768, 8.024999999999991473 ) ) ;
#54081 = CYLINDRICAL_SURFACE ( 'NONE', #24147, 9.524999999999991473 ) ;
#54082 = DIRECTION ( 'NONE',  ( 0.000000000000000000, 0.000000000000000000, -1.000000000000000000 ) ) ;
#54083 = PRESENTATION_STYLE_ASSIGNMENT (( #65681 ) ) ;
#54084 = CARTESIAN_POINT ( 'NONE',  ( -79.49499999999997613, 6.826472737025113702, -4.959722759717902107 ) ) ;
#54085 = CARTESIAN_POINT ( 'NONE',  ( -9.058813317711337021, 135.1550000000000011, -2.943386871421374895 ) ) ;
#54086 = CARTESIAN_POINT ( 'NONE',  ( -4.716976649647097730, 126.2429263765338163, -6.492361379858953896 ) ) ;
#54087 = ADVANCED_FACE ( 'NONE', ( #48447 ), #138, .T. ) ;
#54088 = DIRECTION ( 'NONE',  ( -1.000000000000000000, 0.000000000000000000, 0.000000000000000000 ) ) ;
#54089 = CARTESIAN_POINT ( 'NONE',  ( 0.000000000000000000, 110.4999999999999858, 0.000000000000000000 ) ) ;
#54090 = DIRECTION ( 'NONE',  ( 0.000000000000000000, 0.000000000000000000, 1.000000000000000000 ) ) ;
#54091 = VERTEX_POINT ( 'NONE', #6181 ) ;
#54092 = CIRCLE ( 'NONE', #3542, 1.000000000000000888 ) ;
#54093 = ADVANCED_FACE ( 'NONE', ( #47412 ), #68836, .T. ) ;
#54094 = PRODUCT ( '3. Padlock', '3. Padlock', '', ( #28990 ) ) ;
#54095 =( NAMED_UNIT ( * ) SI_UNIT ( $, .STERADIAN. ) SOLID_ANGLE_UNIT ( ) );
#54096 = MECHANICAL_DESIGN_GEOMETRIC_PRESENTATION_REPRESENTATION (  '', ( #29342 ), #47381 ) ;
#54097 =( LENGTH_UNIT ( ) NAMED_UNIT ( * ) SI_UNIT ( .MILLI., .METRE. ) );
#54098 = AXIS2_PLACEMENT_3D ( 'NONE', #4886, #53438, #20015 ) ;
#54099 = DIRECTION ( 'NONE',  ( -1.000000000000000000, 0.000000000000000000, 0.000000000000000000 ) ) ;
#54100 = ORIENTED_EDGE ( 'NONE', *, *, #359, .T. ) ;
#54101 = ORIENTED_EDGE ( 'NONE', *, *, #23551, .F. ) ;
#54102 = AXIS2_PLACEMENT_3D ( 'NONE', #56191, #56546, #45355 ) ;
#54103 = SURFACE_SIDE_STYLE ('',( #16521 ) ) ;
#54104 =( NAMED_UNIT ( * ) SI_UNIT ( $, .STERADIAN. ) SOLID_ANGLE_UNIT ( ) );
#54105 = STYLED_ITEM ( 'NONE', ( #17375 ), #53463 ) ;
#54106 = DIRECTION ( 'NONE',  ( -1.000000000000000000, 0.000000000000000000, 0.000000000000000000 ) ) ;
#54107 = ORIENTED_EDGE ( 'NONE', *, *, #10262, .F. ) ;
#54108 = CARTESIAN_POINT ( 'NONE',  ( -110.4549999999999841, 7.632228543268599452, -2.479861379858951942 ) ) ;
#54109 = ORIENTED_EDGE ( 'NONE', *, *, #29056, .T. ) ;
#54110 = SURFACE_SIDE_STYLE ('',( #39021 ) ) ;
#54111 = CARTESIAN_POINT ( 'NONE',  ( 20.03990113061529144, 115.4999999999999574, -9.999999999999998224 ) ) ;
#54112 = AXIS2_PLACEMENT_3D ( 'NONE', #16125, #58651, #69548 ) ;
#54113 = EDGE_LOOP ( 'NONE', ( #37577, #50657, #32579, #26258 ) ) ;
#54114 = CARTESIAN_POINT ( 'NONE',  ( 39.74999999999999289, 18.99999999999997868, -3.750000000000000000 ) ) ;
#54115 = CARTESIAN_POINT ( 'NONE',  ( -7.766025168014157209, -1.733974831985841458, 0.5488498361408482573 ) ) ;
#54116 = ORIENTED_EDGE ( 'NONE', *, *, #15823, .F. ) ;
#54117 = AXIS2_PLACEMENT_3D ( 'NONE', #20864, #52544, #52882 ) ;
#54118 = CARTESIAN_POINT ( 'NONE',  ( -3.094860106618434248, 158.7949999999999875, 9.525000000000000355 ) ) ;
#54119 = EDGE_LOOP ( 'NONE', ( #44337, #17153, #8993, #67439 ) ) ;
#54120 = ADVANCED_FACE ( 'NONE', ( #10437 ), #12480, .F. ) ;
#54121 = VERTEX_POINT ( 'NONE', #31867 ) ;
#54122 = CARTESIAN_POINT ( 'NONE',  ( -195.0000000000000000, 0.000000000000000000, 0.000000000000000000 ) ) ;
#54123 = CARTESIAN_POINT ( 'NONE',  ( -13.68996927307399858, -10.98240371287465322, 4.836514277720893595 ) ) ;
#54124 = CARTESIAN_POINT ( 'NONE',  ( -129.7429263765338021, -5.598654528085803328, -7.705886871421366635 ) ) ;
#54125 = ORIENTED_EDGE ( 'NONE', *, *, #57091, .T. ) ;
#54126 = CARTESIAN_POINT ( 'NONE',  ( -9.827790563157511022E-16, 136.4429263765338192, 8.025000000000000355 ) ) ;
#54127 = CARTESIAN_POINT ( 'NONE',  ( 1.000000000000000000, 43.00000000000000000, -35.50000000000000000 ) ) ;
#54128 = CARTESIAN_POINT ( 'NONE',  ( -47.60707362346616378, -8.102448949553174629, 5.886773742842742685 ) ) ;
#54129 = VECTOR ( 'NONE', #2022, 1000.000000000000000 ) ;
#54130 = CARTESIAN_POINT ( 'NONE',  ( 0.000000000000000000, -9.000000000000007105, 0.000000000000000000 ) ) ;
#54131 = ORIENTED_EDGE ( 'NONE', *, *, #55677, .F. ) ;
#54132 = EDGE_LOOP ( 'NONE', ( #49137, #43532, #35884, #17242, #53036, #64795, #32303, #54398, #61673, #46698, #46551, #59744, #14970 ) ) ;
#54133 = CARTESIAN_POINT ( 'NONE',  ( -49.64292637653380780, -5.598654528085801552, 7.705886871421367523 ) ) ;
#54134 = DIRECTION ( 'NONE',  ( 0.000000000000000000, 0.000000000000000000, 1.000000000000000000 ) ) ;
#54135 = CARTESIAN_POINT ( 'NONE',  ( 74.50000000000000000, 3.473944261090200865E-15, 6.500000000000000000 ) ) ;
#54136 = FACE_OUTER_BOUND ( 'NONE', #50208, .T. ) ;
#54137 = CARTESIAN_POINT ( 'NONE',  ( -143.3050000000000068, 8.437984349512085203, -1.550032578732815448E-15 ) ) ;
#54138 = FACE_OUTER_BOUND ( 'NONE', #9498, .T. ) ;
#54139 = CARTESIAN_POINT ( 'NONE',  ( 6.750018943533632410, 42.91041480136897945, -27.90050555725692405 ) ) ;
#54140 = STYLED_ITEM ( 'NONE', ( #16292 ), #46002 ) ;
#54141 = ADVANCED_FACE ( 'NONE', ( #6505 ), #1544, .T. ) ;
#54142 = AXIS2_PLACEMENT_3D ( 'NONE', #45058, #22181, #66470 ) ;
#54143 = CARTESIAN_POINT ( 'NONE',  ( -43.24371837588274303, -14.00594677377896069, 0.7702318141522507267 ) ) ;
#54144 = DIRECTION ( 'NONE',  ( 1.000000000000000000, -0.000000000000000000, -0.000000000000000000 ) ) ;
#54145 = FILL_AREA_STYLE_COLOUR ( '', #1053 ) ;
#54146 = EDGE_LOOP ( 'NONE', ( #61559, #27404, #45980, #22538 ) ) ;
#54147 = MECHANICAL_DESIGN_GEOMETRIC_PRESENTATION_REPRESENTATION (  '', ( #21615 ), #35071 ) ;
#54148 = ORIENTED_EDGE ( 'NONE', *, *, #36974, .T. ) ;
#54149 = CARTESIAN_POINT ( 'NONE',  ( -45.07457192895288500, 8.173863537799691770, 3.593626512517976934 ) ) ;
#54150 = CARTESIAN_POINT ( 'NONE',  ( 11.00000000000001776, 42.00000000000000000, -28.38386403503541899 ) ) ;
#54151 = EDGE_CURVE ( 'NONE', #17986, #25904, #65960, .T. ) ;
#54152 = CARTESIAN_POINT ( 'NONE',  ( -53.30499999999998550, 8.437984349512085203, -1.550032578732815448E-15 ) ) ;
#54153 = ORIENTED_EDGE ( 'NONE', *, *, #33980, .T. ) ;
#54154 = PRESENTATION_STYLE_ASSIGNMENT (( #32698 ) ) ;
#54155 = EDGE_CURVE ( 'NONE', #13586, #11926, #28218, .T. ) ;
#54156 = FILL_AREA_STYLE_COLOUR ( '', #62105 ) ;
#54157 = AXIS2_PLACEMENT_3D ( 'NONE', #61708, #19158, #29007 ) ;
#54158 = CARTESIAN_POINT ( 'NONE',  ( 0.000000000000000000, 36.74999999999999289, 3.000000000000000000 ) ) ;
#54159 = AXIS2_PLACEMENT_3D ( 'NONE', #7340, #66773, #28769 ) ;
#54160 = DIRECTION ( 'NONE',  ( -0.000000000000000000, -1.000000000000000000, -0.000000000000000000 ) ) ;
#54161 = DIRECTION ( 'NONE',  ( -0.000000000000000000, 1.000000000000000000, -0.000000000000000000 ) ) ;
#54162 = ORIENTED_EDGE ( 'NONE', *, *, #14728, .T. ) ;
#54163 =( GEOMETRIC_REPRESENTATION_CONTEXT ( 3 ) GLOBAL_UNCERTAINTY_ASSIGNED_CONTEXT ( ( #29157 ) ) GLOBAL_UNIT_ASSIGNED_CONTEXT ( ( #64529, #54301, #38172 ) ) REPRESENTATION_CONTEXT ( 'NONE', 'WORKASPACE' ) );
#54164 = ADVANCED_FACE ( 'NONE', ( #1182 ), #34990, .F. ) ;
#54165 = CARTESIAN_POINT ( 'NONE',  ( -23.71231517720798010, 112.9999999999999858, 7.500000000000000000 ) ) ;
#54166 =( NAMED_UNIT ( * ) SI_UNIT ( $, .STERADIAN. ) SOLID_ANGLE_UNIT ( ) );
#54167 =( LENGTH_UNIT ( ) NAMED_UNIT ( * ) SI_UNIT ( .MILLI., .METRE. ) );
#54168 = CARTESIAN_POINT ( 'NONE',  ( 179.4361977533490347, 14.00000000000000000, -103.7004518695263044 ) ) ;
#54169 = CARTESIAN_POINT ( 'NONE',  ( 4.750000000000002665, 24.74999999999998579, -3.750000000000000000 ) ) ;
#54170 = EDGE_CURVE ( 'NONE', #22828, #65411, #39495, .T. ) ;
#54171 = VECTOR ( 'NONE', #23357, 1000.000000000000000 ) ;
#54172 = CARTESIAN_POINT ( 'NONE',  ( -110.5449999999999875, -7.632228543268600340, -2.479861379858950166 ) ) ;
#54173 = CARTESIAN_POINT ( 'NONE',  ( 8.102448949553181734, 112.5049999999999670, 5.886773742842750679 ) ) ;
#54174 = CARTESIAN_POINT ( 'NONE',  ( -89.84499999999999886, -7.632228543268599452, 2.479861379858951054 ) ) ;
#54175 = STYLED_ITEM ( 'NONE', ( #45382 ), #18831 ) ;
#54176 = SURFACE_STYLE_USAGE ( .BOTH. , #32363 ) ;
#54177 = FACE_OUTER_BOUND ( 'NONE', #13774, .T. ) ;
#54178 = VECTOR ( 'NONE', #64873, 1000.000000000000000 ) ;
#54179 = DIRECTION ( 'NONE',  ( -0.000000000000000000, 1.000000000000000000, 0.000000000000000000 ) ) ;
#54180 = ORIENTED_EDGE ( 'NONE', *, *, #52300, .T. ) ;
#54181 = CARTESIAN_POINT ( 'NONE',  ( -120.7429263765338021, -5.598654528085803328, -7.705886871421366635 ) ) ;
#54182 = CARTESIAN_POINT ( 'NONE',  ( -149.3949999999999818, -6.826472737025115478, -4.959722759717899443 ) ) ;
#54183 = CARTESIAN_POINT ( 'NONE',  ( -2.755190520427474699, 7.000000000000004441, 0.4949495880430779260 ) ) ;
#54184 = AXIS2_PLACEMENT_3D ( 'NONE', #43480, #37849, #60284 ) ;
#54185 = DIRECTION ( 'NONE',  ( -0.000000000000000000, 1.000000000000000000, -0.000000000000000000 ) ) ;
#54186 = ORIENTED_EDGE ( 'NONE', *, *, #34620, .F. ) ;
#54187 = ORIENTED_EDGE ( 'NONE', *, *, #345, .F. ) ;
#54188 = VECTOR ( 'NONE', #8363, 1000.000000000000000 ) ;
#54189 = EDGE_CURVE ( 'NONE', #22486, #56480, #48486, .T. ) ;
#54190 = CARTESIAN_POINT ( 'NONE',  ( 60.00000000000000000, 1.797044900979284448E-15, -6.500000000000000000 ) ) ;
#54191 = CARTESIAN_POINT ( 'NONE',  ( 3.749999999999999556, 34.24999999999998579, 4.000000000000000000 ) ) ;
#54192 = AXIS2_PLACEMENT_3D ( 'NONE', #58059, #25333, #30949 ) ;
#54193 =( NAMED_UNIT ( * ) SI_UNIT ( $, .STERADIAN. ) SOLID_ANGLE_UNIT ( ) );
#54194 = DIRECTION ( 'NONE',  ( 0.000000000000000000, 0.000000000000000000, -1.000000000000000000 ) ) ;
#54195 = FILL_AREA_STYLE ('',( #48975 ) ) ;
#54196 = VECTOR ( 'NONE', #8641, 1000.000000000000000 ) ;
#54197 = CARTESIAN_POINT ( 'NONE',  ( -115.9429263765338050, 0.000000000000000000, 9.524999999999991473 ) ) ;
#54198 = FILL_AREA_STYLE_COLOUR ( '', #69044 ) ;
#54199 = ORIENTED_EDGE ( 'NONE', *, *, #13589, .F. ) ;
#54200 = CARTESIAN_POINT ( 'NONE',  ( -137.1550000000000011, 7.632228543268600340, 2.479861379858949277 ) ) ;
#54201 = EDGE_LOOP ( 'NONE', ( #2446, #63781, #46598, #963 ) ) ;
#54202 = AXIS2_PLACEMENT_3D ( 'NONE', #57596, #25230, #37220 ) ;
#54203 = ORIENTED_EDGE ( 'NONE', *, *, #52296, .F. ) ;
#54204 = FACE_BOUND ( 'NONE', #2316, .T. ) ;
#54205 = ORIENTED_EDGE ( 'NONE', *, *, #63046, .T. ) ;
#54206 = CARTESIAN_POINT ( 'NONE',  ( -4.041451884327381450, -7.000000000000002665, 7.500000000000000000 ) ) ;
#54207 = TOROIDAL_SURFACE ( 'NONE', #30602, 1.000000000000000000, 0.5000000000000000000 ) ;
#54208 = DIRECTION ( 'NONE',  ( 0.000000000000000000, 0.000000000000000000, -1.000000000000000000 ) ) ;
#54209 = CARTESIAN_POINT ( 'NONE',  ( -8.102448949553181734, 128.4950000000000045, 5.886773742842747126 ) ) ;
#54210 = CARTESIAN_POINT ( 'NONE',  ( 0.9999999999999991118, 43.00000000000000000, -74.38749456993816978 ) ) ;
#54211 = CIRCLE ( 'NONE', #30607, 0.2500000000000002220 ) ;
#54212 = ORIENTED_EDGE ( 'NONE', *, *, #2834, .T. ) ;
#54213 = CARTESIAN_POINT ( 'NONE',  ( -95.15707362346617515, -9.058813317711329915, -2.943386871421370898 ) ) ;
#54214 = CARTESIAN_POINT ( 'NONE',  ( 3.094860106618431583, 133.2049999999999841, 9.525000000000000355 ) ) ;
#54215 = CARTESIAN_POINT ( 'NONE',  ( -57.20499999999996987, -2.607480562269071545, -8.024999999999991473 ) ) ;
#54216 = CARTESIAN_POINT ( 'NONE',  ( -124.0449999999999875, 7.632228543268600340, 2.479861379858949277 ) ) ;
#54217 = CARTESIAN_POINT ( 'NONE',  ( -118.5570736234661808, -1.166476076187852838E-15, -9.524999999999991473 ) ) ;
#54218 = ORIENTED_EDGE ( 'NONE', *, *, #28814, .T. ) ;
#54219 = CARTESIAN_POINT ( 'NONE',  ( -1.166476076187854022E-15, 145.0549999999999784, 9.525000000000000355 ) ) ;
#54220 = AXIS2_PLACEMENT_3D ( 'NONE', #69205, #64253, #52684 ) ;
#54221 = PRESENTATION_STYLE_ASSIGNMENT (( #12334 ) ) ;
#54222 = VECTOR ( 'NONE', #46784, 1000.000000000000000 ) ;
#54223 = EDGE_CURVE ( 'NONE', #5343, #17478, #12138, .T. ) ;
#54224 = DIRECTION ( 'NONE',  ( 0.000000000000000000, 0.000000000000000000, 1.000000000000000000 ) ) ;
#54225 = EDGE_LOOP ( 'NONE', ( #56299, #24381, #7130, #5923 ) ) ;
#54226 = DIRECTION ( 'NONE',  ( 1.224646799147353207E-16, 1.000000000000000000, -0.000000000000000000 ) ) ;
#54227 = CARTESIAN_POINT ( 'NONE',  ( -172.1050000000000182, -6.826472737025115478, 4.959722759717900331 ) ) ;
#54228 = ORIENTED_EDGE ( 'NONE', *, *, #18695, .T. ) ;
#54229 = LINE ( 'NONE', #21536, #38529 ) ;
#54230 = CIRCLE ( 'NONE', #64386, 1.000000000000000000 ) ;
#54231 = ADVANCED_FACE ( 'NONE', ( #60668 ), #3454, .T. ) ;
#54232 = FILL_AREA_STYLE_COLOUR ( '', #65598 ) ;
#54233 = CARTESIAN_POINT ( 'NONE',  ( 9.985360875542987458, -1.514639124457112018, 0.7048476316490990268 ) ) ;
#54234 = DIRECTION ( 'NONE',  ( -0.000000000000000000, -1.000000000000000000, 0.000000000000000000 ) ) ;
#54235 = VERTEX_POINT ( 'NONE', #6872 ) ;
#54236 =( GEOMETRIC_REPRESENTATION_CONTEXT ( 3 ) GLOBAL_UNCERTAINTY_ASSIGNED_CONTEXT ( ( #432 ) ) GLOBAL_UNIT_ASSIGNED_CONTEXT ( ( #8140, #29581, #24299 ) ) REPRESENTATION_CONTEXT ( 'NONE', 'WORKASPACE' ) );
#54238 = EDGE_CURVE ( 'NONE', #37266, #29977, #45923, .T. ) ;
#54237 = FILL_AREA_STYLE ('',( #20865 ) ) ;
#54239 = CARTESIAN_POINT ( 'NONE',  ( -84.80499999999999261, -8.437984349512085203, 5.166775262442717831E-16 ) ) ;
#54240 = ORIENTED_EDGE ( 'NONE', *, *, #48996, .T. ) ;
#54241 = VECTOR ( 'NONE', #7363, 1000.000000000000000 ) ;
#54242 = CARTESIAN_POINT ( 'NONE',  ( 6.826472737025119919, 144.0070736234661126, 4.959722759717908325 ) ) ;
#54243 = FILL_AREA_STYLE ('',( #32802 ) ) ;
#54244 = CARTESIAN_POINT ( 'NONE',  ( -63.80707362346617373, 10.01517768586948698, -1.839758294383808571E-15 ) ) ;
#54245 = STYLED_ITEM ( 'NONE', ( #24198 ), #46516 ) ;
#54246 = CARTESIAN_POINT ( 'NONE',  ( 3.000000000000002665, 42.00000000000000000, 3.772833609257260986E-15 ) ) ;
#54247 = ORIENTED_EDGE ( 'NONE', *, *, #40690, .T. ) ;
#54248 = DIRECTION ( 'NONE',  ( 1.000000000000000000, -0.000000000000000000, -0.000000000000000000 ) ) ;
#54249 =( NAMED_UNIT ( * ) PLANE_ANGLE_UNIT ( ) SI_UNIT ( $, .RADIAN. ) );
#54250 = ADVANCED_FACE ( 'NONE', ( #19500 ), #61697, .T. ) ;
#54251 = CARTESIAN_POINT ( 'NONE',  ( -103.8549999999999898, 4.716976649647094177, 6.492361379858945902 ) ) ;
#54252 = CARTESIAN_POINT ( 'NONE',  ( -5.598654528085808657, 125.6449999999999818, 7.705886871421373741 ) ) ;
#54253 = CIRCLE ( 'NONE', #8235, 1.000000000000000888 ) ;
#54254 = CARTESIAN_POINT ( 'NONE',  ( -117.2949999999999875, -2.607480562269069768, 8.024999999999991473 ) ) ;
#54255 = VECTOR ( 'NONE', #61562, 1000.000000000000000 ) ;
#54256 = DIRECTION ( 'NONE',  ( 0.000000000000000000, 0.000000000000000000, -1.000000000000000000 ) ) ;
#54257 = VECTOR ( 'NONE', #24201, 1000.000000000000000 ) ;
#54259 = CARTESIAN_POINT ( 'NONE',  ( 28.58578643762692550, 42.99999999999999289, 90.00000000000000000 ) ) ;
#54258 = CARTESIAN_POINT ( 'NONE',  ( 45.44163888576682098, 10.14721296192227129, 3.260160134650226027 ) ) ;
#54260 = CARTESIAN_POINT ( 'NONE',  ( -154.3429263765337964, -9.058813317711329915, 2.943386871421371787 ) ) ;
#54261 = VECTOR ( 'NONE', #42248, 1000.000000000000000 ) ;
#54262 = CARTESIAN_POINT ( 'NONE',  ( -179.6949999999999932, -8.437984349512085203, 5.166775262442717831E-16 ) ) ;
#54263 = CIRCLE ( 'NONE', #64419, 0.4999999999999994449 ) ;
#54264 = CARTESIAN_POINT ( 'NONE',  ( -23.71231517720798010, 112.9999999999999858, -7.000000000000000000 ) ) ;
#54265 = CARTESIAN_POINT ( 'NONE',  ( -42.80176904642062397, -12.14886544991757233, 3.185780282727390222 ) ) ;
#54266 = ORIENTED_EDGE ( 'NONE', *, *, #11100, .F. ) ;
#54267 = SURFACE_STYLE_USAGE ( .BOTH. , #65526 ) ;
#54268 =( NAMED_UNIT ( * ) PLANE_ANGLE_UNIT ( ) SI_UNIT ( $, .RADIAN. ) );
#54269 = ORIENTED_EDGE ( 'NONE', *, *, #32812, .T. ) ;
#54270 = CARTESIAN_POINT ( 'NONE',  ( -74.99292637653380211, 8.102448949553171076, -5.886773742842744461 ) ) ;
#54271 = EDGE_CURVE ( 'NONE', #35810, #12948, #2324, .T. ) ;
#54272 = CONTEXT_DEPENDENT_SHAPE_REPRESENTATION ( #979, #65463 ) ;
#54273 = CARTESIAN_POINT ( 'NONE',  ( -45.50000000000000000, 7.768687147774684831, 6.500000000000000000 ) ) ;
#54274 = CARTESIAN_POINT ( 'NONE',  ( 22.00000000000000711, 50.00000000000000000, -65.00000000000000000 ) ) ;
#54275 = AXIS2_PLACEMENT_3D ( 'NONE', #52471, #20065, #25357 ) ;
#54277 = FILL_AREA_STYLE_COLOUR ( '', #33770 ) ;
#54276 =( BOUNDED_CURVE ( )  B_SPLINE_CURVE ( 3, ( #59027, #22085, #21737, #43249 ),
 .UNSPECIFIED., .F., .F. ) 
 B_SPLINE_CURVE_WITH_KNOTS ( ( 4, 4 ),
 ( 4.712388980384689674, 6.283185307179586232 ),
 .UNSPECIFIED. ) 
 CURVE ( )  GEOMETRIC_REPRESENTATION_ITEM ( )  RATIONAL_B_SPLINE_CURVE ( ( 1.000000000000000000, 0.8047378541243649375, 0.8047378541243649375, 1.000000000000000000 ) ) 
 REPRESENTATION_ITEM ( '' )  );
#54278 = LINE ( 'NONE', #11021, #57221 ) ;
#54279 = CARTESIAN_POINT ( 'NONE',  ( -79.64292637653380780, -5.598654528085801552, 7.705886871421367523 ) ) ;
#54280 = ORIENTED_EDGE ( 'NONE', *, *, #58702, .T. ) ;
#54281 = CARTESIAN_POINT ( 'NONE',  ( -169.4049999999999443, -2.607480562269069768, 8.024999999999991473 ) ) ;
#54282 = VERTEX_POINT ( 'NONE', #29355 ) ;
#54283 = CARTESIAN_POINT ( 'NONE',  ( -112.0429263765337993, -9.058813317711329915, -2.943386871421370898 ) ) ;
#54284 =( LENGTH_UNIT ( ) NAMED_UNIT ( * ) SI_UNIT ( .MILLI., .METRE. ) );
#54285 = LINE ( 'NONE', #20910, #25078 ) ;
#54286 =( NAMED_UNIT ( * ) PLANE_ANGLE_UNIT ( ) SI_UNIT ( $, .RADIAN. ) );
#54287 = STYLED_ITEM ( 'NONE', ( #35039 ), #47845 ) ;
#54288 = AXIS2_PLACEMENT_3D ( 'NONE', #61701, #46652, #19149 ) ;
#54289 = CARTESIAN_POINT ( 'NONE',  ( -182.0070736234661979, -8.102448949553174629, -5.886773742842741797 ) ) ;
#54290 = CARTESIAN_POINT ( 'NONE',  ( 2.607480562269076430, 156.9070736234661467, -8.025000000000000355 ) ) ;
#54291 = ORIENTED_EDGE ( 'NONE', *, *, #9138, .T. ) ;
#54292 = DIRECTION ( 'NONE',  ( -1.000000000000000000, -0.000000000000000000, -0.000000000000000000 ) ) ;
#54293 = CARTESIAN_POINT ( 'NONE',  ( -92.00499999999998124, 6.826472737025115478, 4.959722759717899443 ) ) ;
#54294 = FACE_OUTER_BOUND ( 'NONE', #21173, .T. ) ;
#54295 = VERTEX_POINT ( 'NONE', #13527 ) ;
#54296 = CARTESIAN_POINT ( 'NONE',  ( -92.75707362346618368, -5.598654528085801552, 7.705886871421367523 ) ) ;
#54297 = CARTESIAN_POINT ( 'NONE',  ( -169.0429263765338135, -9.058813317711329915, -2.943386871421370898 ) ) ;
#54298 = CARTESIAN_POINT ( 'NONE',  ( 12.34222745343792127, 114.9999999999999574, 10.18181818181818166 ) ) ;
#54299 = DIRECTION ( 'NONE',  ( 1.000000000000000000, 0.000000000000000000, -0.000000000000000000 ) ) ;
#54300 = EDGE_CURVE ( 'NONE', #46307, #45388, #18166, .T. ) ;
#54301 =( NAMED_UNIT ( * ) PLANE_ANGLE_UNIT ( ) SI_UNIT ( $, .RADIAN. ) );
#54302 = ORIENTED_EDGE ( 'NONE', *, *, #30980, .F. ) ;
#54303 =( GEOMETRIC_REPRESENTATION_CONTEXT ( 3 ) GLOBAL_UNCERTAINTY_ASSIGNED_CONTEXT ( ( #7439 ) ) GLOBAL_UNIT_ASSIGNED_CONTEXT ( ( #17248, #39050, #11933 ) ) REPRESENTATION_CONTEXT ( 'NONE', 'WORKASPACE' ) );
#54304 = CARTESIAN_POINT ( 'NONE',  ( -12.74999999999999822, -0.9999999999999995559, 7.000000000000001776 ) ) ;
#54305 = CARTESIAN_POINT ( 'NONE',  ( -66.14499999999998181, -4.716976649647092401, 6.492361379858946790 ) ) ;
#54306 = ORIENTED_EDGE ( 'NONE', *, *, #9040, .F. ) ;
#54307 = CARTESIAN_POINT ( 'NONE',  ( -49.94292637653380496, 0.000000000000000000, 9.524999999999991473 ) ) ;
#54308 = CARTESIAN_POINT ( 'NONE',  ( -45.00000000000000000, 9.482577857128609011, -6.485016072424587108 ) ) ;
#54309 = VERTEX_POINT ( 'NONE', #29723 ) ;
#54310 = FACE_OUTER_BOUND ( 'NONE', #47119, .T. ) ;
#54311 = ORIENTED_EDGE ( 'NONE', *, *, #21138, .T. ) ;
#54312 = MECHANICAL_DESIGN_GEOMETRIC_PRESENTATION_REPRESENTATION (  '', ( #46546 ), #390 ) ;
#54313 = TOROIDAL_SURFACE ( 'NONE', #11644, 0.5000000000000000000, 0.2500000000000000000 ) ;
#54314 = DIRECTION ( 'NONE',  ( -0.000000000000000000, -0.000000000000000000, -1.000000000000000000 ) ) ;
#54315 = ADVANCED_FACE ( 'NONE', ( #14583 ), #51516, .F. ) ;
#54316 = CARTESIAN_POINT ( 'NONE',  ( -110.9049999999999727, 2.607480562269068880, -8.024999999999993250 ) ) ;
#54317 = ORIENTED_EDGE ( 'NONE', *, *, #13220, .F. ) ;
#54318 = CARTESIAN_POINT ( 'NONE',  ( 2.755156416453790058, 1.983268963954968989, -7.000000000000002665 ) ) ;
#54319 = CARTESIAN_POINT ( 'NONE',  ( -73.04292637653379927, -9.058813317711329915, -2.943386871421370898 ) ) ;
#54320 = DIRECTION ( 'NONE',  ( -0.000000000000000000, 1.000000000000000000, -0.000000000000000000 ) ) ;
#54321 = B_SPLINE_CURVE_WITH_KNOTS ( 'NONE', 3,
 ( #32110, #61165, #56222, #65141, #23875, #17914 ),
 .UNSPECIFIED., .F., .F.,
 ( 4, 2, 4 ),
 ( 0.004189585287972440175, 0.006269578072783815043, 0.008349570857595189910 ),
 .UNSPECIFIED. ) ;
#54322 = FACE_OUTER_BOUND ( 'NONE', #64940, .T. ) ;
#54323 = CARTESIAN_POINT ( 'NONE',  ( -152.1570736234661751, -9.058813317711329915, -2.943386871421370898 ) ) ;
#54324 = AXIS2_PLACEMENT_3D ( 'NONE', #41894, #63312, #46124 ) ;
#54325 = EDGE_CURVE ( 'NONE', #2782, #36655, #8963, .T. ) ;
#54326 = CARTESIAN_POINT ( 'NONE',  ( -5.598654528085806881, 136.7449999999999761, -7.705886871421374629 ) ) ;
#54327 = CARTESIAN_POINT ( 'NONE',  ( -97.25707362346618368, 5.598654528085800663, -7.705886871421367523 ) ) ;
#54328 = CONICAL_SURFACE ( 'NONE', #59998, 5.500000000000005329, 0.7853981633974482790 ) ;
#54329 = EDGE_CURVE ( 'NONE', #57410, #32866, #49499, .T. ) ;
#54330 = DIRECTION ( 'NONE',  ( 1.000000000000000000, 0.000000000000000000, 0.000000000000000000 ) ) ;
#54331 = ORIENTED_EDGE ( 'NONE', *, *, #17803, .T. ) ;
#54332 = FILL_AREA_STYLE ('',( #53641 ) ) ;
#54333 = DIRECTION ( 'NONE',  ( 1.000000000000000000, 0.000000000000000000, 0.000000000000000000 ) ) ;
#54334 = CARTESIAN_POINT ( 'NONE',  ( -34.99999999999992895, 112.9999999999999858, -7.000000000000000000 ) ) ;
#54335 = ADVANCED_FACE ( 'NONE', ( #36051 ), #52246, .F. ) ;
#54336 = PRESENTATION_LAYER_ASSIGNMENT (  '', '', ( #28514 ) ) ;
#54337 = CARTESIAN_POINT ( 'NONE',  ( -129.5049999999999670, -6.826472737025115478, -4.959722759717899443 ) ) ;
#54338 = CARTESIAN_POINT ( 'NONE',  ( -72.00000000000000000, 13.41640786499872284, 9.500000000000000000 ) ) ;
#54339 = DIRECTION ( 'NONE',  ( -0.000000000000000000, -0.3420201433256629953, 0.9396926207859104263 ) ) ;
#54340 = CARTESIAN_POINT ( 'NONE',  ( -141.1449999999999818, -4.716976649647092401, 6.492361379858946790 ) ) ;
#54341 = STYLED_ITEM ( 'NONE', ( #37570 ), #48335 ) ;
#54342 = CARTESIAN_POINT ( 'NONE',  ( -129.7450000000000045, 4.716976649647094177, 6.492361379858945902 ) ) ;
#54343 = ORIENTED_EDGE ( 'NONE', *, *, #20239, .F. ) ;
#54344 = CARTESIAN_POINT ( 'NONE',  ( 44.82448674805845457, 10.57670410873387823, -3.609649266065385387 ) ) ;
#54345 = AXIS2_PLACEMENT_3D ( 'NONE', #12021, #33479, #16640 ) ;
#54346 = DIRECTION ( 'NONE',  ( -1.000000000000000000, 0.000000000000000000, 0.000000000000000000 ) ) ;
#54347 = UNCERTAINTY_MEASURE_WITH_UNIT (LENGTH_MEASURE( 1.000000000000000082E-05 ), #13982, 'distance_accuracy_value', 'NONE');
#54348 = CARTESIAN_POINT ( 'NONE',  ( -53.15499999999997982, 7.632228543268600340, 2.479861379858949277 ) ) ;
#54349 = SURFACE_SIDE_STYLE ('',( #11085 ) ) ;
#54350 = CARTESIAN_POINT ( 'NONE',  ( -59.99499999999996902, -6.826472737025115478, 4.959722759717900331 ) ) ;
#54351 = LINE ( 'NONE', #43845, #26414 ) ;
#54352 = FILL_AREA_STYLE_COLOUR ( '', #14459 ) ;
#54353 = FACE_OUTER_BOUND ( 'NONE', #6980, .T. ) ;
#54354 = SURFACE_SIDE_STYLE ('',( #32922 ) ) ;
#54355 = FACE_OUTER_BOUND ( 'NONE', #45443, .T. ) ;
#54356 = CARTESIAN_POINT ( 'NONE',  ( -107.9929263765337879, 8.102448949553171076, -5.886773742842744461 ) ) ;
#54357 = DIRECTION ( 'NONE',  ( 4.528264053928434474E-17, -4.528264053928433857E-17, 1.000000000000000000 ) ) ;
#54358 = VECTOR ( 'NONE', #21621, 1000.000000000000000 ) ;
#54359 = FACE_OUTER_BOUND ( 'NONE', #34330, .T. ) ;
#54360 = TOROIDAL_SURFACE ( 'NONE', #63362, 29.50000000000000000, 0.5000000000000000000 ) ;
#54361 = CARTESIAN_POINT ( 'NONE',  ( -69.99999999999998579, 50.00000000000000000, -6.999999999999988454 ) ) ;
#54362 = DIRECTION ( 'NONE',  ( 0.000000000000000000, 0.000000000000000000, -1.000000000000000000 ) ) ;
#54363 = EDGE_LOOP ( 'NONE', ( #56928, #7212, #3308, #7156, #16060, #60283, #2408, #16675 ) ) ;
#54364 = FACE_OUTER_BOUND ( 'NONE', #2710, .T. ) ;
#54365 = VERTEX_POINT ( 'NONE', #46985 ) ;
#54366 = FACE_BOUND ( 'NONE', #32375, .T. ) ;
#54367 =( GEOMETRIC_REPRESENTATION_CONTEXT ( 3 ) GLOBAL_UNCERTAINTY_ASSIGNED_CONTEXT ( ( #19874 ) ) GLOBAL_UNIT_ASSIGNED_CONTEXT ( ( #37048, #10286, #53203 ) ) REPRESENTATION_CONTEXT ( 'NONE', 'WORKASPACE' ) );
#54368 = CARTESIAN_POINT ( 'NONE',  ( 6.826472737025119919, 111.0070736234661553, 4.959722759717908325 ) ) ;
#54369 = AXIS2_PLACEMENT_3D ( 'NONE', #51468, #16211, #37686 ) ;
#54370 = DIRECTION ( 'NONE',  ( 0.000000000000000000, -1.000000000000000000, 1.301042606982604216E-14 ) ) ;
#54371 = VERTEX_POINT ( 'NONE', #36436 ) ;
#54372 = EDGE_LOOP ( 'NONE', ( #48833, #66306 ) ) ;
#54373 = SURFACE_SIDE_STYLE ('',( #28674 ) ) ;
#54374 = LINE ( 'NONE', #29011, #49603 ) ;
#54375 = EDGE_LOOP ( 'NONE', ( #43047, #40674, #28045, #590 ) ) ;
#54376 = CARTESIAN_POINT ( 'NONE',  ( 4.500000000000002665, 24.74999999999998579, 3.750000000000000000 ) ) ;
#54377 = CARTESIAN_POINT ( 'NONE',  ( -118.7070736234669539, -3.094860106631741381, -9.524999999990320987 ) ) ;
#54378 = EDGE_CURVE ( 'NONE', #40144, #21270, #63032, .T. ) ;
#54379 = AXIS2_PLACEMENT_3D ( 'NONE', #10781, #32932, #11807 ) ;
#54380 = CIRCLE ( 'NONE', #24071, 0.9999999999999995559 ) ;
#54381 = CARTESIAN_POINT ( 'NONE',  ( 7.632228543268607446, 134.0429263765338135, 2.479861379858954606 ) ) ;
#54382 = CARTESIAN_POINT ( 'NONE',  ( -87.74499999999999034, 4.716976649647094177, 6.492361379858945902 ) ) ;
#54383 = ORIENTED_EDGE ( 'NONE', *, *, #58011, .T. ) ;
#54384 = EDGE_CURVE ( 'NONE', #12618, #2274, #23786, .T. ) ;
#54385 = DIRECTION ( 'NONE',  ( -0.000000000000000000, -0.000000000000000000, -1.000000000000000000 ) ) ;
#54386 = EDGE_CURVE ( 'NONE', #18337, #65809, #8479, .T. ) ;
#54387 = CARTESIAN_POINT ( 'NONE',  ( 86.21825843581743243, 5.000000000000000000, -39.83014742847162637 ) ) ;
#54388 = CARTESIAN_POINT ( 'NONE',  ( 0.000000000000000000, -2.500000000000000000, 0.000000000000000000 ) ) ;
#54389 = UNCERTAINTY_MEASURE_WITH_UNIT (LENGTH_MEASURE( 1.000000000000000082E-05 ), #3847, 'distance_accuracy_value', 'NONE');
#54390 = VERTEX_POINT ( 'NONE', #61548 ) ;
#54391 = CARTESIAN_POINT ( 'NONE',  ( 4.041451884327375232, 2.500000000000000000, -7.000000000000002665 ) ) ;
#54392 =( NAMED_UNIT ( * ) SI_UNIT ( $, .STERADIAN. ) SOLID_ANGLE_UNIT ( ) );
#54393 = ADVANCED_FACE ( 'NONE', ( #29562 ), #45779, .T. ) ;
#54394 = CIRCLE ( 'NONE', #3812, 0.5000000000000000000 ) ;
#54395 = EDGE_CURVE ( 'NONE', #49493, #29467, #35193, .T. ) ;
#54396 = VERTEX_POINT ( 'NONE', #24609 ) ;
#54397 = EDGE_CURVE ( 'NONE', #37946, #65858, #14415, .T. ) ;
#54398 = ORIENTED_EDGE ( 'NONE', *, *, #52653, .T. ) ;
#54399 = CARTESIAN_POINT ( 'NONE',  ( -195.0000000000000000, 0.000000000000000000, 0.000000000000000000 ) ) ;
#54400 = CARTESIAN_POINT ( 'NONE',  ( 8.250000000000001776, 30.74999999999998579, 4.000000000000000000 ) ) ;
#54401 = FACE_OUTER_BOUND ( 'NONE', #1961, .T. ) ;
#54402 = CIRCLE ( 'NONE', #16298, 8.000000000000000000 ) ;
#54403 = SURFACE_STYLE_FILL_AREA ( #37940 ) ;
#54404 = CARTESIAN_POINT ( 'NONE',  ( -183.0000000000000000, 7.623482428031956637, -5.710353812986356026 ) ) ;
#54405 = MECHANICAL_DESIGN_GEOMETRIC_PRESENTATION_REPRESENTATION (  '', ( #16303 ), #45486 ) ;
#54406 =( BOUNDED_CURVE ( )  B_SPLINE_CURVE ( 2, ( #62936, #45442, #45770, #50672, #2413, #23927, #66862, #18666, #40485, #37662, #16183 ),
 .UNSPECIFIED., .F., .F. ) 
 B_SPLINE_CURVE_WITH_KNOTS ( ( 3, 2, 2, 2, 2, 3 ),
 ( 0.7282608695652174058, 0.7304347826086956541, 0.7326086956521739024, 0.7347826086956521507, 0.7369565217391303991, 0.7391304347826086474 ),
 .UNSPECIFIED. ) 
 CURVE ( )  GEOMETRIC_REPRESENTATION_ITEM ( )  RATIONAL_B_SPLINE_CURVE ( ( 1.000000000000000000, 0.9510565162951535312, 1.000000000000000000, 0.9510565162951535312, 1.000000000000000000, 0.9510565162951535312, 1.000000000000000000, 0.9510565162951535312, 1.000000000000000000, 0.9510565162951535312, 1.000000000000000000 ) ) 
 REPRESENTATION_ITEM ( '' )  );
#54407 = LINE ( 'NONE', #27306, #49738 ) ;
#54408 = EDGE_CURVE ( 'NONE', #37329, #17336, #57334, .T. ) ;
#54409 = CARTESIAN_POINT ( 'NONE',  ( -7.789749869348518985, 153.4012064374781517, -3.257487185497862203 ) ) ;
#54410 = ORIENTED_EDGE ( 'NONE', *, *, #23654, .T. ) ;
#54411 = FACE_BOUND ( 'NONE', #10135, .T. ) ;
#54412 = VECTOR ( 'NONE', #44736, 1000.000000000000000 ) ;
#54413 = CARTESIAN_POINT ( 'NONE',  ( 74.99999999999998579, 119.9999999999997584, 9.500000000000000000 ) ) ;
#54414 = EDGE_LOOP ( 'NONE', ( #57509, #54107, #69449, #190 ) ) ;
#54415 = CARTESIAN_POINT ( 'NONE',  ( -163.5550000000000068, 0.000000000000000000, 8.024999999999991473 ) ) ;
#54416 = DIRECTION ( 'NONE',  ( 0.000000000000000000, -1.000000000000000000, 0.000000000000000000 ) ) ;
#54417 = CARTESIAN_POINT ( 'NONE',  ( -147.6570736234662036, 9.058813317711329915, 2.943386871421369566 ) ) ;
#54418 = CARTESIAN_POINT ( 'NONE',  ( -175.4949999999999761, 6.826472737025113702, -4.959722759717902107 ) ) ;
#54419 = CARTESIAN_POINT ( 'NONE',  ( -171.4449999999999932, 0.000000000000000000, 8.024999999999991473 ) ) ;
#54420 = ORIENTED_EDGE ( 'NONE', *, *, #20970, .F. ) ;
#54421 = CIRCLE ( 'NONE', #52208, 8.499999999999992895 ) ;
#54422 = CIRCLE ( 'NONE', #34206, 0.2500000000000002220 ) ;
#54423 = DIRECTION ( 'NONE',  ( -1.000000000000000000, 0.000000000000000000, 0.000000000000000000 ) ) ;
#54424 = CARTESIAN_POINT ( 'NONE',  ( -8.437984349512095861, 150.6929263765338192, -5.166775262442723748E-16 ) ) ;
#54425 = CARTESIAN_POINT ( 'NONE',  ( -84.35499999999998977, -4.716976649647093289, -6.492361379858945902 ) ) ;
#54426 = CARTESIAN_POINT ( 'NONE',  ( 24.50817055128190347, 25.15492634751250733, 27.39952695552187478 ) ) ;
#54427 =( NAMED_UNIT ( * ) PLANE_ANGLE_UNIT ( ) SI_UNIT ( $, .RADIAN. ) );
#54428 = AXIS2_PLACEMENT_3D ( 'NONE', #13678, #35138, #29856 ) ;
#54429 = CARTESIAN_POINT ( 'NONE',  ( -79.34499999999998465, 7.632228543268599452, -2.479861379858951942 ) ) ;
#54430 = CARTESIAN_POINT ( 'NONE',  ( -3.094860106618432471, 134.7050000000000125, -9.525000000000000355 ) ) ;
#54431 = CARTESIAN_POINT ( 'NONE',  ( -134.4570736234661865, -9.058813317711329915, 2.943386871421371787 ) ) ;
#54432 = TOROIDAL_SURFACE ( 'NONE', #10670, 0.5000000000000000000, 0.2500000000000000000 ) ;
#54433 = MECHANICAL_DESIGN_GEOMETRIC_PRESENTATION_REPRESENTATION (  '', ( #24114 ), #8420 ) ;
#54434 = DIRECTION ( 'NONE',  ( 0.000000000000000000, 0.000000000000000000, -1.000000000000000000 ) ) ;
#54435 = UNCERTAINTY_MEASURE_WITH_UNIT (LENGTH_MEASURE( 1.000000000000000082E-05 ), #33642, 'distance_accuracy_value', 'NONE');
#54436 = ADVANCED_FACE ( 'NONE', ( #61231 ), #30584, .T. ) ;
#54437 = FILL_AREA_STYLE_COLOUR ( '', #65172 ) ;
#54438 = PRESENTATION_STYLE_ASSIGNMENT (( #10165 ) ) ;
#54439 = ORIENTED_EDGE ( 'NONE', *, *, #46754, .F. ) ;
#54440 = DIRECTION ( 'NONE',  ( 0.000000000000000000, 0.000000000000000000, 1.000000000000000000 ) ) ;
#54441 = LINE ( 'NONE', #44969, #50564 ) ;
#54442 = PRESENTATION_LAYER_ASSIGNMENT (  '', '', ( #30837 ) ) ;
#54443 = COLOUR_RGB ( '', 0.09019608, 0.27058824, 0.51372549) ;
#54444 = CARTESIAN_POINT ( 'NONE',  ( 24.21231517720798010, 112.9999999999999858, -7.500000000000000000 ) ) ;
#54445 = VECTOR ( 'NONE', #13462, 1000.000000000000000 ) ;
#54446 = CARTESIAN_POINT ( 'NONE',  ( -44.99999999999998579, 119.9999999999999716, 10.00000000000000000 ) ) ;
#54447 = CARTESIAN_POINT ( 'NONE',  ( 44.50000000000000000, 10.36037961002804408, 3.500000000000000000 ) ) ;
#54448 = ORIENTED_EDGE ( 'NONE', *, *, #36135, .T. ) ;
#54449 = EDGE_LOOP ( 'NONE', ( #3493, #42089, #32117, #36144 ) ) ;
#54450 = CARTESIAN_POINT ( 'NONE',  ( 1.000000000000000888, 14.00000000000000533, -35.50000000000000000 ) ) ;
#54451 = CARTESIAN_POINT ( 'NONE',  ( 1.000000000000000000, -60.04052944165106709, 36.50000000000000000 ) ) ;
#54452 = VECTOR ( 'NONE', #47258, 1000.000000000000000 ) ;
#54453 = PRESENTATION_STYLE_ASSIGNMENT (( #59364 ) ) ;
#54454 =( NAMED_UNIT ( * ) SI_UNIT ( $, .STERADIAN. ) SOLID_ANGLE_UNIT ( ) );
#54455 =( NAMED_UNIT ( * ) PLANE_ANGLE_UNIT ( ) SI_UNIT ( $, .RADIAN. ) );
#54456 = DIRECTION ( 'NONE',  ( 1.000000000000000000, 0.000000000000000000, 0.000000000000000000 ) ) ;
#54457 = VERTEX_POINT ( 'NONE', #46848 ) ;
#54458 = CARTESIAN_POINT ( 'NONE',  ( -110.1549999999999869, 7.632228543268600340, 2.479861379858949277 ) ) ;
#54459 = ORIENTED_EDGE ( 'NONE', *, *, #45805, .F. ) ;
#54460 = EDGE_CURVE ( 'NONE', #5580, #12869, #26044, .T. ) ;
#54461 = EDGE_LOOP ( 'NONE', ( #60844, #39212, #44987, #46590 ) ) ;
#54462 = DIRECTION ( 'NONE',  ( -0.000000000000000000, 0.000000000000000000, -1.000000000000000000 ) ) ;
#54463 = CARTESIAN_POINT ( 'NONE',  ( -6.767634268437465295, -2.367558512213881361, 2.278113600022078078 ) ) ;
#54464 = ORIENTED_EDGE ( 'NONE', *, *, #58361, .F. ) ;
#54465 = CYLINDRICAL_SURFACE ( 'NONE', #22031, 0.5000000000000004441 ) ;
#54466 =( NAMED_UNIT ( * ) PLANE_ANGLE_UNIT ( ) SI_UNIT ( $, .RADIAN. ) );
#54467 = ORIENTED_EDGE ( 'NONE', *, *, #68101, .F. ) ;
#54468 = EDGE_CURVE ( 'NONE', #36987, #33115, #46884, .T. ) ;
#54469 = PRESENTATION_LAYER_ASSIGNMENT (  '', '', ( #29781 ) ) ;
#54470 = VERTEX_POINT ( 'NONE', #41531 ) ;
#54471 = CIRCLE ( 'NONE', #55585, 0.9999999999999986677 ) ;
#54472 = DIRECTION ( 'NONE',  ( -1.000000000000000000, -0.000000000000000000, -0.000000000000000000 ) ) ;
#54473 = FILL_AREA_STYLE ('',( #42943 ) ) ;
#54474 =( LENGTH_UNIT ( ) NAMED_UNIT ( * ) SI_UNIT ( .MILLI., .METRE. ) );
#54475 = ORIENTED_EDGE ( 'NONE', *, *, #24503, .T. ) ;
#54476 = CARTESIAN_POINT ( 'NONE',  ( 4.716976649647099507, 131.6429263765338362, -6.492361379858953008 ) ) ;
#54477 = CARTESIAN_POINT ( 'NONE',  ( -5.000000000000000000, 0.000000000000000000, 0.7500000000000000000 ) ) ;
#54478 = DIRECTION ( 'NONE',  ( 0.000000000000000000, 0.000000000000000000, 1.000000000000000000 ) ) ;
#54479 = DIRECTION ( 'NONE',  ( 1.000000000000000000, 0.000000000000000000, 0.000000000000000000 ) ) ;
#54480 = VERTEX_POINT ( 'NONE', #47535 ) ;
#54481 = EDGE_CURVE ( 'NONE', #24854, #4102, #10354, .T. ) ;
#54482 = EDGE_LOOP ( 'NONE', ( #61478, #51342, #6284 ) ) ;
#54483 = CARTESIAN_POINT ( 'NONE',  ( -50.84292637653378932, 9.058813317711329915, -2.943386871421373119 ) ) ;
#54484 = STYLED_ITEM ( 'NONE', ( #2684 ), #49191 ) ;
#54485 = CARTESIAN_POINT ( 'NONE',  ( 0.000000000000000000, 0.000000000000000000, 0.000000000000000000 ) ) ;
#54486 = DIRECTION ( 'NONE',  ( 0.000000000000000000, 0.000000000000000000, 1.000000000000000000 ) ) ;
#54487 = CARTESIAN_POINT ( 'NONE',  ( -159.0570736234661808, 0.000000000000000000, 9.524999999999991473 ) ) ;
#54488 = AXIS2_PLACEMENT_3D ( 'NONE', #43202, #36531, #34925 ) ;
#54489 = CARTESIAN_POINT ( 'NONE',  ( -147.3549999999999898, -4.716976649647093289, -6.492361379858945902 ) ) ;
#54490 = FACE_OUTER_BOUND ( 'NONE', #40002, .T. ) ;
#54491 = UNCERTAINTY_MEASURE_WITH_UNIT (LENGTH_MEASURE( 1.000000000000000082E-05 ), #15115, 'distance_accuracy_value', 'NONE');
#54492 = ORIENTED_EDGE ( 'NONE', *, *, #6942, .F. ) ;
#54493 = CARTESIAN_POINT ( 'NONE',  ( -2.607480562269032909, 116.4070736234661609, 8.025000000000032330 ) ) ;
#54494 = EDGE_CURVE ( 'NONE', #46872, #26109, #41896, .T. ) ;
#54495 =( LENGTH_UNIT ( ) NAMED_UNIT ( * ) SI_UNIT ( .MILLI., .METRE. ) );
#54496 = VERTEX_POINT ( 'NONE', #42586 ) ;
#54497 = VERTEX_POINT ( 'NONE', #69292 ) ;
#54498 = FACE_OUTER_BOUND ( 'NONE', #53673, .T. ) ;
#54499 = CARTESIAN_POINT ( 'NONE',  ( -108.5929263765347770, -3.094860106634296670, -9.524999999988466470 ) ) ;
#54500 = CARTESIAN_POINT ( 'NONE',  ( -60.50499999999998124, -6.826472737025115478, -4.959722759717899443 ) ) ;
#54502 = EDGE_LOOP ( 'NONE', ( #9886, #47286, #23351, #22855 ) ) ;
#54501 =( GEOMETRIC_REPRESENTATION_CONTEXT ( 3 ) GLOBAL_UNCERTAINTY_ASSIGNED_CONTEXT ( ( #19351 ) ) GLOBAL_UNIT_ASSIGNED_CONTEXT ( ( #59201, #20908, #27184 ) ) REPRESENTATION_CONTEXT ( 'NONE', 'WORKASPACE' ) );
#54503 = CARTESIAN_POINT ( 'NONE',  ( -45.50000000000000000, 99.99999999999992895, -10.00000000000000000 ) ) ;
#54504 = DIRECTION ( 'NONE',  ( -0.000000000000000000, -0.000000000000000000, -1.000000000000000000 ) ) ;
#54505 = LINE ( 'NONE', #43334, #26157 ) ;
#54506 = LINE ( 'NONE', #64381, #43695 ) ;
#54507 = AXIS2_PLACEMENT_3D ( 'NONE', #59145, #15905, #53876 ) ;
#54508 = DIRECTION ( 'NONE',  ( 0.000000000000000000, 0.000000000000000000, -1.000000000000000000 ) ) ;
#54509 = CARTESIAN_POINT ( 'NONE',  ( 57.74999999999998579, 30.74999999999999289, -3.750000000000000000 ) ) ;
#54510 = CIRCLE ( 'NONE', #44476, 1.000000000000000000 ) ;
#54511 = ORIENTED_EDGE ( 'NONE', *, *, #17806, .F. ) ;
#54512 = SURFACE_STYLE_FILL_AREA ( #33076 ) ;
#54513 = PRESENTATION_LAYER_ASSIGNMENT (  '', '', ( #41089 ) ) ;
#54514 = CARTESIAN_POINT ( 'NONE',  ( -5.196152422706636465, 1.107695154586736175, -9.000000000000003553 ) ) ;
#54515 = FILL_AREA_STYLE_COLOUR ( '', #66850 ) ;
#54516 = CARTESIAN_POINT ( 'NONE',  ( -23.71231517720798010, 112.9999999999999858, -9.500000000000000000 ) ) ;
#54517 = DIRECTION ( 'NONE',  ( -0.000000000000000000, -0.000000000000000000, 1.000000000000000000 ) ) ;
#54518 = CARTESIAN_POINT ( 'NONE',  ( -105.7449999999999903, 4.716976649647094177, 6.492361379858945902 ) ) ;
#54519 = CARTESIAN_POINT ( 'NONE',  ( 3.094860106618431583, 156.0949999999999989, 9.525000000000000355 ) ) ;
#54520 = CARTESIAN_POINT ( 'NONE',  ( -91.64499999999999602, 4.716976649647091513, -6.492361379858946790 ) ) ;
#54521 = FACE_OUTER_BOUND ( 'NONE', #42561, .T. ) ;
#54522 = CARTESIAN_POINT ( 'NONE',  ( 0.4882456337924178658, 112.0289864169386789, -8.025000000000002132 ) ) ;
#54523 = CARTESIAN_POINT ( 'NONE',  ( 9.827790563157511022E-16, 87.30187232391182306, -8.025000000000000355 ) ) ;
#54524 = CARTESIAN_POINT ( 'NONE',  ( 32.00000000000000711, 42.00000000000000000, -36.50000000000000000 ) ) ;
#54525 = UNCERTAINTY_MEASURE_WITH_UNIT (LENGTH_MEASURE( 1.000000000000000082E-05 ), #17244, 'distance_accuracy_value', 'NONE');
#54526 = VECTOR ( 'NONE', #3955, 1000.000000000000227 ) ;
#54527 = ADVANCED_FACE ( 'NONE', ( #57694 ), #37358, .F. ) ;
#54528 = AXIS2_PLACEMENT_3D ( 'NONE', #38986, #33654, #61077 ) ;
#54529 = ORIENTED_EDGE ( 'NONE', *, *, #41495, .F. ) ;
#54530 = CARTESIAN_POINT ( 'NONE',  ( -123.5929263765337822, -3.094860106618431139, -9.524999999999991473 ) ) ;
#54531 = CARTESIAN_POINT ( 'NONE',  ( -144.1449999999999818, -4.716976649647092401, 6.492361379858946790 ) ) ;
#54532 = PRESENTATION_STYLE_ASSIGNMENT (( #37731 ) ) ;
#54533 = AXIS2_PLACEMENT_3D ( 'NONE', #69499, #21296, #32919 ) ;
#54534 = VECTOR ( 'NONE', #42165, 1000.000000000000227 ) ;
#54535 = CARTESIAN_POINT ( 'NONE',  ( 5.000000000000000000, 6.123233995736766282E-16, 42.50000000000000000 ) ) ;
#54536 = ORIENTED_EDGE ( 'NONE', *, *, #56423, .F. ) ;
#54537 = VERTEX_POINT ( 'NONE', #47177 ) ;
#54538 = AXIS2_PLACEMENT_3D ( 'NONE', #45723, #12620, #66806 ) ;
#54539 = CARTESIAN_POINT ( 'NONE',  ( 39.24999999999999289, 15.74999999999997513, -4.000000000000000000 ) ) ;
#54540 = DIRECTION ( 'NONE',  ( 0.000000000000000000, 0.000000000000000000, 1.000000000000000000 ) ) ;
#54541 = ADVANCED_FACE ( 'NONE', ( #62947 ), #42923, .F. ) ;
#54542 = SPHERICAL_SURFACE ( 'NONE', #39337, 1.000000000000000000 ) ;
#54543 = CARTESIAN_POINT ( 'NONE',  ( -50.60707362346616378, -8.102448949553174629, 5.886773742842742685 ) ) ;
#54544 = CARTESIAN_POINT ( 'NONE',  ( -151.6429263765338078, -5.598654528085801552, 7.705886871421367523 ) ) ;
#54545 = ORIENTED_EDGE ( 'NONE', *, *, #9112, .T. ) ;
#54546 = CARTESIAN_POINT ( 'NONE',  ( -140.3049999999999500, 8.437984349512086979, -1.550032578732815448E-15 ) ) ;
#54548 = ADVANCED_FACE ( 'NONE', ( #255 ), #7341, .T. ) ;
#54547 = ORIENTED_EDGE ( 'NONE', *, *, #40551, .F. ) ;
#54549 = AXIS2_PLACEMENT_3D ( 'NONE', #28132, #60181, #11991 ) ;
#54550 = ADVANCED_FACE ( 'NONE', ( #43972 ), #6985, .T. ) ;
#54551 = ORIENTED_EDGE ( 'NONE', *, *, #38007, .T. ) ;
#54552 = DIRECTION ( 'NONE',  ( -0.000000000000000000, -1.000000000000000000, -0.000000000000000000 ) ) ;
#54553 = ORIENTED_EDGE ( 'NONE', *, *, #16502, .F. ) ;
#54554 = MECHANICAL_DESIGN_GEOMETRIC_PRESENTATION_REPRESENTATION (  '', ( #38890 ), #52386 ) ;
#54555 = CARTESIAN_POINT ( 'NONE',  ( -55.11316530407558645, -8.908978040980905178, -2.125589934168188755 ) ) ;
#54556 = CARTESIAN_POINT ( 'NONE',  ( -5.598654528085806881, 130.7450000000000045, -7.705886871421374629 ) ) ;
#54557 = SURFACE_SIDE_STYLE ('',( #38778 ) ) ;
#54558 = CIRCLE ( 'NONE', #59086, 1.000000000000000000 ) ;
#54559 = EDGE_LOOP ( 'NONE', ( #3233, #38849, #13377, #46489 ) ) ;
#54561 = EDGE_CURVE ( 'NONE', #9250, #53882, #65425, .T. ) ;
#54560 = CARTESIAN_POINT ( 'NONE',  ( 8.102448949553179958, 133.5049999999999955, 5.886773742842750679 ) ) ;
#54562 = CARTESIAN_POINT ( 'NONE',  ( -50.75499999999999545, 4.716976649647091513, -6.492361379858946790 ) ) ;
#54563 = AXIS2_PLACEMENT_3D ( 'NONE', #69089, #69424, #5047 ) ;
#54564 = CARTESIAN_POINT ( 'NONE',  ( -115.6449999999999818, 4.716976649647091513, -6.492361379858946790 ) ) ;
#54565 = CARTESIAN_POINT ( 'NONE',  ( -40.82744559481908908, 108.1269596360033347, -3.302666768370059902 ) ) ;
#54566 = EDGE_LOOP ( 'NONE', ( #45734, #39156, #56942, #36706 ) ) ;
#54567 = CARTESIAN_POINT ( 'NONE',  ( -1.166476076187854022E-15, 154.0550000000000068, 9.525000000000000355 ) ) ;
#54568 = CARTESIAN_POINT ( 'NONE',  ( 0.000000000000000000, 0.000000000000000000, -5.000000000000000000 ) ) ;
#54569 = UNCERTAINTY_MEASURE_WITH_UNIT (LENGTH_MEASURE( 1.000000000000000082E-05 ), #7356, 'distance_accuracy_value', 'NONE');
#54570 = EDGE_CURVE ( 'NONE', #62177, #60780, #55270, .T. ) ;
#54571 = CARTESIAN_POINT ( 'NONE',  ( 33.00000000000000000, 15.00000000000000000, -80.00402776293826435 ) ) ;
#54572 = CARTESIAN_POINT ( 'NONE',  ( 26.25000000000001066, 19.24999999999997868, 4.000000000000000000 ) ) ;
#54573 =( NAMED_UNIT ( * ) SI_UNIT ( $, .STERADIAN. ) SOLID_ANGLE_UNIT ( ) );
#54574 = EDGE_CURVE ( 'NONE', #16179, #34526, #65706, .T. ) ;
#54575 = ORIENTED_EDGE ( 'NONE', *, *, #17978, .F. ) ;
#54576 = SURFACE_STYLE_FILL_AREA ( #60527 ) ;
#54577 = DIRECTION ( 'NONE',  ( 1.000000000000000000, 0.000000000000000000, 0.000000000000000000 ) ) ;
#54578 = CARTESIAN_POINT ( 'NONE',  ( -167.9050000000000011, 2.607480562269068880, -8.024999999999993250 ) ) ;
#54579 = ORIENTED_EDGE ( 'NONE', *, *, #26889, .F. ) ;
#54580 = DIRECTION ( 'NONE',  ( 0.000000000000000000, 0.000000000000000000, -1.000000000000000000 ) ) ;
#54581 = UNCERTAINTY_MEASURE_WITH_UNIT (LENGTH_MEASURE( 1.000000000000000082E-05 ), #12438, 'distance_accuracy_value', 'NONE');
#54582 = DIRECTION ( 'NONE',  ( -0.000000000000000000, -0.000000000000000000, -1.000000000000000000 ) ) ;
#54583 = EDGE_CURVE ( 'NONE', #65886, #25898, #44666, .T. ) ;
#54584 = DIRECTION ( 'NONE',  ( 0.000000000000000000, 0.000000000000000000, -1.000000000000000000 ) ) ;
#54585 = CARTESIAN_POINT ( 'NONE',  ( 53.25000000000000000, 25.24999999999998579, 4.000000000000000000 ) ) ;
#54586 = ORIENTED_EDGE ( 'NONE', *, *, #44776, .T. ) ;
#54587 = CARTESIAN_POINT ( 'NONE',  ( -45.07463294676507815, 8.173953816254709182, -3.593564820753269107 ) ) ;
#54588 = TOROIDAL_SURFACE ( 'NONE', #2831, 9.525000000000000355, 1.000000000000000888 ) ;
#54589 = DIRECTION ( 'NONE',  ( -1.000000000000000000, 0.000000000000000000, 0.000000000000000000 ) ) ;
#54590 = CARTESIAN_POINT ( 'NONE',  ( -86.60500000000000398, 6.826472737025113702, -4.959722759717902107 ) ) ;
#54591 = ORIENTED_EDGE ( 'NONE', *, *, #57243, .T. ) ;
#54592 = DIRECTION ( 'NONE',  ( 0.000000000000000000, 0.000000000000000000, 1.000000000000000000 ) ) ;
#54593 = AXIS2_PLACEMENT_3D ( 'NONE', #49385, #64854, #26840 ) ;
#54594 = AXIS2_PLACEMENT_3D ( 'NONE', #61748, #29043, #23117 ) ;
#54595 = CARTESIAN_POINT ( 'NONE',  ( -15.98999599679679839, 118.4999999999999716, -10.00000000000000000 ) ) ;
#54596 = CARTESIAN_POINT ( 'NONE',  ( -69.50707362346615525, 8.102448949553176405, 5.886773742842740909 ) ) ;
#54597 = CARTESIAN_POINT ( 'NONE',  ( -75.00000000000000000, 8.745397170020957844, -6.877347455809927013 ) ) ;
#54598 = VERTEX_POINT ( 'NONE', #60772 ) ;
#54599 =( NAMED_UNIT ( * ) SI_UNIT ( $, .STERADIAN. ) SOLID_ANGLE_UNIT ( ) );
#54601 = FACE_OUTER_BOUND ( 'NONE', #15759, .T. ) ;
#54600 = SURFACE_SIDE_STYLE ('',( #32438 ) ) ;
#54602 = VECTOR ( 'NONE', #28760, 1000.000000000000000 ) ;
#54603 = CARTESIAN_POINT ( 'NONE',  ( -100.4050000000000011, -2.607480562269069768, 8.024999999999991473 ) ) ;
#54604 = CARTESIAN_POINT ( 'NONE',  ( -10.01517768586949231, 131.1949999999999363, -6.132527647946036459E-16 ) ) ;
#54605 = CARTESIAN_POINT ( 'NONE',  ( -113.0949999999999989, -2.607480562269071545, -8.024999999999991473 ) ) ;
#54606 = LINE ( 'NONE', #11005, #12256 ) ;
#54608 = CARTESIAN_POINT ( 'NONE',  ( -154.1070736234661922, 8.102448949553172852, -5.886773742842744461 ) ) ;
#54607 = LINE ( 'NONE', #65158, #15563 ) ;
#54609 = CARTESIAN_POINT ( 'NONE',  ( -149.6929263765338192, 10.01517768586948698, -1.839758294383808571E-15 ) ) ;
#54610 = CARTESIAN_POINT ( 'NONE',  ( -175.3449999999999989, 7.632228543268599452, -2.479861379858951942 ) ) ;
#54611 = CARTESIAN_POINT ( 'NONE',  ( 47.50000000000000000, 14.49137674618942562, -9.500000000000000000 ) ) ;
#54612 = LINE ( 'NONE', #32452, #45112 ) ;
#54613 = EDGE_LOOP ( 'NONE', ( #39515, #4539 ) ) ;
#54614 = CARTESIAN_POINT ( 'NONE',  ( 25.00000000000001421, 43.00000000000000000, -29.68999999999999417 ) ) ;
#54615 = LINE ( 'NONE', #55308, #55274 ) ;
#54616 = ORIENTED_EDGE ( 'NONE', *, *, #62164, .T. ) ;
#54617 = CARTESIAN_POINT ( 'NONE',  ( -66.44292637653380496, -1.166476076187852838E-15, -9.524999999999991473 ) ) ;
#54618 = FACE_OUTER_BOUND ( 'NONE', #3511, .T. ) ;
#54619 = CARTESIAN_POINT ( 'NONE',  ( 3.000000000000002665, 43.00000000000000000, -90.00000000000000000 ) ) ;
#54620 = EDGE_CURVE ( 'NONE', #46203, #30560, #21788, .T. ) ;
#54621 = CARTESIAN_POINT ( 'NONE',  ( -142.1929263765337339, -10.01517768586948698, 6.132527647946031529E-16 ) ) ;
#54622 = FACE_OUTER_BOUND ( 'NONE', #68124, .T. ) ;
#54623 = EDGE_CURVE ( 'NONE', #48074, #51470, #17479, .T. ) ;
#54624 = LINE ( 'NONE', #10089, #16256 ) ;
#54625 = COLOUR_RGB ( '', 0.66274510, 0.83137255, 0.94901961) ;
#54626 = ORIENTED_EDGE ( 'NONE', *, *, #34052, .F. ) ;
#54627 = CARTESIAN_POINT ( 'NONE',  ( -172.2549999999999955, -4.716976649647092401, 6.492361379858946790 ) ) ;
#54628 = EDGE_CURVE ( 'NONE', #67437, #52838, #56951, .T. ) ;
#54629 = VECTOR ( 'NONE', #27376, 1000.000000000000000 ) ;
#54630 = ORIENTED_EDGE ( 'NONE', *, *, #6901, .F. ) ;
#54631 = CARTESIAN_POINT ( 'NONE',  ( 57.00000000000000000, 16.00000000000000000, 60.00402776293825724 ) ) ;
#54632 = CARTESIAN_POINT ( 'NONE',  ( 31.00000000000001421, 42.00000000000000000, 36.50000000000000000 ) ) ;
#54633 = FILL_AREA_STYLE_COLOUR ( '', #13884 ) ;
#54634 = CIRCLE ( 'NONE', #46880, 8.999999999999994671 ) ;
#54635 = CARTESIAN_POINT ( 'NONE',  ( 12.50000000000000355, 30.74999999999998579, -3.750000000000000000 ) ) ;
#54636 = B_SPLINE_CURVE_WITH_KNOTS ( 'NONE', 3,
 ( #8222, #46232, #45866, #2530, #14191, #18760, #25085, #24373 ),
 .UNSPECIFIED., .F., .F.,
 ( 4, 2, 2, 4 ),
 ( 2.544316211735810720E-07, 0.002094919859796807744, 0.003142252573884624176, 0.004189585287972440175 ),
 .UNSPECIFIED. ) ;
#54637 = DIRECTION ( 'NONE',  ( 1.000000000000000000, 0.000000000000000000, 0.000000000000000000 ) ) ;
#54638 = CARTESIAN_POINT ( 'NONE',  ( -9.827790563157511022E-16, 155.5570736234661524, 8.025000000000000355 ) ) ;
#54639 = ORIENTED_EDGE ( 'NONE', *, *, #6663, .F. ) ;
#54640 = CARTESIAN_POINT ( 'NONE',  ( 7.632228543268607446, 137.0429263765338135, 2.479861379858954606 ) ) ;
#54641 = CARTESIAN_POINT ( 'NONE',  ( -80.45499999999998408, 7.632228543268599452, -2.479861379858951942 ) ) ;
#54642 = UNCERTAINTY_MEASURE_WITH_UNIT (LENGTH_MEASURE( 1.000000000000000082E-05 ), #57357, 'distance_accuracy_value', 'NONE');
#54643 = CARTESIAN_POINT ( 'NONE',  ( 8.000000000000030198, 5.000000000000000000, -29.00402776293826079 ) ) ;
#54644 = ADVANCED_FACE ( 'NONE', ( #73 ), #55314, .F. ) ;
#54645 = AXIS2_PLACEMENT_3D ( 'NONE', #11120, #64610, #22733 ) ;
#54646 = DIRECTION ( 'NONE',  ( 0.000000000000000000, 0.000000000000000000, -1.000000000000000000 ) ) ;
#54647 = FILL_AREA_STYLE ('',( #58903 ) ) ;
#54648 =( LENGTH_UNIT ( ) NAMED_UNIT ( * ) SI_UNIT ( .MILLI., .METRE. ) );
#54649 = CARTESIAN_POINT ( 'NONE',  ( 75.83633811589984930, 0.9999999999999991118, 66.72655454856716517 ) ) ;
#54650 = ORIENTED_EDGE ( 'NONE', *, *, #42771, .F. ) ;
#54651 = CARTESIAN_POINT ( 'NONE',  ( 33.00000000000000000, 15.00000000000000000, -79.00402776293826435 ) ) ;
#54652 = CARTESIAN_POINT ( 'NONE',  ( -59.84499999999998465, -7.632228543268599452, 2.479861379858951054 ) ) ;
#54653 = EDGE_LOOP ( 'NONE', ( #30130, #5916, #29821 ) ) ;
#54654 = CARTESIAN_POINT ( 'NONE',  ( -18.25000000000000711, 0.000000000000000000, 4.000000000000000000 ) ) ;
#54655 = CARTESIAN_POINT ( 'NONE',  ( -45.89386150022815514, 9.348154474468870490, -6.165151716360228740 ) ) ;
#54656 = ORIENTED_EDGE ( 'NONE', *, *, #66817, .T. ) ;
#54657 = FILL_AREA_STYLE ('',( #5759 ) ) ;
#54658 = SURFACE_STYLE_FILL_AREA ( #32873 ) ;
#54659 = ORIENTED_EDGE ( 'NONE', *, *, #46595, .F. ) ;
#54660 = STYLED_ITEM ( 'NONE', ( #53948 ), #508 ) ;
#54661 = CARTESIAN_POINT ( 'NONE',  ( 45.00000000000000000, 10.69371294336137979, -5.999999999999999112 ) ) ;
#54662 = CARTESIAN_POINT ( 'NONE',  ( -75.00000000000000000, 7.966012280117817923, 7.000000003579910590 ) ) ;
#54663 = CARTESIAN_POINT ( 'NONE',  ( -113.3049999999999784, 8.437984349512085203, -1.550032578732815448E-15 ) ) ;
#54664 = ORIENTED_EDGE ( 'NONE', *, *, #8673, .F. ) ;
#54665 = ADVANCED_FACE ( 'NONE', ( #6123 ), #30852, .F. ) ;
#54666 = LINE ( 'NONE', #6468, #52992 ) ;
#54667 =( NAMED_UNIT ( * ) SI_UNIT ( $, .STERADIAN. ) SOLID_ANGLE_UNIT ( ) );
#54668 = SURFACE_STYLE_USAGE ( .BOTH. , #48066 ) ;
#54669 = DIRECTION ( 'NONE',  ( 5.782411586589351722E-16, -1.000000000000000000, -0.000000000000000000 ) ) ;
#54670 = CARTESIAN_POINT ( 'NONE',  ( -155.1570736234661751, -9.058813317711329915, -2.943386871421370898 ) ) ;
#54671 = EDGE_CURVE ( 'NONE', #60124, #43339, #53585, .T. ) ;
#54672 = CARTESIAN_POINT ( 'NONE',  ( -10.01517768586949408, 137.1949999999999363, -6.132527647946036459E-16 ) ) ;
#54673 = CARTESIAN_POINT ( 'NONE',  ( -96.50707362346616947, 8.102448949553176405, 5.886773742842740909 ) ) ;
#54674 = FILL_AREA_STYLE_COLOUR ( '', #47125 ) ;
#54675 = ORIENTED_EDGE ( 'NONE', *, *, #14378, .T. ) ;
#54676 = FACE_OUTER_BOUND ( 'NONE', #44312, .T. ) ;
#54677 = AXIS2_PLACEMENT_3D ( 'NONE', #29396, #61736, #67387 ) ;
#54678 = CARTESIAN_POINT ( 'NONE',  ( -135.3549999999999898, -4.716976649647093289, -6.492361379858945902 ) ) ;
#54679 = COLOUR_RGB ( '', 0.31764706, 0.68627451, 0.89019608) ;
#54680 = SURFACE_STYLE_USAGE ( .BOTH. , #28636 ) ;
#54681 = CARTESIAN_POINT ( 'NONE',  ( -7.511572993685801073E-16, 2.500000000000000000, 7.000000000000000888 ) ) ;
#54682 = CARTESIAN_POINT ( 'NONE',  ( -143.6949999999999932, -8.437984349512085203, 5.166775262442717831E-16 ) ) ;
#54683 = CIRCLE ( 'NONE', #55834, 7.000000000000001776 ) ;
#54684 = CARTESIAN_POINT ( 'NONE',  ( -127.0449999999999875, 7.632228543268600340, 2.479861379858949277 ) ) ;
#54685 = ORIENTED_EDGE ( 'NONE', *, *, #1773, .F. ) ;
#54686 = DIRECTION ( 'NONE',  ( 0.000000000000000000, -0.000000000000000000, 1.000000000000000000 ) ) ;
#54687 = CARTESIAN_POINT ( 'NONE',  ( -49.25499999999999545, -4.716976649647092401, 6.492361379858946790 ) ) ;
#54688 =( BOUNDED_CURVE ( )  B_SPLINE_CURVE ( 2, ( #58263, #60256, #54279, #17382, #12058, #65885, #54955, #44810, #11374, #36849, #20982 ),
 .UNSPECIFIED., .F., .F. ) 
 B_SPLINE_CURVE_WITH_KNOTS ( ( 3, 2, 2, 2, 2, 3 ),
 ( 0.7608695652173913526, 0.7630434782608696009, 0.7652173913043478493, 0.7673913043478260976, 0.7695652173913043459, 0.7717391304347825942 ),
 .UNSPECIFIED. ) 
 CURVE ( )  GEOMETRIC_REPRESENTATION_ITEM ( )  RATIONAL_B_SPLINE_CURVE ( ( 1.000000000000000000, 0.9510565162951535312, 1.000000000000000000, 0.9510565162951535312, 1.000000000000000000, 0.9510565162951535312, 1.000000000000000000, 0.9510565162951535312, 1.000000000000000000, 0.9510565162951535312, 1.000000000000000000 ) ) 
 REPRESENTATION_ITEM ( '' )  );
#54689 = CARTESIAN_POINT ( 'NONE',  ( -58.64499999999998892, 4.716976649647091513, -6.492361379858946790 ) ) ;
#54690 = CIRCLE ( 'NONE', #708, 23.00000000000000355 ) ;
#54691 = DIRECTION ( 'NONE',  ( -0.4468085106382997385, 0.000000000000000000, 0.8946296187927071930 ) ) ;
#54692 =( LENGTH_UNIT ( ) NAMED_UNIT ( * ) SI_UNIT ( .MILLI., .METRE. ) );
#54693 = EDGE_CURVE ( 'NONE', #38966, #62390, #56425, .T. ) ;
#54694 = LINE ( 'NONE', #2205, #55218 ) ;
#54695 = CARTESIAN_POINT ( 'NONE',  ( -91.04292637653379927, -9.058813317711329915, -2.943386871421370898 ) ) ;
#54696 = APPLICATION_PROTOCOL_DEFINITION ( 'draft international standard', 'automotive_design', 1998, #52753 ) ;
#54697 = CARTESIAN_POINT ( 'NONE',  ( -51.46090993356868637, -11.68865663075333039, 1.590926122486572725 ) ) ;
#54698 = CARTESIAN_POINT ( 'NONE',  ( 60.00000000000000000, 1.797044900979284448E-15, 10.50000000000000000 ) ) ;
#54699 = DIRECTION ( 'NONE',  ( 1.000000000000000000, 3.469446951953611033E-15, 0.000000000000000000 ) ) ;
#54700 = DIRECTION ( 'NONE',  ( -1.000000000000000000, 0.000000000000000000, 0.000000000000000000 ) ) ;
#54701 = SURFACE_SIDE_STYLE ('',( #28998 ) ) ;
#54702 = EDGE_CURVE ( 'NONE', #47647, #60379, #35096, .T. ) ;
#54703 = ORIENTED_EDGE ( 'NONE', *, *, #19029, .F. ) ;
#54704 = DIRECTION ( 'NONE',  ( -1.000000000000000000, 0.000000000000000000, -0.000000000000000000 ) ) ;
#54705 = EDGE_LOOP ( 'NONE', ( #11273, #7587, #30595, #4521, #17643 ) ) ;
#54706 = FACE_OUTER_BOUND ( 'NONE', #4291, .T. ) ;
#54707 = CARTESIAN_POINT ( 'NONE',  ( -4.716976649647097730, 127.3570736234661496, -6.492361379858953896 ) ) ;
#54708 = CARTESIAN_POINT ( 'NONE',  ( 75.00000000000000000, 20.36037960999352237, -6.130923279862114939 ) ) ;
#54709 = MECHANICAL_DESIGN_GEOMETRIC_PRESENTATION_REPRESENTATION (  '', ( #3003 ), #53627 ) ;
#54710 = ORIENTED_EDGE ( 'NONE', *, *, #33793, .F. ) ;
#54711 = ORIENTED_EDGE ( 'NONE', *, *, #11599, .F. ) ;
#54712 = CARTESIAN_POINT ( 'NONE',  ( -117.0570736234661808, 0.000000000000000000, 9.524999999999991473 ) ) ;
#54713 = EDGE_CURVE ( 'NONE', #19997, #44738, #13755, .T. ) ;
#54714 = VERTEX_POINT ( 'NONE', #28595 ) ;
#54715 = CARTESIAN_POINT ( 'NONE',  ( 24.21231517720798010, 113.4999999999999858, -7.000000000000000000 ) ) ;
#54716 = TOROIDAL_SURFACE ( 'NONE', #63717, 1.000000000000000000, 0.5000000000000000000 ) ;
#54717 = DIRECTION ( 'NONE',  ( 0.000000000000000000, 0.000000000000000000, 1.000000000000000000 ) ) ;
#54718 = CARTESIAN_POINT ( 'NONE',  ( 6.826472737025121695, 134.4929263765338305, -4.959722759717905660 ) ) ;
#54719 = CARTESIAN_POINT ( 'NONE',  ( -89.39499999999996760, -6.826472737025115478, -4.959722759717899443 ) ) ;
#54720 = ORIENTED_EDGE ( 'NONE', *, *, #52300, .F. ) ;
#54721 = DIRECTION ( 'NONE',  ( -6.122553444624043322E-15, 0.8823529411764708952, -0.4705882352941173630 ) ) ;
#54722 = CARTESIAN_POINT ( 'NONE',  ( 1.000000000000000888, 0.000000000000000000, -79.00402776293826435 ) ) ;
#54723 =( LENGTH_UNIT ( ) NAMED_UNIT ( * ) SI_UNIT ( .MILLI., .METRE. ) );
#54724 = ORIENTED_EDGE ( 'NONE', *, *, #34379, .F. ) ;
#54725 = DIRECTION ( 'NONE',  ( 0.000000000000000000, -1.000000000000000000, 0.000000000000000000 ) ) ;
#54726 =( GEOMETRIC_REPRESENTATION_CONTEXT ( 3 ) GLOBAL_UNCERTAINTY_ASSIGNED_CONTEXT ( ( #4410 ) ) GLOBAL_UNIT_ASSIGNED_CONTEXT ( ( #44545, #43511, #59616 ) ) REPRESENTATION_CONTEXT ( 'NONE', 'WORKASPACE' ) );
#54727 = AXIS2_PLACEMENT_3D ( 'NONE', #55158, #6616, #17897 ) ;
#54728 = DIRECTION ( 'NONE',  ( -1.300977106640435137E-16, 0.000000000000000000, -1.000000000000000000 ) ) ;
#54729 = EDGE_LOOP ( 'NONE', ( #62507, #34511, #4285, #14006 ) ) ;
#54730 = CARTESIAN_POINT ( 'NONE',  ( -6.759171781091400710, 2.392512705203732715, -2.292771058063876488 ) ) ;
#54731 = VERTEX_POINT ( 'NONE', #1114 ) ;
#54732 = FACE_OUTER_BOUND ( 'NONE', #8882, .T. ) ;
#54733 = FILL_AREA_STYLE_COLOUR ( '', #18380 ) ;
#54734 = CARTESIAN_POINT ( 'NONE',  ( -30.38025804287907050, -8.500000000000000000, 7.999999999999983125 ) ) ;
#54735 = CARTESIAN_POINT ( 'NONE',  ( -176.0070736234661695, -8.102448949553172852, -5.886773742842741797 ) ) ;
#54736 = CARTESIAN_POINT ( 'NONE',  ( -45.89905495956738690, 9.405628579031729330, 3.000000000000000000 ) ) ;
#54737 = CARTESIAN_POINT ( 'NONE',  ( 4.041451884327379673, -7.000000000000002665, 7.500000000000000000 ) ) ;
#54738 = SURFACE_STYLE_USAGE ( .BOTH. , #32261 ) ;
#54739 = CARTESIAN_POINT ( 'NONE',  ( -115.9429263765338050, 0.000000000000000000, 9.524999999999991473 ) ) ;
#54740 = EDGE_LOOP ( 'NONE', ( #59664, #10230, #60375, #10483 ) ) ;
#54741 = CARTESIAN_POINT ( 'NONE',  ( -4.250000000000001776, 21.99999999999998579, -3.750000000000000000 ) ) ;
#54742 = DIRECTION ( 'NONE',  ( 0.3403530053317450621, -0.9351121967924954648, 0.09861547125863368013 ) ) ;
#54743 = CARTESIAN_POINT ( 'NONE',  ( -149.3070736234662093, -10.01517768586948698, 6.132527647946031529E-16 ) ) ;
#54744 = ORIENTED_EDGE ( 'NONE', *, *, #2994, .T. ) ;
#54745 = CARTESIAN_POINT ( 'NONE',  ( -155.4549999999999841, 7.632228543268599452, -2.479861379858951942 ) ) ;
#54746 = CARTESIAN_POINT ( 'NONE',  ( -7.500000000000000000, 4.592425496802573972E-16, 0.000000000000000000 ) ) ;
#54747 = CARTESIAN_POINT ( 'NONE',  ( -183.8867045463858574, -8.535045582951720888, -1.368092718024570109 ) ) ;
#54748 = CARTESIAN_POINT ( 'NONE',  ( -171.2949999999999875, -2.607480562269069768, 8.024999999999991473 ) ) ;
#54749 = CARTESIAN_POINT ( 'NONE',  ( -160.7949999999999591, 2.607480562269069324, -8.024999999999993250 ) ) ;
#54750 = VERTEX_POINT ( 'NONE', #28933 ) ;
#54751 = FACE_OUTER_BOUND ( 'NONE', #39456, .T. ) ;
#54752 = CARTESIAN_POINT ( 'NONE',  ( 44.82807636874886725, 9.942692122916287900, 2.999113325960788501 ) ) ;
#54753 = AXIS2_PLACEMENT_3D ( 'NONE', #46349, #18855, #14293 ) ;
#54754 =( NAMED_UNIT ( * ) PLANE_ANGLE_UNIT ( ) SI_UNIT ( $, .RADIAN. ) );
#54755 = CARTESIAN_POINT ( 'NONE',  ( -73.85499999999998977, 4.716976649647094177, 6.492361379858945902 ) ) ;
#54756 = FILL_AREA_STYLE_COLOUR ( '', #39409 ) ;
#54757 = CIRCLE ( 'NONE', #5357, 0.2500000000000002220 ) ;
#54758 = AXIS2_PLACEMENT_3D ( 'NONE', #26626, #43235, #195 ) ;
#54759 = CARTESIAN_POINT ( 'NONE',  ( -68.84499999999998465, -7.632228543268599452, 2.479861379858951054 ) ) ;
#54760 = CARTESIAN_POINT ( 'NONE',  ( -1.166476076187854022E-15, 136.0549999999999784, 9.525000000000000355 ) ) ;
#54761 = EDGE_CURVE ( 'NONE', #35924, #5028, #55343, .T. ) ;
#54762 = AXIS2_PLACEMENT_3D ( 'NONE', #1875, #44203, #27938 ) ;
#54763 = PRODUCT_DEFINITION_SHAPE ( 'NONE', 'NONE',  #69713 ) ;
#54764 =( NAMED_UNIT ( * ) PLANE_ANGLE_UNIT ( ) SI_UNIT ( $, .RADIAN. ) );
#54765 = ADVANCED_FACE ( 'NONE', ( #66239 ), #68806, .T. ) ;
#54766 = DIRECTION ( 'NONE',  ( 0.000000000000000000, 1.000000000000000000, 0.000000000000000000 ) ) ;
#54767 = VERTEX_POINT ( 'NONE', #54649 ) ;
#54768 = CIRCLE ( 'NONE', #63779, 1.000000000000000888 ) ;
#54769 = DIRECTION ( 'NONE',  ( 0.000000000000000000, 0.000000000000000000, 1.000000000000000000 ) ) ;
#54770 = PRESENTATION_LAYER_ASSIGNMENT (  '', '', ( #49194 ) ) ;
#54771 = ADVANCED_FACE ( 'NONE', ( #44157 ), #33545, .T. ) ;
#54772 = COLOUR_RGB ( '', 0.09019608, 0.27058824, 0.51372549) ;
#54773 = CARTESIAN_POINT ( 'NONE',  ( 7.999999999999998224, 0.000000000000000000, -37.00402776293825724 ) ) ;
#54774 = EDGE_CURVE ( 'NONE', #60684, #17419, #19443, .T. ) ;
#54775 = EDGE_CURVE ( 'NONE', #6066, #67943, #57438, .T. ) ;
#54776 = DIRECTION ( 'NONE',  ( -1.000000000000000000, -0.000000000000000000, -0.000000000000000000 ) ) ;
#54777 = DIRECTION ( 'NONE',  ( -0.000000000000000000, -0.000000000000000000, -1.000000000000000000 ) ) ;
#54778 = ORIENTED_EDGE ( 'NONE', *, *, #31682, .T. ) ;
#54779 = ORIENTED_EDGE ( 'NONE', *, *, #62499, .F. ) ;
#54780 = CARTESIAN_POINT ( 'NONE',  ( -48.50000000000000000, 14.49137674618942562, -7.000000000000000000 ) ) ;
#54781 = ADVANCED_FACE ( 'NONE', ( #40585 ), #30678, .F. ) ;
#54782 = EDGE_CURVE ( 'NONE', #42291, #3117, #39597, .T. ) ;
#54783 = DIRECTION ( 'NONE',  ( 0.000000000000000000, 0.000000000000000000, 1.000000000000000000 ) ) ;
#54784 = DIRECTION ( 'NONE',  ( 1.000000000000000000, 0.000000000000000000, -0.000000000000000000 ) ) ;
#54785 = CARTESIAN_POINT ( 'NONE',  ( -21.02379604162863913, 154.9999999999999716, -10.50000000000000000 ) ) ;
#54786 = CARTESIAN_POINT ( 'NONE',  ( -69.80707362346613820, 10.01517768586948698, -1.839758294383808966E-15 ) ) ;
#54787 = ORIENTED_EDGE ( 'NONE', *, *, #61840, .F. ) ;
#54788 = CARTESIAN_POINT ( 'NONE',  ( -108.6549999999999869, -7.632228543268600340, -2.479861379858950166 ) ) ;
#54789 = ORIENTED_EDGE ( 'NONE', *, *, #16575, .T. ) ;
#54790 = DIRECTION ( 'NONE',  ( -1.000000000000000000, -2.168404344971006896E-16, 0.000000000000000000 ) ) ;
#54791 =( NAMED_UNIT ( * ) PLANE_ANGLE_UNIT ( ) SI_UNIT ( $, .RADIAN. ) );
#54792 = ORIENTED_EDGE ( 'NONE', *, *, #16734, .T. ) ;
#54793 = SURFACE_STYLE_USAGE ( .BOTH. , #44657 ) ;
#54794 = LINE ( 'NONE', #39026, #54602 ) ;
#54795 = EDGE_LOOP ( 'NONE', ( #35635, #59158, #45716, #55150 ) ) ;
#54796 = CARTESIAN_POINT ( 'NONE',  ( 62.24999999999998579, 33.74999999999999289, -3.750000000000000000 ) ) ;
#54797 = CARTESIAN_POINT ( 'NONE',  ( -5.598654528085806881, 157.7450000000000045, -7.705886871421374629 ) ) ;
#54798 = ORIENTED_EDGE ( 'NONE', *, *, #9081, .T. ) ;
#54799 =( BOUNDED_CURVE ( )  B_SPLINE_CURVE ( 2, ( #42922, #63966, #16172, #15812, #41873, #37295, #10863, #3818, #46828, #47154, #68231 ),
 .UNSPECIFIED., .F., .F. ) 
 B_SPLINE_CURVE_WITH_KNOTS ( ( 3, 2, 2, 2, 2, 3 ),
 ( 0.3823529411764706176, 0.3882352941176471228, 0.3941176470588235725, 0.4000000000000001332, 0.4058823529411765829, 0.4117647058823530326 ),
 .UNSPECIFIED. ) 
 CURVE ( )  GEOMETRIC_REPRESENTATION_ITEM ( )  RATIONAL_B_SPLINE_CURVE ( ( 0.9999999999999995559, 0.9510565162951539753, 1.000000000000000000, 0.9510565162951535312, 1.000000000000000000, 0.9510565162951535312, 1.000000000000000000, 0.9510565162951535312, 1.000000000000000000, 0.9510565162951526430, 1.000000000000000888 ) ) 
 REPRESENTATION_ITEM ( '' )  );
#54800 = ORIENTED_EDGE ( 'NONE', *, *, #62642, .T. ) ;
#54801 = CARTESIAN_POINT ( 'NONE',  ( -74.14894111157977363, 9.184645374706621013, -6.276135203588958156 ) ) ;
#54802 = DIRECTION ( 'NONE',  ( -1.000000000000000000, 0.000000000000000000, 0.000000000000000000 ) ) ;
#54803 = LINE ( 'NONE', #6987, #31865 ) ;
#54804 = ORIENTED_EDGE ( 'NONE', *, *, #25453, .F. ) ;
#54805 = CARTESIAN_POINT ( 'NONE',  ( 6.826472737025121695, 131.4929263765337737, -4.959722759717905660 ) ) ;
#54806 = CARTESIAN_POINT ( 'NONE',  ( 4.750000000000002665, 24.74999999999998579, -3.750000000000000000 ) ) ;
#54807 = CARTESIAN_POINT ( 'NONE',  ( 31.00000000000002132, 42.00000000000000000, 79.00402776293823592 ) ) ;
#54808 = COLOUR_RGB ( '', 0.72549020, 0.75294118, 0.79215686) ;
#54809 = CARTESIAN_POINT ( 'NONE',  ( -104.6929263765337907, 10.01517768586948698, -1.839758294383808966E-15 ) ) ;
#54810 = DIRECTION ( 'NONE',  ( -0.000000000000000000, -0.000000000000000000, -1.000000000000000000 ) ) ;
#54811 = ORIENTED_EDGE ( 'NONE', *, *, #51076, .T. ) ;
#54812 = DIRECTION ( 'NONE',  ( -1.000000000000000000, 0.000000000000000000, 0.000000000000000000 ) ) ;
#54813 = EDGE_LOOP ( 'NONE', ( #27564, #27431, #10745, #7963 ) ) ;
#54814 = CARTESIAN_POINT ( 'NONE',  ( -49.34292637653378222, -9.058813317711329915, 2.943386871421371787 ) ) ;
#54815 = DIRECTION ( 'NONE',  ( -1.000000000000000000, 0.000000000000000000, 0.000000000000000000 ) ) ;
#54816 = SURFACE_STYLE_USAGE ( .BOTH. , #270 ) ;
#54817 =( GEOMETRIC_REPRESENTATION_CONTEXT ( 3 ) GLOBAL_UNCERTAINTY_ASSIGNED_CONTEXT ( ( #5954 ) ) GLOBAL_UNIT_ASSIGNED_CONTEXT ( ( #24085, #45909, #23732 ) ) REPRESENTATION_CONTEXT ( 'NONE', 'WORKASPACE' ) );
#54818 = CARTESIAN_POINT ( 'NONE',  ( -146.7549999999999955, 4.716976649647091513, -6.492361379858946790 ) ) ;
#54819 = CARTESIAN_POINT ( 'NONE',  ( -60.00000000000000000, -2.024042244987997205E-14, 6.999999999999999112 ) ) ;
#54820 =( NAMED_UNIT ( * ) SI_UNIT ( $, .STERADIAN. ) SOLID_ANGLE_UNIT ( ) );
#54821 = ORIENTED_EDGE ( 'NONE', *, *, #68314, .F. ) ;
#54822 = CARTESIAN_POINT ( 'NONE',  ( -106.7929263765347656, -3.094860106602296046, 9.525000000011715429 ) ) ;
#54823 = CARTESIAN_POINT ( 'NONE',  ( 45.00000000000000000, 99.99999999999992895, 9.500000000000000000 ) ) ;
#54824 = CARTESIAN_POINT ( 'NONE',  ( -45.00000000000000000, 9.680388875877742549, -6.198302543666470932 ) ) ;
#54825 = EDGE_LOOP ( 'NONE', ( #40132, #8445, #69303 ) ) ;
#54826 = COLOUR_RGB ( '', 0.09019608, 0.27058824, 0.51372549) ;
#54827 = ORIENTED_EDGE ( 'NONE', *, *, #14469, .F. ) ;
#54828 = CARTESIAN_POINT ( 'NONE',  ( -45.90207868045609985, 9.410163051192631301, 3.203717355333229655 ) ) ;
#54829 = CARTESIAN_POINT ( 'NONE',  ( -109.7929263765347656, -3.094860106602833394, 9.525000000011322854 ) ) ;
#54830 = CARTESIAN_POINT ( 'NONE',  ( -54.05499999999999261, -9.827790563157499189E-16, -8.024999999999991473 ) ) ;
#54831 = ORIENTED_EDGE ( 'NONE', *, *, #17429, .T. ) ;
#54832 = LINE ( 'NONE', #952, #56159 ) ;
#54833 = PRESENTATION_STYLE_ASSIGNMENT (( #38731 ) ) ;
#54834 = SURFACE_STYLE_USAGE ( .BOTH. , #12979 ) ;
#54835 = DIRECTION ( 'NONE',  ( -0.7071067811865447972, 8.659560562354899578E-17, 0.7071067811865502373 ) ) ;
#54836 = DIRECTION ( 'NONE',  ( -1.000000000000000000, -0.000000000000000000, -0.000000000000000000 ) ) ;
#54837 = CARTESIAN_POINT ( 'NONE',  ( -96.59292637653489066, -3.094860106636716512, -9.524999999986706101 ) ) ;
#54838 = ORIENTED_EDGE ( 'NONE', *, *, #9365, .F. ) ;
#54840 = VECTOR ( 'NONE', #58091, 1000.000000000000000 ) ;
#54839 = CARTESIAN_POINT ( 'NONE',  ( -145.2570736234661695, 5.598654528085800663, -7.705886871421367523 ) ) ;
#54841 = DIRECTION ( 'NONE',  ( 0.7071067811865425767, 8.659560562354873694E-17, -0.7071067811865525687 ) ) ;
#54842 = LINE ( 'NONE', #52561, #58417 ) ;
#54843 = DIRECTION ( 'NONE',  ( -0.000000000000000000, -0.000000000000000000, -1.000000000000000000 ) ) ;
#54844 = AXIS2_PLACEMENT_3D ( 'NONE', #60221, #22592, #61256 ) ;
#54845 = CARTESIAN_POINT ( 'NONE',  ( -109.7949999999999875, 2.607480562269069324, -8.024999999999993250 ) ) ;
#54846 = CARTESIAN_POINT ( 'NONE',  ( 5.598654528085809545, 154.1449999999999818, -7.705886871421373741 ) ) ;
#54847 = CARTESIAN_POINT ( 'NONE',  ( -73.79499999999997328, 2.607480562269068880, -8.024999999999993250 ) ) ;
#54848 = CARTESIAN_POINT ( 'NONE',  ( -6.826472737025120807, 112.5070736234661410, -4.959722759717907437 ) ) ;
#54849 = ADVANCED_FACE ( 'NONE', ( #24703 ), #34934, .F. ) ;
#54850 = VECTOR ( 'NONE', #69363, 1000.000000000000000 ) ;
#54851 = LINE ( 'NONE', #54523, #11272 ) ;
#54852 = FACE_OUTER_BOUND ( 'NONE', #41820, .T. ) ;
#54853 = AXIS2_PLACEMENT_3D ( 'NONE', #61060, #55447, #12519 ) ;
#54854 = EDGE_CURVE ( 'NONE', #60539, #21950, #10462, .T. ) ;
#54855 = CARTESIAN_POINT ( 'NONE',  ( -20.71231517720797655, 149.4999999999999716, -10.00000000000000000 ) ) ;
#54856 = CARTESIAN_POINT ( 'NONE',  ( 14.98999599679679662, 117.9999999999999716, -10.00000000000000000 ) ) ;
#54857 = ORIENTED_EDGE ( 'NONE', *, *, #3614, .T. ) ;
#54858 = CARTESIAN_POINT ( 'NONE',  ( -121.6429263765338078, -5.598654528085801552, 7.705886871421367523 ) ) ;
#54859 = CARTESIAN_POINT ( 'NONE',  ( -136.6449999999999818, 4.716976649647091513, -6.492361379858946790 ) ) ;
#54860 = SURFACE_STYLE_USAGE ( .BOTH. , #17946 ) ;
#54861 = STYLED_ITEM ( 'NONE', ( #15950 ), #50950 ) ;
#54862 = COLOUR_RGB ( '', 0.72549020, 0.75294118, 0.79215686) ;
#54863 = ADVANCED_FACE ( 'NONE', ( #24365 ), #19079, .T. ) ;
#54864 = CARTESIAN_POINT ( 'NONE',  ( -66.50707362346616947, 8.102448949553176405, 5.886773742842740909 ) ) ;
#54865 = ORIENTED_EDGE ( 'NONE', *, *, #49641, .T. ) ;
#54866 = AXIS2_PLACEMENT_3D ( 'NONE', #8670, #68813, #30099 ) ;
#54867 = ORIENTED_EDGE ( 'NONE', *, *, #49935, .F. ) ;
#54868 = DIRECTION ( 'NONE',  ( 1.000000000000000000, 0.000000000000000000, -0.000000000000000000 ) ) ;
#54869 = CARTESIAN_POINT ( 'NONE',  ( -79.99999999999998579, 50.00000000000000000, -11.50000000000001066 ) ) ;
#54870 = COLOUR_RGB ( '', 0.09019608, 0.27058824, 0.51372549) ;
#54871 = ADVANCED_FACE ( 'NONE', ( #14892 ), #36293, .T. ) ;
#54872 = CARTESIAN_POINT ( 'NONE',  ( 44.99999999999977973, 149.9999999999999716, -9.500000000000000000 ) ) ;
#54873 = DIRECTION ( 'NONE',  ( -0.000000000000000000, -0.000000000000000000, -1.000000000000000000 ) ) ;
#54874 = CIRCLE ( 'NONE', #884, 0.2500000000000002220 ) ;
#54875 = EDGE_LOOP ( 'NONE', ( #41910, #19411 ) ) ;
#54876 = CARTESIAN_POINT ( 'NONE',  ( -141.9549999999999841, -7.632228543268599452, 2.479861379858951054 ) ) ;
#54877 = ORIENTED_EDGE ( 'NONE', *, *, #60264, .T. ) ;
#54878 = ORIENTED_EDGE ( 'NONE', *, *, #6756, .T. ) ;
#54879 = CARTESIAN_POINT ( 'NONE',  ( 1.000000000000000000, 0.9999999999999991118, -79.00402776293826435 ) ) ;
#54880 = LINE ( 'NONE', #60859, #65808 ) ;
#54881 = ORIENTED_EDGE ( 'NONE', *, *, #10877, .F. ) ;
#54882 = CARTESIAN_POINT ( 'NONE',  ( -195.0000000000000000, 1.166476076187852838E-15, -9.524999999999991473 ) ) ;
#54883 = CARTESIAN_POINT ( 'NONE',  ( 9.058813317711338797, 132.8449999999999989, -2.943386871421372675 ) ) ;
#54884 = ORIENTED_EDGE ( 'NONE', *, *, #32096, .F. ) ;
#54885 = CARTESIAN_POINT ( 'NONE',  ( -61.49999999999998579, 50.00000000000000000, -10.00000000000000000 ) ) ;
#54886 = CARTESIAN_POINT ( 'NONE',  ( -10.01517768586949408, 135.3049999999999784, -6.132527647946036459E-16 ) ) ;
#54887 = CARTESIAN_POINT ( 'NONE',  ( -51.65499999999997982, -7.632228543268600340, -2.479861379858950166 ) ) ;
#54888 = CARTESIAN_POINT ( 'NONE',  ( 15.00000000000000000, 8.000000000000000000, 3.500000000000003997 ) ) ;
#54889 = ORIENTED_EDGE ( 'NONE', *, *, #57091, .F. ) ;
#54890 = CARTESIAN_POINT ( 'NONE',  ( 3.094860106618431583, 160.2050000000000125, 9.525000000000000355 ) ) ;
#54891 = CARTESIAN_POINT ( 'NONE',  ( 60.00000000000000000, 1.797044900979284448E-15, -7.000000000000000888 ) ) ;
#54892 = FILL_AREA_STYLE_COLOUR ( '', #34402 ) ;
#54893 = VECTOR ( 'NONE', #66006, 1000.000000000000000 ) ;
#54894 = ORIENTED_EDGE ( 'NONE', *, *, #41680, .T. ) ;
#54895 = STYLED_ITEM ( 'NONE', ( #33664 ), #20075 ) ;
#54896 = FILL_AREA_STYLE ('',( #43721 ) ) ;
#54897 = ORIENTED_EDGE ( 'NONE', *, *, #54238, .T. ) ;
#54898 = AXIS2_PLACEMENT_3D ( 'NONE', #60763, #17880, #17558 ) ;
#54899 = DIRECTION ( 'NONE',  ( -0.000000000000000000, -0.000000000000000000, 1.000000000000000000 ) ) ;
#54900 = LINE ( 'NONE', #28523, #45265 ) ;
#54901 = CARTESIAN_POINT ( 'NONE',  ( -170.7549999999999955, 4.716976649647091513, -6.492361379858946790 ) ) ;
#54902 = VERTEX_POINT ( 'NONE', #35290 ) ;
#54903 =( NAMED_UNIT ( * ) PLANE_ANGLE_UNIT ( ) SI_UNIT ( $, .RADIAN. ) );
#54904 =( GEOMETRIC_REPRESENTATION_CONTEXT ( 3 ) GLOBAL_UNCERTAINTY_ASSIGNED_CONTEXT ( ( #3667 ) ) GLOBAL_UNIT_ASSIGNED_CONTEXT ( ( #15354, #14996, #41381 ) ) REPRESENTATION_CONTEXT ( 'NONE', 'WORKASPACE' ) );
#54905 = EDGE_CURVE ( 'NONE', #50331, #30753, #8184, .T. ) ;
#54906 = CARTESIAN_POINT ( 'NONE',  ( -24.21231517720798010, 113.4999999999999858, 9.500000000000000000 ) ) ;
#54907 = CARTESIAN_POINT ( 'NONE',  ( -183.9999999999999716, -7.591759853317446627, 2.884858859289065602 ) ) ;
#54908 = CARTESIAN_POINT ( 'NONE',  ( -44.99999999999999289, 9.678668534234134313, 3.511107231047464694 ) ) ;
#54909 = VERTEX_POINT ( 'NONE', #32090 ) ;
#54910 = VECTOR ( 'NONE', #49030, 1000.000000000000000 ) ;
#54911 = CARTESIAN_POINT ( 'NONE',  ( -45.15332280914032737, 8.289991779376686409, -3.464680026297982440 ) ) ;
#54912 = CARTESIAN_POINT ( 'NONE',  ( -7.794228634059948035, 2.500000000000000000, 4.499999999999999112 ) ) ;
#54913 = CARTESIAN_POINT ( 'NONE',  ( -87.80500000000000682, -8.437984349512085203, 5.166775262442717831E-16 ) ) ;
#54914 = EDGE_LOOP ( 'NONE', ( #8487, #66385, #10536, #66692 ) ) ;
#54915 =( NAMED_UNIT ( * ) PLANE_ANGLE_UNIT ( ) SI_UNIT ( $, .RADIAN. ) );
#54916 = MECHANICAL_DESIGN_GEOMETRIC_PRESENTATION_REPRESENTATION (  '', ( #51578 ), #21230 ) ;
#54917 =( NAMED_UNIT ( * ) SI_UNIT ( $, .STERADIAN. ) SOLID_ANGLE_UNIT ( ) );
#54918 = CARTESIAN_POINT ( 'NONE',  ( -52.40707362346616804, 3.094860106618428031, -9.524999999999993250 ) ) ;
#54919 = VECTOR ( 'NONE', #24232, 1000.000000000000000 ) ;
#54920 = CARTESIAN_POINT ( 'NONE',  ( -74.99999999999998579, 8.340816515359708916, -6.279506003889757437 ) ) ;
#54921 = ORIENTED_EDGE ( 'NONE', *, *, #53071, .F. ) ;
#54922 = CARTESIAN_POINT ( 'NONE',  ( 22.00000000000002132, 43.00000000000000000, 45.61250543006183733 ) ) ;
#54923 = VECTOR ( 'NONE', #67851, 1000.000000000000000 ) ;
#54925 = SURFACE_SIDE_STYLE ('',( #44108 ) ) ;
#54924 = DIRECTION ( 'NONE',  ( 0.000000000000000000, 1.000000000000000000, 0.000000000000000000 ) ) ;
#54926 = EDGE_CURVE ( 'NONE', #25430, #26545, #64447, .T. ) ;
#54927 = EDGE_CURVE ( 'NONE', #47340, #69646, #54211, .T. ) ;
#54928 = CARTESIAN_POINT ( 'NONE',  ( -8.102448949553181734, 125.4949999999999903, 5.886773742842747126 ) ) ;
#54929 = CARTESIAN_POINT ( 'NONE',  ( -104.9949999999999761, -6.826472737025115478, 4.959722759717900331 ) ) ;
#54930 = CARTESIAN_POINT ( 'NONE',  ( 8.000000000000030198, 5.000000000000000000, -29.00402776293826079 ) ) ;
#54932 = CARTESIAN_POINT ( 'NONE',  ( -15.32933058623710565, 10.90871211463570845, -4.999999999999999112 ) ) ;
#54931 = SURFACE_SIDE_STYLE ('',( #47677 ) ) ;
#54933 = EDGE_CURVE ( 'NONE', #57325, #31700, #59148, .T. ) ;
#54934 = AXIS2_PLACEMENT_3D ( 'NONE', #1067, #38131, #5363 ) ;
#54935 = CARTESIAN_POINT ( 'NONE',  ( -148.6429263765338078, -5.598654528085801552, 7.705886871421367523 ) ) ;
#54936 = CARTESIAN_POINT ( 'NONE',  ( -175.4949999999999761, 6.826472737025113702, -4.959722759717902107 ) ) ;
#54937 = AXIS2_PLACEMENT_3D ( 'NONE', #784, #64191, #32894 ) ;
#54938 =( NAMED_UNIT ( * ) SI_UNIT ( $, .STERADIAN. ) SOLID_ANGLE_UNIT ( ) );
#54939 = VECTOR ( 'NONE', #58590, 1000.000000000000000 ) ;
#54940 = ADVANCED_FACE ( 'NONE', ( #32413 ), #694, .T. ) ;
#54941 = CIRCLE ( 'NONE', #58335, 0.5000000000000004441 ) ;
#54942 = CARTESIAN_POINT ( 'NONE',  ( -43.33682035272221356, -12.17003437142647648, 3.180123757613341873 ) ) ;
#54943 = ORIENTED_EDGE ( 'NONE', *, *, #50924, .F. ) ;
#54944 = CARTESIAN_POINT ( 'NONE',  ( -45.50000000000000000, -2.024042244987997205E-14, 6.999999999999999112 ) ) ;
#54945 = ORIENTED_EDGE ( 'NONE', *, *, #32640, .F. ) ;
#54946 = CARTESIAN_POINT ( 'NONE',  ( -65.54292637653379927, 9.058813317711329915, 2.943386871421369566 ) ) ;
#54947 = AXIS2_PLACEMENT_3D ( 'NONE', #42409, #64504, #49056 ) ;
#54948 = CARTESIAN_POINT ( 'NONE',  ( 0.000000000000000000, 0.000000000000000000, 0.000000000000000000 ) ) ;
#54949 = CARTESIAN_POINT ( 'NONE',  ( 24.21231517720798010, 113.4999999999999858, 7.000000000000000000 ) ) ;
#54950 = CIRCLE ( 'NONE', #5390, 9.000000000000000000 ) ;
#54951 = ADVANCED_FACE ( 'NONE', ( #48302 ), #11318, .F. ) ;
#54952 = CARTESIAN_POINT ( 'NONE',  ( 6.826472737025121695, 147.6070736234661354, -4.959722759717905660 ) ) ;
#54953 = DIRECTION ( 'NONE',  ( 0.000000000000000000, 0.000000000000000000, -1.000000000000000000 ) ) ;
#54954 = VECTOR ( 'NONE', #15897, 1000.000000000000000 ) ;
#54955 = CARTESIAN_POINT ( 'NONE',  ( -79.04292637653379927, -9.058813317711329915, -2.943386871421370898 ) ) ;
#54956 = VERTEX_POINT ( 'NONE', #15941 ) ;
#54957 = CARTESIAN_POINT ( 'NONE',  ( -167.6050000000000182, 6.826472737025113702, -4.959722759717902107 ) ) ;
#54958 = ORIENTED_EDGE ( 'NONE', *, *, #44296, .T. ) ;
#54959 = DIRECTION ( 'NONE',  ( 0.000000000000000000, 0.000000000000000000, -1.000000000000000000 ) ) ;
#54960 = DIRECTION ( 'NONE',  ( 0.000000000000000000, 1.000000000000000000, -0.000000000000000000 ) ) ;
#54961 = PLANE ( 'NONE',  #22887 ) ;
#54962 = PRESENTATION_STYLE_ASSIGNMENT (( #53936 ) ) ;
#54963 = STYLED_ITEM ( 'NONE', ( #13147 ), #14875 ) ;
#54964 = CARTESIAN_POINT ( 'NONE',  ( 7.632228543268608334, 153.4570736234661581, -2.479861379858951942 ) ) ;
#54965 = APPLICATION_CONTEXT ( 'automotive_design' ) ;
#54966 = ORIENTED_EDGE ( 'NONE', *, *, #10624, .T. ) ;
#54967 = PRESENTATION_STYLE_ASSIGNMENT (( #43789 ) ) ;
#54968 = CARTESIAN_POINT ( 'NONE',  ( -81.05499999999999261, -9.827790563157499189E-16, -8.024999999999991473 ) ) ;
#54969 = AXIS2_PLACEMENT_3D ( 'NONE', #25448, #34606, #66641 ) ;
#54970 = CARTESIAN_POINT ( 'NONE',  ( 7.632228543268607446, 132.1570736234661467, 2.479861379858954606 ) ) ;
#54971 = LINE ( 'NONE', #39201, #30991 ) ;
#54972 = CARTESIAN_POINT ( 'NONE',  ( -126.4429263765338192, -1.166476076187852838E-15, -9.524999999999991473 ) ) ;
#54973 = DIRECTION ( 'NONE',  ( 0.000000000000000000, 0.000000000000000000, 1.000000000000000000 ) ) ;
#54974 = CARTESIAN_POINT ( 'NONE',  ( 31.00000000000001066, 42.00000000000000000, -4.033029030585349936E-15 ) ) ;
#54975 = VERTEX_POINT ( 'NONE', #27478 ) ;
#54976 =( LENGTH_UNIT ( ) NAMED_UNIT ( * ) SI_UNIT ( .MILLI., .METRE. ) );
#54977 = DIRECTION ( 'NONE',  ( -0.000000000000000000, -1.000000000000000000, -0.000000000000000000 ) ) ;
#54978 = CIRCLE ( 'NONE', #21300, 16.00000000000000000 ) ;
#54980 = CARTESIAN_POINT ( 'NONE',  ( -61.49499999999998323, 6.826472737025113702, -4.959722759717902107 ) ) ;
#54979 = AXIS2_PLACEMENT_3D ( 'NONE', #15349, #10726, #25850 ) ;
#54981 = VERTEX_POINT ( 'NONE', #37423 ) ;
#54982 = FACE_OUTER_BOUND ( 'NONE', #28430, .T. ) ;
#54983 = ADVANCED_FACE ( 'NONE', ( #58822 ), #26101, .F. ) ;
#54984 = CARTESIAN_POINT ( 'NONE',  ( 0.000000000000000000, 0.9999999999999991118, 79.00402776293826435 ) ) ;
#54985 = CARTESIAN_POINT ( 'NONE',  ( -45.70728519569756543, 8.623151806617487480, -6.441684343570499571 ) ) ;
#54986 = CIRCLE ( 'NONE', #3290, 0.5000000000000004441 ) ;
#54987 = ORIENTED_EDGE ( 'NONE', *, *, #9401, .F. ) ;
#54988 = CARTESIAN_POINT ( 'NONE',  ( -1.113559396844004956, 154.5000000000000000, -9.459683423334018570 ) ) ;
#54989 = DIRECTION ( 'NONE',  ( 1.000000000000000000, 2.312964634635707951E-15, 0.000000000000000000 ) ) ;
#54990 = VERTEX_POINT ( 'NONE', #31728 ) ;
#54991 = VECTOR ( 'NONE', #53568, 1000.000000000000000 ) ;
#54992 = DIRECTION ( 'NONE',  ( -0.000000000000000000, -1.000000000000000000, 0.000000000000000000 ) ) ;
#54993 = CARTESIAN_POINT ( 'NONE',  ( -110.6049999999999898, 6.826472737025113702, -4.959722759717902107 ) ) ;
#54994 = ORIENTED_EDGE ( 'NONE', *, *, #13090, .T. ) ;
#54995 = CARTESIAN_POINT ( 'NONE',  ( 0.000000000000000000, 36.99999999999999289, 4.000000000000000000 ) ) ;
#54996 = STYLED_ITEM ( 'NONE', ( #3445 ), #20903 ) ;
#54997 = FACE_OUTER_BOUND ( 'NONE', #61327, .T. ) ;
#54998 = CARTESIAN_POINT ( 'NONE',  ( 23.21231517720797655, 118.4999999999999716, 7.000000000000000000 ) ) ;
#54999 = CARTESIAN_POINT ( 'NONE',  ( -154.5570736234661808, -1.166476076187852838E-15, -9.524999999999991473 ) ) ;
#55000 = CIRCLE ( 'NONE', #11239, 0.2500000000000002220 ) ;
#55001 = CARTESIAN_POINT ( 'NONE',  ( 39.49999999999999289, 16.24999999999997513, 4.000000000000000000 ) ) ;
#55002 = CARTESIAN_POINT ( 'NONE',  ( -3.094860106618432471, 130.5949999999999989, -9.525000000000000355 ) ) ;
#55003 = CARTESIAN_POINT ( 'NONE',  ( -83.15707362346617515, -9.058813317711329915, -2.943386871421370898 ) ) ;
#55004 = EDGE_CURVE ( 'NONE', #36954, #41190, #47559, .T. ) ;
#55005 =( GEOMETRIC_REPRESENTATION_CONTEXT ( 3 ) GLOBAL_UNCERTAINTY_ASSIGNED_CONTEXT ( ( #15843 ) ) GLOBAL_UNIT_ASSIGNED_CONTEXT ( ( #14527, #2890, #57807 ) ) REPRESENTATION_CONTEXT ( 'NONE', 'WORKASPACE' ) );
#55006 = CARTESIAN_POINT ( 'NONE',  ( -53.76864595461378826, -9.688118915545649301, -3.017821087588400619 ) ) ;
#55007 = ORIENTED_EDGE ( 'NONE', *, *, #3034, .F. ) ;
#55008 = AXIS2_PLACEMENT_3D ( 'NONE', #33681, #60402, #65695 ) ;
#55009 = DIRECTION ( 'NONE',  ( 0.000000000000000000, 0.000000000000000000, 1.000000000000000000 ) ) ;
#55011 =( NAMED_UNIT ( * ) SI_UNIT ( $, .STERADIAN. ) SOLID_ANGLE_UNIT ( ) );
#55010 = SURFACE_STYLE_FILL_AREA ( #21634 ) ;
#55012 = EDGE_CURVE ( 'NONE', #64235, #26176, #18273, .T. ) ;
#55013 = CARTESIAN_POINT ( 'NONE',  ( -128.0049999999999670, 6.826472737025116366, 4.959722759717898555 ) ) ;
#55014 =( NAMED_UNIT ( * ) SI_UNIT ( $, .STERADIAN. ) SOLID_ANGLE_UNIT ( ) );
#55015 = EDGE_CURVE ( 'NONE', #53321, #68848, #7762, .T. ) ;
#55016 = DIRECTION ( 'NONE',  ( 0.000000000000000000, 0.000000000000000000, 1.000000000000000000 ) ) ;
#55017 = CARTESIAN_POINT ( 'NONE',  ( 48.50000000000000000, 14.49137674618942206, -7.000000000000000000 ) ) ;
#55018 = CARTESIAN_POINT ( 'NONE',  ( -141.8950000000000102, 6.826472737025116366, 4.959722759717898555 ) ) ;
#55019 = VECTOR ( 'NONE', #45493, 1000.000000000000000 ) ;
#55020 = CARTESIAN_POINT ( 'NONE',  ( -124.3449999999999847, 7.632228543268599452, -2.479861379858951942 ) ) ;
#55021 = VERTEX_POINT ( 'NONE', #6382 ) ;
#55022 = DIRECTION ( 'NONE',  ( -0.9396926207859093161, -0.3420201433256664370, 0.000000000000000000 ) ) ;
#55023 = CARTESIAN_POINT ( 'NONE',  ( 44.45130529142733877, 9.817101763808881998, -3.473322258837261867 ) ) ;
#55024 =( GEOMETRIC_REPRESENTATION_CONTEXT ( 3 ) GLOBAL_UNCERTAINTY_ASSIGNED_CONTEXT ( ( #31859 ) ) GLOBAL_UNIT_ASSIGNED_CONTEXT ( ( #19404, #25034, #39871 ) ) REPRESENTATION_CONTEXT ( 'NONE', 'WORKASPACE' ) );
#55025 =( LENGTH_UNIT ( ) NAMED_UNIT ( * ) SI_UNIT ( .MILLI., .METRE. ) );
#55026 = EDGE_CURVE ( 'NONE', #13223, #32655, #49315, .T. ) ;
#55027 = LINE ( 'NONE', #6853, #19291 ) ;
#55028 = UNCERTAINTY_MEASURE_WITH_UNIT (LENGTH_MEASURE( 1.000000000000000082E-05 ), #32320, 'distance_accuracy_value', 'NONE');
#55029 = CARTESIAN_POINT ( 'NONE',  ( -181.1929263765337907, -10.01517768586948698, 6.132527647946031529E-16 ) ) ;
#55030 = AXIS2_PLACEMENT_3D ( 'NONE', #12638, #35146, #1340 ) ;
#55031 = CARTESIAN_POINT ( 'NONE',  ( -56.09499999999997044, -2.607480562269071545, -8.024999999999991473 ) ) ;
#55032 = EDGE_CURVE ( 'NONE', #40785, #43530, #50348, .T. ) ;
#55033 = DIRECTION ( 'NONE',  ( 0.000000000000000000, 0.000000000000000000, 1.000000000000000000 ) ) ;
#55034 = CARTESIAN_POINT ( 'NONE',  ( -102.2070736234672097, 3.094860106635239028, 9.524999999987784349 ) ) ;
#55035 = DIRECTION ( 'NONE',  ( 0.4999999999999998890, 0.000000000000000000, -0.8660254037844387076 ) ) ;
#55036 = DIRECTION ( 'NONE',  ( -0.000000000000000000, -0.000000000000000000, 1.000000000000000000 ) ) ;
#55037 = CARTESIAN_POINT ( 'NONE',  ( -8.082903768654762899, 3.516382302766490365E-15, 7.500000000000000000 ) ) ;
#55038 =( GEOMETRIC_REPRESENTATION_CONTEXT ( 3 ) GLOBAL_UNCERTAINTY_ASSIGNED_CONTEXT ( ( #18641 ) ) GLOBAL_UNIT_ASSIGNED_CONTEXT ( ( #2813, #19009, #35218 ) ) REPRESENTATION_CONTEXT ( 'NONE', 'WORKASPACE' ) );
#55039 = PRODUCT_DEFINITION_CONTEXT ( 'detailed design', #54965, 'design' ) ;
#55040 = CARTESIAN_POINT ( 'NONE',  ( -91.64292637653380780, -5.598654528085801552, 7.705886871421367523 ) ) ;
#55041 = PRODUCT_CONTEXT ( 'NONE', #33423, 'mechanical' ) ;
#55042 = CYLINDRICAL_SURFACE ( 'NONE', #5628, 4.999999999999999112 ) ;
#55043 = PRESENTATION_STYLE_ASSIGNMENT (( #43524 ) ) ;
#55044 = AXIS2_PLACEMENT_3D ( 'NONE', #19306, #8074, #9126 ) ;
#55045 =( NAMED_UNIT ( * ) PLANE_ANGLE_UNIT ( ) SI_UNIT ( $, .RADIAN. ) );
#55046 = DIRECTION ( 'NONE',  ( -1.000000000000000000, -0.000000000000000000, -0.000000000000000000 ) ) ;
#55047 = EDGE_CURVE ( 'NONE', #31646, #63887, #27224, .T. ) ;
#55048 = ORIENTED_EDGE ( 'NONE', *, *, #23920, .F. ) ;
#55049 = COLOUR_RGB ( '', 0.40784314, 0.44705882, 0.49803922) ;
#55050 = CARTESIAN_POINT ( 'NONE',  ( 57.24999999999999289, 28.24999999999998934, 4.000000000000000000 ) ) ;
#55051 = CIRCLE ( 'NONE', #52836, 0.2500000000000002220 ) ;
#55052 = VERTEX_POINT ( 'NONE', #65833 ) ;
#55053 = SURFACE_STYLE_USAGE ( .BOTH. , #33277 ) ;
#55054 = ADVANCED_FACE ( 'NONE', ( #28149 ), #41919, .T. ) ;
#55055 = STYLED_ITEM ( 'NONE', ( #43951 ), #34609 ) ;
#55056 = CARTESIAN_POINT ( 'NONE',  ( -2.607480562269075097, 119.4070736234661467, 8.025000000000000355 ) ) ;
#55057 = COLOUR_RGB ( '', 0.08235294, 0.09019608, 0.10196078) ;
#55058 = CARTESIAN_POINT ( 'NONE',  ( 75.00000000000000000, 19.95407619327929183, -6.799666827783447332 ) ) ;
#55059 = CIRCLE ( 'NONE', #30294, 0.5000000000000004441 ) ;
#55060 = ORIENTED_EDGE ( 'NONE', *, *, #1626, .F. ) ;
#55061 = FACE_OUTER_BOUND ( 'NONE', #38635, .T. ) ;
#55062 = ORIENTED_EDGE ( 'NONE', *, *, #31773, .F. ) ;
#55063 = CARTESIAN_POINT ( 'NONE',  ( 0.000000000000000000, 0.000000000000000000, 0.000000000000000000 ) ) ;
#55064 = VECTOR ( 'NONE', #46823, 1000.000000000000000 ) ;
#55065 = AXIS2_PLACEMENT_3D ( 'NONE', #60149, #7384, #61183 ) ;
#55066 = CARTESIAN_POINT ( 'NONE',  ( 34.99999999999999289, 99.99999999999997158, -10.00000000000000000 ) ) ;
#55067 = CARTESIAN_POINT ( 'NONE',  ( -88.64499999999998181, 4.716976649647091513, -6.492361379858946790 ) ) ;
#55068 = EDGE_LOOP ( 'NONE', ( #7063, #38805 ) ) ;
#55069 = CIRCLE ( 'NONE', #68617, 0.2500000000000002220 ) ;
#55070 = AXIS2_PLACEMENT_3D ( 'NONE', #32545, #54357, #132 ) ;
#55071 = CARTESIAN_POINT ( 'NONE',  ( -8.437984349512095861, 123.6929263765338192, -5.166775262442723748E-16 ) ) ;
#55072 =( NAMED_UNIT ( * ) PLANE_ANGLE_UNIT ( ) SI_UNIT ( $, .RADIAN. ) );
#55073 = VERTEX_POINT ( 'NONE', #27811 ) ;
#55074 = DIRECTION ( 'NONE',  ( 1.000000000000000000, -1.596582957076308193E-15, 0.000000000000000000 ) ) ;
#55075 = PRESENTATION_STYLE_ASSIGNMENT (( #38271 ) ) ;
#55076 = LINE ( 'NONE', #23773, #48058 ) ;
#55077 = ORIENTED_EDGE ( 'NONE', *, *, #3711, .F. ) ;
#55078 = ADVANCED_FACE ( 'NONE', ( #38458 ), #44433, .F. ) ;
#55079 = FACE_OUTER_BOUND ( 'NONE', #13946, .T. ) ;
#55080 = ORIENTED_EDGE ( 'NONE', *, *, #1527, .F. ) ;
#55081 = CARTESIAN_POINT ( 'NONE',  ( 26.00000000000001066, 21.74999999999998224, 3.750000000000000000 ) ) ;
#55082 = CARTESIAN_POINT ( 'NONE',  ( 60.00000000000000000, 1.797044900979284448E-15, -6.500000000000000000 ) ) ;
#55083 = CARTESIAN_POINT ( 'NONE',  ( -180.6570736234661751, 9.058813317711329915, 2.943386871421369566 ) ) ;
#55084 = VECTOR ( 'NONE', #48142, 1000.000000000000000 ) ;
#55085 = DIRECTION ( 'NONE',  ( 0.000000000000000000, 0.000000000000000000, -1.000000000000000000 ) ) ;
#55086 = STYLED_ITEM ( 'NONE', ( #13033 ), #45407 ) ;
#55087 = ADVANCED_FACE ( 'NONE', ( #23602 ), #17331, .F. ) ;
#55088 = CARTESIAN_POINT ( 'NONE',  ( -0.2274700367024033443, 9.000000000000008882, 3.467894058216981173E-15 ) ) ;
#55089 = VECTOR ( 'NONE', #15535, 1000.000000000000000 ) ;
#55090 = LINE ( 'NONE', #1919, #20060 ) ;
#55091 = ORIENTED_EDGE ( 'NONE', *, *, #26440, .T. ) ;
#55092 =( BOUNDED_CURVE ( )  B_SPLINE_CURVE ( 2, ( #64631, #42879, #55722, #28622, #40606, #29682, #62021, #7528, #67664, #66264, #61332 ),
 .UNSPECIFIED., .F., .F. ) 
 B_SPLINE_CURVE_WITH_KNOTS ( ( 3, 2, 2, 2, 2, 3 ),
 ( 0.8913043478260869179, 0.8934782608695651662, 0.8956521739130435256, 0.8978260869565217739, 0.9000000000000000222, 0.9021739130434782705 ),
 .UNSPECIFIED. ) 
 CURVE ( )  GEOMETRIC_REPRESENTATION_ITEM ( )  RATIONAL_B_SPLINE_CURVE ( ( 1.000000000000000000, 0.9510565162951535312, 1.000000000000000000, 0.9510565162951535312, 1.000000000000000000, 0.9510565162951535312, 1.000000000000000000, 0.9510565162951535312, 1.000000000000000000, 0.9510565162951535312, 1.000000000000000000 ) ) 
 REPRESENTATION_ITEM ( '' )  );
#55093 = CARTESIAN_POINT ( 'NONE',  ( 7.794228634059946259, -2.500000000000000000, -4.500000000000001776 ) ) ;
#55094 = FILL_AREA_STYLE ('',( #13225 ) ) ;
#55095 = CARTESIAN_POINT ( 'NONE',  ( -148.7070736234666697, -3.094860106625556995, -9.524999999994815170 ) ) ;
#55096 = DIRECTION ( 'NONE',  ( -0.000000000000000000, -1.000000000000000000, -0.000000000000000000 ) ) ;
#55097 = ORIENTED_EDGE ( 'NONE', *, *, #18202, .T. ) ;
#55098 = EDGE_CURVE ( 'NONE', #15891, #10808, #51741, .T. ) ;
#55099 = CARTESIAN_POINT ( 'NONE',  ( -162.6550000000000011, -7.632228543268600340, -2.479861379858950166 ) ) ;
#55100 = DIRECTION ( 'NONE',  ( 0.000000000000000000, 0.000000000000000000, 1.000000000000000000 ) ) ;
#55101 = CARTESIAN_POINT ( 'NONE',  ( -183.5232763065959602, -3.916627572773804022, -8.111163545727393398 ) ) ;
#55102 = AXIS2_PLACEMENT_3D ( 'NONE', #69434, #42408, #11372 ) ;
#55103 = CARTESIAN_POINT ( 'NONE',  ( -177.7449999999999761, 4.716976649647094177, 6.492361379858945902 ) ) ;
#55104 = CARTESIAN_POINT ( 'NONE',  ( -157.0449999999999875, 7.632228543268600340, 2.479861379858949277 ) ) ;
#55105 =( GEOMETRIC_REPRESENTATION_CONTEXT ( 3 ) GLOBAL_UNCERTAINTY_ASSIGNED_CONTEXT ( ( #33467 ) ) GLOBAL_UNIT_ASSIGNED_CONTEXT ( ( #55590, #46375, #17962 ) ) REPRESENTATION_CONTEXT ( 'NONE', 'WORKASPACE' ) );
#55106 = EDGE_LOOP ( 'NONE', ( #36086, #10539, #47741, #26768 ) ) ;
#55107 =( GEOMETRIC_REPRESENTATION_CONTEXT ( 3 ) GLOBAL_UNCERTAINTY_ASSIGNED_CONTEXT ( ( #52490 ) ) GLOBAL_UNIT_ASSIGNED_CONTEXT ( ( #61780, #35072, #46730 ) ) REPRESENTATION_CONTEXT ( 'NONE', 'WORKASPACE' ) );
#55108 = CARTESIAN_POINT ( 'NONE',  ( -2.607480562269116842, 151.2929263765338135, 8.024999999999970157 ) ) ;
#55109 = CARTESIAN_POINT ( 'NONE',  ( -68.75499999999998124, 4.716976649647091513, -6.492361379858946790 ) ) ;
#55110 = CARTESIAN_POINT ( 'NONE',  ( -37.47117118679384618, -12.53100696609209308, 2.887820269590780420 ) ) ;
#55111 = CONICAL_SURFACE ( 'NONE', #31513, 9.000000000000000000, 0.7853981633974500554 ) ;
#55112 = EDGE_CURVE ( 'NONE', #61213, #52614, #3487, .T. ) ;
#55113 = CARTESIAN_POINT ( 'NONE',  ( -72.74499999999999034, 4.716976649647094177, 6.492361379858945902 ) ) ;
#55114 = CARTESIAN_POINT ( 'NONE',  ( 9.058813317711338797, 145.9550000000000125, -2.943386871421372675 ) ) ;
#55115 = FACE_OUTER_BOUND ( 'NONE', #45519, .T. ) ;
#55116 = CIRCLE ( 'NONE', #16949, 0.5000000000000000000 ) ;
#55117 = CARTESIAN_POINT ( 'NONE',  ( -176.5429263765338135, 9.058813317711329915, 2.943386871421369566 ) ) ;
#55118 = UNCERTAINTY_MEASURE_WITH_UNIT (LENGTH_MEASURE( 1.000000000000000082E-05 ), #28558, 'distance_accuracy_value', 'NONE');
#55119 = AXIS2_PLACEMENT_3D ( 'NONE', #54698, #49795, #5813 ) ;
#55120 = DIRECTION ( 'NONE',  ( -1.000000000000000000, 0.000000000000000000, 1.300977106640434644E-16 ) ) ;
#55121 = DIRECTION ( 'NONE',  ( 0.000000000000000000, 1.000000000000000000, 0.000000000000000000 ) ) ;
#55122 = VERTEX_POINT ( 'NONE', #23949 ) ;
#55123 = CARTESIAN_POINT ( 'NONE',  ( -50.99292637653379501, 8.102448949553172852, -5.886773742842744461 ) ) ;
#55124 = CARTESIAN_POINT ( 'NONE',  ( 0.000000000000000000, 87.30187232391182306, 8.025000000000000355 ) ) ;
#55125 =( NAMED_UNIT ( * ) PLANE_ANGLE_UNIT ( ) SI_UNIT ( $, .RADIAN. ) );
#55126 = VERTEX_POINT ( 'NONE', #30597 ) ;
#55127 = ORIENTED_EDGE ( 'NONE', *, *, #36524, .F. ) ;
#55128 = CARTESIAN_POINT ( 'NONE',  ( -74.99999999999998579, 50.00000000000000000, -12.00000000000000000 ) ) ;
#55129 = PRESENTATION_LAYER_ASSIGNMENT (  '', '', ( #67505 ) ) ;
#55130 = EDGE_CURVE ( 'NONE', #40384, #33911, #13195, .T. ) ;
#55131 = PRESENTATION_LAYER_ASSIGNMENT (  '', '', ( #15875 ) ) ;
#55132 = VECTOR ( 'NONE', #51676, 1000.000000000000000 ) ;
#55133 = FACE_OUTER_BOUND ( 'NONE', #36304, .T. ) ;
#55134 = CARTESIAN_POINT ( 'NONE',  ( 8.082903768654762899, -1.105959442090949618E-15, 7.500000000000000000 ) ) ;
#55135 = DIRECTION ( 'NONE',  ( 1.000000000000000000, 0.000000000000000000, -0.000000000000000000 ) ) ;
#55136 = ORIENTED_EDGE ( 'NONE', *, *, #46420, .F. ) ;
#55137 = AXIS2_PLACEMENT_3D ( 'NONE', #35155, #3804, #35852 ) ;
#55138 = CARTESIAN_POINT ( 'NONE',  ( -116.7549999999999812, 4.716976649647091513, -6.492361379858946790 ) ) ;
#55139 = EDGE_LOOP ( 'NONE', ( #12460, #49113 ) ) ;
#55140 = LINE ( 'NONE', #44315, #42211 ) ;
#55141 = CARTESIAN_POINT ( 'NONE',  ( 7.342319042881621627, -5.282730372348553693, -4.573977915173220598E-17 ) ) ;
#55142 = VERTEX_POINT ( 'NONE', #52103 ) ;
#55143 = CARTESIAN_POINT ( 'NONE',  ( -56.24292637653380211, 5.598654528085804216, 7.705886871421366635 ) ) ;
#55144 = LINE ( 'NONE', #27367, #41188 ) ;
#55145 = ORIENTED_EDGE ( 'NONE', *, *, #4183, .T. ) ;
#55146 = AXIS2_PLACEMENT_3D ( 'NONE', #46464, #29175, #19682 ) ;
#55147 = PRESENTATION_STYLE_ASSIGNMENT (( #38344 ) ) ;
#55148 = VECTOR ( 'NONE', #47710, 1000.000000000000000 ) ;
#55149 = CARTESIAN_POINT ( 'NONE',  ( -8.082903768654762899, 3.516382302766490365E-15, 7.500000000000000000 ) ) ;
#55150 = ORIENTED_EDGE ( 'NONE', *, *, #9401, .T. ) ;
#55151 = COLOUR_RGB ( '', 0.09019608, 0.27058824, 0.51372549) ;
#55152 = ORIENTED_EDGE ( 'NONE', *, *, #47642, .F. ) ;
#55153 = CARTESIAN_POINT ( 'NONE',  ( -8.705293062390095926, 110.4999999999999716, -3.890206119981057142 ) ) ;
#55154 = CARTESIAN_POINT ( 'NONE',  ( -21.02379604162863913, 110.4999999999999858, -10.50000000000000000 ) ) ;
#55155 = CARTESIAN_POINT ( 'NONE',  ( 45.00000000000000000, 10.69371294336137801, 4.000000000000000000 ) ) ;
#55156 = VERTEX_POINT ( 'NONE', #57002 ) ;
#55157 = CARTESIAN_POINT ( 'NONE',  ( -9.827790563157511022E-16, 139.4429263765338192, 8.025000000000000355 ) ) ;
#55158 = CARTESIAN_POINT ( 'NONE',  ( 45.50000000000000000, -1.469576158976824618E-14, -9.500000000000000000 ) ) ;
#55159 = STYLED_ITEM ( 'NONE', ( #21497 ), #52566 ) ;
#55160 = FACE_OUTER_BOUND ( 'NONE', #38858, .T. ) ;
#55161 = LINE ( 'NONE', #12600, #50115 ) ;
#55162 = ORIENTED_EDGE ( 'NONE', *, *, #5147, .T. ) ;
#55163 = AXIS2_PLACEMENT_3D ( 'NONE', #26942, #43900, #10809 ) ;
#55164 = EDGE_CURVE ( 'NONE', #1567, #63720, #40507, .T. ) ;
#55165 = VERTEX_POINT ( 'NONE', #41541 ) ;
#55166 = CARTESIAN_POINT ( 'NONE',  ( -6.062177826491071286, 3.500000000000000888, 0.000000000000000000 ) ) ;
#55167 = CARTESIAN_POINT ( 'NONE',  ( -131.0049999999999670, 6.826472737025116366, 4.959722759717898555 ) ) ;
#55168 = DIRECTION ( 'NONE',  ( 0.000000000000000000, 0.000000000000000000, -1.000000000000000000 ) ) ;
#55169 = SURFACE_STYLE_FILL_AREA ( #33722 ) ;
#55170 = ORIENTED_EDGE ( 'NONE', *, *, #19717, .T. ) ;
#55171 = CARTESIAN_POINT ( 'NONE',  ( -5.598654528085808657, 122.6449999999999960, 7.705886871421373741 ) ) ;
#55172 = CARTESIAN_POINT ( 'NONE',  ( -5.000000000000000000, 0.000000000000000000, 0.2500000000000011102 ) ) ;
#55173 = FACE_OUTER_BOUND ( 'NONE', #2094, .T. ) ;
#55174 = CARTESIAN_POINT ( 'NONE',  ( -4.750000000000002665, 24.74999999999998579, 4.000000000000000000 ) ) ;
#55175 = ORIENTED_EDGE ( 'NONE', *, *, #1245, .F. ) ;
#55176 = MECHANICAL_DESIGN_GEOMETRIC_PRESENTATION_REPRESENTATION (  '', ( #31588 ), #43999 ) ;
#55177 = ORIENTED_EDGE ( 'NONE', *, *, #29248, .F. ) ;
#55178 = CARTESIAN_POINT ( 'NONE',  ( -45.91547274699541958, 9.430195759334528915, 3.560059854842081872 ) ) ;
#55179 = CARTESIAN_POINT ( 'NONE',  ( 179.4361977533490631, 5.000000000000000000, -103.7004518695262192 ) ) ;
#55180 = DIRECTION ( 'NONE',  ( 0.000000000000000000, 0.000000000000000000, 1.000000000000000000 ) ) ;
#55181 = ORIENTED_EDGE ( 'NONE', *, *, #54378, .F. ) ;
#55182 = PLANE ( 'NONE',  #7865 ) ;
#55183 = EDGE_CURVE ( 'NONE', #20470, #50261, #35204, .T. ) ;
#55184 = CARTESIAN_POINT ( 'NONE',  ( -53.60138881051016568, -9.947368421052624754, 2.722470280083841843 ) ) ;
#55185 =( NAMED_UNIT ( * ) PLANE_ANGLE_UNIT ( ) SI_UNIT ( $, .RADIAN. ) );
#55186 = EDGE_CURVE ( 'NONE', #57001, #22068, #22430, .T. ) ;
#55187 = B_SPLINE_CURVE_WITH_KNOTS ( 'NONE', 3,
 ( #8410, #60798, #18926, #12973, #2356, #34087, #61487, #2725, #24217, #49018 ),
 .UNSPECIFIED., .F., .F.,
 ( 4, 2, 2, 2, 4 ),
 ( 0.000000000000000000, 0.0004159702800446777042, 0.0008319405600893554084, 0.001247910840134033167, 0.001663881120178710817 ),
 .UNSPECIFIED. ) ;
#55188 = EDGE_CURVE ( 'NONE', #44668, #47418, #519, .T. ) ;
#55189 = CYLINDRICAL_SURFACE ( 'NONE', #21683, 9.524999999999991473 ) ;
#55190 = SURFACE_STYLE_FILL_AREA ( #33739 ) ;
#55191 = ORIENTED_EDGE ( 'NONE', *, *, #8592, .T. ) ;
#55192 = LINE ( 'NONE', #28445, #54919 ) ;
#55193 = MECHANICAL_DESIGN_GEOMETRIC_PRESENTATION_REPRESENTATION (  '', ( #33852 ), #14811 ) ;
#55194 = EDGE_CURVE ( 'NONE', #14819, #5042, #47672, .T. ) ;
#55195 = VECTOR ( 'NONE', #34695, 1000.000000000000000 ) ;
#55196 = LINE ( 'NONE', #7379, #3294 ) ;
#55197 = CARTESIAN_POINT ( 'NONE',  ( -7.566679973970432016, 2.499999999999994671, -4.894125840469273570 ) ) ;
#55198 = CARTESIAN_POINT ( 'NONE',  ( 34.99999999999999289, 99.99999999999998579, -7.000000000000000000 ) ) ;
#55199 = FILL_AREA_STYLE_COLOUR ( '', #12352 ) ;
#55200 = CARTESIAN_POINT ( 'NONE',  ( 14.09999999999999609, 11.99999999999999289, 4.000000000000000000 ) ) ;
#55201 = AXIS2_PLACEMENT_3D ( 'NONE', #36019, #29688, #56410 ) ;
#55202 = EDGE_CURVE ( 'NONE', #63907, #34321, #14982, .T. ) ;
#55203 = CARTESIAN_POINT ( 'NONE',  ( -103.9449999999999932, -9.827790563157499189E-16, -8.024999999999991473 ) ) ;
#55204 = CARTESIAN_POINT ( 'NONE',  ( -3.094860106618432471, 122.7049999999999699, -9.525000000000000355 ) ) ;
#55205 = CARTESIAN_POINT ( 'NONE',  ( -75.59499999999998465, 2.607480562269073321, 8.024999999999991473 ) ) ;
#55206 = AXIS2_PLACEMENT_3D ( 'NONE', #12221, #43282, #44646 ) ;
#55207 = CYLINDRICAL_SURFACE ( 'NONE', #24090, 0.2500000000000000000 ) ;
#55208 = CARTESIAN_POINT ( 'NONE',  ( -87.50000000000000000, -8.499999999999989342, 24.00000000000000000 ) ) ;
#55209 = COLOUR_RGB ( '', 0.72549020, 0.75294118, 0.79215686) ;
#55210 = DIRECTION ( 'NONE',  ( 7.703719777548942317E-32, -1.000000000000000000, -0.000000000000000000 ) ) ;
#55211 = UNCERTAINTY_MEASURE_WITH_UNIT (LENGTH_MEASURE( 1.000000000000000082E-05 ), #26364, 'distance_accuracy_value', 'NONE');
#55212 = STYLED_ITEM ( 'NONE', ( #49216 ), #54548 ) ;
#55213 = CARTESIAN_POINT ( 'NONE',  ( 41.26950967128010461, 107.7917145016473768, -3.849034857644456409 ) ) ;
#55214 = ORIENTED_EDGE ( 'NONE', *, *, #7547, .F. ) ;
#55215 = CARTESIAN_POINT ( 'NONE',  ( -119.8429263765338106, 9.058813317711329915, -2.943386871421373119 ) ) ;
#55216 = B_SPLINE_CURVE_WITH_KNOTS ( 'NONE', 3,
 ( #37251, #4470, #19015, #40524, #20688, #42197 ),
 .UNSPECIFIED., .F., .F.,
 ( 4, 2, 4 ),
 ( 0.000000000000000000, 0.003161799692372087474, 0.006323599384744174948 ),
 .UNSPECIFIED. ) ;
#55217 = CARTESIAN_POINT ( 'NONE',  ( -133.1950000000000216, 8.437984349512085203, -1.550032578732815448E-15 ) ) ;
#55219 = DIRECTION ( 'NONE',  ( -0.000000000000000000, 1.000000000000000000, -0.000000000000000000 ) ) ;
#55218 = VECTOR ( 'NONE', #17456, 1000.000000000000000 ) ;
#55220 = CONICAL_SURFACE ( 'NONE', #3517, 5.500000000000005329, 0.7853981633974579379 ) ;
#55221 = DIRECTION ( 'NONE',  ( -0.000000000000000000, -0.000000000000000000, -1.000000000000000000 ) ) ;
#55222 = ORIENTED_EDGE ( 'NONE', *, *, #53577, .F. ) ;
#55223 = ORIENTED_EDGE ( 'NONE', *, *, #20248, .F. ) ;
#55224 = CARTESIAN_POINT ( 'NONE',  ( -47.00571487472603849, -11.85301361210300897, 3.279042910798403820 ) ) ;
#55225 =( LENGTH_UNIT ( ) NAMED_UNIT ( * ) SI_UNIT ( .MILLI., .METRE. ) );
#55226 = AXIS2_PLACEMENT_3D ( 'NONE', #46409, #56569, #8401 ) ;
#55227 = CARTESIAN_POINT ( 'NONE',  ( 0.000000000000000000, 0.000000000000000000, 4.000000000000000000 ) ) ;
#55228 = CARTESIAN_POINT ( 'NONE',  ( 8.319377385370872346, -3.000000000000000888, -2.000000000000000000 ) ) ;
#55229 = VECTOR ( 'NONE', #31812, 1000.000000000000000 ) ;
#55230 = DIRECTION ( 'NONE',  ( -1.000000000000000000, -0.000000000000000000, -0.000000000000000000 ) ) ;
#55231 = FILL_AREA_STYLE ('',( #13977 ) ) ;
#55232 = ORIENTED_EDGE ( 'NONE', *, *, #34759, .T. ) ;
#55233 = CARTESIAN_POINT ( 'NONE',  ( -143.3049999999999784, 8.437984349512086979, -1.550032578732815448E-15 ) ) ;
#55234 = ORIENTED_EDGE ( 'NONE', *, *, #38491, .T. ) ;
#55235 = ORIENTED_EDGE ( 'NONE', *, *, #14623, .T. ) ;
#55236 = DIRECTION ( 'NONE',  ( 0.000000000000000000, 0.000000000000000000, -1.000000000000000000 ) ) ;
#55237 = CARTESIAN_POINT ( 'NONE',  ( -34.99999999999999289, 99.99999999999998579, 4.000000000000000000 ) ) ;
#55238 = ORIENTED_EDGE ( 'NONE', *, *, #18109, .T. ) ;
#55239 = VECTOR ( 'NONE', #27774, 1000.000000000000000 ) ;
#55240 = CARTESIAN_POINT ( 'NONE',  ( 0.000000000000000000, 2.299999999999999822, 0.000000000000000000 ) ) ;
#55241 = CARTESIAN_POINT ( 'NONE',  ( 55.65811388300842566, 13.02565835097472657, -6.500000000000000000 ) ) ;
#55242 = CARTESIAN_POINT ( 'NONE',  ( 5.598654528085809545, 133.1449999999999818, -7.705886871421373741 ) ) ;
#55243 = LINE ( 'NONE', #17316, #64299 ) ;
#55244 = ORIENTED_EDGE ( 'NONE', *, *, #21455, .T. ) ;
#55245 = MECHANICAL_DESIGN_GEOMETRIC_PRESENTATION_REPRESENTATION (  '', ( #46309 ), #46411 ) ;
#55246 = CARTESIAN_POINT ( 'NONE',  ( 66.49999999999998579, 34.24999999999999289, -3.750000000000000000 ) ) ;
#55247 = CARTESIAN_POINT ( 'NONE',  ( 10.01517768586949408, 127.8050000000000068, 1.839758294383810543E-15 ) ) ;
#55248 = CIRCLE ( 'NONE', #13681, 7.500000000000007105 ) ;
#55249 = CARTESIAN_POINT ( 'NONE',  ( -54.35499999999998977, -4.716976649647093289, -6.492361379858945902 ) ) ;
#55250 = DIRECTION ( 'NONE',  ( 1.000000000000000000, 0.000000000000000000, 0.000000000000000000 ) ) ;
#55251 = EDGE_LOOP ( 'NONE', ( #50244, #30941, #30481, #52705 ) ) ;
#55252 = CARTESIAN_POINT ( 'NONE',  ( 5.598654528085805993, 160.3549999999999898, 7.705886871421374629 ) ) ;
#55253 = CARTESIAN_POINT ( 'NONE',  ( -195.0000000000000000, 1.166476076187852838E-15, -9.524999999999991473 ) ) ;
#55254 = UNCERTAINTY_MEASURE_WITH_UNIT (LENGTH_MEASURE( 1.000000000000000082E-05 ), #37519, 'distance_accuracy_value', 'NONE');
#55255 = SURFACE_STYLE_USAGE ( .BOTH. , #45106 ) ;
#55256 = CIRCLE ( 'NONE', #19299, 16.00000000000000000 ) ;
#55257 =( NAMED_UNIT ( * ) SI_UNIT ( $, .STERADIAN. ) SOLID_ANGLE_UNIT ( ) );
#55258 = CARTESIAN_POINT ( 'NONE',  ( -14.98999599679678951, 146.9999999999999716, -10.00000000000000000 ) ) ;
#55259 = VERTEX_POINT ( 'NONE', #8489 ) ;
#55260 = AXIS2_PLACEMENT_3D ( 'NONE', #30478, #51974, #4803 ) ;
#55261 = ADVANCED_FACE ( 'NONE', ( #2803 ), #51382, .T. ) ;
#55262 = ORIENTED_EDGE ( 'NONE', *, *, #23551, .T. ) ;
#55263 = CARTESIAN_POINT ( 'NONE',  ( 12.50000000000000533, 27.74999999999998224, -3.750000000000000000 ) ) ;
#55264 = CARTESIAN_POINT ( 'NONE',  ( -159.5049999999999955, -6.826472737025115478, -4.959722759717899443 ) ) ;
#55266 = ORIENTED_EDGE ( 'NONE', *, *, #62970, .F. ) ;
#55265 = AXIS2_PLACEMENT_3D ( 'NONE', #12778, #63896, #44504 ) ;
#55267 = FILL_AREA_STYLE ('',( #28156 ) ) ;
#55268 = UNCERTAINTY_MEASURE_WITH_UNIT (LENGTH_MEASURE( 1.000000000000000082E-05 ), #16031, 'distance_accuracy_value', 'NONE');
#55269 = EDGE_CURVE ( 'NONE', #59375, #42973, #38010, .T. ) ;
#55270 = CIRCLE ( 'NONE', #28322, 1.000000000000000888 ) ;
#55271 = DIRECTION ( 'NONE',  ( -0.000000000000000000, 0.000000000000000000, 1.000000000000000000 ) ) ;
#55272 = SURFACE_STYLE_USAGE ( .BOTH. , #33149 ) ;
#55273 = CARTESIAN_POINT ( 'NONE',  ( 44.99999999999977973, 149.9999999999999716, 10.00000000000000000 ) ) ;
#55274 = VECTOR ( 'NONE', #1795, 1000.000000000000000 ) ;
#55275 = EDGE_LOOP ( 'NONE', ( #47960, #66017, #34557, #37542 ) ) ;
#55276 = EDGE_CURVE ( 'NONE', #50329, #60715, #37506, .T. ) ;
#55277 = ORIENTED_EDGE ( 'NONE', *, *, #11779, .F. ) ;
#55278 = CARTESIAN_POINT ( 'NONE',  ( -45.21668476334829734, 8.382617245700997088, -3.141643734658259302 ) ) ;
#55279 = CARTESIAN_POINT ( 'NONE',  ( 48.50000000000000000, 14.49137674618942917, 7.000000000000000000 ) ) ;
#55280 = STYLED_ITEM ( 'NONE', ( #67312 ), #28742 ) ;
#55281 = CARTESIAN_POINT ( 'NONE',  ( -87.50499999999995282, -6.826472737025115478, -4.959722759717899443 ) ) ;
#55282 = ORIENTED_EDGE ( 'NONE', *, *, #27467, .F. ) ;
#55283 = CARTESIAN_POINT ( 'NONE',  ( 71.62068965517239860, 36.41396814395972115, -7.000000000000000000 ) ) ;
#55284 = VECTOR ( 'NONE', #11246, 1000.000000000000000 ) ;
#55285 = ADVANCED_FACE ( 'NONE', ( #53128 ), #44223, .T. ) ;
#55286 = FILL_AREA_STYLE ('',( #13408 ) ) ;
#55287 = DIRECTION ( 'NONE',  ( -0.000000000000000000, -1.000000000000000000, -0.000000000000000000 ) ) ;
#55288 = EDGE_CURVE ( 'NONE', #34398, #30766, #48516, .T. ) ;
#55289 = CARTESIAN_POINT ( 'NONE',  ( -74.27256294509165002, 8.702587636786763170, -6.424237564331914285 ) ) ;
#55290 = ORIENTED_EDGE ( 'NONE', *, *, #65799, .T. ) ;
#55291 = DIRECTION ( 'NONE',  ( -0.000000000000000000, -1.000000000000000000, -0.000000000000000000 ) ) ;
#55292 = PRESENTATION_LAYER_ASSIGNMENT (  '', '', ( #6992 ) ) ;
#55294 = FACE_BOUND ( 'NONE', #3588, .T. ) ;
#55293 = CARTESIAN_POINT ( 'NONE',  ( 96.10348817448824832, 5.000000000000000000, -27.38099488609876531 ) ) ;
#55295 = CARTESIAN_POINT ( 'NONE',  ( -9.058813317711337021, 128.0449999999999875, -2.943386871421374895 ) ) ;
#55296 = CARTESIAN_POINT ( 'NONE',  ( -108.8949999999999960, 6.826472737025116366, 4.959722759717898555 ) ) ;
#55297 = AXIS2_PLACEMENT_3D ( 'NONE', #65702, #54777, #50570 ) ;
#55298 = DIRECTION ( 'NONE',  ( 0.000000000000000000, 0.000000000000000000, 1.000000000000000000 ) ) ;
#55300 = CARTESIAN_POINT ( 'NONE',  ( -18.05533399021871332, 11.32548081226861569, 3.971246689443173050 ) ) ;
#55299 = DIRECTION ( 'NONE',  ( 1.000000000000000000, 0.000000000000000000, -0.000000000000000000 ) ) ;
#55301 = VECTOR ( 'NONE', #41208, 1000.000000000000000 ) ;
#55302 = CARTESIAN_POINT ( 'NONE',  ( -157.0429263765338135, -9.058813317711329915, -2.943386871421370898 ) ) ;
#55303 = CARTESIAN_POINT ( 'NONE',  ( -171.4449999999999932, 0.000000000000000000, 8.024999999999991473 ) ) ;
#55304 = ADVANCED_FACE ( 'NONE', ( #58739 ), #36337, .T. ) ;
#55305 = CARTESIAN_POINT ( 'NONE',  ( 57.74999999999999289, 28.24999999999998934, -4.000000000000000000 ) ) ;
#55306 = FACE_OUTER_BOUND ( 'NONE', #20421, .T. ) ;
#55307 = ORIENTED_EDGE ( 'NONE', *, *, #62830, .T. ) ;
#55308 = CARTESIAN_POINT ( 'NONE',  ( 2.999999999999998668, 0.000000000000000000, 72.00402776293822171 ) ) ;
#55309 = ORIENTED_EDGE ( 'NONE', *, *, #31596, .F. ) ;
#55310 = CARTESIAN_POINT ( 'NONE',  ( -66.59292637653381064, -3.094860106618431139, -9.524999999999991473 ) ) ;
#55311 = CARTESIAN_POINT ( 'NONE',  ( -45.90010448357104877, 9.371898184802233800, 6.142471281331792987 ) ) ;
#55312 = DIRECTION ( 'NONE',  ( -1.000000000000000000, 0.000000000000000000, 0.000000000000000000 ) ) ;
#55313 = EDGE_CURVE ( 'NONE', #21392, #23152, #12679, .T. ) ;
#55314 = TOROIDAL_SURFACE ( 'NONE', #14876, 14.49999999999999822, 0.5000000000000000000 ) ;
#55315 = VECTOR ( 'NONE', #40399, 1000.000000000000000 ) ;
#55316 = CARTESIAN_POINT ( 'NONE',  ( -4.750000000000002665, 24.74999999999998579, -3.750000000000000000 ) ) ;
#55317 = CARTESIAN_POINT ( 'NONE',  ( -43.75000000000000000, 0.000000000000000000, -2.000000000000000000 ) ) ;
#55318 = DIRECTION ( 'NONE',  ( -1.000000000000000000, -7.709882115452468306E-16, 0.000000000000000000 ) ) ;
#55319 = LINE ( 'NONE', #33191, #66734 ) ;
#55320 = ORIENTED_EDGE ( 'NONE', *, *, #27291, .F. ) ;
#55321 = CARTESIAN_POINT ( 'NONE',  ( -173.3049999999999500, 8.437984349512086979, -1.550032578732815448E-15 ) ) ;
#55322 = VECTOR ( 'NONE', #56404, 1000.000000000000000 ) ;
#55323 = ORIENTED_EDGE ( 'NONE', *, *, #30083, .T. ) ;
#55324 = AXIS2_PLACEMENT_3D ( 'NONE', #7964, #45646, #61747 ) ;
#55325 = DIRECTION ( 'NONE',  ( 0.000000000000000000, 1.000000000000000000, 0.000000000000000000 ) ) ;
#55326 =( LENGTH_UNIT ( ) NAMED_UNIT ( * ) SI_UNIT ( .MILLI., .METRE. ) );
#55327 = FACE_BOUND ( 'NONE', #14392, .T. ) ;
#55328 = CARTESIAN_POINT ( 'NONE',  ( -4.716976649647098618, 149.2570736234661695, 6.492361379858953008 ) ) ;
#55329 = AXIS2_PLACEMENT_3D ( 'NONE', #32797, #54592, #6398 ) ;
#55330 = ORIENTED_EDGE ( 'NONE', *, *, #56064, .T. ) ;
#55331 = FILL_AREA_STYLE_COLOUR ( '', #63104 ) ;
#55332 = STYLED_ITEM ( 'NONE', ( #24439 ), #310 ) ;
#55333 = CARTESIAN_POINT ( 'NONE',  ( -87.65499999999998693, -7.632228543268600340, -2.479861379858950166 ) ) ;
#55334 = DIRECTION ( 'NONE',  ( 0.000000000000000000, 0.000000000000000000, -1.000000000000000000 ) ) ;
#55335 = CARTESIAN_POINT ( 'NONE',  ( 10.01517768586949231, 130.8049999999999784, 1.839758294383810543E-15 ) ) ;
#55336 = UNCERTAINTY_MEASURE_WITH_UNIT (LENGTH_MEASURE( 1.000000000000000082E-05 ), #51582, 'distance_accuracy_value', 'NONE');
#55337 = SURFACE_STYLE_USAGE ( .BOTH. , #12072 ) ;
#55338 = DIRECTION ( 'NONE',  ( -0.000000000000000000, -1.000000000000000000, -0.000000000000000000 ) ) ;
#55339 = ADVANCED_FACE ( 'NONE', ( #52786 ), #9872, .F. ) ;
#55340 = EDGE_CURVE ( 'NONE', #59244, #33888, #26366, .T. ) ;
#55341 = CARTESIAN_POINT ( 'NONE',  ( -113.2429263765338163, 5.598654528085804216, 7.705886871421366635 ) ) ;
#55342 = DIRECTION ( 'NONE',  ( -1.000000000000000000, 0.000000000000000000, 0.000000000000000000 ) ) ;
#55343 = LINE ( 'NONE', #23334, #24938 ) ;
#55344 = ORIENTED_EDGE ( 'NONE', *, *, #578, .F. ) ;
#55345 = AXIS2_PLACEMENT_3D ( 'NONE', #1994, #56573, #40090 ) ;
#55346 = STYLED_ITEM ( 'NONE', ( #38240 ), #60998 ) ;
#55347 = CARTESIAN_POINT ( 'NONE',  ( -140.4570736234661865, -9.058813317711329915, 2.943386871421371787 ) ) ;
#55348 = CARTESIAN_POINT ( 'NONE',  ( -57.89499999999996760, 6.826472737025116366, 4.959722759717898555 ) ) ;
#55349 = ORIENTED_EDGE ( 'NONE', *, *, #54012, .T. ) ;
#55350 = DIRECTION ( 'NONE',  ( 1.000000000000000000, -0.000000000000000000, -0.000000000000000000 ) ) ;
#55351 = EDGE_CURVE ( 'NONE', #2410, #50347, #26186, .T. ) ;
#55352 = AXIS2_PLACEMENT_3D ( 'NONE', #19255, #24527, #29477 ) ;
#55353 =( LENGTH_UNIT ( ) NAMED_UNIT ( * ) SI_UNIT ( .MILLI., .METRE. ) );
#55354 = CARTESIAN_POINT ( 'NONE',  ( -45.00000000000000000, 8.552062714373262153, -6.929199553059594230 ) ) ;
#55355 = DIRECTION ( 'NONE',  ( -0.000000000000000000, -1.000000000000000000, -0.000000000000000000 ) ) ;
#55356 = ORIENTED_EDGE ( 'NONE', *, *, #55415, .F. ) ;
#55357 = CARTESIAN_POINT ( 'NONE',  ( -47.95907446719336775, -11.64228093534878994, 3.355646384069886246 ) ) ;
#55358 = CARTESIAN_POINT ( 'NONE',  ( -57.14499999999997470, -4.716976649647092401, 6.492361379858946790 ) ) ;
#55359 = ORIENTED_EDGE ( 'NONE', *, *, #46388, .T. ) ;
#55360 = CARTESIAN_POINT ( 'NONE',  ( -75.00000000000000000, 36.00000000000000711, 9.500000000000000000 ) ) ;
#55362 = CLOSED_SHELL ( 'NONE', ( #31703, #66220, #44795, #32816, #59893, #43008, #37715, #10675, #48732, #44985, #42472, #60563, #3960, #54038, #16306, #30245, #16478, #38161, #11849, #58293, #57586, #10719, #3607, #36561, #44997, #5498, #41251, #58385, #36449, #45643, #49434, #15132, #13506, #54335, #48091, #41252, #59880, #4938, #27983, #47244, #53323, #16444, #52891, #63317, #44761, #46804, #30379, #45300, #42878, #7564, #27429, #5026, #67679, #45565, #27993, #10903, #60035, #69531, #64869, #52290, #52368, #19545, #14822, #9011, #3277, #14147, #57416, #54068, #55943, #33670, #3905, #27056, #60345, #20432, #23745, #8997, #46812, #1908, #53427, #36982, #65871, #43094, #67412, #32160, #35514, #39850, #54951 ) ) ;
#55361 = CARTESIAN_POINT ( 'NONE',  ( -114.5050000000000097, -6.826472737025115478, -4.959722759717899443 ) ) ;
#55363 = ORIENTED_EDGE ( 'NONE', *, *, #43201, .T. ) ;
#55365 = STYLED_ITEM ( 'NONE', ( #33703 ), #22907 ) ;
#55364 = SURFACE_STYLE_FILL_AREA ( #55718 ) ;
#55366 = EDGE_CURVE ( 'NONE', #63828, #22057, #18331, .T. ) ;
#55367 = CYLINDRICAL_SURFACE ( 'NONE', #12272, 0.2500000000000002220 ) ;
#55368 = CARTESIAN_POINT ( 'NONE',  ( -4.250000000000001776, 22.24999999999998579, -3.750000000000000000 ) ) ;
#55369 = CARTESIAN_POINT ( 'NONE',  ( -150.8070736234661808, 10.01517768586948698, -1.839758294383808571E-15 ) ) ;
#55370 = PRODUCT_DEFINITION_SHAPE ( 'NONE', 'NONE',  #69721 ) ;
#55371 = AXIS2_PLACEMENT_3D ( 'NONE', #12341, #38795, #23270 ) ;
#55372 = DIRECTION ( 'NONE',  ( 0.000000000000000000, 1.000000000000000000, -0.000000000000000000 ) ) ;
#55373 = CARTESIAN_POINT ( 'NONE',  ( -5.598654528085806881, 130.7450000000000045, -7.705886871421374629 ) ) ;
#55374 = CARTESIAN_POINT ( 'NONE',  ( -84.05707362346618083, 0.000000000000000000, 9.524999999999991473 ) ) ;
#55375 = STYLED_ITEM ( 'NONE', ( #12337 ), #55087 ) ;
#55376 = EDGE_CURVE ( 'NONE', #44849, #443, #42278, .T. ) ;
#55377 = VERTEX_POINT ( 'NONE', #266 ) ;
#55378 = CARTESIAN_POINT ( 'NONE',  ( 48.50000000000000000, 99.99999999999998579, -7.000000000000000000 ) ) ;
#55379 = FILL_AREA_STYLE_COLOUR ( '', #50375 ) ;
#55381 = AXIS2_PLACEMENT_3D ( 'NONE', #18154, #66331, #38618 ) ;
#55380 = PLANE ( 'NONE',  #43452 ) ;
#55382 = CARTESIAN_POINT ( 'NONE',  ( -133.4049999999999443, -2.607480562269069768, 8.024999999999991473 ) ) ;
#55383 = CARTESIAN_POINT ( 'NONE',  ( 22.00000000000000355, 42.00000000000000000, -75.00000000000001421 ) ) ;
#55384 = CARTESIAN_POINT ( 'NONE',  ( 23.21231517720798010, 117.4999999999999716, -10.00000000000000000 ) ) ;
#55385 =( GEOMETRIC_REPRESENTATION_CONTEXT ( 3 ) GLOBAL_UNCERTAINTY_ASSIGNED_CONTEXT ( ( #67793 ) ) GLOBAL_UNIT_ASSIGNED_CONTEXT ( ( #31833, #37528, #27913 ) ) REPRESENTATION_CONTEXT ( 'NONE', 'WORKASPACE' ) );
#55386 = CARTESIAN_POINT ( 'NONE',  ( -54.89292637653381490, -8.102448949553174629, -5.886773742842741797 ) ) ;
#55387 = CARTESIAN_POINT ( 'NONE',  ( -139.0450000000000159, 7.632228543268600340, 2.479861379858949277 ) ) ;
#55388 = CARTESIAN_POINT ( 'NONE',  ( -126.4450000000000074, 0.000000000000000000, 8.024999999999991473 ) ) ;
#55389 = DIRECTION ( 'NONE',  ( 0.000000000000000000, 0.000000000000000000, -1.000000000000000000 ) ) ;
#55390 = ORIENTED_EDGE ( 'NONE', *, *, #44912, .T. ) ;
#55391 = DIRECTION ( 'NONE',  ( -0.000000000000000000, 1.000000000000000000, -0.000000000000000000 ) ) ;
#55392 = CARTESIAN_POINT ( 'NONE',  ( -12.72792206135785698, 115.4999999999999574, 10.50000000000000000 ) ) ;
#55393 =( LENGTH_UNIT ( ) NAMED_UNIT ( * ) SI_UNIT ( .MILLI., .METRE. ) );
#55394 = CARTESIAN_POINT ( 'NONE',  ( -181.4929263765337737, -8.102448949553172852, 5.886773742842742685 ) ) ;
#55395 = CARTESIAN_POINT ( 'NONE',  ( -48.14499999999999602, -4.716976649647092401, 6.492361379858946790 ) ) ;
#55396 = CARTESIAN_POINT ( 'NONE',  ( -74.99999999999998579, 146.4999999999999716, 7.000000000000000000 ) ) ;
#55397 = CARTESIAN_POINT ( 'NONE',  ( -102.0570736234661808, 0.000000000000000000, 9.524999999999991473 ) ) ;
#55398 = CIRCLE ( 'NONE', #19445, 6.000000000000005329 ) ;
#55399 = CARTESIAN_POINT ( 'NONE',  ( -56.25180925730852977, -8.571333231932012353, -0.5793937067663862406 ) ) ;
#55400 = CARTESIAN_POINT ( 'NONE',  ( -94.49292637653381632, -8.102448949553172852, 5.886773742842742685 ) ) ;
#55401 = CARTESIAN_POINT ( 'NONE',  ( -53.60138881051016568, -9.947368421052624754, 2.722470280083841843 ) ) ;
#55402 = EDGE_CURVE ( 'NONE', #22419, #15243, #10556, .T. ) ;
#55403 = DIRECTION ( 'NONE',  ( 1.000000000000000000, 0.000000000000000000, 0.000000000000000000 ) ) ;
#55404 = CARTESIAN_POINT ( 'NONE',  ( -163.0429263765338135, -9.058813317711329915, -2.943386871421370898 ) ) ;
#55405 = DIRECTION ( 'NONE',  ( 0.000000000000000000, 1.000000000000000000, 0.000000000000000000 ) ) ;
#55406 = CIRCLE ( 'NONE', #7116, 0.5000000000000004441 ) ;
#55407 = VERTEX_POINT ( 'NONE', #68962 ) ;
#55408 = DIRECTION ( 'NONE',  ( 1.000000000000000000, -0.000000000000000000, 0.000000000000000000 ) ) ;
#55409 = DIRECTION ( 'NONE',  ( 0.000000000000000000, 1.000000000000000000, 0.000000000000000000 ) ) ;
#55410 = ORIENTED_EDGE ( 'NONE', *, *, #65130, .T. ) ;
#55411 = CARTESIAN_POINT ( 'NONE',  ( -45.00000000000000000, 0.000000000000000000, 0.000000000000000000 ) ) ;
#55412 = AXIS2_PLACEMENT_3D ( 'NONE', #26371, #4564, #68612 ) ;
#55413 = CARTESIAN_POINT ( 'NONE',  ( -9.827790563157511022E-16, 128.5570736234661524, 8.025000000000000355 ) ) ;
#55414 = PRODUCT_RELATED_PRODUCT_CATEGORY ( 'part', '', ( #26552 ) ) ;
#55415 = EDGE_CURVE ( 'NONE', #58900, #34410, #5588, .T. ) ;
#55416 = LINE ( 'NONE', #64921, #64151 ) ;
#55417 = EDGE_CURVE ( 'NONE', #36029, #13814, #23303, .T. ) ;
#55418 = CARTESIAN_POINT ( 'NONE',  ( -195.0000000000000000, 1.166476076187852838E-15, -9.524999999999991473 ) ) ;
#55419 = ORIENTED_EDGE ( 'NONE', *, *, #25804, .T. ) ;
#55420 = COLOUR_RGB ( '', 0.31764706, 0.68627451, 0.89019608) ;
#55421 = PRESENTATION_STYLE_ASSIGNMENT (( #1200 ) ) ;
#55422 = ADVANCED_FACE ( 'NONE', ( #64711 ), #11231, .F. ) ;
#55423 = COLOUR_RGB ( '', 0.09019608, 0.27058824, 0.51372549) ;
#55424 = FACE_OUTER_BOUND ( 'NONE', #54795, .T. ) ;
#55425 = EDGE_LOOP ( 'NONE', ( #49552, #50005, #29592, #14789 ) ) ;
#55426 = EDGE_CURVE ( 'NONE', #42065, #36018, #39728, .T. ) ;
#55427 = CARTESIAN_POINT ( 'NONE',  ( 11.00000000000001776, 26.00000000000000355, 23.99999999999999645 ) ) ;
#55428 = SURFACE_STYLE_FILL_AREA ( #2949 ) ;
#55429 = CARTESIAN_POINT ( 'NONE',  ( 4.716976649647099507, 149.6429263765338078, -6.492361379858953008 ) ) ;
#55430 = CARTESIAN_POINT ( 'NONE',  ( -94.19499999999999318, 8.437984349512085203, -1.550032578732815448E-15 ) ) ;
#55431 = ORIENTED_EDGE ( 'NONE', *, *, #42162, .F. ) ;
#55432 =( BOUNDED_CURVE ( )  B_SPLINE_CURVE ( 2, ( #38383, #54829, #65415, #39401, #33730, #60799, #60459, #59785, #61167, #54499, #28433 ),
 .UNSPECIFIED., .F., .F. ) 
 B_SPLINE_CURVE_WITH_KNOTS ( ( 3, 2, 2, 2, 2, 3 ),
 ( 0.5434782608695523098, 0.5456521739130305582, 0.5478260869565086955, 0.5499999999999870548, 0.5521739130434651921, 0.5543478260869434404 ),
 .UNSPECIFIED. ) 
 CURVE ( )  GEOMETRIC_REPRESENTATION_ITEM ( )  RATIONAL_B_SPLINE_CURVE ( ( 1.000000000000289990, 0.9510565162948635409, 1.000000000000000000, 0.9510565162951535312, 1.000000000000000000, 0.9510565162951535312, 1.000000000000000000, 0.9510565162951535312, 1.000000000000000000, 0.9510565162954485174, 0.9999999999997050137 ) ) 
 REPRESENTATION_ITEM ( '' )  );
#55433 = CONICAL_SURFACE ( 'NONE', #62144, 8.025000000000000355, 0.7853981633974491672 ) ;
#55434 = PRESENTATION_STYLE_ASSIGNMENT (( #28323 ) ) ;
#55435 = AXIS2_PLACEMENT_3D ( 'NONE', #41781, #50659, #45427 ) ;
#55436 = ADVANCED_FACE ( 'NONE', ( #65396 ), #33048, .T. ) ;
#55437 = ORIENTED_EDGE ( 'NONE', *, *, #37757, .T. ) ;
#55438 = CARTESIAN_POINT ( 'NONE',  ( -7.632228543268608334, 159.8429263765338249, 2.479861379858952830 ) ) ;
#55439 = DIRECTION ( 'NONE',  ( -0.000000000000000000, -0.000000000000000000, -1.000000000000000000 ) ) ;
#55440 = EDGE_CURVE ( 'NONE', #11647, #18309, #49811, .T. ) ;
#55442 = SPHERICAL_SURFACE ( 'NONE', #1889, 0.5000000000000000000 ) ;
#55441 = CIRCLE ( 'NONE', #5038, 0.5000000000000004441 ) ;
#55443 = EDGE_LOOP ( 'NONE', ( #15081, #21256, #22029, #49237 ) ) ;
#55444 = CARTESIAN_POINT ( 'NONE',  ( 3.000000000000030198, 34.36176364315826248, 80.00402776293826435 ) ) ;
#55445 = ORIENTED_EDGE ( 'NONE', *, *, #19047, .F. ) ;
#55446 = FACE_OUTER_BOUND ( 'NONE', #61926, .T. ) ;
#55447 = DIRECTION ( 'NONE',  ( -1.000000000000000000, 0.000000000000000000, 0.000000000000000000 ) ) ;
#55448 = CARTESIAN_POINT ( 'NONE',  ( -4.041451884327378785, -1.417096231345241542, 7.000000000000000000 ) ) ;
#55449 = PRESENTATION_LAYER_ASSIGNMENT (  '', '', ( #16167 ) ) ;
#55450 = CARTESIAN_POINT ( 'NONE',  ( -181.1070736234661638, 8.102448949553171076, -5.886773742842744461 ) ) ;
#55451 = DIRECTION ( 'NONE',  ( 1.000000000000000000, 0.000000000000000000, 0.000000000000000000 ) ) ;
#55452 = SURFACE_SIDE_STYLE ('',( #60033 ) ) ;
#55453 = CARTESIAN_POINT ( 'NONE',  ( -109.8570736234661780, -5.598654528085803328, -7.705886871421366635 ) ) ;
#55454 = DIRECTION ( 'NONE',  ( -1.000000000000000000, 1.156482317317866302E-16, 0.000000000000000000 ) ) ;
#55455 = CARTESIAN_POINT ( 'NONE',  ( -21.02379604162863913, 114.4999999999999574, -10.00000000000000000 ) ) ;
#55456 = ORIENTED_EDGE ( 'NONE', *, *, #21200, .T. ) ;
#55457 = CARTESIAN_POINT ( 'NONE',  ( 0.7152604538204497819, 42.96841842781390852, 45.59272046071829010 ) ) ;
#55458 =( NAMED_UNIT ( * ) SI_UNIT ( $, .STERADIAN. ) SOLID_ANGLE_UNIT ( ) );
#55459 = PRESENTATION_STYLE_ASSIGNMENT (( #49168 ) ) ;
#55460 = LINE ( 'NONE', #58238, #44544 ) ;
#55461 = ORIENTED_EDGE ( 'NONE', *, *, #7252, .T. ) ;
#55462 = VECTOR ( 'NONE', #48627, 1000.000000000000000 ) ;
#55463 = CARTESIAN_POINT ( 'NONE',  ( -159.3549999999999898, -4.716976649647093289, -6.492361379858945902 ) ) ;
#55464 = CARTESIAN_POINT ( 'NONE',  ( -183.9715320224743778, -8.560729921636262674, 0.5282838339113725690 ) ) ;
#55465 = CARTESIAN_POINT ( 'NONE',  ( -163.3449999999999989, 7.632228543268599452, -2.479861379858951942 ) ) ;
#55466 = VECTOR ( 'NONE', #29111, 1000.000000000000000 ) ;
#55467 = CARTESIAN_POINT ( 'NONE',  ( -153.2949999999999875, -2.607480562269069768, 8.024999999999991473 ) ) ;
#55468 = ADVANCED_FACE ( 'NONE', ( #28779 ), #39383, .T. ) ;
#55469 = ORIENTED_EDGE ( 'NONE', *, *, #59549, .F. ) ;
#55470 = PRESENTATION_LAYER_ASSIGNMENT (  '', '', ( #48742 ) ) ;
#55471 = FACE_OUTER_BOUND ( 'NONE', #12496, .T. ) ;
#55472 = CARTESIAN_POINT ( 'NONE',  ( 23.21231517720797655, 117.4999999999999716, 7.500000000000000000 ) ) ;
#55473 = VECTOR ( 'NONE', #34884, 1000.000000000000000 ) ;
#55474 = CARTESIAN_POINT ( 'NONE',  ( -72.35499999999998977, -4.716976649647093289, -6.492361379858945902 ) ) ;
#55475 = CARTESIAN_POINT ( 'NONE',  ( -34.83068933088741659, -10.82674371711464190, 3.661378181088279060 ) ) ;
#55476 = CARTESIAN_POINT ( 'NONE',  ( 15.98999599679679839, 117.4999999999999716, 10.00000000000000000 ) ) ;
#55477 = AXIS2_PLACEMENT_3D ( 'NONE', #33350, #48880, #27690 ) ;
#55478 = CARTESIAN_POINT ( 'NONE',  ( -73.79499999999997328, 2.607480562269069324, -8.024999999999993250 ) ) ;
#55479 = CARTESIAN_POINT ( 'NONE',  ( -9.058813317711338797, 144.4550000000000125, 2.943386871421373563 ) ) ;
#55480 = DIRECTION ( 'NONE',  ( -1.000000000000000000, 0.000000000000000000, 0.000000000000000000 ) ) ;
#55481 = STYLED_ITEM ( 'NONE', ( #50336 ), #2820 ) ;
#55482 = CARTESIAN_POINT ( 'NONE',  ( -177.2929263765339556, 3.094860106616924345, -9.525000000001085709 ) ) ;
#55483 = VECTOR ( 'NONE', #5788, 1000.000000000000000 ) ;
#55484 = DIRECTION ( 'NONE',  ( 1.300977106640437603E-16, 0.000000000000000000, 1.000000000000000000 ) ) ;
#55485 = STYLED_ITEM ( 'NONE', ( #8308 ), #7259 ) ;
#55486 =( LENGTH_UNIT ( ) NAMED_UNIT ( * ) SI_UNIT ( .MILLI., .METRE. ) );
#55487 = CARTESIAN_POINT ( 'NONE',  ( 10.39230484541326582, 1.107695154586738839, 1.440973567693753677E-18 ) ) ;
#55488 = DIRECTION ( 'NONE',  ( 0.000000000000000000, 0.000000000000000000, 1.000000000000000000 ) ) ;
#55489 = FILL_AREA_STYLE_COLOUR ( '', #32863 ) ;
#55490 = VERTEX_POINT ( 'NONE', #16886 ) ;
#55492 = ORIENTED_EDGE ( 'NONE', *, *, #66654, .T. ) ;
#55491 = PRESENTATION_LAYER_ASSIGNMENT (  '', '', ( #48818 ) ) ;
#55493 =( GEOMETRIC_REPRESENTATION_CONTEXT ( 3 ) GLOBAL_UNCERTAINTY_ASSIGNED_CONTEXT ( ( #48871 ) ) GLOBAL_UNIT_ASSIGNED_CONTEXT ( ( #21677, #58623, #54026 ) ) REPRESENTATION_CONTEXT ( 'NONE', 'WORKASPACE' ) );
#55494 = CARTESIAN_POINT ( 'NONE',  ( -195.0000000000000000, 9.184850993605130195E-16, -7.499999999999984901 ) ) ;
#55495 = CARTESIAN_POINT ( 'NONE',  ( -133.4070736234668004, 3.094860106608142925, -9.525000000007466383 ) ) ;
#55496 = ADVANCED_FACE ( 'NONE', ( #12603 ), #45017, .T. ) ;
#55497 = PRESENTATION_STYLE_ASSIGNMENT (( #60082 ) ) ;
#55498 = FACE_OUTER_BOUND ( 'NONE', #59930, .T. ) ;
#55499 = PRESENTATION_STYLE_ASSIGNMENT (( #60756 ) ) ;
#55500 = ORIENTED_EDGE ( 'NONE', *, *, #26187, .F. ) ;
#55501 = CARTESIAN_POINT ( 'NONE',  ( -107.4549999999999983, 7.632228543268599452, -2.479861379858951942 ) ) ;
#55502 = VERTEX_POINT ( 'NONE', #23503 ) ;
#55503 = CARTESIAN_POINT ( 'NONE',  ( -44.50000000000000000, -1.469576158976824302E-14, -4.000000000000000000 ) ) ;
#55504 = DIRECTION ( 'NONE',  ( 0.000000000000000000, 1.000000000000000000, -0.000000000000000000 ) ) ;
#55505 = EDGE_CURVE ( 'NONE', #40281, #37989, #59765, .T. ) ;
#55506 = VERTEX_POINT ( 'NONE', #2709 ) ;
#55507 = FACE_OUTER_BOUND ( 'NONE', #33897, .T. ) ;
#55508 = CARTESIAN_POINT ( 'NONE',  ( 0.000000000000000000, 2.500000000000000000, 0.000000000000000000 ) ) ;
#55509 = EDGE_LOOP ( 'NONE', ( #27802, #41975 ) ) ;
#55510 = AXIS2_PLACEMENT_3D ( 'NONE', #93, #21989, #43492 ) ;
#55511 = FACE_OUTER_BOUND ( 'NONE', #68977, .T. ) ;
#55512 = B_SPLINE_CURVE_WITH_KNOTS ( 'NONE', 3,
 ( #57873, #31804, #14600, #25486, #20925, #58545, #42422, #3654 ),
 .UNSPECIFIED., .F., .F.,
 ( 4, 2, 2, 4 ),
 ( 0.005458618329390014547, 0.006805794425120373359, 0.008152970520850733038, 0.01084732271231145413 ),
 .UNSPECIFIED. ) ;
#55513 = CARTESIAN_POINT ( 'NONE',  ( 0.000000000000000000, 13.00000000000000178, 80.00402776293826435 ) ) ;
#55514 = ORIENTED_EDGE ( 'NONE', *, *, #11200, .T. ) ;
#55515 = MECHANICAL_DESIGN_GEOMETRIC_PRESENTATION_REPRESENTATION (  '', ( #19565 ), #56628 ) ;
#55516 = ORIENTED_EDGE ( 'NONE', *, *, #33378, .T. ) ;
#55517 = AXIS2_PLACEMENT_3D ( 'NONE', #57513, #57876, #9338 ) ;
#55518 = CARTESIAN_POINT ( 'NONE',  ( 4.041451884327376121, 7.000000000000007105, 7.500000000000000000 ) ) ;
#55519 = DIRECTION ( 'NONE',  ( 0.000000000000000000, -1.000000000000000000, -0.000000000000000000 ) ) ;
#55520 = ORIENTED_EDGE ( 'NONE', *, *, #59076, .F. ) ;
#55521 = CARTESIAN_POINT ( 'NONE',  ( -7.632228543268608334, 132.8429263765338249, 2.479861379858952830 ) ) ;
#55522 = FACE_OUTER_BOUND ( 'NONE', #51724, .T. ) ;
#55523 = DIRECTION ( 'NONE',  ( 0.000000000000000000, 0.000000000000000000, -1.000000000000000000 ) ) ;
#55524 = EDGE_CURVE ( 'NONE', #52175, #27683, #34746, .T. ) ;
#55525 = COLOUR_RGB ( '', 0.40784314, 0.44705882, 0.49803922) ;
#55526 = DIRECTION ( 'NONE',  ( -1.000000000000000000, 0.000000000000000000, 0.000000000000000000 ) ) ;
#55527 = EDGE_LOOP ( 'NONE', ( #50275, #42817, #56532, #23253 ) ) ;
#55528 =( NAMED_UNIT ( * ) SI_UNIT ( $, .STERADIAN. ) SOLID_ANGLE_UNIT ( ) );
#55529 = ORIENTED_EDGE ( 'NONE', *, *, #41915, .T. ) ;
#55530 = DIRECTION ( 'NONE',  ( -0.000000000000000000, -1.000000000000000000, -0.000000000000000000 ) ) ;
#55531 = CARTESIAN_POINT ( 'NONE',  ( -7.632228543268607446, 139.6570736234661467, -2.479861379858953718 ) ) ;
#55532 = PRESENTATION_STYLE_ASSIGNMENT (( #62183 ) ) ;
#55533 = DIRECTION ( 'NONE',  ( 0.000000000000000000, 0.000000000000000000, 1.000000000000000000 ) ) ;
#55534 = CARTESIAN_POINT ( 'NONE',  ( -133.2549999999999955, -4.716976649647092401, 6.492361379858946790 ) ) ;
#55535 = DIRECTION ( 'NONE',  ( 0.000000000000000000, 0.000000000000000000, 1.000000000000000000 ) ) ;
#55536 = ORIENTED_EDGE ( 'NONE', *, *, #37320, .F. ) ;
#55537 = AXIS2_PLACEMENT_3D ( 'NONE', #65238, #38566, #28968 ) ;
#55538 = AXIS2_PLACEMENT_3D ( 'NONE', #7002, #24208, #7360 ) ;
#55539 = SURFACE_STYLE_FILL_AREA ( #45377 ) ;
#55540 = CARTESIAN_POINT ( 'NONE',  ( -156.7429263765338021, -5.598654528085803328, -7.705886871421366635 ) ) ;
#55541 = ORIENTED_EDGE ( 'NONE', *, *, #67754, .T. ) ;
#55542 = ORIENTED_EDGE ( 'NONE', *, *, #39131, .T. ) ;
#55543 = PRESENTATION_STYLE_ASSIGNMENT (( #3411 ) ) ;
#55544 = CARTESIAN_POINT ( 'NONE',  ( -71.62068965517238439, 63.58603185604027885, 9.500000000000000000 ) ) ;
#55545 = PRESENTATION_STYLE_ASSIGNMENT (( #55890 ) ) ;
#55546 = EDGE_LOOP ( 'NONE', ( #29459, #55266, #5943, #67216 ) ) ;
#55547 = CARTESIAN_POINT ( 'NONE',  ( 2.999999999999998668, 5.000000000000000000, -37.00402776293829277 ) ) ;
#55548 = LINE ( 'NONE', #6644, #5976 ) ;
#55549 = ADVANCED_FACE ( 'NONE', ( #66786 ), #50951, .T. ) ;
#55550 = DIRECTION ( 'NONE',  ( -0.000000000000000000, 0.000000000000000000, -1.000000000000000000 ) ) ;
#55551 = STYLED_ITEM ( 'NONE', ( #9511 ), #48817 ) ;
#55552 = VECTOR ( 'NONE', #16699, 1000.000000000000000 ) ;
#55553 = SURFACE_SIDE_STYLE ('',( #29138 ) ) ;
#55554 = EDGE_CURVE ( 'NONE', #65971, #9835, #13291, .T. ) ;
#55555 = CARTESIAN_POINT ( 'NONE',  ( -178.5570736234661808, -1.166476076187852838E-15, -9.524999999999991473 ) ) ;
#55556 = ORIENTED_EDGE ( 'NONE', *, *, #50537, .F. ) ;
#55557 = LINE ( 'NONE', #10665, #3222 ) ;
#55558 = DIRECTION ( 'NONE',  ( 0.7071067811865426878, 8.659560562354873694E-17, -0.7071067811865524577 ) ) ;
#55559 = CARTESIAN_POINT ( 'NONE',  ( -65.00000000000000000, -1.962809905030629631E-14, 11.50000000000003020 ) ) ;
#55560 = CARTESIAN_POINT ( 'NONE',  ( -29.49077592478069221, -8.499999999999996447, -0.3583504194180555102 ) ) ;
#55561 = FACE_OUTER_BOUND ( 'NONE', #23097, .T. ) ;
#55562 = CARTESIAN_POINT ( 'NONE',  ( -34.99999999999992895, 112.9999999999999858, -7.000000000000000000 ) ) ;
#55563 = VECTOR ( 'NONE', #45165, 1000.000000000000000 ) ;
#55564 = CARTESIAN_POINT ( 'NONE',  ( -99.44499999999999318, 0.000000000000000000, 8.024999999999991473 ) ) ;
#55565 = CARTESIAN_POINT ( 'NONE',  ( 8.102448949553183510, 122.1049999999999898, -5.886773742842746238 ) ) ;
#55566 = CARTESIAN_POINT ( 'NONE',  ( -73.64499999999998181, 4.716976649647091513, -6.492361379858946790 ) ) ;
#55567 = ADVANCED_BREP_SHAPE_REPRESENTATION ( '', ( #49805, #42840 ), #18040 ) ;
#55568 = CARTESIAN_POINT ( 'NONE',  ( 15.48999599679679662, 146.4999999999999716, 7.500000000000000000 ) ) ;
#55569 = DIRECTION ( 'NONE',  ( 1.000000000000000000, 0.000000000000000000, 0.000000000000000000 ) ) ;
#55570 = AXIS2_PLACEMENT_3D ( 'NONE', #6013, #33443, #21863 ) ;
#55571 = DIRECTION ( 'NONE',  ( 1.000000000000000000, 0.000000000000000000, -0.000000000000000000 ) ) ;
#55572 = CARTESIAN_POINT ( 'NONE',  ( 24.21231517720798010, 113.4999999999999858, 7.500000000000000000 ) ) ;
#55573 = CARTESIAN_POINT ( 'NONE',  ( 15.98999599679679839, 118.4999999999999716, -7.000000000000000000 ) ) ;
#55574 = VERTEX_POINT ( 'NONE', #56914 ) ;
#55575 = CARTESIAN_POINT ( 'NONE',  ( -127.0429263765337993, -9.058813317711329915, -2.943386871421370898 ) ) ;
#55576 = FILL_AREA_STYLE_COLOUR ( '', #60646 ) ;
#55577 = CARTESIAN_POINT ( 'NONE',  ( -140.5450000000000159, -7.632228543268600340, -2.479861379858950166 ) ) ;
#55578 = CARTESIAN_POINT ( 'NONE',  ( -5.365183871890746303, 4.707228941936129729, 0.1074872947962681735 ) ) ;
#55579 = EDGE_CURVE ( 'NONE', #56002, #18424, #37559, .T. ) ;
#55580 =( LENGTH_UNIT ( ) NAMED_UNIT ( * ) SI_UNIT ( .MILLI., .METRE. ) );
#55581 = ORIENTED_EDGE ( 'NONE', *, *, #6677, .F. ) ;
#55582 = VERTEX_POINT ( 'NONE', #35109 ) ;
#55583 =( LENGTH_UNIT ( ) NAMED_UNIT ( * ) SI_UNIT ( .MILLI., .METRE. ) );
#55584 =( GEOMETRIC_REPRESENTATION_CONTEXT ( 3 ) GLOBAL_UNCERTAINTY_ASSIGNED_CONTEXT ( ( #53209 ) ) GLOBAL_UNIT_ASSIGNED_CONTEXT ( ( #9470, #30186, #51678 ) ) REPRESENTATION_CONTEXT ( 'NONE', 'WORKASPACE' ) );
#55585 = AXIS2_PLACEMENT_3D ( 'NONE', #58998, #26617, #42190 ) ;
#55586 = SURFACE_SIDE_STYLE ('',( #11288 ) ) ;
#55587 = CARTESIAN_POINT ( 'NONE',  ( 6.062177826491067734, 2.500000000000000000, 3.500000000000000000 ) ) ;
#55588 = CARTESIAN_POINT ( 'NONE',  ( -166.9429263765337907, 0.000000000000000000, 9.524999999999991473 ) ) ;
#55589 = DIRECTION ( 'NONE',  ( 0.000000000000000000, -1.000000000000000000, 0.000000000000000000 ) ) ;
#55590 =( LENGTH_UNIT ( ) NAMED_UNIT ( * ) SI_UNIT ( .MILLI., .METRE. ) );
#55591 = ORIENTED_EDGE ( 'NONE', *, *, #39993, .F. ) ;
#55592 = CARTESIAN_POINT ( 'NONE',  ( -138.6550000000000011, -7.632228543268600340, -2.479861379858950166 ) ) ;
#55593 = ORIENTED_EDGE ( 'NONE', *, *, #46837, .F. ) ;
#55594 = CIRCLE ( 'NONE', #19640, 4.999999999999997335 ) ;
#55595 = EDGE_CURVE ( 'NONE', #63408, #63380, #30700, .T. ) ;
#55596 = EDGE_LOOP ( 'NONE', ( #63590, #14898, #7045, #7245 ) ) ;
#55597 = CYLINDRICAL_SURFACE ( 'NONE', #30138, 5.000000000000000000 ) ;
#55598 = FILL_AREA_STYLE ('',( #1379 ) ) ;
#55599 = ORIENTED_EDGE ( 'NONE', *, *, #40859, .F. ) ;
#55600 = PRESENTATION_LAYER_ASSIGNMENT (  '', '', ( #7144 ) ) ;
#55601 = AXIS2_PLACEMENT_3D ( 'NONE', #62506, #24180, #40386 ) ;
#55602 = DIRECTION ( 'NONE',  ( 0.000000000000000000, 0.000000000000000000, 1.000000000000000000 ) ) ;
#55603 = EDGE_CURVE ( 'NONE', #62878, #36379, #3037, .T. ) ;
#55604 = DIRECTION ( 'NONE',  ( -0.000000000000000000, 1.000000000000000000, -0.000000000000000000 ) ) ;
#55605 = CARTESIAN_POINT ( 'NONE',  ( 10.01517768586949231, 132.6949999999999363, 1.839758294383810543E-15 ) ) ;
#55606 = DIRECTION ( 'NONE',  ( -0.000000000000000000, -1.000000000000000000, -0.000000000000000000 ) ) ;
#55607 = ORIENTED_EDGE ( 'NONE', *, *, #34052, .T. ) ;
#55608 =( LENGTH_UNIT ( ) NAMED_UNIT ( * ) SI_UNIT ( .MILLI., .METRE. ) );
#55610 = EDGE_CURVE ( 'NONE', #15954, #66584, #9399, .T. ) ;
#55609 = CARTESIAN_POINT ( 'NONE',  ( 10.01517768586949408, 139.8050000000000068, 1.839758294383810543E-15 ) ) ;
#55611 = CARTESIAN_POINT ( 'NONE',  ( -55.70499999999997698, 2.607480562269072433, 8.024999999999991473 ) ) ;
#55612 = CARTESIAN_POINT ( 'NONE',  ( 40.99999999999998579, 107.7459666864129275, -3.076101031310279232 ) ) ;
#55613 = ORIENTED_EDGE ( 'NONE', *, *, #39590, .T. ) ;
#55614 = CARTESIAN_POINT ( 'NONE',  ( -7.632228543268607446, 111.5429263765338135, -2.479861379858953718 ) ) ;
#55615 = DIRECTION ( 'NONE',  ( -1.000000000000000000, -0.000000000000000000, -0.000000000000000000 ) ) ;
#55616 = FILL_AREA_STYLE_COLOUR ( '', #2922 ) ;
#55617 = EDGE_CURVE ( 'NONE', #25644, #44875, #55871, .T. ) ;
#55618 = FILL_AREA_STYLE ('',( #7759 ) ) ;
#55619 = PRESENTATION_LAYER_ASSIGNMENT (  '', '', ( #10727 ) ) ;
#55620 = DIRECTION ( 'NONE',  ( 0.000000000000000000, -0.000000000000000000, -1.000000000000000000 ) ) ;
#55621 = EDGE_LOOP ( 'NONE', ( #66602, #4842, #3175, #18251, #33464, #35414, #31611, #24958 ) ) ;
#55622 = AXIS2_PLACEMENT_3D ( 'NONE', #1026, #49002, #43399 ) ;
#55623 = DIRECTION ( 'NONE',  ( 1.000000000000000000, 0.000000000000000000, 0.000000000000000000 ) ) ;
#55624 = ORIENTED_EDGE ( 'NONE', *, *, #44074, .T. ) ;
#55625 = DIRECTION ( 'NONE',  ( 0.000000000000000000, 0.000000000000000000, 1.000000000000000000 ) ) ;
#55626 = DIRECTION ( 'NONE',  ( 1.000000000000000000, -0.000000000000000000, -0.000000000000000000 ) ) ;
#55627 = CYLINDRICAL_SURFACE ( 'NONE', #272, 0.5000000000000004441 ) ;
#55628 = CARTESIAN_POINT ( 'NONE',  ( -166.5550000000000068, 0.000000000000000000, 8.024999999999991473 ) ) ;
#55629 = ORIENTED_EDGE ( 'NONE', *, *, #28737, .T. ) ;
#55630 = DIRECTION ( 'NONE',  ( 0.000000000000000000, -1.000000000000000000, 0.000000000000000000 ) ) ;
#55631 = VECTOR ( 'NONE', #4984, 1000.000000000000000 ) ;
#55632 = AXIS2_PLACEMENT_3D ( 'NONE', #18471, #55753, #49449 ) ;
#55633 = DIRECTION ( 'NONE',  ( 0.000000000000000000, 0.000000000000000000, 1.000000000000000000 ) ) ;
#55634 = SURFACE_STYLE_USAGE ( .BOTH. , #8145 ) ;
#55635 = SURFACE_SIDE_STYLE ('',( #66171 ) ) ;
#55636 = EDGE_LOOP ( 'NONE', ( #11118, #17168, #6772, #1549 ) ) ;
#55637 = ORIENTED_EDGE ( 'NONE', *, *, #53401, .F. ) ;
#55638 = CARTESIAN_POINT ( 'NONE',  ( 57.00000000000000000, 16.00000000000000000, -47.50402776293824303 ) ) ;
#55639 = CARTESIAN_POINT ( 'NONE',  ( -45.90208486430518775, 9.410172310978731858, -3.203880287027109919 ) ) ;
#55640 = CARTESIAN_POINT ( 'NONE',  ( -73.10499999999996135, -6.826472737025115478, 4.959722759717900331 ) ) ;
#55641 = VERTEX_POINT ( 'NONE', #51639 ) ;
#55642 = CARTESIAN_POINT ( 'NONE',  ( 0.000000000000000000, 87.30187232391182306, 0.000000000000000000 ) ) ;
#55643 = MECHANICAL_DESIGN_GEOMETRIC_PRESENTATION_REPRESENTATION (  '', ( #46710 ), #30922 ) ;
#55644 = PRESENTATION_LAYER_ASSIGNMENT (  '', '', ( #68015 ) ) ;
#55645 = CYLINDRICAL_SURFACE ( 'NONE', #47185, 0.2500000000000002220 ) ;
#55646 = ORIENTED_EDGE ( 'NONE', *, *, #12640, .F. ) ;
#55647 = LINE ( 'NONE', #39157, #15986 ) ;
#55649 = PRESENTATION_STYLE_ASSIGNMENT (( #60909 ) ) ;
#55648 = CARTESIAN_POINT ( 'NONE',  ( 23.21231517720797655, 117.4999999999999716, 7.000000000000000000 ) ) ;
#55650 = COLOUR_RGB ( '', 0.72549020, 0.75294118, 0.79215686) ;
#55651 = CARTESIAN_POINT ( 'NONE',  ( -1.166476076187854022E-15, 140.9449999999999932, 9.525000000000000355 ) ) ;
#55652 = CARTESIAN_POINT ( 'NONE',  ( -106.3449999999999989, 7.632228543268599452, -2.479861379858951942 ) ) ;
#55653 = AXIS2_PLACEMENT_3D ( 'NONE', #56459, #13193, #13543 ) ;
#55654 = AXIS2_PLACEMENT_3D ( 'NONE', #14356, #41835, #20330 ) ;
#55655 = DIRECTION ( 'NONE',  ( 1.000000000000000000, -0.000000000000000000, -0.000000000000000000 ) ) ;
#55657 = DIRECTION ( 'NONE',  ( 0.000000000000000000, 0.000000000000000000, 1.000000000000000000 ) ) ;
#55656 = CARTESIAN_POINT ( 'NONE',  ( -97.25707362346618368, 5.598654528085800663, -7.705886871421367523 ) ) ;
#55658 = CARTESIAN_POINT ( 'NONE',  ( -157.7929263765337566, -3.094860106618429807, 9.524999999999991473 ) ) ;
#55659 = SURFACE_STYLE_FILL_AREA ( #33176 ) ;
#55660 = CARTESIAN_POINT ( 'NONE',  ( -167.6949999999999363, -8.437984349512085203, 5.166775262442717831E-16 ) ) ;
#55661 = CARTESIAN_POINT ( 'NONE',  ( -156.0570736234661808, 0.000000000000000000, 9.524999999999991473 ) ) ;
#55662 = AXIS2_PLACEMENT_3D ( 'NONE', #60442, #49926, #55526 ) ;
#55663 = EDGE_CURVE ( 'NONE', #8600, #5084, #2338, .T. ) ;
#55664 = ORIENTED_EDGE ( 'NONE', *, *, #65749, .F. ) ;
#55665 = DIRECTION ( 'NONE',  ( -1.000000000000000000, 0.000000000000000000, 0.000000000000000000 ) ) ;
#55666 = ORIENTED_EDGE ( 'NONE', *, *, #33102, .F. ) ;
#55667 = CARTESIAN_POINT ( 'NONE',  ( -68.09292637653379643, 3.094860106618433360, 9.524999999999991473 ) ) ;
#55669 = ADVANCED_FACE ( 'NONE', ( #62525 ), #27486, .F. ) ;
#55668 = DIRECTION ( 'NONE',  ( -0.000000000000000000, -1.000000000000000000, -0.000000000000000000 ) ) ;
#55670 = EDGE_CURVE ( 'NONE', #65056, #19539, #31903, .T. ) ;
#55671 = AXIS2_PLACEMENT_3D ( 'NONE', #4318, #63098, #26494 ) ;
#55672 = CARTESIAN_POINT ( 'NONE',  ( 60.00000000000000000, 1.797044900979284448E-15, -12.00000000000000000 ) ) ;
#55673 = EDGE_CURVE ( 'NONE', #28720, #41266, #42868, .T. ) ;
#55674 = CARTESIAN_POINT ( 'NONE',  ( -6.826472737025120807, 143.1070736234661638, 4.959722759717906548 ) ) ;
#55675 = ORIENTED_EDGE ( 'NONE', *, *, #54774, .F. ) ;
#55676 = CARTESIAN_POINT ( 'NONE',  ( -170.3049999999999784, 8.437984349512086979, -1.550032578732815448E-15 ) ) ;
#55677 = EDGE_CURVE ( 'NONE', #33374, #27703, #36880, .T. ) ;
#55678 = ORIENTED_EDGE ( 'NONE', *, *, #68550, .F. ) ;
#55679 = SURFACE_STYLE_FILL_AREA ( #13102 ) ;
#55680 = EDGE_CURVE ( 'NONE', #31059, #26061, #1351, .T. ) ;
#55681 = CARTESIAN_POINT ( 'NONE',  ( 57.00000000000000000, 14.00000000000000000, -60.00402776293827145 ) ) ;
#55682 = EDGE_CURVE ( 'NONE', #69054, #14523, #15757, .T. ) ;
#55683 = PLANE ( 'NONE',  #62349 ) ;
#55684 = CARTESIAN_POINT ( 'NONE',  ( 2.607480562269076430, 147.9070736234661467, -8.025000000000000355 ) ) ;
#55685 = COLOUR_RGB ( '', 0.72549020, 0.75294118, 0.79215686) ;
#55686 = ORIENTED_EDGE ( 'NONE', *, *, #4793, .F. ) ;
#55687 = FACE_OUTER_BOUND ( 'NONE', #63179, .T. ) ;
#55689 = ADVANCED_FACE ( 'NONE', ( #53701 ), #5488, .T. ) ;
#55688 = CARTESIAN_POINT ( 'NONE',  ( -8.102448949553179958, 111.0049999999999955, -5.886773742842749790 ) ) ;
#55690 = CARTESIAN_POINT ( 'NONE',  ( -84.50499999999998124, -6.826472737025113702, -4.959722759717900331 ) ) ;
#55691 = CARTESIAN_POINT ( 'NONE',  ( -6.826472737025120807, 122.1070736234661638, 4.959722759717906548 ) ) ;
#55692 = CARTESIAN_POINT ( 'NONE',  ( -8.102448949553181734, 132.6050000000000182, 5.886773742842747126 ) ) ;
#55693 = CARTESIAN_POINT ( 'NONE',  ( -114.4429263765338050, -1.166476076187852838E-15, -9.524999999999991473 ) ) ;
#55694 = FILL_AREA_STYLE_COLOUR ( '', #6280 ) ;
#55695 = TOROIDAL_SURFACE ( 'NONE', #7401, 13.49999999999999822, 0.5000000000000000000 ) ;
#55696 = CARTESIAN_POINT ( 'NONE',  ( -73.10707362346616378, 8.102448949553172852, -5.886773742842744461 ) ) ;
#55697 = PLANE ( 'NONE',  #69241 ) ;
#55698 = CARTESIAN_POINT ( 'NONE',  ( -23.21231517720797655, 113.4999999999999858, 10.00000000000000000 ) ) ;
#55699 = MECHANICAL_DESIGN_GEOMETRIC_PRESENTATION_REPRESENTATION (  '', ( #36677 ), #46824 ) ;
#55700 = ORIENTED_EDGE ( 'NONE', *, *, #69589, .F. ) ;
#55701 = VECTOR ( 'NONE', #53105, 1000.000000000000000 ) ;
#55702 = CYLINDRICAL_SURFACE ( 'NONE', #42978, 0.5000000000000000000 ) ;
#55703 = SURFACE_SIDE_STYLE ('',( #50097 ) ) ;
#55704 = CARTESIAN_POINT ( 'NONE',  ( -53.69499999999999318, -8.437984349512085203, 5.166775262442717831E-16 ) ) ;
#55705 = VERTEX_POINT ( 'NONE', #11493 ) ;
#55706 = DIRECTION ( 'NONE',  ( 1.000000000000000000, -0.000000000000000000, -0.000000000000000000 ) ) ;
#55707 = CARTESIAN_POINT ( 'NONE',  ( -45.90418876431856887, 9.387410786201595414, -6.121260521433894652 ) ) ;
#55708 = CARTESIAN_POINT ( 'NONE',  ( 7.794228634059946259, 2.500000000000000000, -4.500000000000001776 ) ) ;
#55709 = ORIENTED_EDGE ( 'NONE', *, *, #3191, .T. ) ;
#55710 = CARTESIAN_POINT ( 'NONE',  ( -51.22377615987210930, -10.33468447027765791, 4.122506284637720064 ) ) ;
#55711 = CARTESIAN_POINT ( 'NONE',  ( -52.64499999999999602, 4.716976649647091513, -6.492361379858946790 ) ) ;
#55712 = SURFACE_SIDE_STYLE ('',( #62011 ) ) ;
#55713 = EDGE_LOOP ( 'NONE', ( #43913, #28094, #60768, #35578 ) ) ;
#55714 = CIRCLE ( 'NONE', #59116, 0.5000000000000004441 ) ;
#55715 = CARTESIAN_POINT ( 'NONE',  ( -74.08601561514839773, 9.424559774107397203, 6.049830996511062153 ) ) ;
#55716 = CARTESIAN_POINT ( 'NONE',  ( -106.5549999999999784, 0.000000000000000000, 8.024999999999991473 ) ) ;
#55717 = ORIENTED_EDGE ( 'NONE', *, *, #67741, .F. ) ;
#55718 = FILL_AREA_STYLE ('',( #60976 ) ) ;
#55719 = CARTESIAN_POINT ( 'NONE',  ( 0.000000000000000000, 36.75000000000000000, 3.750000000000000000 ) ) ;
#55720 = STYLED_ITEM ( 'NONE', ( #40875 ), #1868 ) ;
#55721 = CARTESIAN_POINT ( 'NONE',  ( -149.6070736234661638, -8.102448949553172852, 5.886773742842742685 ) ) ;
#55722 = CARTESIAN_POINT ( 'NONE',  ( -59.75707362346617657, -5.598654528085801552, 7.705886871421367523 ) ) ;
#55723 = CARTESIAN_POINT ( 'NONE',  ( -8.102448949553179958, 146.4949999999999761, 5.886773742842747126 ) ) ;
#55724 = MECHANICAL_DESIGN_GEOMETRIC_PRESENTATION_REPRESENTATION (  '', ( #28735 ), #10782 ) ;
#55725 = CARTESIAN_POINT ( 'NONE',  ( -82.40707362346617515, 3.094860106618428031, -9.524999999999993250 ) ) ;
#55726 = ADVANCED_FACE ( 'NONE', ( #55079 ), #57691, .T. ) ;
#55727 = SURFACE_STYLE_FILL_AREA ( #50802 ) ;
#55728 = DIRECTION ( 'NONE',  ( -1.189524669241239115E-16, -1.000000000000000000, -0.000000000000000000 ) ) ;
#55729 = ORIENTED_EDGE ( 'NONE', *, *, #17037, .T. ) ;
#55730 = DIRECTION ( 'NONE',  ( 0.000000000000000000, 1.000000000000000000, 0.000000000000000000 ) ) ;
#55732 =( NAMED_UNIT ( * ) PLANE_ANGLE_UNIT ( ) SI_UNIT ( $, .RADIAN. ) );
#55731 = CARTESIAN_POINT ( 'NONE',  ( -15.00000000000000000, -12.00000000000000000, -5.000000000000000000 ) ) ;
#55733 = CARTESIAN_POINT ( 'NONE',  ( -132.6550000000000011, -7.632228543268600340, -2.479861379858950166 ) ) ;
#55734 = CARTESIAN_POINT ( 'NONE',  ( 93.00000000000000000, 13.00000000000000178, 0.000000000000000000 ) ) ;
#55735 = DIRECTION ( 'NONE',  ( 0.000000000000000000, 0.000000000000000000, -1.000000000000000000 ) ) ;
#55736 = CARTESIAN_POINT ( 'NONE',  ( 3.094860106618435136, 112.2949999999999733, -9.525000000000000355 ) ) ;
#55737 = CARTESIAN_POINT ( 'NONE',  ( -137.9950000000000045, -6.826472737025115478, 4.959722759717900331 ) ) ;
#55738 = CARTESIAN_POINT ( 'NONE',  ( -125.3949999999999818, -6.826472737025113702, -4.959722759717900331 ) ) ;
#55739 = CARTESIAN_POINT ( 'NONE',  ( 13.75000000000000533, 30.99999999999999289, -3.750000000000000000 ) ) ;
#55740 = EDGE_LOOP ( 'NONE', ( #30385, #10453, #21605, #33008 ) ) ;
#55741 = LINE ( 'NONE', #18791, #41492 ) ;
#55742 = CIRCLE ( 'NONE', #46814, 0.2500000000000002220 ) ;
#55743 = FILL_AREA_STYLE_COLOUR ( '', #4209 ) ;
#55744 = CARTESIAN_POINT ( 'NONE',  ( -120.7429263765338021, -5.598654528085803328, -7.705886871421366635 ) ) ;
#55745 = CARTESIAN_POINT ( 'NONE',  ( -179.8429263765338249, 9.058813317711329915, -2.943386871421373119 ) ) ;
#55746 =( NAMED_UNIT ( * ) PLANE_ANGLE_UNIT ( ) SI_UNIT ( $, .RADIAN. ) );
#55747 = CARTESIAN_POINT ( 'NONE',  ( -51.59499999999997755, 2.607480562269073321, 8.024999999999991473 ) ) ;
#55748 = STYLED_ITEM ( 'NONE', ( #50266 ), #64573 ) ;
#55749 = B_SPLINE_CURVE_WITH_KNOTS ( 'NONE', 3,
 ( #48927, #22144, #32341, #21103, #625, #48222, #43988, #11580 ),
 .UNSPECIFIED., .F., .F.,
 ( 4, 2, 2, 4 ),
 ( 2.544313220903533887E-07, 0.002693395767724532288, 0.004039966435925753697, 0.005386537104126974673 ),
 .UNSPECIFIED. ) ;
#55750 = EDGE_CURVE ( 'NONE', #25818, #51313, #66923, .T. ) ;
#55751 = FACE_OUTER_BOUND ( 'NONE', #908, .T. ) ;
#55752 = COLOUR_RGB ( '', 0.66274510, 0.83137255, 0.94901961) ;
#55753 = DIRECTION ( 'NONE',  ( -0.000000000000000000, -0.000000000000000000, -1.000000000000000000 ) ) ;
#55754 = CARTESIAN_POINT ( 'NONE',  ( -72.50000000000001421, 13.41640786499872284, -10.00000000000000000 ) ) ;
#55755 = PRODUCT_DEFINITION_CONTEXT ( 'detailed design', #40642, 'design' ) ;
#55757 = CARTESIAN_POINT ( 'NONE',  ( -92.54292637653379927, 9.058813317711329915, 2.943386871421369566 ) ) ;
#55756 =( BOUNDED_CURVE ( )  B_SPLINE_CURVE ( 3, ( #25248, #46766, #11495, #43221 ),
 .UNSPECIFIED., .F., .F. ) 
 B_SPLINE_CURVE_WITH_KNOTS ( ( 4, 4 ),
 ( 0.000000000000000000, 1.570796326794896558 ),
 .UNSPECIFIED. ) 
 CURVE ( )  GEOMETRIC_REPRESENTATION_ITEM ( )  RATIONAL_B_SPLINE_CURVE ( ( 1.000000000000000000, 0.8047378541243649375, 0.8047378541243649375, 1.000000000000000000 ) ) 
 REPRESENTATION_ITEM ( '' )  );
#55758 = SHAPE_DEFINITION_REPRESENTATION ( #37285, #60355 ) ;
#55760 = EDGE_CURVE ( 'NONE', #23764, #40740, #52141, .T. ) ;
#55759 = CARTESIAN_POINT ( 'NONE',  ( 74.49999999999998579, 119.9999999999997584, -10.00000000000000000 ) ) ;
#55761 = CARTESIAN_POINT ( 'NONE',  ( -40.78947369313011251, 108.1536491435770131, 3.152202064295502648 ) ) ;
#55762 = CIRCLE ( 'NONE', #46835, 1.499999999999997780 ) ;
#55763 = ORIENTED_EDGE ( 'NONE', *, *, #55750, .T. ) ;
#55764 = FACE_OUTER_BOUND ( 'NONE', #48427, .T. ) ;
#55765 = ADVANCED_FACE ( 'NONE', ( #39297 ), #44593, .T. ) ;
#55766 = CARTESIAN_POINT ( 'NONE',  ( 44.25000000000000000, 21.74999999999998579, 3.750000000000000000 ) ) ;
#55767 = ORIENTED_EDGE ( 'NONE', *, *, #7292, .F. ) ;
#55768 = CARTESIAN_POINT ( 'NONE',  ( -63.89292637653380780, -8.102448949553174629, -5.886773742842741797 ) ) ;
#55769 = CARTESIAN_POINT ( 'NONE',  ( -6.826472737025120807, 121.5070736234661410, -4.959722759717907437 ) ) ;
#55771 = EDGE_CURVE ( 'NONE', #14638, #44423, #34128, .T. ) ;
#55770 = SURFACE_SIDE_STYLE ('',( #50165 ) ) ;
#55772 = CARTESIAN_POINT ( 'NONE',  ( 75.00000000000000000, 19.44429231213349496, -6.999999999972110309 ) ) ;
#55773 = SURFACE_STYLE_USAGE ( .BOTH. , #65969 ) ;
#55774 = EDGE_LOOP ( 'NONE', ( #32168, #59044, #45087, #52237, #25058, #28314, #66056, #60068 ) ) ;
#55775 = CARTESIAN_POINT ( 'NONE',  ( -15.75000000000000000, -0.9999999999999995559, 19.00000000000000000 ) ) ;
#55776 = CARTESIAN_POINT ( 'NONE',  ( -13.23915246117191025, 52.65078610323165265, -2.000000000000000000 ) ) ;
#55777 = CARTESIAN_POINT ( 'NONE',  ( 30.99999999999999289, 0.000000000000000000, -24.00402776293822171 ) ) ;
#55778 = SURFACE_SIDE_STYLE ('',( #55428 ) ) ;
#55779 = DIRECTION ( 'NONE',  ( 0.000000000000000000, 0.000000000000000000, 1.000000000000000000 ) ) ;
#55780 = CARTESIAN_POINT ( 'NONE',  ( -85.79499999999997328, 2.607480562269068880, -8.024999999999993250 ) ) ;
#55781 = ORIENTED_EDGE ( 'NONE', *, *, #44979, .F. ) ;
#55782 = CARTESIAN_POINT ( 'NONE',  ( -2.607480562269041791, 123.0929263765338106, -8.025000000000021672 ) ) ;
#55783 = CARTESIAN_POINT ( 'NONE',  ( 13.75000000000000533, 30.74999999999999289, 3.750000000000000000 ) ) ;
#55784 = SURFACE_STYLE_FILL_AREA ( #28686 ) ;
#55785 = ORIENTED_EDGE ( 'NONE', *, *, #28812, .F. ) ;
#55786 = DIRECTION ( 'NONE',  ( 1.000000000000000000, 0.000000000000000000, 0.000000000000000000 ) ) ;
#55787 = VERTEX_POINT ( 'NONE', #38623 ) ;
#55788 = EDGE_LOOP ( 'NONE', ( #38365, #12177, #9225, #6547 ) ) ;
#55789 = CARTESIAN_POINT ( 'NONE',  ( -138.2929263765344103, 3.094860106608815276, -9.525000000006976109 ) ) ;
#55790 = MECHANICAL_DESIGN_GEOMETRIC_PRESENTATION_REPRESENTATION (  '', ( #17619 ), #24316 ) ;
#55791 = FACE_OUTER_BOUND ( 'NONE', #52553, .T. ) ;
#55792 = CARTESIAN_POINT ( 'NONE',  ( -15.98999599679679839, 118.4999999999999716, -7.000000000000000000 ) ) ;
#55793 = CARTESIAN_POINT ( 'NONE',  ( 0.000000000000000000, 42.00000000000000000, -79.00402776293826435 ) ) ;
#55794 = CARTESIAN_POINT ( 'NONE',  ( -181.5570736234661808, -1.166476076187852838E-15, -9.524999999999991473 ) ) ;
#55795 = DIRECTION ( 'NONE',  ( -1.000000000000000000, -0.000000000000000000, -0.000000000000000000 ) ) ;
#55796 = CARTESIAN_POINT ( 'NONE',  ( 8.102448949553179958, 114.3949999999999676, 5.886773742842750679 ) ) ;
#55797 = CARTESIAN_POINT ( 'NONE',  ( -116.6070736234661638, -8.102448949553172852, 5.886773742842742685 ) ) ;
#55798 = EDGE_CURVE ( 'NONE', #44275, #34188, #49835, .T. ) ;
#55799 = DIRECTION ( 'NONE',  ( -1.000000000000000000, 0.000000000000000000, 0.000000000000000000 ) ) ;
#55800 = CARTESIAN_POINT ( 'NONE',  ( -85.10707362346616378, 8.102448949553172852, -5.886773742842744461 ) ) ;
#55801 = ORIENTED_EDGE ( 'NONE', *, *, #40214, .T. ) ;
#55802 = ADVANCED_FACE ( 'NONE', ( #54049 ), #65307, .F. ) ;
#55803 = CARTESIAN_POINT ( 'NONE',  ( -4.099639464710813641E-16, 42.24290439781479733, 45.14575947097794284 ) ) ;
#55804 = DIRECTION ( 'NONE',  ( 0.000000000000000000, 0.000000000000000000, 1.000000000000000000 ) ) ;
#55805 = DIRECTION ( 'NONE',  ( 0.000000000000000000, -1.000000000000000000, 0.000000000000000000 ) ) ;
#55807 = EDGE_LOOP ( 'NONE', ( #32963, #41708, #29453, #22376 ) ) ;
#55806 = PRESENTATION_LAYER_ASSIGNMENT (  '', '', ( #58041 ) ) ;
#55808 = CARTESIAN_POINT ( 'NONE',  ( -163.7049999999999841, 2.607480562269073321, 8.024999999999991473 ) ) ;
#55809 = CARTESIAN_POINT ( 'NONE',  ( 48.50000000000000000, 14.49137674618942562, 9.500000000000000000 ) ) ;
#55810 = CARTESIAN_POINT ( 'NONE',  ( -183.5631645208122791, -4.726186399133334604, -7.620781825058602799 ) ) ;
#55811 = CARTESIAN_POINT ( 'NONE',  ( -168.2950000000000159, -2.607480562269069768, 8.024999999999991473 ) ) ;
#55812 = CARTESIAN_POINT ( 'NONE',  ( -154.1949999999999648, 8.437984349512086979, -1.550032578732815448E-15 ) ) ;
#55813 = ORIENTED_EDGE ( 'NONE', *, *, #57041, .F. ) ;
#55814 = CARTESIAN_POINT ( 'NONE',  ( -7.794228634059953364, 4.500000000000004441, 0.000000000000000000 ) ) ;
#55815 = CARTESIAN_POINT ( 'NONE',  ( 45.00050070149898573, 10.00016690049882229, 3.905286714425231231 ) ) ;
#55816 = LINE ( 'NONE', #2278, #30477 ) ;
#55817 = CARTESIAN_POINT ( 'NONE',  ( -75.65499999999998693, -7.632228543268600340, -2.479861379858950166 ) ) ;
#55818 = CARTESIAN_POINT ( 'NONE',  ( -34.26930151262192936, -10.31448204818432579, 2.417974663400876079 ) ) ;
#55819 = CARTESIAN_POINT ( 'NONE',  ( -167.9929263765338305, 8.102448949553172852, -5.886773742842744461 ) ) ;
#55820 = EDGE_CURVE ( 'NONE', #16782, #16768, #2598, .T. ) ;
#55821 = CARTESIAN_POINT ( 'NONE',  ( -70.79499999999998749, 2.607480562269069324, -8.024999999999993250 ) ) ;
#55822 = EDGE_CURVE ( 'NONE', #53024, #47418, #16470, .T. ) ;
#55823 = CARTESIAN_POINT ( 'NONE',  ( 9.058813317711338797, 148.9550000000000125, -2.943386871421372675 ) ) ;
#55824 = FILL_AREA_STYLE ('',( #39332 ) ) ;
#55825 = UNCERTAINTY_MEASURE_WITH_UNIT (LENGTH_MEASURE( 1.000000000000000082E-05 ), #7206, 'distance_accuracy_value', 'NONE');
#55826 = CARTESIAN_POINT ( 'NONE',  ( -1.018511207705687038E-14, 42.00000000000000000, 28.38386403503541899 ) ) ;
#55827 = EDGE_CURVE ( 'NONE', #52121, #7949, #56572, .T. ) ;
#55828 = DIRECTION ( 'NONE',  ( -0.000000000000000000, 0.000000000000000000, -1.000000000000000000 ) ) ;
#55829 = CARTESIAN_POINT ( 'NONE',  ( 9.568252947146927312, 1.861307952554195566, -1.427299755870872433 ) ) ;
#55830 = ADVANCED_FACE ( 'NONE', ( #59671 ), #39739, .T. ) ;
#55831 = DIRECTION ( 'NONE',  ( -0.000000000000000000, -1.000000000000000000, -0.000000000000000000 ) ) ;
#55832 = TOROIDAL_SURFACE ( 'NONE', #62608, 12.50000000000000000, 0.5000000000000000000 ) ;
#55833 = FACE_OUTER_BOUND ( 'NONE', #8129, .T. ) ;
#55835 = ADVANCED_FACE ( 'NONE', ( #61732 ), #62094, .T. ) ;
#55834 = AXIS2_PLACEMENT_3D ( 'NONE', #12506, #16793, #27637 ) ;
#55836 = CARTESIAN_POINT ( 'NONE',  ( -34.99999999999992184, 109.9999999999999858, 9.500000000000000000 ) ) ;
#55837 = ORIENTED_EDGE ( 'NONE', *, *, #41366, .T. ) ;
#55838 = ORIENTED_EDGE ( 'NONE', *, *, #23669, .F. ) ;
#55839 = DIRECTION ( 'NONE',  ( 0.000000000000000000, 0.000000000000000000, 1.000000000000000000 ) ) ;
#55840 = CARTESIAN_POINT ( 'NONE',  ( -156.2929263765341545, 3.094860106612411954, -9.525000000004366640 ) ) ;
#55841 =( BOUNDED_CURVE ( )  B_SPLINE_CURVE ( 3, ( #63866, #20263, #15707, #20622 ),
 .UNSPECIFIED., .F., .F. ) 
 B_SPLINE_CURVE_WITH_KNOTS ( ( 4, 4 ),
 ( 3.141592653589794004, 4.712388980384689674 ),
 .UNSPECIFIED. ) 
 CURVE ( )  GEOMETRIC_REPRESENTATION_ITEM ( )  RATIONAL_B_SPLINE_CURVE ( ( 1.000000000000000000, 0.8047378541243652705, 0.8047378541243652705, 1.000000000000000000 ) ) 
 REPRESENTATION_ITEM ( '' )  );
#55842 = ADVANCED_FACE ( 'NONE', ( #8314 ), #39793, .T. ) ;
#55843 = CARTESIAN_POINT ( 'NONE',  ( -45.00000000000000711, 8.747703778475440117, 6.883446876413755966 ) ) ;
#55844 = DIRECTION ( 'NONE',  ( 0.000000000000000000, 0.000000000000000000, 1.000000000000000000 ) ) ;
#55845 = CARTESIAN_POINT ( 'NONE',  ( 1.802043943559354711, 2.359472279213376211, 9.000000000000003553 ) ) ;
#55846 = CARTESIAN_POINT ( 'NONE',  ( 26.00000000000001776, -3.148064030671221758, 29.68999999999999417 ) ) ;
#55847 = EDGE_LOOP ( 'NONE', ( #65889, #54148, #50720, #23167 ) ) ;
#55848 = VERTEX_POINT ( 'NONE', #12874 ) ;
#55849 = VECTOR ( 'NONE', #61234, 1000.000000000000114 ) ;
#55850 = DIRECTION ( 'NONE',  ( 0.000000000000000000, 0.000000000000000000, -1.000000000000000000 ) ) ;
#55851 = ORIENTED_EDGE ( 'NONE', *, *, #36509, .T. ) ;
#55852 = CARTESIAN_POINT ( 'NONE',  ( -3.094860106618434248, 111.9050000000000011, 9.525000000000000355 ) ) ;
#55853 = CARTESIAN_POINT ( 'NONE',  ( -34.99999999999992895, 113.4999999999999858, 7.500000000000000000 ) ) ;
#55854 = ORIENTED_EDGE ( 'NONE', *, *, #40681, .F. ) ;
#55855 = DIRECTION ( 'NONE',  ( 1.000000000000000000, 0.000000000000000000, 0.000000000000000000 ) ) ;
#55856 = FACE_OUTER_BOUND ( 'NONE', #10982, .T. ) ;
#55857 = CARTESIAN_POINT ( 'NONE',  ( -121.3449999999999989, 7.632228543268599452, -2.479861379858951942 ) ) ;
#55858 = EDGE_LOOP ( 'NONE', ( #15578, #27471, #58888, #23245 ) ) ;
#55859 = ORIENTED_EDGE ( 'NONE', *, *, #12000, .T. ) ;
#55860 = CARTESIAN_POINT ( 'NONE',  ( -74.08452722063036333, 9.430195807687214327, -6.039758700367572786 ) ) ;
#55861 = DIRECTION ( 'NONE',  ( 0.000000000000000000, 1.000000000000000000, -0.000000000000000000 ) ) ;
#55862 = CARTESIAN_POINT ( 'NONE',  ( -10.16352198286304009, -11.93264351171969118, -1.310612615857368546 ) ) ;
#55863 = CARTESIAN_POINT ( 'NONE',  ( 0.000000000000000000, 0.000000000000000000, 42.50000000000000000 ) ) ;
#55864 = VERTEX_POINT ( 'NONE', #67740 ) ;
#55865 = CARTESIAN_POINT ( 'NONE',  ( -4.716976649647097730, 141.2429263765338305, -6.492361379858953896 ) ) ;
#55866 = FACE_OUTER_BOUND ( 'NONE', #39924, .T. ) ;
#55867 = DIRECTION ( 'NONE',  ( -1.734723475976805517E-15, 0.000000000000000000, -1.000000000000000000 ) ) ;
#55868 =( LENGTH_UNIT ( ) NAMED_UNIT ( * ) SI_UNIT ( .MILLI., .METRE. ) );
#55869 = CARTESIAN_POINT ( 'NONE',  ( 6.062177826491068622, -2.500000000000000000, -3.500000000000001332 ) ) ;
#55870 = ORIENTED_EDGE ( 'NONE', *, *, #32538, .F. ) ;
#55871 = LINE ( 'NONE', #40765, #68945 ) ;
#55872 = ORIENTED_EDGE ( 'NONE', *, *, #60811, .F. ) ;
#55873 = CARTESIAN_POINT ( 'NONE',  ( -24.00000000000000000, 1.000000000000000000, -3.000000000000000000 ) ) ;
#55874 = CARTESIAN_POINT ( 'NONE',  ( -7.632228543268608334, 139.9570736234661581, 2.479861379858952830 ) ) ;
#55875 = DIRECTION ( 'NONE',  ( 1.000000000000000000, 0.000000000000000000, 0.000000000000000000 ) ) ;
#55876 = CARTESIAN_POINT ( 'NONE',  ( -8.246138225238285102, -3.717269627651450303, -1.631385456411781861E-15 ) ) ;
#55877 = CARTESIAN_POINT ( 'NONE',  ( -136.8550000000000182, 4.716976649647094177, 6.492361379858945902 ) ) ;
#55878 = SURFACE_STYLE_USAGE ( .BOTH. , #17905 ) ;
#55879 = FILL_AREA_STYLE_COLOUR ( '', #48556 ) ;
#55880 = ORIENTED_EDGE ( 'NONE', *, *, #45184, .T. ) ;
#55881 = EDGE_CURVE ( 'NONE', #35167, #61482, #40680, .T. ) ;
#55882 = CARTESIAN_POINT ( 'NONE',  ( 6.000000000000017764, 16.44305403005404287, -2.635024667321593109E-15 ) ) ;
#55883 = CARTESIAN_POINT ( 'NONE',  ( -0.7087670488515479539, -2.466410156631316131, 7.000000000000000000 ) ) ;
#55884 = EDGE_LOOP ( 'NONE', ( #63252, #49947, #6603, #56032 ) ) ;
#55885 = PRESENTATION_LAYER_ASSIGNMENT (  '', '', ( #58164 ) ) ;
#55886 = ORIENTED_EDGE ( 'NONE', *, *, #59422, .T. ) ;
#55887 = CARTESIAN_POINT ( 'NONE',  ( 17.15973193263811680, -3.000000000000000000, -2.000000000000000000 ) ) ;
#55888 = VECTOR ( 'NONE', #52019, 1000.000000000000000 ) ;
#55889 = CARTESIAN_POINT ( 'NONE',  ( -30.01048380477678990, -8.499999999999912959, -0.6003161102128471427 ) ) ;
#55890 = SURFACE_STYLE_USAGE ( .BOTH. , #33400 ) ;
#55891 = CARTESIAN_POINT ( 'NONE',  ( -6.588738478070744975, 51.73049953470015083, 7.044582342571018785 ) ) ;
#55892 = ORIENTED_EDGE ( 'NONE', *, *, #37380, .F. ) ;
#55893 = CARTESIAN_POINT ( 'NONE',  ( 0.000000000000000000, 0.000000000000000000, 1.000000000000000000 ) ) ;
#55894 = FILL_AREA_STYLE ('',( #44698 ) ) ;
#55896 = AXIS2_PLACEMENT_3D ( 'NONE', #26370, #57708, #47192 ) ;
#55895 = CARTESIAN_POINT ( 'NONE',  ( 4.000000000000030198, 34.36176364315826248, 80.00402776293826435 ) ) ;
#55897 = CARTESIAN_POINT ( 'NONE',  ( -7.511572993685801073E-16, 7.000000000000000888, 0.000000000000000000 ) ) ;
#55898 = CARTESIAN_POINT ( 'NONE',  ( 22.99999999999995026, 5.000000000000000000, -32.00402776293824303 ) ) ;
#55899 = CARTESIAN_POINT ( 'NONE',  ( -177.6570736234662036, 9.058813317711329915, 2.943386871421369566 ) ) ;
#55900 = VERTEX_POINT ( 'NONE', #46321 ) ;
#55901 = CARTESIAN_POINT ( 'NONE',  ( -74.96084131305691756, 35.58445536041309509, -9.699738583933323000 ) ) ;
#55902 = ADVANCED_FACE ( 'NONE', ( #34666 ), #24127, .F. ) ;
#55903 = DIRECTION ( 'NONE',  ( -0.000000000000000000, -0.000000000000000000, 1.000000000000000000 ) ) ;
#55904 = FILL_AREA_STYLE_COLOUR ( '', #53999 ) ;
#55905 = CARTESIAN_POINT ( 'NONE',  ( -98.90500000000000114, 2.607480562269068880, -8.024999999999993250 ) ) ;
#55906 = DIRECTION ( 'NONE',  ( 0.000000000000000000, 0.000000000000000000, 1.000000000000000000 ) ) ;
#55907 = VECTOR ( 'NONE', #62951, 1000.000000000000114 ) ;
#55908 = EDGE_CURVE ( 'NONE', #3770, #23886, #66726, .T. ) ;
#55909 = CARTESIAN_POINT ( 'NONE',  ( -96.74499999999999034, 4.716976649647094177, 6.492361379858945902 ) ) ;
#55910 = ADVANCED_FACE ( 'NONE', ( #45633 ), #67050, .T. ) ;
#55911 = CARTESIAN_POINT ( 'NONE',  ( 3.094860106618435136, 113.4050000000000011, -9.525000000000000355 ) ) ;
#55912 = CARTESIAN_POINT ( 'NONE',  ( -82.19499999999999318, 8.437984349512085203, -1.550032578732815448E-15 ) ) ;
#55913 = DIRECTION ( 'NONE',  ( -1.000000000000000000, 0.000000000000000000, 0.000000000000000000 ) ) ;
#55914 = CARTESIAN_POINT ( 'NONE',  ( -57.11974195712093660, -8.499999999999992895, 0.06931351858119066955 ) ) ;
#55915 = UNCERTAINTY_MEASURE_WITH_UNIT (LENGTH_MEASURE( 1.000000000000000082E-05 ), #24364, 'distance_accuracy_value', 'NONE');
#55916 = DIRECTION ( 'NONE',  ( -1.000000000000000000, 0.000000000000000000, 0.000000000000000000 ) ) ;
#55917 = ORIENTED_EDGE ( 'NONE', *, *, #44458, .T. ) ;
#55918 = ADVANCED_FACE ( 'NONE', ( #42789 ), #48788, .T. ) ;
#55919 = CARTESIAN_POINT ( 'NONE',  ( -113.6929263765337907, 10.01517768586948698, -1.839758294383808571E-15 ) ) ;
#55920 = CARTESIAN_POINT ( 'NONE',  ( -134.3949999999999250, -6.826472737025115478, -4.959722759717899443 ) ) ;
#55921 = FACE_OUTER_BOUND ( 'NONE', #39195, .T. ) ;
#55922 = EDGE_CURVE ( 'NONE', #32643, #16561, #3819, .T. ) ;
#55923 = CARTESIAN_POINT ( 'NONE',  ( -45.50000000000000000, 7.768687147774684831, 6.999999999999999112 ) ) ;
#55924 = CARTESIAN_POINT ( 'NONE',  ( -173.3929263765337510, 8.102448949553176405, 5.886773742842740909 ) ) ;
#55925 = ORIENTED_EDGE ( 'NONE', *, *, #29203, .T. ) ;
#55926 = VERTEX_POINT ( 'NONE', #25168 ) ;
#55927 = DIRECTION ( 'NONE',  ( -1.000000000000000000, -0.000000000000000000, -0.000000000000000000 ) ) ;
#55928 = VECTOR ( 'NONE', #31318, 1000.000000000000000 ) ;
#55929 = SURFACE_STYLE_USAGE ( .BOTH. , #66852 ) ;
#55930 = CARTESIAN_POINT ( 'NONE',  ( -98.60707362346616378, -8.102448949553174629, 5.886773742842742685 ) ) ;
#55931 = CARTESIAN_POINT ( 'NONE',  ( 3.749999999999999556, 34.24999999999998579, -3.750000000000000000 ) ) ;
#55933 = CARTESIAN_POINT ( 'NONE',  ( -127.4070736234668715, 3.094860106606866168, -9.525000000008395418 ) ) ;
#55932 = MECHANICAL_DESIGN_GEOMETRIC_PRESENTATION_REPRESENTATION (  '', ( #4236 ), #24481 ) ;
#55934 = ORIENTED_EDGE ( 'NONE', *, *, #68287, .T. ) ;
#55935 = CARTESIAN_POINT ( 'NONE',  ( -129.5049999999999955, -6.826472737025113702, -4.959722759717900331 ) ) ;
#55936 = ORIENTED_EDGE ( 'NONE', *, *, #48274, .T. ) ;
#55937 = ADVANCED_FACE ( 'NONE', ( #30781 ), #25193, .T. ) ;
#55938 = ORIENTED_EDGE ( 'NONE', *, *, #40204, .F. ) ;
#55939 = DIRECTION ( 'NONE',  ( 0.000000000000000000, 0.000000000000000000, 1.000000000000000000 ) ) ;
#55940 = ORIENTED_EDGE ( 'NONE', *, *, #8702, .F. ) ;
#55941 = VECTOR ( 'NONE', #12128, 1000.000000000000000 ) ;
#55942 = CARTESIAN_POINT ( 'NONE',  ( 3.499999999999998668, 36.74999999999999289, 4.000000000000000000 ) ) ;
#55943 = ADVANCED_FACE ( 'NONE', ( #46684 ), #14624, .F. ) ;
#55944 = CARTESIAN_POINT ( 'NONE',  ( 5.598654528085809545, 142.1449999999999818, -7.705886871421373741 ) ) ;
#55945 = PRESENTATION_STYLE_ASSIGNMENT (( #23584 ) ) ;
#55946 = ORIENTED_EDGE ( 'NONE', *, *, #65751, .F. ) ;
#55947 = CARTESIAN_POINT ( 'NONE',  ( 0.000000000000000000, 140.5549999999999784, -9.525000000000000355 ) ) ;
#55948 = DIRECTION ( 'NONE',  ( -1.000000000000000000, -0.000000000000000000, -0.000000000000000000 ) ) ;
#55949 = ORIENTED_EDGE ( 'NONE', *, *, #45847, .T. ) ;
#55950 = CARTESIAN_POINT ( 'NONE',  ( 9.058813317711337021, 160.6550000000000011, 2.943386871421375783 ) ) ;
#55951 = CARTESIAN_POINT ( 'NONE',  ( -60.00000000000000000, -2.024042244987997205E-14, 6.999999999999995559 ) ) ;
#55952 = UNCERTAINTY_MEASURE_WITH_UNIT (LENGTH_MEASURE( 1.000000000000000082E-05 ), #56752, 'distance_accuracy_value', 'NONE');
#55953 = VECTOR ( 'NONE', #61350, 1000.000000000000000 ) ;
#55954 = FILL_AREA_STYLE ('',( #55616 ) ) ;
#55955 = VECTOR ( 'NONE', #4742, 1000.000000000000000 ) ;
#55956 = CARTESIAN_POINT ( 'NONE',  ( -71.75000000000000000, -4.000000000000000000, 20.00000000000000000 ) ) ;
#55957 = ORIENTED_EDGE ( 'NONE', *, *, #37095, .T. ) ;
#55958 = ORIENTED_EDGE ( 'NONE', *, *, #60513, .T. ) ;
#55959 = LINE ( 'NONE', #13747, #25793 ) ;
#55960 = DIRECTION ( 'NONE',  ( 0.000000000000000000, 0.000000000000000000, 1.000000000000000000 ) ) ;
#55961 = CARTESIAN_POINT ( 'NONE',  ( 48.50000000000000000, 22.24999999999998579, -3.750000000000000000 ) ) ;
#55962 = CARTESIAN_POINT ( 'NONE',  ( -161.7549999999999955, 4.716976649647091513, -6.492361379858946790 ) ) ;
#55963 = VERTEX_POINT ( 'NONE', #68798 ) ;
#55964 = CYLINDRICAL_SURFACE ( 'NONE', #38578, 0.5000000000000004441 ) ;
#55965 = UNCERTAINTY_MEASURE_WITH_UNIT (LENGTH_MEASURE( 1.000000000000000082E-05 ), #6629, 'distance_accuracy_value', 'NONE');
#55966 = FILL_AREA_STYLE ('',( #29583 ) ) ;
#55967 =( LENGTH_UNIT ( ) NAMED_UNIT ( * ) SI_UNIT ( .MILLI., .METRE. ) );
#55968 = CARTESIAN_POINT ( 'NONE',  ( 45.00000000000000000, 9.639620389971918613, -7.000000000000000000 ) ) ;
#55969 = CYLINDRICAL_SURFACE ( 'NONE', #23143, 0.5000000000000004441 ) ;
#55970 = ORIENTED_EDGE ( 'NONE', *, *, #59465, .F. ) ;
#55971 = ORIENTED_EDGE ( 'NONE', *, *, #33436, .T. ) ;
#55972 = DIRECTION ( 'NONE',  ( 0.000000000000000000, 0.000000000000000000, -1.000000000000000000 ) ) ;
#55973 = CYLINDRICAL_SURFACE ( 'NONE', #49312, 9.524999999999991473 ) ;
#55974 = CARTESIAN_POINT ( 'NONE',  ( -80.15499999999998693, 7.632228543268600340, 2.479861379858949277 ) ) ;
#55975 = EDGE_LOOP ( 'NONE', ( #10852, #36081, #40995, #28744 ) ) ;
#55976 = EDGE_CURVE ( 'NONE', #17294, #6425, #68104, .T. ) ;
#55977 = CARTESIAN_POINT ( 'NONE',  ( -64.25707362346616947, 5.598654528085800663, -7.705886871421367523 ) ) ;
#55978 = PRESENTATION_STYLE_ASSIGNMENT (( #28884 ) ) ;
#55979 = CIRCLE ( 'NONE', #12174, 1.000000000000000000 ) ;
#55980 = EDGE_CURVE ( 'NONE', #39091, #25818, #64514, .T. ) ;
#55981 = CARTESIAN_POINT ( 'NONE',  ( -75.00000000000000000, 7.768687147774688384, -7.000000000000000000 ) ) ;
#55982 = EDGE_LOOP ( 'NONE', ( #36871, #40535, #19059, #15841 ) ) ;
#55983 = CARTESIAN_POINT ( 'NONE',  ( 4.041451884327376121, 7.000000000000007105, 1.082903768654759569 ) ) ;
#55984 =( GEOMETRIC_REPRESENTATION_CONTEXT ( 3 ) GLOBAL_UNCERTAINTY_ASSIGNED_CONTEXT ( ( #20079 ) ) GLOBAL_UNIT_ASSIGNED_CONTEXT ( ( #41639, #41294, #52192 ) ) REPRESENTATION_CONTEXT ( 'NONE', 'WORKASPACE' ) );
#55986 = FILL_AREA_STYLE ('',( #50724 ) ) ;
#55985 =( NAMED_UNIT ( * ) SI_UNIT ( $, .STERADIAN. ) SOLID_ANGLE_UNIT ( ) );
#55987 = TOROIDAL_SURFACE ( 'NONE', #34637, 1.000000000000000000, 0.5000000000000000000 ) ;
#55988 = ADVANCED_FACE ( 'NONE', ( #52280, #36468 ), #14994, .T. ) ;
#55989 = CARTESIAN_POINT ( 'NONE',  ( -3.094860106618434248, 137.7950000000000159, 9.525000000000000355 ) ) ;
#55990 = CARTESIAN_POINT ( 'NONE',  ( -111.1449999999999960, -4.716976649647092401, 6.492361379858946790 ) ) ;
#55991 = CIRCLE ( 'NONE', #12145, 0.5000000000000004441 ) ;
#55992 = PRESENTATION_STYLE_ASSIGNMENT (( #45499 ) ) ;
#55993 = CARTESIAN_POINT ( 'NONE',  ( -19.86963632605004548, 11.94623282526795371, 1.146258047298002181 ) ) ;
#55994 = CARTESIAN_POINT ( 'NONE',  ( -140.9929263765338305, 8.102448949553171076, -5.886773742842744461 ) ) ;
#55995 = CARTESIAN_POINT ( 'NONE',  ( -162.5949999999999704, 2.607480562269073321, 8.024999999999991473 ) ) ;
#55996 = MECHANICAL_DESIGN_GEOMETRIC_PRESENTATION_REPRESENTATION (  '', ( #63871 ), #62715 ) ;
#55997 = ADVANCED_FACE ( 'NONE', ( #31122 ), #15090, .T. ) ;
#55998 = DIRECTION ( 'NONE',  ( 0.000000000000000000, 0.000000000000000000, 1.000000000000000000 ) ) ;
#55999 = SURFACE_SIDE_STYLE ('',( #50738 ) ) ;
#56000 = ORIENTED_EDGE ( 'NONE', *, *, #28394, .F. ) ;
#56001 = CARTESIAN_POINT ( 'NONE',  ( -24.00000000000000355, 36.75000000000000000, 3.000000000000000000 ) ) ;
#56002 = VERTEX_POINT ( 'NONE', #63829 ) ;
#56003 =( LENGTH_UNIT ( ) NAMED_UNIT ( * ) SI_UNIT ( .MILLI., .METRE. ) );
#56004 = CIRCLE ( 'NONE', #45903, 5.000000000000004441 ) ;
#56005 = CARTESIAN_POINT ( 'NONE',  ( 30.25000000000001066, 16.24999999999997513, 3.750000000000000000 ) ) ;
#56006 = CARTESIAN_POINT ( 'NONE',  ( -15.48999599679679662, 147.4999999999999716, 10.00000000000000000 ) ) ;
#56007 = CARTESIAN_POINT ( 'NONE',  ( 0.000000000000000000, 142.0570736234661524, -8.025000000000000355 ) ) ;
#56008 = TOROIDAL_SURFACE ( 'NONE', #54844, 2.000000000000000000, 1.000000000000000000 ) ;
#56009 = ORIENTED_EDGE ( 'NONE', *, *, #60201, .F. ) ;
#56010 = CARTESIAN_POINT ( 'NONE',  ( -161.3050000000000068, 8.437984349512086979, -1.550032578732815448E-15 ) ) ;
#56011 = EDGE_LOOP ( 'NONE', ( #35384, #21786, #41094, #69462 ) ) ;
#56012 = LINE ( 'NONE', #19775, #18892 ) ;
#56013 = DIRECTION ( 'NONE',  ( 0.000000000000000000, 0.000000000000000000, 1.000000000000000000 ) ) ;
#56014 = FACE_OUTER_BOUND ( 'NONE', #15147, .T. ) ;
#56015 = AXIS2_PLACEMENT_3D ( 'NONE', #67901, #45089, #45441 ) ;
#56016 = CARTESIAN_POINT ( 'NONE',  ( -8.102448949553181734, 112.8949999999999818, -5.886773742842749790 ) ) ;
#56017 = ORIENTED_EDGE ( 'NONE', *, *, #38583, .F. ) ;
#56018 = CARTESIAN_POINT ( 'NONE',  ( 74.99999999999998579, 50.00000000000000000, 7.000000000000000000 ) ) ;
#56019 = CARTESIAN_POINT ( 'NONE',  ( -9.058813317711337021, 111.1549999999999869, -2.943386871421374895 ) ) ;
#56020 = CARTESIAN_POINT ( 'NONE',  ( -82.10499999999996135, -6.826472737025113702, 4.959722759717902107 ) ) ;
#56021 = CARTESIAN_POINT ( 'NONE',  ( -8.437984349512095861, 121.8070736234661524, -5.166775262442723748E-16 ) ) ;
#56022 = CARTESIAN_POINT ( 'NONE',  ( -8.102448949553181734, 126.6050000000000040, 5.886773742842747126 ) ) ;
#56023 = UNCERTAINTY_MEASURE_WITH_UNIT (LENGTH_MEASURE( 1.000000000000000082E-05 ), #14360, 'distance_accuracy_value', 'NONE');
#56024 = AXIS2_PLACEMENT_3D ( 'NONE', #63083, #64118, #36749 ) ;
#56025 = CARTESIAN_POINT ( 'NONE',  ( 20.43039690318515156, 114.8190495831791793, 10.32375696423105360 ) ) ;
#56026 = CARTESIAN_POINT ( 'NONE',  ( -45.00000000000000000, 9.708372675170618749, 10.00000000000000000 ) ) ;
#56027 = FILL_AREA_STYLE ('',( #34244 ) ) ;
#56028 = ORIENTED_EDGE ( 'NONE', *, *, #19924, .T. ) ;
#56029 =( GEOMETRIC_REPRESENTATION_CONTEXT ( 3 ) GLOBAL_UNCERTAINTY_ASSIGNED_CONTEXT ( ( #6630 ) ) GLOBAL_UNIT_ASSIGNED_CONTEXT ( ( #24819, #25520, #42118 ) ) REPRESENTATION_CONTEXT ( 'NONE', 'WORKASPACE' ) );
#56030 = SURFACE_STYLE_USAGE ( .BOTH. , #34936 ) ;
#56031 = CARTESIAN_POINT ( 'NONE',  ( -52.64499999999999602, 4.716976649647091513, -6.492361379858946790 ) ) ;
#56032 = ORIENTED_EDGE ( 'NONE', *, *, #48246, .F. ) ;
#56033 = FACE_OUTER_BOUND ( 'NONE', #3861, .T. ) ;
#56034 = COLOUR_RGB ( '', 0.09019608, 0.27058824, 0.51372549) ;
#56035 = LINE ( 'NONE', #66612, #45874 ) ;
#56036 = CARTESIAN_POINT ( 'NONE',  ( 13.25000000000000355, 28.24999999999998934, 4.000000000000000000 ) ) ;
#56037 = DIRECTION ( 'NONE',  ( 0.000000000000000000, 0.000000000000000000, -1.000000000000000000 ) ) ;
#56038 = ORIENTED_EDGE ( 'NONE', *, *, #67361, .T. ) ;
#56039 = CARTESIAN_POINT ( 'NONE',  ( 60.00000000000000000, 1.797044900979284448E-15, 11.50000000000000000 ) ) ;
#56040 = CARTESIAN_POINT ( 'NONE',  ( -53.54499999999998039, -7.632228543268600340, -2.479861379858950166 ) ) ;
#56041 = SPHERICAL_SURFACE ( 'NONE', #44953, 0.5000000000000000000 ) ;
#56042 = ORIENTED_EDGE ( 'NONE', *, *, #39088, .F. ) ;
#56043 = CIRCLE ( 'NONE', #58313, 14.49999999999999822 ) ;
#56044 = CARTESIAN_POINT ( 'NONE',  ( -75.00000000000000000, 8.589831058620905679, 5.576814063797191245 ) ) ;
#56045 = CARTESIAN_POINT ( 'NONE',  ( -109.4049999999999727, -2.607480562269069768, 8.024999999999991473 ) ) ;
#56046 = VERTEX_POINT ( 'NONE', #31469 ) ;
#56047 = DIRECTION ( 'NONE',  ( 0.000000000000000000, 0.000000000000000000, -1.000000000000000000 ) ) ;
#56048 = EDGE_CURVE ( 'NONE', #8712, #53612, #41780, .T. ) ;
#56049 = SPHERICAL_SURFACE ( 'NONE', #6651, 0.5000000000000000000 ) ;
#56050 = FACE_OUTER_BOUND ( 'NONE', #61711, .T. ) ;
#56051 = CARTESIAN_POINT ( 'NONE',  ( -138.3570736234661638, 5.598654528085804216, 7.705886871421366635 ) ) ;
#56052 = LINE ( 'NONE', #60981, #13703 ) ;
#56053 = CARTESIAN_POINT ( 'NONE',  ( -1.166476076187854022E-15, 137.9449999999999932, 9.525000000000000355 ) ) ;
#56054 = CARTESIAN_POINT ( 'NONE',  ( -80.30707362346616662, -10.01517768586948698, 6.132527647946031529E-16 ) ) ;
#56055 = COLOUR_RGB ( '', 0.40784314, 0.44705882, 0.49803922) ;
#56056 = CARTESIAN_POINT ( 'NONE',  ( -95.39292637653380780, 8.102448949553176405, 5.886773742842740909 ) ) ;
#56057 = DIRECTION ( 'NONE',  ( -0.000000000000000000, -1.000000000000000000, 0.000000000000000000 ) ) ;
#56058 = FACE_OUTER_BOUND ( 'NONE', #34847, .T. ) ;
#56059 = EDGE_CURVE ( 'NONE', #10174, #42918, #22997, .T. ) ;
#56061 = DIRECTION ( 'NONE',  ( 1.000000000000000000, 0.000000000000000000, 0.000000000000000000 ) ) ;
#56060 = CARTESIAN_POINT ( 'NONE',  ( 2.000000000000008438, 26.00000000000000355, -27.50000000000000355 ) ) ;
#56062 = CIRCLE ( 'NONE', #43759, 13.99999999999999822 ) ;
#56063 = CARTESIAN_POINT ( 'NONE',  ( -120.5049999999999812, -6.826472737025115478, -4.959722759717899443 ) ) ;
#56064 = EDGE_CURVE ( 'NONE', #20404, #5343, #39223, .T. ) ;
#56065 = DIRECTION ( 'NONE',  ( 0.000000000000000000, 0.000000000000000000, 1.000000000000000000 ) ) ;
#56066 = CARTESIAN_POINT ( 'NONE',  ( -159.4429263765338192, -1.166476076187852838E-15, -9.524999999999991473 ) ) ;
#56067 =( LENGTH_UNIT ( ) NAMED_UNIT ( * ) SI_UNIT ( .MILLI., .METRE. ) );
#56068 = CARTESIAN_POINT ( 'NONE',  ( -140.0949999999999989, -2.607480562269071545, -8.024999999999991473 ) ) ;
#56069 = EDGE_CURVE ( 'NONE', #51444, #44068, #39282, .T. ) ;
#56070 = AXIS2_PLACEMENT_3D ( 'NONE', #61002, #18107, #40625 ) ;
#56071 = CIRCLE ( 'NONE', #25737, 0.5000000000000004441 ) ;
#56072 = CARTESIAN_POINT ( 'NONE',  ( -119.6949999999999932, -8.437984349512086979, 5.166775262442717831E-16 ) ) ;
#56073 = ADVANCED_FACE ( 'NONE', ( #38189 ), #68999, .T. ) ;
#56074 = DIRECTION ( 'NONE',  ( 0.000000000000000000, -1.000000000000000000, 0.000000000000000000 ) ) ;
#56075 = VECTOR ( 'NONE', #58260, 1000.000000000000000 ) ;
#56076 = ORIENTED_EDGE ( 'NONE', *, *, #9407, .F. ) ;
#56077 = CIRCLE ( 'NONE', #56115, 29.50000000000000000 ) ;
#56078 = CARTESIAN_POINT ( 'NONE',  ( 24.00000000000000355, 37.00000000000000000, 3.750000000000000000 ) ) ;
#56079 = SURFACE_SIDE_STYLE ('',( #29701 ) ) ;
#56080 = ADVANCED_FACE ( 'NONE', ( #27903 ), #31911, .T. ) ;
#56081 = CARTESIAN_POINT ( 'NONE',  ( 0.000000000000000000, 154.9999999999999716, 0.000000000000000000 ) ) ;
#56082 = CARTESIAN_POINT ( 'NONE',  ( -172.6429263765338078, -5.598654528085801552, 7.705886871421367523 ) ) ;
#56083 = DIRECTION ( 'NONE',  ( -1.000000000000000000, -0.000000000000000000, 0.000000000000000000 ) ) ;
#56084 = AXIS2_PLACEMENT_3D ( 'NONE', #18302, #23911, #8084 ) ;
#56085 = SURFACE_STYLE_USAGE ( .BOTH. , #57752 ) ;
#56086 = CARTESIAN_POINT ( 'NONE',  ( -60.99999999999998579, 50.00000000000000000, 9.500000000000000000 ) ) ;
#56087 = COLOUR_RGB ( '', 0.08235294, 0.09019608, 0.10196078) ;
#56088 = LINE ( 'NONE', #14230, #34994 ) ;
#56089 = CARTESIAN_POINT ( 'NONE',  ( -94.64292637653380780, -5.598654528085801552, 7.705886871421367523 ) ) ;
#56090 = APPLICATION_PROTOCOL_DEFINITION ( 'draft international standard', 'automotive_design', 1998, #54965 ) ;
#56091 = STYLED_ITEM ( 'NONE', ( #50897 ), #15826 ) ;
#56092 = CYLINDRICAL_SURFACE ( 'NONE', #1188, 0.5000000000000004441 ) ;
#56093 = CARTESIAN_POINT ( 'NONE',  ( -179.2429263765338021, 5.598654528085804216, 7.705886871421366635 ) ) ;
#56094 = CYLINDRICAL_SURFACE ( 'NONE', #20265, 0.2500000000000002220 ) ;
#56095 = CARTESIAN_POINT ( 'NONE',  ( -79.55707362346616662, -1.166476076187852838E-15, -9.524999999999991473 ) ) ;
#56096 = STYLED_ITEM ( 'NONE', ( #11073 ), #68566 ) ;
#56097 = CARTESIAN_POINT ( 'NONE',  ( 12.25000000000000355, 30.74999999999998579, -3.750000000000000000 ) ) ;
#56098 = ORIENTED_EDGE ( 'NONE', *, *, #10877, .T. ) ;
#56099 = DIRECTION ( 'NONE',  ( 0.000000000000000000, 0.000000000000000000, -1.000000000000000000 ) ) ;
#56100 = DIRECTION ( 'NONE',  ( 1.000000000000000000, 0.000000000000000000, 0.000000000000000000 ) ) ;
#56101 = ORIENTED_EDGE ( 'NONE', *, *, #17803, .F. ) ;
#56102 = CIRCLE ( 'NONE', #40414, 19.99999999999998934 ) ;
#56103 = CARTESIAN_POINT ( 'NONE',  ( 0.000000000000000000, 127.0570736234661666, -8.025000000000000355 ) ) ;
#56104 = CARTESIAN_POINT ( 'NONE',  ( 3.000000000000030198, 43.00000000000000000, 89.00000000000000000 ) ) ;
#56105 = DIRECTION ( 'NONE',  ( 0.000000000000000000, 0.000000000000000000, -1.000000000000000000 ) ) ;
#56107 = ORIENTED_EDGE ( 'NONE', *, *, #39425, .T. ) ;
#56106 = AXIS2_PLACEMENT_3D ( 'NONE', #20520, #36017, #57817 ) ;
#56108 =( NAMED_UNIT ( * ) SI_UNIT ( $, .STERADIAN. ) SOLID_ANGLE_UNIT ( ) );
#56109 = CARTESIAN_POINT ( 'NONE',  ( -75.00000000000000000, -2.215169945516535778E-14, -6.500000000000000888 ) ) ;
#56110 = MECHANICAL_DESIGN_GEOMETRIC_PRESENTATION_REPRESENTATION (  '', ( #54996 ), #34775 ) ;
#56111 = AXIS2_PLACEMENT_3D ( 'NONE', #7049, #32739, #23237 ) ;
#56112 = CARTESIAN_POINT ( 'NONE',  ( -79.04499999999998749, 7.632228543268600340, 2.479861379858949277 ) ) ;
#56114 = ORIENTED_EDGE ( 'NONE', *, *, #20652, .F. ) ;
#56113 = VECTOR ( 'NONE', #28912, 1000.000000000000000 ) ;
#56115 = AXIS2_PLACEMENT_3D ( 'NONE', #26791, #47657, #38118 ) ;
#56116 = SURFACE_SIDE_STYLE ('',( #23766 ) ) ;
#56117 = DIRECTION ( 'NONE',  ( -2.312964634635740689E-15, 1.000000000000000000, -0.000000000000000000 ) ) ;
#56118 = VERTEX_POINT ( 'NONE', #49758 ) ;
#56119 = SURFACE_STYLE_USAGE ( .BOTH. , #50522 ) ;
#56120 = CARTESIAN_POINT ( 'NONE',  ( -10.39230484541327293, 3.469446951953614189E-15, 7.500000000000000000 ) ) ;
#56121 = ORIENTED_EDGE ( 'NONE', *, *, #31523, .T. ) ;
#56122 = FILL_AREA_STYLE ('',( #34340 ) ) ;
#56124 = ORIENTED_EDGE ( 'NONE', *, *, #19140, .T. ) ;
#56123 = ADVANCED_FACE ( 'NONE', ( #65223 ), #38552, .T. ) ;
#56125 = CARTESIAN_POINT ( 'NONE',  ( -138.1429263765338078, 5.598654528085800663, -7.705886871421367523 ) ) ;
#56126 = SURFACE_STYLE_FILL_AREA ( #12877 ) ;
#56127 =( NAMED_UNIT ( * ) PLANE_ANGLE_UNIT ( ) SI_UNIT ( $, .RADIAN. ) );
#56128 = CARTESIAN_POINT ( 'NONE',  ( -178.2570736234661695, 5.598654528085800663, -7.705886871421367523 ) ) ;
#56129 = CIRCLE ( 'NONE', #34797, 0.2500000000000002220 ) ;
#56130 = CARTESIAN_POINT ( 'NONE',  ( 4.250000000000001776, 22.24999999999998579, 4.000000000000000000 ) ) ;
#56131 = ADVANCED_FACE ( 'NONE', ( #19011 ), #19373, .F. ) ;
#56132 = CARTESIAN_POINT ( 'NONE',  ( -112.8570736234661638, -5.598654528085803328, -7.705886871421366635 ) ) ;
#56133 = CARTESIAN_POINT ( 'NONE',  ( -183.1444352087858363, 4.866151391066206422, -8.027994637291957503 ) ) ;
#56134 = DIRECTION ( 'NONE',  ( -0.000000000000000000, -0.000000000000000000, 1.000000000000000000 ) ) ;
#56135 = ORIENTED_EDGE ( 'NONE', *, *, #17518, .F. ) ;
#56136 = STYLED_ITEM ( 'NONE', ( #57287 ), #69261 ) ;
#56137 = CARTESIAN_POINT ( 'NONE',  ( 0.000000000000000000, -3.500000000000000000, 24.00000000000000000 ) ) ;
#56138 = DIRECTION ( 'NONE',  ( 1.000000000000000000, -1.156482317317866302E-16, 0.000000000000000000 ) ) ;
#56139 = DIRECTION ( 'NONE',  ( 0.2413793103448194644, -0.9704308468600220117, 0.000000000000000000 ) ) ;
#56140 = FILL_AREA_STYLE_COLOUR ( '', #20858 ) ;
#56141 = CARTESIAN_POINT ( 'NONE',  ( -146.3049999999999784, 8.437984349512085203, -1.550032578732815448E-15 ) ) ;
#56142 = CARTESIAN_POINT ( 'NONE',  ( -4.750000000000000000, 0.000000000000000000, 1.000000000000000000 ) ) ;
#56143 = CARTESIAN_POINT ( 'NONE',  ( -164.9949999999999761, -6.826472737025115478, 4.959722759717900331 ) ) ;
#56144 = EDGE_CURVE ( 'NONE', #31434, #35184, #14118, .T. ) ;
#56145 = CARTESIAN_POINT ( 'NONE',  ( -158.5449999999999875, -7.632228543268600340, -2.479861379858950166 ) ) ;
#56146 = MECHANICAL_DESIGN_GEOMETRIC_PRESENTATION_REPRESENTATION (  '', ( #22467 ), #43849 ) ;
#56147 = AXIS2_PLACEMENT_3D ( 'NONE', #19727, #27403, #21811 ) ;
#56148 =( BOUNDED_CURVE ( )  B_SPLINE_CURVE ( 2, ( #28605, #60610, #447, #60964, #44843, #39211, #27563, #39561, #64863, #50102, #21978 ),
 .UNSPECIFIED., .F., .F. ) 
 B_SPLINE_CURVE_WITH_KNOTS ( ( 3, 2, 2, 2, 2, 3 ),
 ( 0.3152173913043405107, 0.3173913043478187035, 0.3195652173912968963, 0.3217391304347750891, 0.3239130434782533374, 0.3260869565217315302 ),
 .UNSPECIFIED. ) 
 CURVE ( )  GEOMETRIC_REPRESENTATION_ITEM ( )  RATIONAL_B_SPLINE_CURVE ( ( 1.000000000000164979, 0.9510565162949885520, 1.000000000000000000, 0.9510565162951535312, 1.000000000000000000, 0.9510565162951535312, 1.000000000000000000, 0.9510565162951535312, 1.000000000000000000, 0.9510565162953247276, 0.9999999999998288036 ) ) 
 REPRESENTATION_ITEM ( '' )  );
#56149 = ORIENTED_EDGE ( 'NONE', *, *, #45328, .F. ) ;
#56150 = CARTESIAN_POINT ( 'NONE',  ( 27.99999999999999645, 0.000000000000000000, 24.00402776293821816 ) ) ;
#56151 = DIRECTION ( 'NONE',  ( -2.168404344971007882E-16, 0.000000000000000000, -1.000000000000000000 ) ) ;
#56152 = CIRCLE ( 'NONE', #38232, 4.999999999999997335 ) ;
#56153 = EDGE_CURVE ( 'NONE', #48456, #66133, #44382, .T. ) ;
#56154 = CARTESIAN_POINT ( 'NONE',  ( -74.15499999999998693, 7.632228543268600340, 2.479861379858949277 ) ) ;
#56155 = CARTESIAN_POINT ( 'NONE',  ( -36.85730689286826589, -10.63899366288961090, 3.897680902423376725 ) ) ;
#56156 = CARTESIAN_POINT ( 'NONE',  ( -67.64499999999998181, 4.716976649647091513, -6.492361379858946790 ) ) ;
#56157 = CARTESIAN_POINT ( 'NONE',  ( -8.102448949553181734, 144.6049999999999613, 5.886773742842747126 ) ) ;
#56158 = DIRECTION ( 'NONE',  ( -0.000000000000000000, -0.000000000000000000, 1.000000000000000000 ) ) ;
#56159 = VECTOR ( 'NONE', #39404, 1000.000000000000000 ) ;
#56160 = CIRCLE ( 'NONE', #22494, 14.00000000000000533 ) ;
#56161 = CARTESIAN_POINT ( 'NONE',  ( -160.4070736234664594, 3.094860106613722905, -9.525000000003412737 ) ) ;
#56162 = CARTESIAN_POINT ( 'NONE',  ( -20.04014546381213435, 115.4999999869038163, -10.00000000000000000 ) ) ;
#56163 = CARTESIAN_POINT ( 'NONE',  ( 9.984889265949528081, 1.515110734050476582, -0.7056644834263100519 ) ) ;
#56164 = MECHANICAL_DESIGN_GEOMETRIC_PRESENTATION_REPRESENTATION (  '', ( #38247 ), #47299 ) ;
#56165 = DIRECTION ( 'NONE',  ( 0.000000000000000000, 1.000000000000000000, 0.000000000000000000 ) ) ;
#56166 = AXIS2_PLACEMENT_3D ( 'NONE', #9140, #52060, #3815 ) ;
#56167 = DIRECTION ( 'NONE',  ( -1.000000000000000000, 0.000000000000000000, -0.000000000000000000 ) ) ;
#56168 = VERTEX_POINT ( 'NONE', #57016 ) ;
#56169 = AXIS2_PLACEMENT_3D ( 'NONE', #28811, #45051, #22872 ) ;
#56170 = EDGE_LOOP ( 'NONE', ( #9602, #23470, #4641, #11753 ) ) ;
#56171 = CARTESIAN_POINT ( 'NONE',  ( -61.25707362346617657, 5.598654528085800663, -7.705886871421367523 ) ) ;
#56172 = CARTESIAN_POINT ( 'NONE',  ( -155.6929263765338192, 10.01517768586948698, -1.839758294383808966E-15 ) ) ;
#56173 = ADVANCED_FACE ( 'NONE', ( #30257 ), #56818, .F. ) ;
#56174 = PRESENTATION_LAYER_ASSIGNMENT (  '', '', ( #43888 ) ) ;
#56175 = DIRECTION ( 'NONE',  ( 1.000000000000000000, 0.000000000000000000, 0.000000000000000000 ) ) ;
#56176 = CIRCLE ( 'NONE', #38272, 1.000000000000000888 ) ;
#56177 = PRESENTATION_STYLE_ASSIGNMENT (( #28389 ) ) ;
#56178 = ORIENTED_EDGE ( 'NONE', *, *, #67119, .F. ) ;
#56179 = ORIENTED_EDGE ( 'NONE', *, *, #64734, .F. ) ;
#56180 = DIRECTION ( 'NONE',  ( 0.000000000000000000, 1.000000000000000000, 0.000000000000000000 ) ) ;
#56181 = FILL_AREA_STYLE ('',( #30132 ) ) ;
#56182 = ORIENTED_EDGE ( 'NONE', *, *, #22023, .F. ) ;
#56183 = CARTESIAN_POINT ( 'NONE',  ( 5.598654528085805993, 112.3549999999999898, 7.705886871421374629 ) ) ;
#56184 = CARTESIAN_POINT ( 'NONE',  ( -7.511572993685801073E-16, 7.000000000000000888, 0.000000000000000000 ) ) ;
#56185 = ORIENTED_EDGE ( 'NONE', *, *, #57235, .F. ) ;
#56186 = AXIS2_PLACEMENT_3D ( 'NONE', #35516, #56960, #9486 ) ;
#56187 = DIRECTION ( 'NONE',  ( -0.000000000000000000, -0.000000000000000000, 1.000000000000000000 ) ) ;
#56188 = CARTESIAN_POINT ( 'NONE',  ( -107.2449999999999903, -4.716976649647093289, -6.492361379858945902 ) ) ;
#56189 = ORIENTED_EDGE ( 'NONE', *, *, #65281, .T. ) ;
#56190 = CARTESIAN_POINT ( 'NONE',  ( -3.453468097287629046, 110.4999999999999858, -8.920302546751260664 ) ) ;
#56191 = CARTESIAN_POINT ( 'NONE',  ( 1.709458476932651091E-14, -60.04052944165106709, 35.50000000000000000 ) ) ;
#56192 = CARTESIAN_POINT ( 'NONE',  ( -11.69070681507827736, -11.39755657220772633, 3.762028377819578218 ) ) ;
#56193 = TOROIDAL_SURFACE ( 'NONE', #69670, 0.5000000000000000000, 0.2500000000000000000 ) ;
#56194 = LINE ( 'NONE', #52351, #40905 ) ;
#56195 = VERTEX_POINT ( 'NONE', #20557 ) ;
#56196 = CARTESIAN_POINT ( 'NONE',  ( -2.607480562269073765, 144.0929263765338249, -8.025000000000000355 ) ) ;
#56197 = CARTESIAN_POINT ( 'NONE',  ( 12.75000000000000533, 27.99999999999998224, -3.750000000000000000 ) ) ;
#56198 = LINE ( 'NONE', #62521, #50382 ) ;
#56199 = EDGE_CURVE ( 'NONE', #52477, #39971, #67953, .T. ) ;
#56200 =( NAMED_UNIT ( * ) SI_UNIT ( $, .STERADIAN. ) SOLID_ANGLE_UNIT ( ) );
#56201 = PRESENTATION_STYLE_ASSIGNMENT (( #8028 ) ) ;
#56202 = EDGE_CURVE ( 'NONE', #36334, #49504, #13997, .T. ) ;
#56203 = VERTEX_POINT ( 'NONE', #41700 ) ;
#56204 = CIRCLE ( 'NONE', #21418, 13.99999999999999822 ) ;
#56205 = SURFACE_SIDE_STYLE ('',( #45708 ) ) ;
#56206 = ORIENTED_EDGE ( 'NONE', *, *, #18853, .F. ) ;
#56207 = DIRECTION ( 'NONE',  ( 0.000000000000000000, 0.000000000000000000, 1.000000000000000000 ) ) ;
#56208 = CARTESIAN_POINT ( 'NONE',  ( 40.99999999999999289, 107.7459666924148110, -3.099782425413943443 ) ) ;
#56209 = CARTESIAN_POINT ( 'NONE',  ( -137.3049999999999784, 8.437984349512085203, -1.550032578732815448E-15 ) ) ;
#56210 = DIRECTION ( 'NONE',  ( -1.000000000000000000, -0.000000000000000000, -0.000000000000000000 ) ) ;
#56211 = PRESENTATION_STYLE_ASSIGNMENT (( #23511 ) ) ;
#56212 = EDGE_LOOP ( 'NONE', ( #47679, #20693, #49768, #30744 ) ) ;
#56213 = CARTESIAN_POINT ( 'NONE',  ( 0.000000000000000000, 87.30187232391182306, 0.000000000000000000 ) ) ;
#56214 = EDGE_CURVE ( 'NONE', #10996, #15405, #25478, .T. ) ;
#56215 = SURFACE_SIDE_STYLE ('',( #55539 ) ) ;
#56216 = VECTOR ( 'NONE', #67784, 1000.000000000000000 ) ;
#56217 = CARTESIAN_POINT ( 'NONE',  ( 3.542013698345604755, 9.000000000000008882, 0.6642442188400928815 ) ) ;
#56218 = ORIENTED_EDGE ( 'NONE', *, *, #23676, .T. ) ;
#56219 = CIRCLE ( 'NONE', #50615, 1.000000000000000888 ) ;
#56220 = ORIENTED_EDGE ( 'NONE', *, *, #50364, .T. ) ;
#56221 = FILL_AREA_STYLE ('',( #17913 ) ) ;
#56222 = CARTESIAN_POINT ( 'NONE',  ( 5.365183871890737421, -2.392512705203734935, -4.707228941936126176 ) ) ;
#56223 = CARTESIAN_POINT ( 'NONE',  ( -93.05707362346616662, 0.000000000000000000, 9.524999999999991473 ) ) ;
#56224 = FILL_AREA_STYLE ('',( #28435 ) ) ;
#56225 = EDGE_LOOP ( 'NONE', ( #56981, #39916, #66927, #5629 ) ) ;
#56226 = DIRECTION ( 'NONE',  ( 0.000000000000000000, 1.000000000000000000, 0.000000000000000000 ) ) ;
#56227 =( LENGTH_UNIT ( ) NAMED_UNIT ( * ) SI_UNIT ( .MILLI., .METRE. ) );
#56228 =( NAMED_UNIT ( * ) SI_UNIT ( $, .STERADIAN. ) SOLID_ANGLE_UNIT ( ) );
#56229 = STYLED_ITEM ( 'NONE', ( #17902 ), #17813 ) ;
#56230 = CARTESIAN_POINT ( 'NONE',  ( -57.50707362346615525, 8.102448949553176405, 5.886773742842740909 ) ) ;
#56231 = ADVANCED_FACE ( 'NONE', ( #57500 ), #8970, .F. ) ;
#56232 = DIRECTION ( 'NONE',  ( 0.000000000000000000, 0.000000000000000000, 1.000000000000000000 ) ) ;
#56233 = FACE_OUTER_BOUND ( 'NONE', #11969, .T. ) ;
#56234 = AXIS2_PLACEMENT_3D ( 'NONE', #45748, #41163, #14753 ) ;
#56235 = EDGE_LOOP ( 'NONE', ( #37510, #43864, #24863, #23272 ) ) ;
#56236 = AXIS2_PLACEMENT_3D ( 'NONE', #32924, #38589, #22357 ) ;
#56237 = SURFACE_STYLE_FILL_AREA ( #68203 ) ;
#56238 = EDGE_CURVE ( 'NONE', #37840, #25507, #62066, .T. ) ;
#56239 = CARTESIAN_POINT ( 'NONE',  ( -97.40499999999997272, -2.607480562269069768, 8.024999999999991473 ) ) ;
#56240 = CARTESIAN_POINT ( 'NONE',  ( -60.07797655783572566, -8.499999999999992895, 0.9794583065829002289 ) ) ;
#56241 = MECHANICAL_DESIGN_GEOMETRIC_PRESENTATION_REPRESENTATION (  '', ( #18095 ), #31529 ) ;
#56242 = DIRECTION ( 'NONE',  ( -0.000000000000000000, -0.000000000000000000, 1.000000000000000000 ) ) ;
#56243 = CARTESIAN_POINT ( 'NONE',  ( -96.14499999999999602, -4.716976649647092401, 6.492361379858946790 ) ) ;
#56244 = CARTESIAN_POINT ( 'NONE',  ( -3.094860106618432471, 116.7049999999999983, -9.525000000000000355 ) ) ;
#56245 = CARTESIAN_POINT ( 'NONE',  ( -78.14499999999999602, -4.716976649647092401, 6.492361379858946790 ) ) ;
#56246 = SURFACE_STYLE_FILL_AREA ( #7030 ) ;
#56247 = CARTESIAN_POINT ( 'NONE',  ( -56.75707362346615525, -5.598654528085801552, 7.705886871421367523 ) ) ;
#56248 = VECTOR ( 'NONE', #405, 1000.000000000000000 ) ;
#56249 = DIRECTION ( 'NONE',  ( 1.982541115402068561E-16, 0.000000000000000000, -1.000000000000000000 ) ) ;
#56250 =( BOUNDED_CURVE ( )  B_SPLINE_CURVE ( 2, ( #20361, #67880, #62571, #63282, #67514, #15130, #30553, #4155, #35858, #20000, #25625 ),
 .UNSPECIFIED., .F., .F. ) 
 B_SPLINE_CURVE_WITH_KNOTS ( ( 3, 2, 2, 2, 2, 3 ),
 ( 0.7058823529411762943, 0.7117647058823527439, 0.7176470588235291936, 0.7235294117647056433, 0.7294117647058820930, 0.7352941176470586537 ),
 .UNSPECIFIED. ) 
 CURVE ( )  GEOMETRIC_REPRESENTATION_ITEM ( )  RATIONAL_B_SPLINE_CURVE ( ( 1.000000000000001776, 0.9510565162951516438, 1.000000000000000000, 0.9510565162951535312, 1.000000000000000000, 0.9510565162951535312, 1.000000000000000000, 0.9510565162951535312, 1.000000000000000000, 0.9510565162951554186, 0.9999999999999981126 ) ) 
 REPRESENTATION_ITEM ( '' )  );
#56251 = CARTESIAN_POINT ( 'NONE',  ( 23.21231517720797655, 117.4999999999999716, 9.500000000000000000 ) ) ;
#56252 =( LENGTH_UNIT ( ) NAMED_UNIT ( * ) SI_UNIT ( .MILLI., .METRE. ) );
#56254 = ORIENTED_EDGE ( 'NONE', *, *, #24301, .T. ) ;
#56253 =( GEOMETRIC_REPRESENTATION_CONTEXT ( 3 ) GLOBAL_UNCERTAINTY_ASSIGNED_CONTEXT ( ( #31150 ) ) GLOBAL_UNIT_ASSIGNED_CONTEXT ( ( #66588, #34562, #2508 ) ) REPRESENTATION_CONTEXT ( 'NONE', 'WORKASPACE' ) );
#56255 = CARTESIAN_POINT ( 'NONE',  ( -117.2929263765337993, 3.094860106618428031, -9.524999999999993250 ) ) ;
#56256 = TOROIDAL_SURFACE ( 'NONE', #32648, 2.000000000000000000, 1.000000000000000000 ) ;
#56257 = CARTESIAN_POINT ( 'NONE',  ( -134.6950000000000216, -8.437984349512085203, 5.166775262442717831E-16 ) ) ;
#56258 = MECHANICAL_DESIGN_GEOMETRIC_PRESENTATION_REPRESENTATION (  '', ( #59666 ), #1166 ) ;
#56259 = DIRECTION ( 'NONE',  ( 1.000000000000000000, 0.000000000000000000, 0.000000000000000000 ) ) ;
#56260 = AXIS2_PLACEMENT_3D ( 'NONE', #17636, #28481, #49988 ) ;
#56261 = SURFACE_SIDE_STYLE ('',( #34806 ) ) ;
#56262 = ORIENTED_EDGE ( 'NONE', *, *, #66301, .T. ) ;
#56263 = EDGE_LOOP ( 'NONE', ( #34136, #21399, #37284, #9105 ) ) ;
#56264 = VECTOR ( 'NONE', #23399, 1000.000000000000000 ) ;
#56265 = CARTESIAN_POINT ( 'NONE',  ( 32.00000000000000000, 42.00000000000000000, -75.00000000000001421 ) ) ;
#56266 = CARTESIAN_POINT ( 'NONE',  ( -62.24292637653379501, 5.598654528085804216, 7.705886871421366635 ) ) ;
#56267 = ADVANCED_FACE ( 'NONE', ( #13896 ), #68765, .F. ) ;
#56268 = COLOUR_RGB ( '', 0.09019608, 0.27058824, 0.51372549) ;
#56269 = CARTESIAN_POINT ( 'NONE',  ( 8.250000000000001776, 31.24999999999998579, 3.750000000000000000 ) ) ;
#56270 = CARTESIAN_POINT ( 'NONE',  ( 60.00000000000000000, 110.4999999999999858, -10.00000000000000000 ) ) ;
#56271 = CIRCLE ( 'NONE', #66367, 1.000000000000000888 ) ;
#56272 = DIRECTION ( 'NONE',  ( 0.000000000000000000, 0.000000000000000000, -1.000000000000000000 ) ) ;
#56273 = ORIENTED_EDGE ( 'NONE', *, *, #66493, .T. ) ;
#56274 = CARTESIAN_POINT ( 'NONE',  ( -129.3549999999999898, -4.716976649647093289, -6.492361379858945902 ) ) ;
#56275 = ORIENTED_EDGE ( 'NONE', *, *, #51163, .T. ) ;
#56276 = CARTESIAN_POINT ( 'NONE',  ( -122.1570736234661751, -9.058813317711329915, -2.943386871421370898 ) ) ;
#56277 = ORIENTED_EDGE ( 'NONE', *, *, #45263, .T. ) ;
#56278 = LINE ( 'NONE', #61902, #40327 ) ;
#56279 =( LENGTH_UNIT ( ) NAMED_UNIT ( * ) SI_UNIT ( .MILLI., .METRE. ) );
#56280 = EDGE_LOOP ( 'NONE', ( #45766, #43394, #19175, #604 ) ) ;
#56281 = PRESENTATION_LAYER_ASSIGNMENT (  '', '', ( #47348 ) ) ;
#56282 = FACE_OUTER_BOUND ( 'NONE', #67123, .T. ) ;
#56283 = CARTESIAN_POINT ( 'NONE',  ( 8.102448949553183510, 141.9950000000000045, -5.886773742842746238 ) ) ;
#56284 = EDGE_LOOP ( 'NONE', ( #32435, #8544, #58075, #18971, #50933, #16533, #40709, #25234 ) ) ;
#56285 = EDGE_CURVE ( 'NONE', #22594, #5489, #51070, .T. ) ;
#56286 = DIRECTION ( 'NONE',  ( 0.000000000000000000, 0.000000000000000000, -1.000000000000000000 ) ) ;
#56287 = CARTESIAN_POINT ( 'NONE',  ( 5.598654528085805993, 142.3549999999999898, 7.705886871421374629 ) ) ;
#56288 = CARTESIAN_POINT ( 'NONE',  ( 0.000000000000000000, 0.000000000000000000, 0.000000000000000000 ) ) ;
#56289 = CARTESIAN_POINT ( 'NONE',  ( 41.12389261647935967, 107.5649728523252691, -3.335908204272119981 ) ) ;
#56290 = ORIENTED_EDGE ( 'NONE', *, *, #28312, .F. ) ;
#56291 = CARTESIAN_POINT ( 'NONE',  ( -9.827790563157511022E-16, 118.4429263765338192, 8.025000000000000355 ) ) ;
#56292 = CYLINDRICAL_SURFACE ( 'NONE', #48079, 5.000000000000000000 ) ;
#56293 =( NAMED_UNIT ( * ) PLANE_ANGLE_UNIT ( ) SI_UNIT ( $, .RADIAN. ) );
#56294 = ADVANCED_FACE ( 'NONE', ( #69108 ), #35362, .T. ) ;
#56295 =( LENGTH_UNIT ( ) NAMED_UNIT ( * ) SI_UNIT ( .MILLI., .METRE. ) );
#56296 = EDGE_CURVE ( 'NONE', #37694, #41190, #40998, .T. ) ;
#56297 = EDGE_LOOP ( 'NONE', ( #37308, #43580, #7462, #23319 ) ) ;
#56298 = DIRECTION ( 'NONE',  ( 0.000000000000000000, 1.000000000000000000, 0.000000000000000000 ) ) ;
#56299 = ORIENTED_EDGE ( 'NONE', *, *, #62001, .F. ) ;
#56300 = DIRECTION ( 'NONE',  ( 0.7833176619561811327, 0.6216216216216278179, -0.000000000000000000 ) ) ;
#56301 = CARTESIAN_POINT ( 'NONE',  ( -51.84221223720477667, -9.947368421052628307, 4.481646853389226415 ) ) ;
#56303 = CARTESIAN_POINT ( 'NONE',  ( -165.3549999999999898, -4.716976649647093289, -6.492361379858945902 ) ) ;
#56302 = PRESENTATION_LAYER_ASSIGNMENT (  '', '', ( #10280 ) ) ;
#56304 = ORIENTED_EDGE ( 'NONE', *, *, #38298, .T. ) ;
#56305 = SURFACE_SIDE_STYLE ('',( #7450 ) ) ;
#56306 = ADVANCED_FACE ( 'NONE', ( #53605 ), #478, .T. ) ;
#56307 = COLOUR_RGB ( '', 0.08235294, 0.09019608, 0.10196078) ;
#56308 = FILL_AREA_STYLE ('',( #23612 ) ) ;
#56309 = CARTESIAN_POINT ( 'NONE',  ( -84.49999999999998579, -2.499999999999999556, 0.000000000000000000 ) ) ;
#56310 = CARTESIAN_POINT ( 'NONE',  ( 45.00000000000000000, 9.905302582396059208, -6.348323522272433017 ) ) ;
#56311 = EDGE_LOOP ( 'NONE', ( #14446, #18222, #1997, #49597 ) ) ;
#56313 = ADVANCED_FACE ( 'NONE', ( #21957 ), #69441, .T. ) ;
#56312 = ORIENTED_EDGE ( 'NONE', *, *, #21352, .T. ) ;
#56314 = DIRECTION ( 'NONE',  ( 1.000000000000000000, 0.000000000000000000, 0.000000000000000000 ) ) ;
#56315 = CYLINDRICAL_SURFACE ( 'NONE', #61614, 8.025000000000000355 ) ;
#56316 = CARTESIAN_POINT ( 'NONE',  ( -77.30499999999996419, 8.437984349512085203, -1.550032578732815448E-15 ) ) ;
#56317 = ORIENTED_EDGE ( 'NONE', *, *, #58695, .T. ) ;
#56318 = VECTOR ( 'NONE', #20203, 1000.000000000000000 ) ;
#56319 = FACE_OUTER_BOUND ( 'NONE', #14783, .T. ) ;
#56320 = VECTOR ( 'NONE', #26248, 1000.000000000000000 ) ;
#56321 =( REPRESENTATION_RELATIONSHIP ('NONE','NONE', #5102, #46015 ) REPRESENTATION_RELATIONSHIP_WITH_TRANSFORMATION ( #63459 )SHAPE_REPRESENTATION_RELATIONSHIP( ) );
#56322 =( LENGTH_UNIT ( ) NAMED_UNIT ( * ) SI_UNIT ( .MILLI., .METRE. ) );
#56323 = ORIENTED_EDGE ( 'NONE', *, *, #58090, .T. ) ;
#56324 = CARTESIAN_POINT ( 'NONE',  ( 22.29422224269976027, 26.17759303819800820, -27.50000000000001066 ) ) ;
#56325 = AXIS2_PLACEMENT_3D ( 'NONE', #30834, #24498, #46013 ) ;
#56327 = LINE ( 'NONE', #62312, #53879 ) ;
#56326 = DIRECTION ( 'NONE',  ( 0.000000000000000000, 0.000000000000000000, -1.000000000000000000 ) ) ;
#56328 = CARTESIAN_POINT ( 'NONE',  ( -1.166476076187854022E-15, 143.9449999999999932, 9.525000000000000355 ) ) ;
#56329 = CARTESIAN_POINT ( 'NONE',  ( -103.7949999999999733, 2.607480562269068880, -8.024999999999993250 ) ) ;
#56330 = CIRCLE ( 'NONE', #3520, 0.2500000000000002220 ) ;
#56331 = CYLINDRICAL_SURFACE ( 'NONE', #24041, 0.9999999999999995559 ) ;
#56332 = DIRECTION ( 'NONE',  ( 1.000000000000000000, 0.000000000000000000, 0.000000000000000000 ) ) ;
#56333 = EDGE_CURVE ( 'NONE', #23842, #50598, #38522, .T. ) ;
#56334 = CIRCLE ( 'NONE', #51846, 0.2500000000000002220 ) ;
#56335 = VECTOR ( 'NONE', #9094, 1000.000000000000000 ) ;
#56337 = LINE ( 'NONE', #62643, #6673 ) ;
#56336 = CARTESIAN_POINT ( 'NONE',  ( 27.00000000000001776, 14.00000000000000000, -60.00402776293827145 ) ) ;
#56338 = CARTESIAN_POINT ( 'NONE',  ( -141.5929263765337680, -3.094860106618431139, -9.524999999999991473 ) ) ;
#56339 = SURFACE_SIDE_STYLE ('',( #51423 ) ) ;
#56340 = CARTESIAN_POINT ( 'NONE',  ( -169.3449999999999989, 7.632228543268599452, -2.479861379858951942 ) ) ;
#56341 = VECTOR ( 'NONE', #34428, 1000.000000000000227 ) ;
#56342 = LINE ( 'NONE', #3173, #68546 ) ;
#56343 = VERTEX_POINT ( 'NONE', #5741 ) ;
#56344 = LINE ( 'NONE', #19045, #2391 ) ;
#56345 = ORIENTED_EDGE ( 'NONE', *, *, #16332, .F. ) ;
#56346 = AXIS2_PLACEMENT_3D ( 'NONE', #62682, #24362, #56749 ) ;
#56347 =( GEOMETRIC_REPRESENTATION_CONTEXT ( 3 ) GLOBAL_UNCERTAINTY_ASSIGNED_CONTEXT ( ( #16558 ) ) GLOBAL_UNIT_ASSIGNED_CONTEXT ( ( #802, #64899, #65249 ) ) REPRESENTATION_CONTEXT ( 'NONE', 'WORKASPACE' ) );
#56348 = DIRECTION ( 'NONE',  ( -0.000000000000000000, -0.000000000000000000, 1.000000000000000000 ) ) ;
#56349 = CARTESIAN_POINT ( 'NONE',  ( 6.000000000000017764, -35.45414562583513884, -57.63767942241966580 ) ) ;
#56350 = CARTESIAN_POINT ( 'NONE',  ( 44.64644201180199445, 9.999999999999980460, -3.314822853082296295 ) ) ;
#56351 = AXIS2_PLACEMENT_3D ( 'NONE', #61800, #46032, #13631 ) ;
#56353 = MECHANICAL_DESIGN_GEOMETRIC_PRESENTATION_REPRESENTATION (  '', ( #9076 ), #46163 ) ;
#56352 = CARTESIAN_POINT ( 'NONE',  ( -15.98999599679679839, 146.9999999999999716, 9.500000000000000000 ) ) ;
#56354 = ORIENTED_EDGE ( 'NONE', *, *, #12298, .F. ) ;
#56355 = CARTESIAN_POINT ( 'NONE',  ( -157.5550000000000068, 0.000000000000000000, 8.024999999999991473 ) ) ;
#56356 = ORIENTED_EDGE ( 'NONE', *, *, #42686, .F. ) ;
#56357 = CARTESIAN_POINT ( 'NONE',  ( -195.0000000000000000, 1.166476076187852838E-15, -9.524999999999991473 ) ) ;
#56359 = EDGE_CURVE ( 'NONE', #28296, #30333, #51340, .T. ) ;
#56358 = PRESENTATION_STYLE_ASSIGNMENT (( #13447 ) ) ;
#56360 = CIRCLE ( 'NONE', #68797, 7.500000000000000000 ) ;
#56361 = EDGE_LOOP ( 'NONE', ( #1999, #14691, #46470, #1444 ) ) ;
#56362 = DIRECTION ( 'NONE',  ( 0.000000000000000000, 0.000000000000000000, 1.000000000000000000 ) ) ;
#56363 =( GEOMETRIC_REPRESENTATION_CONTEXT ( 3 ) GLOBAL_UNCERTAINTY_ASSIGNED_CONTEXT ( ( #39820 ) ) GLOBAL_UNIT_ASSIGNED_CONTEXT ( ( #34408, #1971, #24520 ) ) REPRESENTATION_CONTEXT ( 'NONE', 'WORKASPACE' ) );
#56364 = DIRECTION ( 'NONE',  ( 0.000000000000000000, 0.000000000000000000, 1.000000000000000000 ) ) ;
#56365 = CARTESIAN_POINT ( 'NONE',  ( 5.598654528085809545, 115.1449999999999818, -7.705886871421373741 ) ) ;
#56366 = VECTOR ( 'NONE', #35887, 1000.000000000000000 ) ;
#56367 = ORIENTED_EDGE ( 'NONE', *, *, #36239, .T. ) ;
#56368 = EDGE_CURVE ( 'NONE', #55502, #31194, #12884, .T. ) ;
#56369 = CARTESIAN_POINT ( 'NONE',  ( 66.24999999999998579, 34.24999999999999289, 4.000000000000000000 ) ) ;
#56370 = CARTESIAN_POINT ( 'NONE',  ( 24.21231517720798010, 112.9999999999999858, 9.500000000000000000 ) ) ;
#56371 = CARTESIAN_POINT ( 'NONE',  ( -72.35499999999998977, -4.716976649647093289, -6.492361379858945902 ) ) ;
#56372 = CARTESIAN_POINT ( 'NONE',  ( 8.102448949553183510, 134.1049999999999329, -5.886773742842746238 ) ) ;
#56373 = AXIS2_PLACEMENT_3D ( 'NONE', #45513, #3176, #55665 ) ;
#56374 =( NAMED_UNIT ( * ) PLANE_ANGLE_UNIT ( ) SI_UNIT ( $, .RADIAN. ) );
#56375 = DIRECTION ( 'NONE',  ( 0.000000000000000000, 0.000000000000000000, 1.000000000000000000 ) ) ;
#56376 = ADVANCED_FACE ( 'NONE', ( #59915 ), #11786, .F. ) ;
#56377 = AXIS2_PLACEMENT_3D ( 'NONE', #45562, #66982, #28955 ) ;
#56378 = DIRECTION ( 'NONE',  ( 3.469446951953610639E-15, -1.000000000000000000, 0.000000000000000000 ) ) ;
#56379 = AXIS2_PLACEMENT_3D ( 'NONE', #53801, #27049, #6309 ) ;
#56380 = CARTESIAN_POINT ( 'NONE',  ( 24.21231517720798010, 113.4999999999999858, 7.000000000000000000 ) ) ;
#56381 = ORIENTED_EDGE ( 'NONE', *, *, #46425, .F. ) ;
#56382 = SURFACE_STYLE_USAGE ( .BOTH. , #40234 ) ;
#56383 = SPHERICAL_SURFACE ( 'NONE', #17184, 0.5000000000000000000 ) ;
#56384 = CARTESIAN_POINT ( 'NONE',  ( -54.74499999999999034, 4.716976649647094177, 6.492361379858945902 ) ) ;
#56385 = ORIENTED_EDGE ( 'NONE', *, *, #15492, .F. ) ;
#56386 = DIRECTION ( 'NONE',  ( 0.000000000000000000, -0.000000000000000000, 1.000000000000000000 ) ) ;
#56387 = VECTOR ( 'NONE', #11410, 1000.000000000000000 ) ;
#56388 = CARTESIAN_POINT ( 'NONE',  ( -44.99999999999998579, 119.9999999999999716, 9.500000000000000000 ) ) ;
#56389 = DIRECTION ( 'NONE',  ( -0.000000000000000000, -1.000000000000000000, 0.000000000000000000 ) ) ;
#56390 = ORIENTED_EDGE ( 'NONE', *, *, #47455, .F. ) ;
#56391 = CARTESIAN_POINT ( 'NONE',  ( -51.97253254664954625, -11.33456255750827602, 1.777144971367008441 ) ) ;
#56392 = CARTESIAN_POINT ( 'NONE',  ( -49.94499999999998607, -9.827790563157499189E-16, -8.024999999999991473 ) ) ;
#56393 = PRESENTATION_STYLE_ASSIGNMENT (( #45195 ) ) ;
#56394 = ORIENTED_EDGE ( 'NONE', *, *, #39425, .F. ) ;
#56395 = AXIS2_PLACEMENT_3D ( 'NONE', #51826, #25080, #68011 ) ;
#56396 = EDGE_CURVE ( 'NONE', #10181, #15297, #1635, .T. ) ;
#56397 =( NAMED_UNIT ( * ) PLANE_ANGLE_UNIT ( ) SI_UNIT ( $, .RADIAN. ) );
#56398 = CARTESIAN_POINT ( 'NONE',  ( -107.3049999999999784, 8.437984349512085203, -1.550032578732815448E-15 ) ) ;
#56399 = ORIENTED_EDGE ( 'NONE', *, *, #16409, .F. ) ;
#56400 = DIRECTION ( 'NONE',  ( 1.000000000000000000, -0.000000000000000000, 0.000000000000000000 ) ) ;
#56401 = CARTESIAN_POINT ( 'NONE',  ( 0.000000000000000000, 154.9999999999999716, 0.000000000000000000 ) ) ;
#56402 = CARTESIAN_POINT ( 'NONE',  ( -140.3070736234661524, -10.01517768586948698, 6.132527647946031529E-16 ) ) ;
#56403 = MECHANICAL_DESIGN_GEOMETRIC_PRESENTATION_REPRESENTATION (  '', ( #17127 ), #19398 ) ;
#56404 = DIRECTION ( 'NONE',  ( -0.000000000000000000, -0.000000000000000000, 1.000000000000000000 ) ) ;
#56405 = CARTESIAN_POINT ( 'NONE',  ( -5.598654528085806881, 145.7449999999999761, -7.705886871421374629 ) ) ;
#56406 = CARTESIAN_POINT ( 'NONE',  ( -86.90707362346616094, -3.094860106618429807, 9.524999999999991473 ) ) ;
#56407 = TOROIDAL_SURFACE ( 'NONE', #65406, 13.49999999999999822, 0.5000000000000000000 ) ;
#56408 = CIRCLE ( 'NONE', #26073, 0.2500000000000002220 ) ;
#56409 = DIRECTION ( 'NONE',  ( 1.000000000000000000, 1.073081856240828566E-16, 0.000000000000000000 ) ) ;
#56410 = DIRECTION ( 'NONE',  ( -1.000000000000000000, 0.000000000000000000, 0.000000000000000000 ) ) ;
#56412 = FACE_OUTER_BOUND ( 'NONE', #52955, .T. ) ;
#56411 = CONICAL_SURFACE ( 'NONE', #45256, 3.100000000000000533, 0.7853981633974447263 ) ;
#56414 =( NAMED_UNIT ( * ) PLANE_ANGLE_UNIT ( ) SI_UNIT ( $, .RADIAN. ) );
#56413 = CARTESIAN_POINT ( 'NONE',  ( 71.99999999999998579, 119.9999999999997868, -7.500000000000000000 ) ) ;
#56415 = CARTESIAN_POINT ( 'NONE',  ( -126.0550000000000068, -9.827790563157499189E-16, -8.024999999999991473 ) ) ;
#56416 = FACE_OUTER_BOUND ( 'NONE', #10292, .T. ) ;
#56417 = DIRECTION ( 'NONE',  ( 0.000000000000000000, 1.000000000000000000, -0.000000000000000000 ) ) ;
#56418 = STYLED_ITEM ( 'NONE', ( #18494 ), #22466 ) ;
#56419 = CARTESIAN_POINT ( 'NONE',  ( -131.0949999999999989, -2.607480562269071545, -8.024999999999991473 ) ) ;
#56420 = CARTESIAN_POINT ( 'NONE',  ( -115.6449999999999818, 4.716976649647091513, -6.492361379858946790 ) ) ;
#56421 = COLOUR_RGB ( '', 0.66274510, 0.83137255, 0.94901961) ;
#56422 = CARTESIAN_POINT ( 'NONE',  ( 53.00000000000000000, 24.74999999999998224, -3.750000000000000000 ) ) ;
#56423 = EDGE_CURVE ( 'NONE', #50024, #11058, #41045, .T. ) ;
#56424 = EDGE_LOOP ( 'NONE', ( #68310, #6997, #53992, #56624 ) ) ;
#56425 = CIRCLE ( 'NONE', #18211, 0.5000000000000004441 ) ;
#56426 = DIRECTION ( 'NONE',  ( 1.000000000000000000, 2.312964634635707951E-15, 0.000000000000000000 ) ) ;
#56427 = CARTESIAN_POINT ( 'NONE',  ( -45.00000000000000000, 99.99999999999992895, -9.500000000000000000 ) ) ;
#56428 = CARTESIAN_POINT ( 'NONE',  ( -168.4429263765337907, -1.166476076187852838E-15, -9.524999999999991473 ) ) ;
#56429 = SURFACE_STYLE_FILL_AREA ( #34980 ) ;
#56430 = CARTESIAN_POINT ( 'NONE',  ( -51.29499999999997328, -2.607480562269069768, 8.024999999999991473 ) ) ;
#56431 = MECHANICAL_DESIGN_GEOMETRIC_PRESENTATION_REPRESENTATION (  '', ( #47502 ), #58692 ) ;
#56432 = SURFACE_STYLE_FILL_AREA ( #36686 ) ;
#56433 = AXIS2_PLACEMENT_3D ( 'NONE', #9802, #52706, #9101 ) ;
#56434 = CARTESIAN_POINT ( 'NONE',  ( -15.00000000000000000, 8.000000000000000000, 4.000000000000000000 ) ) ;
#56435 = DIRECTION ( 'NONE',  ( -0.000000000000000000, -0.000000000000000000, 1.000000000000000000 ) ) ;
#56436 = ORIENTED_EDGE ( 'NONE', *, *, #36067, .T. ) ;
#56437 = PRODUCT_DEFINITION_CONTEXT ( 'detailed design', #50483, 'design' ) ;
#56438 = CARTESIAN_POINT ( 'NONE',  ( -85.19292637653381917, -10.01517768586948698, 6.132527647946031529E-16 ) ) ;
#56439 = APPLICATION_PROTOCOL_DEFINITION ( 'draft international standard', 'automotive_design', 1998, #38410 ) ;
#56440 = CARTESIAN_POINT ( 'NONE',  ( -34.99999999999999289, 99.99999999999998579, 10.00000000000000000 ) ) ;
#56441 = COLOUR_RGB ( '', 0.31764706, 0.68627451, 0.89019608) ;
#56442 = SURFACE_STYLE_USAGE ( .BOTH. , #3999 ) ;
#56443 = CARTESIAN_POINT ( 'NONE',  ( -79.40707362346617515, 3.094860106618428031, -9.524999999999993250 ) ) ;
#56444 = VECTOR ( 'NONE', #21897, 1000.000000000000000 ) ;
#56445 = ORIENTED_EDGE ( 'NONE', *, *, #12392, .T. ) ;
#56446 = CARTESIAN_POINT ( 'NONE',  ( -15.98999599679679839, 146.4999999999999716, 7.500000000000000000 ) ) ;
#56448 = EDGE_CURVE ( 'NONE', #18730, #63828, #2509, .T. ) ;
#56447 = SURFACE_SIDE_STYLE ('',( #34999 ) ) ;
#56449 = VERTEX_POINT ( 'NONE', #22640 ) ;
#56450 = FACE_OUTER_BOUND ( 'NONE', #21891, .T. ) ;
#56451 = PRESENTATION_LAYER_ASSIGNMENT (  '', '', ( #17339 ) ) ;
#56452 = VECTOR ( 'NONE', #54704, 1000.000000000000000 ) ;
#56453 = CARTESIAN_POINT ( 'NONE',  ( 6.826472737025121695, 129.6070736234661638, -4.959722759717905660 ) ) ;
#56454 = CARTESIAN_POINT ( 'NONE',  ( 0.000000000000000000, 87.30187232391182306, 8.025000000000000355 ) ) ;
#56455 = CARTESIAN_POINT ( 'NONE',  ( 75.00000000000000000, 19.46449454893560116, -6.525737028834473819 ) ) ;
#56456 =( GEOMETRIC_REPRESENTATION_CONTEXT ( 3 ) GLOBAL_UNCERTAINTY_ASSIGNED_CONTEXT ( ( #38528 ) ) GLOBAL_UNIT_ASSIGNED_CONTEXT ( ( #6453, #53619, #5407 ) ) REPRESENTATION_CONTEXT ( 'NONE', 'WORKASPACE' ) );
#56457 = CARTESIAN_POINT ( 'NONE',  ( -49.75000000000000000, 2.168404344971008128E-16, -5.100000000000000533 ) ) ;
#56458 = ORIENTED_EDGE ( 'NONE', *, *, #30772, .F. ) ;
#56459 = CARTESIAN_POINT ( 'NONE',  ( 74.50000000000000000, 3.473944261090200865E-15, -6.999999999999999112 ) ) ;
#56460 = ADVANCED_FACE ( 'NONE', ( #12405, #1099, #49725, #24018 ), #7152, .T. ) ;
#56461 = DIRECTION ( 'NONE',  ( 1.000000000000000000, 0.000000000000000000, 0.000000000000000000 ) ) ;
#56462 = CARTESIAN_POINT ( 'NONE',  ( 2.999999999999993339, 5.000000000000000000, 24.00402776293822882 ) ) ;
#56463 = PRESENTATION_LAYER_ASSIGNMENT (  '', '', ( #44119 ) ) ;
#56464 = ADVANCED_FACE ( 'NONE', ( #17391 ), #28216, .T. ) ;
#56465 = CARTESIAN_POINT ( 'NONE',  ( -71.75707362346616947, -5.598654528085801552, 7.705886871421367523 ) ) ;
#56466 = CARTESIAN_POINT ( 'NONE',  ( -78.29499999999997328, -2.607480562269069768, 8.024999999999991473 ) ) ;
#56467 = ORIENTED_EDGE ( 'NONE', *, *, #3438, .T. ) ;
#56468 = COLOUR_RGB ( '', 0.08235294, 0.09019608, 0.10196078) ;
#56469 = CARTESIAN_POINT ( 'NONE',  ( 12.72792206135785875, 1.797044900979284448E-15, -10.00000000000000000 ) ) ;
#56470 = CARTESIAN_POINT ( 'NONE',  ( -60.00000000000000000, -2.024042244987997205E-14, 11.50000000000003020 ) ) ;
#56471 = EDGE_CURVE ( 'NONE', #58037, #55052, #45527, .T. ) ;
#56472 = SURFACE_SIDE_STYLE ('',( #4031 ) ) ;
#56473 = UNCERTAINTY_MEASURE_WITH_UNIT (LENGTH_MEASURE( 1.000000000000000082E-05 ), #17388, 'distance_accuracy_value', 'NONE');
#56474 = ORIENTED_EDGE ( 'NONE', *, *, #19814, .T. ) ;
#56475 = CARTESIAN_POINT ( 'NONE',  ( -75.59292637653379643, -3.094860106618431139, -9.524999999999991473 ) ) ;
#56476 = SURFACE_STYLE_USAGE ( .BOTH. , #40319 ) ;
#56477 = MECHANICAL_DESIGN_GEOMETRIC_PRESENTATION_REPRESENTATION (  '', ( #46440 ), #65476 ) ;
#56478 = ADVANCED_FACE ( 'NONE', ( #34229 ), #55683, .F. ) ;
#56479 = DIRECTION ( 'NONE',  ( 0.000000000000000000, 0.000000000000000000, -1.000000000000000000 ) ) ;
#56480 = VERTEX_POINT ( 'NONE', #63030 ) ;
#56481 = VERTEX_POINT ( 'NONE', #41613 ) ;
#56482 = FILL_AREA_STYLE ('',( #60369 ) ) ;
#56483 = DIRECTION ( 'NONE',  ( 0.000000000000000000, 0.000000000000000000, 1.000000000000000000 ) ) ;
#56484 = CARTESIAN_POINT ( 'NONE',  ( 27.00000000000001776, 42.00000000000000000, 34.49999999999999289 ) ) ;
#56485 = CARTESIAN_POINT ( 'NONE',  ( -164.9070736234662036, -3.094860106618429807, 9.524999999999991473 ) ) ;
#56486 = CARTESIAN_POINT ( 'NONE',  ( -18.00000000000000711, 30.99999999999999289, 3.750000000000000000 ) ) ;
#56487 = CARTESIAN_POINT ( 'NONE',  ( -9.058813317711337021, 113.0449999999999875, -2.943386871421374895 ) ) ;
#56488 = CARTESIAN_POINT ( 'NONE',  ( -117.6570736234661894, 9.058813317711329915, 2.943386871421369566 ) ) ;
#56489 = DIRECTION ( 'NONE',  ( 0.000000000000000000, 1.000000000000000000, 0.000000000000000000 ) ) ;
#56490 = CARTESIAN_POINT ( 'NONE',  ( -69.05707362346618083, 0.000000000000000000, 9.524999999999991473 ) ) ;
#56491 = ORIENTED_EDGE ( 'NONE', *, *, #42790, .T. ) ;
#56492 = CARTESIAN_POINT ( 'NONE',  ( 44.50000000000000000, 99.99999999999992895, 3.500000000000000000 ) ) ;
#56493 =( NAMED_UNIT ( * ) SI_UNIT ( $, .STERADIAN. ) SOLID_ANGLE_UNIT ( ) );
#56494 = DIRECTION ( 'NONE',  ( 0.000000000000000000, 1.000000000000000000, 0.000000000000000000 ) ) ;
#56495 = SURFACE_STYLE_USAGE ( .BOTH. , #23441 ) ;
#56496 = CARTESIAN_POINT ( 'NONE',  ( -152.6050000000000182, 6.826472737025113702, -4.959722759717902107 ) ) ;
#56497 = CARTESIAN_POINT ( 'NONE',  ( -75.00000000000000000, 9.290263934145983171, 6.640705990143894510 ) ) ;
#56498 = CARTESIAN_POINT ( 'NONE',  ( -147.4429263765338192, -1.166476076187852838E-15, -9.524999999999991473 ) ) ;
#56499 = CARTESIAN_POINT ( 'NONE',  ( -165.4450000000000216, 0.000000000000000000, 8.024999999999991473 ) ) ;
#56500 = TOROIDAL_SURFACE ( 'NONE', #29537, 7.500000000000011546, 0.5000000000000000000 ) ;
#56501 = CARTESIAN_POINT ( 'NONE',  ( -146.8449999999999989, -7.632228543268599452, 2.479861379858951054 ) ) ;
#56502 = ORIENTED_EDGE ( 'NONE', *, *, #43481, .F. ) ;
#56503 = DIRECTION ( 'NONE',  ( 0.000000000000000000, 0.000000000000000000, 1.000000000000000000 ) ) ;
#56504 = CARTESIAN_POINT ( 'NONE',  ( -123.4429263765338192, -1.166476076187852838E-15, -9.524999999999991473 ) ) ;
#56505 = CARTESIAN_POINT ( 'NONE',  ( -61.10499999999997556, -6.826472737025115478, 4.959722759717900331 ) ) ;
#56506 = CARTESIAN_POINT ( 'NONE',  ( -40.70406133565712992, -11.89285714285713880, 3.265330863013268026 ) ) ;
#56507 = DIRECTION ( 'NONE',  ( 0.000000000000000000, 0.000000000000000000, 1.000000000000000000 ) ) ;
#56508 = CARTESIAN_POINT ( 'NONE',  ( -59.39499999999998892, -6.826472737025113702, -4.959722759717900331 ) ) ;
#56509 = CARTESIAN_POINT ( 'NONE',  ( -10.01517768586949231, 150.3050000000000068, -6.132527647946036459E-16 ) ) ;
#56510 = CARTESIAN_POINT ( 'NONE',  ( -48.50000000000000000, 99.99999999999992895, -7.000000000000000000 ) ) ;
#56511 = CIRCLE ( 'NONE', #41964, 0.5000000000000004441 ) ;
#56512 = UNCERTAINTY_MEASURE_WITH_UNIT (LENGTH_MEASURE( 1.000000000000000082E-05 ), #37966, 'distance_accuracy_value', 'NONE');
#56513 = AXIS2_PLACEMENT_3D ( 'NONE', #34846, #56298, #8131 ) ;
#56514 = DIRECTION ( 'NONE',  ( -1.000000000000000000, 0.000000000000000000, 0.000000000000000000 ) ) ;
#56515 = CARTESIAN_POINT ( 'NONE',  ( -20.22843684326250369, 114.9428328902810676, -10.38991920486588327 ) ) ;
#56516 = STYLED_ITEM ( 'NONE', ( #14486 ), #30408 ) ;
#56517 =( NAMED_UNIT ( * ) PLANE_ANGLE_UNIT ( ) SI_UNIT ( $, .RADIAN. ) );
#56518 = PRESENTATION_LAYER_ASSIGNMENT (  '', '', ( #38606 ) ) ;
#56519 = CIRCLE ( 'NONE', #47614, 9.000000000000000000 ) ;
#56520 = CARTESIAN_POINT ( 'NONE',  ( 3.999798566743338668, 58.31681314173471975, 6.349999999999996092 ) ) ;
#56521 = EDGE_CURVE ( 'NONE', #65809, #58402, #37429, .T. ) ;
#56522 = CARTESIAN_POINT ( 'NONE',  ( 36.00000000000002842, 5.000000000000000000, 29.00402776293825724 ) ) ;
#56523 = ORIENTED_EDGE ( 'NONE', *, *, #34532, .F. ) ;
#56524 = ORIENTED_EDGE ( 'NONE', *, *, #57023, .T. ) ;
#56525 = CARTESIAN_POINT ( 'NONE',  ( 71.50000000000000000, 35.92875272052971525, -9.500000000000000000 ) ) ;
#56526 = EDGE_CURVE ( 'NONE', #30954, #26439, #68676, .T. ) ;
#56527 = VECTOR ( 'NONE', #34093, 1000.000000000000000 ) ;
#56528 = ADVANCED_FACE ( 'NONE', ( #36357 ), #24351, .T. ) ;
#56529 = LINE ( 'NONE', #7323, #49661 ) ;
#56530 = EDGE_CURVE ( 'NONE', #44609, #599, #32028, .T. ) ;
#56531 = DIRECTION ( 'NONE',  ( 1.000000000000000000, 0.000000000000000000, 0.000000000000000000 ) ) ;
#56532 = ORIENTED_EDGE ( 'NONE', *, *, #15385, .T. ) ;
#56533 = ORIENTED_EDGE ( 'NONE', *, *, #35286, .F. ) ;
#56534 = EDGE_CURVE ( 'NONE', #52976, #50401, #69095, .T. ) ;
#56535 = ORIENTED_EDGE ( 'NONE', *, *, #45184, .F. ) ;
#56536 = CARTESIAN_POINT ( 'NONE',  ( -8.102448949553181734, 114.0049999999999812, -5.886773742842749790 ) ) ;
#56537 = CARTESIAN_POINT ( 'NONE',  ( -145.6429263765338078, -5.598654528085801552, 7.705886871421367523 ) ) ;
#56538 = VERTEX_POINT ( 'NONE', #25739 ) ;
#56539 = EDGE_CURVE ( 'NONE', #63248, #19250, #39892, .T. ) ;
#56540 = VECTOR ( 'NONE', #28704, 1000.000000000000000 ) ;
#56541 = PRESENTATION_LAYER_ASSIGNMENT (  '', '', ( #34109 ) ) ;
#56542 = FACE_OUTER_BOUND ( 'NONE', #52406, .T. ) ;
#56543 = CARTESIAN_POINT ( 'NONE',  ( -111.1449999999999960, -4.716976649647092401, 6.492361379858946790 ) ) ;
#56544 = ORIENTED_EDGE ( 'NONE', *, *, #11771, .F. ) ;
#56545 = DIRECTION ( 'NONE',  ( -0.000000000000000000, -1.000000000000000000, -0.000000000000000000 ) ) ;
#56546 = DIRECTION ( 'NONE',  ( -0.000000000000000000, 0.000000000000000000, 1.000000000000000000 ) ) ;
#56547 = CARTESIAN_POINT ( 'NONE',  ( -14.33487782743413064, -10.92424365012867504, -4.966485406155142890 ) ) ;
#56548 = PRESENTATION_LAYER_ASSIGNMENT (  '', '', ( #17288 ) ) ;
#56549 = EDGE_CURVE ( 'NONE', #9757, #21109, #41981, .T. ) ;
#56550 = LINE ( 'NONE', #67114, #13905 ) ;
#56551 = ORIENTED_EDGE ( 'NONE', *, *, #49043, .T. ) ;
#56552 = CARTESIAN_POINT ( 'NONE',  ( 8.437984349512095861, 146.1929263765337907, 1.550032578732817026E-15 ) ) ;
#56553 = DIRECTION ( 'NONE',  ( -0.000000000000000000, 1.000000000000000000, -0.000000000000000000 ) ) ;
#56554 = DIRECTION ( 'NONE',  ( -1.000000000000000000, -0.000000000000000000, -0.000000000000000000 ) ) ;
#56555 = FACE_OUTER_BOUND ( 'NONE', #50031, .T. ) ;
#56556 = DIRECTION ( 'NONE',  ( -0.000000000000000000, -0.000000000000000000, -1.000000000000000000 ) ) ;
#56557 = AXIS2_PLACEMENT_3D ( 'NONE', #20184, #46981, #2927 ) ;
#56558 = ORIENTED_EDGE ( 'NONE', *, *, #17028, .F. ) ;
#56559 = CARTESIAN_POINT ( 'NONE',  ( 44.25000000000000000, 21.74999999999998579, -4.000000000000000000 ) ) ;
#56560 = VERTEX_POINT ( 'NONE', #19429 ) ;
#56561 = DIRECTION ( 'NONE',  ( 0.000000000000000000, -0.000000000000000000, 1.000000000000000000 ) ) ;
#56562 = FACE_OUTER_BOUND ( 'NONE', #40387, .T. ) ;
#56563 = DIRECTION ( 'NONE',  ( 0.000000000000000000, 0.000000000000000000, -1.000000000000000000 ) ) ;
#56564 = CARTESIAN_POINT ( 'NONE',  ( -158.0070736234661695, -8.102448949553174629, -5.886773742842741797 ) ) ;
#56565 = CARTESIAN_POINT ( 'NONE',  ( -135.5049999999999670, -6.826472737025115478, -4.959722759717899443 ) ) ;
#56566 = PRESENTATION_LAYER_ASSIGNMENT (  '', '', ( #25140 ) ) ;
#56567 = FACE_BOUND ( 'NONE', #67536, .T. ) ;
#56568 =( BOUNDED_CURVE ( )  B_SPLINE_CURVE ( 2, ( #25699, #47930, #299, #64035, #52818, #58768, #26724, #59105, #69331, #36671, #21832 ),
 .UNSPECIFIED., .F., .F. ) 
 B_SPLINE_CURVE_WITH_KNOTS ( ( 3, 2, 2, 2, 2, 3 ),
 ( 0.3235294117647058987, 0.3294117647058823484, 0.3352941176470587981, 0.3411764705882353033, 0.3470588235294117530, 0.3529411764705882582 ),
 .UNSPECIFIED. ) 
 CURVE ( )  GEOMETRIC_REPRESENTATION_ITEM ( )  RATIONAL_B_SPLINE_CURVE ( ( 1.000000000000000000, 0.9510565162951535312, 1.000000000000000000, 0.9510565162951535312, 1.000000000000000000, 0.9510565162951535312, 1.000000000000000000, 0.9510565162951535312, 1.000000000000000000, 0.9510565162951535312, 1.000000000000000000 ) ) 
 REPRESENTATION_ITEM ( '' )  );
#56569 = DIRECTION ( 'NONE',  ( -1.000000000000000000, 0.000000000000000000, 0.000000000000000000 ) ) ;
#56570 = ORIENTED_EDGE ( 'NONE', *, *, #22798, .F. ) ;
#56571 =( LENGTH_UNIT ( ) NAMED_UNIT ( * ) SI_UNIT ( .MILLI., .METRE. ) );
#56572 = CIRCLE ( 'NONE', #42027, 0.2500000000000002220 ) ;
#56573 = DIRECTION ( 'NONE',  ( -0.7292845505553197105, -0.6842105263157864936, -0.000000000000000000 ) ) ;
#56575 = SURFACE_SIDE_STYLE ('',( #40420 ) ) ;
#56574 = VECTOR ( 'NONE', #60755, 1000.000000000000000 ) ;
#56576 = DIRECTION ( 'NONE',  ( 0.000000000000000000, 0.000000000000000000, -1.000000000000000000 ) ) ;
#56577 = ORIENTED_EDGE ( 'NONE', *, *, #23293, .F. ) ;
#56578 = VERTEX_POINT ( 'NONE', #57064 ) ;
#56579 = TOROIDAL_SURFACE ( 'NONE', #22906, 0.5000000000000000000, 0.2500000000000000000 ) ;
#56580 = CARTESIAN_POINT ( 'NONE',  ( -31.70202421807500315, -8.271493738783197713, -1.899217192902302509 ) ) ;
#56581 = CARTESIAN_POINT ( 'NONE',  ( 34.99999999999992895, 109.9999999999999858, -9.500000000000000000 ) ) ;
#56582 = CIRCLE ( 'NONE', #21741, 0.2500000000000002220 ) ;
#56583 = SURFACE_SIDE_STYLE ('',( #35129 ) ) ;
#56584 = VERTEX_POINT ( 'NONE', #62672 ) ;
#56585 =( LENGTH_UNIT ( ) NAMED_UNIT ( * ) SI_UNIT ( .MILLI., .METRE. ) );
#56586 = CARTESIAN_POINT ( 'NONE',  ( -180.0550000000000068, -9.827790563157499189E-16, -8.024999999999991473 ) ) ;
#56587 = CARTESIAN_POINT ( 'NONE',  ( 6.000000000000017764, 14.00000000000000533, -35.50000000000000000 ) ) ;
#56588 = DIRECTION ( 'NONE',  ( 0.000000000000000000, 0.000000000000000000, 1.000000000000000000 ) ) ;
#56589 = CARTESIAN_POINT ( 'NONE',  ( -51.65707362346616804, 9.058813317711329915, 2.943386871421369566 ) ) ;
#56590 = AXIS2_PLACEMENT_3D ( 'NONE', #48908, #10882, #42942 ) ;
#56591 = CARTESIAN_POINT ( 'NONE',  ( -174.2949999999999875, -2.607480562269069768, 8.024999999999991473 ) ) ;
#56592 = DIRECTION ( 'NONE',  ( 1.000000000000000000, 0.000000000000000000, 0.000000000000000000 ) ) ;
#56593 = VERTEX_POINT ( 'NONE', #35973 ) ;
#56594 = EDGE_CURVE ( 'NONE', #36214, #53938, #66836, .T. ) ;
#56595 = AXIS2_PLACEMENT_3D ( 'NONE', #57547, #13580, #52301 ) ;
#56596 = CARTESIAN_POINT ( 'NONE',  ( -160.5570736234661808, -1.166476076187852838E-15, -9.524999999999991473 ) ) ;
#56597 = TOROIDAL_SURFACE ( 'NONE', #67797, 16.50000000000000000, 0.5000000000000000000 ) ;
#56598 = LINE ( 'NONE', #8062, #13571 ) ;
#56599 = CARTESIAN_POINT ( 'NONE',  ( -96.50499999999998124, -6.826472737025115478, -4.959722759717899443 ) ) ;
#56600 = LINE ( 'NONE', #34447, #35364 ) ;
#56601 = SURFACE_STYLE_FILL_AREA ( #7709 ) ;
#56602 =( LENGTH_UNIT ( ) NAMED_UNIT ( * ) SI_UNIT ( .MILLI., .METRE. ) );
#56603 = VECTOR ( 'NONE', #49846, 1000.000000000000000 ) ;
#56604 = CARTESIAN_POINT ( 'NONE',  ( -101.5449999999999875, -7.632228543268600340, -2.479861379858950166 ) ) ;
#56605 = CARTESIAN_POINT ( 'NONE',  ( 5.598654528085805993, 115.3549999999999898, 7.705886871421374629 ) ) ;
#56606 = CARTESIAN_POINT ( 'NONE',  ( -63.89499999999998181, 6.826472737025116366, 4.959722759717898555 ) ) ;
#56607 = CARTESIAN_POINT ( 'NONE',  ( 33.00000000000000711, 14.00000000000000000, -36.50000000000000000 ) ) ;
#56608 = AXIS2_PLACEMENT_3D ( 'NONE', #57227, #19936, #15055 ) ;
#56609 = CARTESIAN_POINT ( 'NONE',  ( -83.49999999999998579, 4.336808689942018722E-16, 24.00000000000000000 ) ) ;
#56610 = UNCERTAINTY_MEASURE_WITH_UNIT (LENGTH_MEASURE( 1.000000000000000082E-05 ), #54495, 'distance_accuracy_value', 'NONE');
#56611 = CARTESIAN_POINT ( 'NONE',  ( 41.49999999999997868, 9.999999999999978684, -3.500000000000000000 ) ) ;
#56612 = VECTOR ( 'NONE', #52460, 1000.000000000000000 ) ;
#56613 = DIRECTION ( 'NONE',  ( 0.000000000000000000, 0.000000000000000000, 1.000000000000000000 ) ) ;
#56614 = ORIENTED_EDGE ( 'NONE', *, *, #12368, .F. ) ;
#56615 = CARTESIAN_POINT ( 'NONE',  ( -112.9429263765338050, 0.000000000000000000, 9.524999999999991473 ) ) ;
#56616 = CARTESIAN_POINT ( 'NONE',  ( -126.7449999999999903, 4.716976649647094177, 6.492361379858945902 ) ) ;
#56617 = CYLINDRICAL_SURFACE ( 'NONE', #50523, 0.5000000000000004441 ) ;
#56618 = CIRCLE ( 'NONE', #19501, 0.2500000000000002220 ) ;
#56619 = EDGE_CURVE ( 'NONE', #3488, #6428, #52173, .T. ) ;
#56620 = DIRECTION ( 'NONE',  ( 0.000000000000000000, 0.000000000000000000, -1.000000000000000000 ) ) ;
#56622 = DIRECTION ( 'NONE',  ( 0.000000000000000000, -0.000000000000000000, 1.000000000000000000 ) ) ;
#56621 = CARTESIAN_POINT ( 'NONE',  ( 57.00000000000000000, 0.000000000000000000, -60.00402776293827145 ) ) ;
#56623 = DIRECTION ( 'NONE',  ( 0.000000000000000000, 0.000000000000000000, -1.000000000000000000 ) ) ;
#56624 = ORIENTED_EDGE ( 'NONE', *, *, #29954, .F. ) ;
#56625 = ORIENTED_EDGE ( 'NONE', *, *, #28203, .F. ) ;
#56626 = PRESENTATION_LAYER_ASSIGNMENT (  '', '', ( #17350 ) ) ;
#56627 = CYLINDRICAL_SURFACE ( 'NONE', #10635, 0.2500000000000002220 ) ;
#56628 =( GEOMETRIC_REPRESENTATION_CONTEXT ( 3 ) GLOBAL_UNCERTAINTY_ASSIGNED_CONTEXT ( ( #27766 ) ) GLOBAL_UNIT_ASSIGNED_CONTEXT ( ( #24801, #9001, #23776 ) ) REPRESENTATION_CONTEXT ( 'NONE', 'WORKASPACE' ) );
#56629 = EDGE_CURVE ( 'NONE', #50943, #19358, #6162, .T. ) ;
#56630 = CIRCLE ( 'NONE', #9446, 8.000000000000007105 ) ;
#56631 = DIRECTION ( 'NONE',  ( 1.000000000000000000, 0.000000000000000000, 0.000000000000000000 ) ) ;
#56632 = SURFACE_STYLE_FILL_AREA ( #61892 ) ;
#56633 = CARTESIAN_POINT ( 'NONE',  ( 8.000000000000030198, 5.000000000000000000, 29.00402776293826079 ) ) ;
#56634 = CARTESIAN_POINT ( 'NONE',  ( -126.9570736234661723, 9.058813317711329915, -2.943386871421373119 ) ) ;
#56635 = ORIENTED_EDGE ( 'NONE', *, *, #36828, .F. ) ;
#56636 = CARTESIAN_POINT ( 'NONE',  ( -131.6049999999999898, 6.826472737025113702, -4.959722759717902107 ) ) ;
#56637 = ORIENTED_EDGE ( 'NONE', *, *, #49481, .F. ) ;
#56638 = CONICAL_SURFACE ( 'NONE', #43236, 8.025000000000000355, 0.7853981633974421728 ) ;
#56639 = DIRECTION ( 'NONE',  ( -1.000000000000000000, 0.000000000000000000, 0.000000000000000000 ) ) ;
#56640 = CARTESIAN_POINT ( 'NONE',  ( -120.6570736234661751, 9.058813317711329915, 2.943386871421369566 ) ) ;
#56641 = ORIENTED_EDGE ( 'NONE', *, *, #1983, .F. ) ;
#56642 = CARTESIAN_POINT ( 'NONE',  ( 5.590169943749474513, 6.123233995736765296E-16, -4.999999999999999112 ) ) ;
#56643 = CARTESIAN_POINT ( 'NONE',  ( 108.3664351561509278, 0.000000000000000000, 18.43563588791581509 ) ) ;
#56644 = ORIENTED_EDGE ( 'NONE', *, *, #6820, .F. ) ;
#56645 = EDGE_CURVE ( 'NONE', #53774, #2421, #34283, .T. ) ;
#56646 = CYLINDRICAL_SURFACE ( 'NONE', #25388, 113.0000000000030127 ) ;
#56647 = CARTESIAN_POINT ( 'NONE',  ( 3.094860106618431583, 138.0949999999999989, 9.525000000000000355 ) ) ;
#56648 = AXIS2_PLACEMENT_3D ( 'NONE', #18099, #60308, #1513 ) ;
#56649 = ORIENTED_EDGE ( 'NONE', *, *, #8824, .F. ) ;
#56650 = CARTESIAN_POINT ( 'NONE',  ( 8.102448949553181734, 137.1049999999999898, -5.886773742842746238 ) ) ;
#56651 = CARTESIAN_POINT ( 'NONE',  ( -11.74999999999999645, -0.9999999999999995559, 19.00000000000000000 ) ) ;
#56652 = EDGE_CURVE ( 'NONE', #51660, #21355, #58459, .T. ) ;
#56653 = LINE ( 'NONE', #9859, #21796 ) ;
#56654 = VERTEX_POINT ( 'NONE', #59841 ) ;
#56655 = CARTESIAN_POINT ( 'NONE',  ( -2.607480562269073765, 117.0929263765338249, -8.025000000000000355 ) ) ;
#56656 = CARTESIAN_POINT ( 'NONE',  ( 2.999999999999996447, 5.000000000000000000, -37.00402776293829277 ) ) ;
#56657 = UNCERTAINTY_MEASURE_WITH_UNIT (LENGTH_MEASURE( 1.000000000000000082E-05 ), #59207, 'distance_accuracy_value', 'NONE');
#56658 =( NAMED_UNIT ( * ) SI_UNIT ( $, .STERADIAN. ) SOLID_ANGLE_UNIT ( ) );
#56659 = CIRCLE ( 'NONE', #26308, 1.000000000000000888 ) ;
#56660 = CARTESIAN_POINT ( 'NONE',  ( 7.750000000000019540, 4.481368979606759023E-15, 4.000000000000000000 ) ) ;
#56661 = ORIENTED_EDGE ( 'NONE', *, *, #41018, .T. ) ;
#56662 = CARTESIAN_POINT ( 'NONE',  ( 41.11245223800544579, 107.5819305320973172, 3.325569371602613344 ) ) ;
#56663 = VERTEX_POINT ( 'NONE', #26760 ) ;
#56664 = DIRECTION ( 'NONE',  ( 0.000000000000000000, 1.000000000000000000, 0.000000000000000000 ) ) ;
#56665 = AXIS2_PLACEMENT_3D ( 'NONE', #49808, #22721, #64918 ) ;
#56666 = AXIS2_PLACEMENT_3D ( 'NONE', #44908, #34320, #61379 ) ;
#56667 = DIRECTION ( 'NONE',  ( 0.000000000000000000, 0.000000000000000000, -1.000000000000000000 ) ) ;
#56668 = DIRECTION ( 'NONE',  ( 0.000000000000000000, 0.000000000000000000, -1.000000000000000000 ) ) ;
#56669 = CARTESIAN_POINT ( 'NONE',  ( -165.6550000000000011, -7.632228543268600340, -2.479861379858950166 ) ) ;
#56670 = VERTEX_POINT ( 'NONE', #37403 ) ;
#56671 = DIRECTION ( 'NONE',  ( 0.000000000000000000, 0.000000000000000000, -1.000000000000000000 ) ) ;
#56672 = UNCERTAINTY_MEASURE_WITH_UNIT (LENGTH_MEASURE( 1.000000000000000082E-05 ), #53806, 'distance_accuracy_value', 'NONE');
#56673 = DIRECTION ( 'NONE',  ( 0.000000000000000000, 0.000000000000000000, -1.000000000000000000 ) ) ;
#56674 = CARTESIAN_POINT ( 'NONE',  ( 75.00000000000000000, 19.30628705663858113, 7.000000000000000888 ) ) ;
#56675 = CARTESIAN_POINT ( 'NONE',  ( 5.196152422706636465, -9.000000000000005329, 7.500000000000000000 ) ) ;
#56676 = EDGE_LOOP ( 'NONE', ( #56755, #49218, #5335, #26471 ) ) ;
#56677 = CARTESIAN_POINT ( 'NONE',  ( -74.50000000000000000, -2.220952357103124925E-14, -9.500000000000000000 ) ) ;
#56678 = ORIENTED_EDGE ( 'NONE', *, *, #47642, .T. ) ;
#56679 = DIRECTION ( 'NONE',  ( 0.000000000000000000, 1.000000000000000000, 0.000000000000000000 ) ) ;
#56680 = DIRECTION ( 'NONE',  ( -0.000000000000000000, -0.000000000000000000, -1.000000000000000000 ) ) ;
#56681 = CARTESIAN_POINT ( 'NONE',  ( -71.90499999999995850, 2.607480562269068880, -8.024999999999993250 ) ) ;
#56683 = ORIENTED_EDGE ( 'NONE', *, *, #4864, .F. ) ;
#56682 =( GEOMETRIC_REPRESENTATION_CONTEXT ( 3 ) GLOBAL_UNCERTAINTY_ASSIGNED_CONTEXT ( ( #2432 ) ) GLOBAL_UNIT_ASSIGNED_CONTEXT ( ( #24097, #7913, #61700 ) ) REPRESENTATION_CONTEXT ( 'NONE', 'WORKASPACE' ) );
#56684 = CARTESIAN_POINT ( 'NONE',  ( -87.50000000000000000, -7.499999999999990230, 0.000000000000000000 ) ) ;
#56685 = CARTESIAN_POINT ( 'NONE',  ( -63.50707362346615525, 8.102448949553176405, 5.886773742842740909 ) ) ;
#56686 = CARTESIAN_POINT ( 'NONE',  ( -4.041451884327381450, -7.000000000000002665, 1.082903768654759791 ) ) ;
#56687 =( BOUNDED_CURVE ( )  B_SPLINE_CURVE ( 2, ( #38587, #811, #1876, #22355, #6862, #17112, #59981, #38923, #33263, #6496, #60325 ),
 .UNSPECIFIED., .F., .F. ) 
 B_SPLINE_CURVE_WITH_KNOTS ( ( 3, 2, 2, 2, 2, 3 ),
 ( 0.7717391304347825942, 0.7739130434782608425, 0.7760869565217390909, 0.7782608695652173392, 0.7804347826086956985, 0.7826086956521739468 ),
 .UNSPECIFIED. ) 
 CURVE ( )  GEOMETRIC_REPRESENTATION_ITEM ( )  RATIONAL_B_SPLINE_CURVE ( ( 1.000000000000000000, 0.9510565162951535312, 1.000000000000000000, 0.9510565162951535312, 1.000000000000000000, 0.9510565162951535312, 1.000000000000000000, 0.9510565162951535312, 1.000000000000000000, 0.9510565162951535312, 1.000000000000000000 ) ) 
 REPRESENTATION_ITEM ( '' )  );
#56688 = EDGE_CURVE ( 'NONE', #45031, #31418, #47967, .T. ) ;
#56689 = FILL_AREA_STYLE_COLOUR ( '', #44808 ) ;
#56690 = AXIS2_PLACEMENT_3D ( 'NONE', #11963, #33419, #13335 ) ;
#56691 = CYLINDRICAL_SURFACE ( 'NONE', #28747, 1.000000000000000888 ) ;
#56692 = ORIENTED_EDGE ( 'NONE', *, *, #21264, .T. ) ;
#56693 = CARTESIAN_POINT ( 'NONE',  ( -32.85469148339993950, -8.952884650950863943, -2.692699799268927219 ) ) ;
#56695 = DIRECTION ( 'NONE',  ( -0.000000000000000000, -1.000000000000000000, -0.000000000000000000 ) ) ;
#56694 = LINE ( 'NONE', #8513, #60538 ) ;
#56696 = COLOUR_RGB ( '', 0.66274510, 0.83137255, 0.94901961) ;
#56697 = CARTESIAN_POINT ( 'NONE',  ( 10.01517768586949231, 135.6949999999999932, 1.839758294383810543E-15 ) ) ;
#56698 = CARTESIAN_POINT ( 'NONE',  ( -95.54499999999998749, -7.632228543268600340, -2.479861379858950166 ) ) ;
#56699 = SURFACE_STYLE_USAGE ( .BOTH. , #40541 ) ;
#56700 = UNCERTAINTY_MEASURE_WITH_UNIT (LENGTH_MEASURE( 1.000000000000000082E-05 ), #65621, 'distance_accuracy_value', 'NONE');
#56701 =( GEOMETRIC_REPRESENTATION_CONTEXT ( 3 ) GLOBAL_UNCERTAINTY_ASSIGNED_CONTEXT ( ( #23673 ) ) GLOBAL_UNIT_ASSIGNED_CONTEXT ( ( #33078, #5278, #38036 ) ) REPRESENTATION_CONTEXT ( 'NONE', 'WORKASPACE' ) );
#56703 = CARTESIAN_POINT ( 'NONE',  ( -41.11245223800543158, 107.5819305320972745, -3.325569371602613788 ) ) ;
#56702 = CARTESIAN_POINT ( 'NONE',  ( 47.50000000000000000, 99.99999999999992895, -10.00000000000000000 ) ) ;
#56704 = AXIS2_PLACEMENT_3D ( 'NONE', #64715, #22493, #10562 ) ;
#56705 = CARTESIAN_POINT ( 'NONE',  ( -144.4429263765337907, -1.166476076187852838E-15, -9.524999999999991473 ) ) ;
#56706 = DIRECTION ( 'NONE',  ( 0.000000000000000000, 0.000000000000000000, -1.000000000000000000 ) ) ;
#56707 = CARTESIAN_POINT ( 'NONE',  ( -163.1949999999999648, 8.437984349512085203, -1.550032578732815448E-15 ) ) ;
#56708 = ADVANCED_FACE ( 'NONE', ( #53196 ), #16279, .T. ) ;
#56709 = AXIS2_PLACEMENT_3D ( 'NONE', #32201, #3067, #59252 ) ;
#56710 = EDGE_CURVE ( 'NONE', #45813, #42291, #66889, .T. ) ;
#56711 = DIRECTION ( 'NONE',  ( 0.000000000000000000, 0.000000000000000000, -1.000000000000000000 ) ) ;
#56712 = CIRCLE ( 'NONE', #57827, 0.5000000000000004441 ) ;
#56713 = SURFACE_SIDE_STYLE ('',( #60924 ) ) ;
#56714 = ORIENTED_EDGE ( 'NONE', *, *, #46847, .T. ) ;
#56715 = CARTESIAN_POINT ( 'NONE',  ( 0.000000000000000000, 127.0570736234661666, -8.025000000000000355 ) ) ;
#56716 = EDGE_LOOP ( 'NONE', ( #2924, #66150, #35873 ) ) ;
#56717 = CIRCLE ( 'NONE', #3913, 0.7499999999999997780 ) ;
#56718 = SURFACE_STYLE_FILL_AREA ( #46556 ) ;
#56719 = UNCERTAINTY_MEASURE_WITH_UNIT (LENGTH_MEASURE( 1.000000000000000082E-05 ), #57986, 'distance_accuracy_value', 'NONE');
#56720 = EDGE_CURVE ( 'NONE', #1408, #27268, #5315, .T. ) ;
#56721 = FACE_OUTER_BOUND ( 'NONE', #23518, .T. ) ;
#56722 = CARTESIAN_POINT ( 'NONE',  ( -45.00000000000000000, 7.967232421023206612, 7.000000003139142279 ) ) ;
#56723 = DIRECTION ( 'NONE',  ( 0.000000000000000000, 0.000000000000000000, -1.000000000000000000 ) ) ;
#56724 = VECTOR ( 'NONE', #50874, 1000.000000000000000 ) ;
#56725 = EDGE_CURVE ( 'NONE', #62320, #63218, #69143, .T. ) ;
#56726 = ORIENTED_EDGE ( 'NONE', *, *, #65277, .F. ) ;
#56727 = CARTESIAN_POINT ( 'NONE',  ( -157.2549999999999955, -4.716976649647092401, 6.492361379858946790 ) ) ;
#56728 = COLOUR_RGB ( '', 0.72549020, 0.75294118, 0.79215686) ;
#56729 = VERTEX_POINT ( 'NONE', #339 ) ;
#56730 = SURFACE_STYLE_FILL_AREA ( #35269 ) ;
#56731 = ORIENTED_EDGE ( 'NONE', *, *, #28963, .T. ) ;
#56732 =( GEOMETRIC_REPRESENTATION_CONTEXT ( 3 ) GLOBAL_UNCERTAINTY_ASSIGNED_CONTEXT ( ( #34112 ) ) GLOBAL_UNIT_ASSIGNED_CONTEXT ( ( #56750, #35289, #40940 ) ) REPRESENTATION_CONTEXT ( 'NONE', 'WORKASPACE' ) );
#56733 = ADVANCED_FACE ( 'NONE', ( #43705 ), #26086, .T. ) ;
#56734 = FILL_AREA_STYLE_COLOUR ( '', #1161 ) ;
#56735 = DIRECTION ( 'NONE',  ( 0.3361263392814427542, -0.000000000000000000, 0.9418169057949938860 ) ) ;
#56736 = CARTESIAN_POINT ( 'NONE',  ( -9.058813317711337021, 116.0449999999999875, -2.943386871421374895 ) ) ;
#56737 =( GEOMETRIC_REPRESENTATION_CONTEXT ( 3 ) GLOBAL_UNCERTAINTY_ASSIGNED_CONTEXT ( ( #38409 ) ) GLOBAL_UNIT_ASSIGNED_CONTEXT ( ( #13108, #6788, #44144 ) ) REPRESENTATION_CONTEXT ( 'NONE', 'WORKASPACE' ) );
#56738 = ORIENTED_EDGE ( 'NONE', *, *, #63776, .T. ) ;
#56739 = DIRECTION ( 'NONE',  ( 1.000000000000000000, 0.000000000000000000, 0.000000000000000000 ) ) ;
#56740 = CARTESIAN_POINT ( 'NONE',  ( -10.01517768586949408, 111.3049999999999784, -6.132527647946036459E-16 ) ) ;
#56741 = CARTESIAN_POINT ( 'NONE',  ( -76.10499999999997556, -6.826472737025113702, 4.959722759717902107 ) ) ;
#56742 = CIRCLE ( 'NONE', #17450, 1.000000000000000000 ) ;
#56743 = ADVANCED_FACE ( 'NONE', ( #6024, #27462 ), #48987, .T. ) ;
#56744 = CARTESIAN_POINT ( 'NONE',  ( -80.00707362346618368, -8.102448949553174629, -5.886773742842741797 ) ) ;
#56745 = ORIENTED_EDGE ( 'NONE', *, *, #34309, .F. ) ;
#56746 = CARTESIAN_POINT ( 'NONE',  ( -5.598654528085806881, 137.8549999999999898, -7.705886871421374629 ) ) ;
#56747 = UNCERTAINTY_MEASURE_WITH_UNIT (LENGTH_MEASURE( 1.000000000000000082E-05 ), #30334, 'distance_accuracy_value', 'NONE');
#56748 = SURFACE_SIDE_STYLE ('',( #57430 ) ) ;
#56749 = DIRECTION ( 'NONE',  ( 1.000000000000000000, 0.000000000000000000, 0.000000000000000000 ) ) ;
#56750 =( LENGTH_UNIT ( ) NAMED_UNIT ( * ) SI_UNIT ( .MILLI., .METRE. ) );
#56751 = ORIENTED_EDGE ( 'NONE', *, *, #667, .T. ) ;
#56752 =( LENGTH_UNIT ( ) NAMED_UNIT ( * ) SI_UNIT ( .MILLI., .METRE. ) );
#56753 = FACE_OUTER_BOUND ( 'NONE', #19244, .T. ) ;
#56754 = CARTESIAN_POINT ( 'NONE',  ( -48.44499999999998607, 0.000000000000000000, 8.024999999999991473 ) ) ;
#56755 = ORIENTED_EDGE ( 'NONE', *, *, #14311, .T. ) ;
#56756 = DIRECTION ( 'NONE',  ( 0.000000000000000000, 1.000000000000000000, 0.000000000000000000 ) ) ;
#56757 = AXIS2_PLACEMENT_3D ( 'NONE', #207, #47850, #32618 ) ;
#56758 = CIRCLE ( 'NONE', #490, 1.000000000000000888 ) ;
#56759 = DIRECTION ( 'NONE',  ( 0.000000000000000000, 1.000000000000000000, 0.000000000000000000 ) ) ;
#56760 = DIRECTION ( 'NONE',  ( 1.000000000000000000, 0.000000000000000000, 0.000000000000000000 ) ) ;
#56761 = EDGE_LOOP ( 'NONE', ( #28712, #43413, #16372 ) ) ;
#56762 = CARTESIAN_POINT ( 'NONE',  ( -57.29499999999998039, -2.607480562269069768, 8.024999999999991473 ) ) ;
#56763 = VERTEX_POINT ( 'NONE', #20835 ) ;
#56764 = TOROIDAL_SURFACE ( 'NONE', #6232, 22.50000000000000000, 0.5000000000000000000 ) ;
#56765 = CARTESIAN_POINT ( 'NONE',  ( -101.0049999999999812, 6.826472737025116366, 4.959722759717898555 ) ) ;
#56766 = ORIENTED_EDGE ( 'NONE', *, *, #28165, .T. ) ;
#56767 = CARTESIAN_POINT ( 'NONE',  ( 28.00000000000002842, 37.76051491742381216, 89.34202014332566932 ) ) ;
#56768 = AXIS2_PLACEMENT_3D ( 'NONE', #37658, #36622, #58040 ) ;
#56769 = CARTESIAN_POINT ( 'NONE',  ( -136.2570736234661695, 5.598654528085800663, -7.705886871421367523 ) ) ;
#56770 = STYLED_ITEM ( 'NONE', ( #15775 ), #5150 ) ;
#56771 = DIRECTION ( 'NONE',  ( 0.000000000000000000, 0.000000000000000000, 1.000000000000000000 ) ) ;
#56772 = CARTESIAN_POINT ( 'NONE',  ( -5.598654528085806881, 142.7449999999999761, -7.705886871421374629 ) ) ;
#56773 = CARTESIAN_POINT ( 'NONE',  ( -78.95707362346617231, 9.058813317711329915, -2.943386871421373119 ) ) ;
#56774 = DIRECTION ( 'NONE',  ( 1.000000000000000000, 0.000000000000000000, 0.000000000000000000 ) ) ;
#56775 = CARTESIAN_POINT ( 'NONE',  ( -18.75822517221693175, -11.53590615615684634, 3.313539367360412324 ) ) ;
#56777 = SPHERICAL_SURFACE ( 'NONE', #50476, 1.000000000000000000 ) ;
#56776 = DIRECTION ( 'NONE',  ( -1.000000000000000000, 0.000000000000000000, 0.000000000000000000 ) ) ;
#56778 = AXIS2_PLACEMENT_3D ( 'NONE', #3189, #34913, #2856 ) ;
#56779 = CARTESIAN_POINT ( 'NONE',  ( -117.6550000000000011, -7.632228543268600340, -2.479861379858950166 ) ) ;
#56780 = CARTESIAN_POINT ( 'NONE',  ( 8.250000000000001776, 30.74999999999998579, -4.000000000000000000 ) ) ;
#56781 = CARTESIAN_POINT ( 'NONE',  ( -1.166476076187854022E-15, 110.9449999999999932, 9.525000000000000355 ) ) ;
#56782 = CARTESIAN_POINT ( 'NONE',  ( -134.9950000000000045, -6.826472737025115478, 4.959722759717900331 ) ) ;
#56783 = CIRCLE ( 'NONE', #60139, 0.2500000000000002220 ) ;
#56784 = CARTESIAN_POINT ( 'NONE',  ( -120.5949999999999704, 2.607480562269072433, 8.024999999999991473 ) ) ;
#56785 = FILL_AREA_STYLE_COLOUR ( '', #3241 ) ;
#56786 = VERTEX_POINT ( 'NONE', #42337 ) ;
#56787 = COLOUR_RGB ( '', 0.09019608, 0.27058824, 0.51372549) ;
#56788 = LINE ( 'NONE', #24075, #39284 ) ;
#56789 =( NAMED_UNIT ( * ) SI_UNIT ( $, .STERADIAN. ) SOLID_ANGLE_UNIT ( ) );
#56790 = EDGE_CURVE ( 'NONE', #35826, #22128, #63723, .T. ) ;
#56791 = CARTESIAN_POINT ( 'NONE',  ( -121.4929263765337879, -8.102448949553174629, 5.886773742842742685 ) ) ;
#56792 = CARTESIAN_POINT ( 'NONE',  ( -176.2429263765338021, 5.598654528085804216, 7.705886871421366635 ) ) ;
#56793 = CARTESIAN_POINT ( 'NONE',  ( -50.69499999999998607, -8.437984349512085203, 5.166775262442717831E-16 ) ) ;
#56794 = ADVANCED_FACE ( 'NONE', ( #39459 ), #7748, .F. ) ;
#56795 = EDGE_CURVE ( 'NONE', #1034, #10730, #54510, .T. ) ;
#56796 = CARTESIAN_POINT ( 'NONE',  ( -44.99154893936433552, 9.591540374752316467, -3.000000000000000444 ) ) ;
#56797 = CARTESIAN_POINT ( 'NONE',  ( -15.98999599679679839, 118.4999999999999716, -7.000000000000000000 ) ) ;
#56798 = CARTESIAN_POINT ( 'NONE',  ( 9.250000000000003553, 27.99999999999998934, -3.750000000000000000 ) ) ;
#56799 = ORIENTED_EDGE ( 'NONE', *, *, #24126, .T. ) ;
#56800 = CARTESIAN_POINT ( 'NONE',  ( -83.99292637653380211, 8.102448949553171076, -5.886773742842744461 ) ) ;
#56801 = B_SPLINE_CURVE_WITH_KNOTS ( 'NONE', 3,
 ( #10846, #58017, #48518, #31949, #36599, #32290, #53740, #9827 ),
 .UNSPECIFIED., .F., .F.,
 ( 4, 2, 2, 4 ),
 ( 0.004248627969284164696, 0.005296391997195108725, 0.006344156025106052754, 0.008439684080927939078 ),
 .UNSPECIFIED. ) ;
#56802 = ITEM_DEFINED_TRANSFORMATION ( 'NONE', 'NONE', #42802,  #42840 ) ;
#56803 = LINE ( 'NONE', #38145, #63302 ) ;
#56804 =( NAMED_UNIT ( * ) PLANE_ANGLE_UNIT ( ) SI_UNIT ( $, .RADIAN. ) );
#56805 = COLOUR_RGB ( '', 0.40784314, 0.44705882, 0.49803922) ;
#56806 =( NAMED_UNIT ( * ) SI_UNIT ( $, .STERADIAN. ) SOLID_ANGLE_UNIT ( ) );
#56807 = CARTESIAN_POINT ( 'NONE',  ( -87.50000000000000000, -6.499999999999990230, 21.00000000000000000 ) ) ;
#56808 = CARTESIAN_POINT ( 'NONE',  ( 32.00000000000001421, -60.04052944165106709, -35.50000000000000000 ) ) ;
#56809 = EDGE_CURVE ( 'NONE', #64972, #46307, #20838, .T. ) ;
#56810 = AXIS2_PLACEMENT_3D ( 'NONE', #6299, #7000, #17585 ) ;
#56811 = VERTEX_POINT ( 'NONE', #49643 ) ;
#56812 = DIRECTION ( 'NONE',  ( -1.000000000000000000, 0.000000000000000000, 0.000000000000000000 ) ) ;
#56813 = SURFACE_SIDE_STYLE ('',( #3641 ) ) ;
#56815 = ORIENTED_EDGE ( 'NONE', *, *, #68416, .F. ) ;
#56814 = AXIS2_PLACEMENT_3D ( 'NONE', #24785, #45940, #23404 ) ;
#56816 = FACE_OUTER_BOUND ( 'NONE', #38393, .T. ) ;
#56817 = AXIS2_PLACEMENT_3D ( 'NONE', #67065, #50197, #56138 ) ;
#56818 = CYLINDRICAL_SURFACE ( 'NONE', #39854, 0.5000000000000004441 ) ;
#56819 = CARTESIAN_POINT ( 'NONE',  ( 7.632228543268608334, 129.4570736234661581, -2.479861379858951942 ) ) ;
#56820 = ORIENTED_EDGE ( 'NONE', *, *, #22876, .T. ) ;
#56821 = CARTESIAN_POINT ( 'NONE',  ( 75.00000000000000000, 20.36037961002804053, -6.000000000000000000 ) ) ;
#56822 = CARTESIAN_POINT ( 'NONE',  ( -106.7049999999999983, 2.607480562269072433, 8.024999999999991473 ) ) ;
#56823 = SURFACE_STYLE_USAGE ( .BOTH. , #35369 ) ;
#56824 = DIRECTION ( 'NONE',  ( -1.000000000000000000, 0.000000000000000000, 0.000000000000000000 ) ) ;
#56825 = EDGE_LOOP ( 'NONE', ( #56254, #312, #2819, #9788 ) ) ;
#56826 = TOROIDAL_SURFACE ( 'NONE', #19754, 9.499999999999998224, 0.5000000000000000000 ) ;
#56827 = CARTESIAN_POINT ( 'NONE',  ( -74.75000000000000000, -0.9999999999999995559, 6.000000000000001776 ) ) ;
#56828 =( NAMED_UNIT ( * ) PLANE_ANGLE_UNIT ( ) SI_UNIT ( $, .RADIAN. ) );
#56829 = EDGE_CURVE ( 'NONE', #41309, #57325, #28683, .T. ) ;
#56830 = COLOUR_RGB ( '', 0.40784314, 0.44705882, 0.49803922) ;
#56831 = AXIS2_PLACEMENT_3D ( 'NONE', #1043, #54234, #65489 ) ;
#56832 = DIRECTION ( 'NONE',  ( 1.156482317317873451E-16, 1.000000000000000000, -0.000000000000000000 ) ) ;
#56833 = ADVANCED_FACE ( 'NONE', ( #1742 ), #46737, .T. ) ;
#56834 = CARTESIAN_POINT ( 'NONE',  ( -77.54499999999998749, -7.632228543268600340, -2.479861379858950166 ) ) ;
#56835 = VERTEX_POINT ( 'NONE', #33789 ) ;
#56836 = DIRECTION ( 'NONE',  ( 0.000000000000000000, -0.000000000000000000, 1.000000000000000000 ) ) ;
#56837 = FACE_OUTER_BOUND ( 'NONE', #28431, .T. ) ;
#56838 = VERTEX_POINT ( 'NONE', #66506 ) ;
#56839 = FILL_AREA_STYLE ('',( #66694 ) ) ;
#56840 = FILL_AREA_STYLE_COLOUR ( '', #60606 ) ;
#56841 = ORIENTED_EDGE ( 'NONE', *, *, #8361, .T. ) ;
#56842 =( NAMED_UNIT ( * ) SI_UNIT ( $, .STERADIAN. ) SOLID_ANGLE_UNIT ( ) );
#56843 = ORIENTED_EDGE ( 'NONE', *, *, #54386, .T. ) ;
#56844 = CARTESIAN_POINT ( 'NONE',  ( 18.00000000000000711, 30.99999999999999289, 3.750000000000000000 ) ) ;
#56845 = CARTESIAN_POINT ( 'NONE',  ( -57.11974195712093660, -7.499999999999993783, 0.06931351858119048914 ) ) ;
#56846 = PRESENTATION_STYLE_ASSIGNMENT (( #51222 ) ) ;
#56847 = CARTESIAN_POINT ( 'NONE',  ( -173.0070736234661979, -8.102448949553172852, -5.886773742842741797 ) ) ;
#56848 = DIRECTION ( 'NONE',  ( 0.07854820085872894764, 0.9914125719358882760, -0.1045528208578022367 ) ) ;
#56849 = CARTESIAN_POINT ( 'NONE',  ( -3.094860106618434248, 116.7949999999999733, 9.525000000000000355 ) ) ;
#56850 = CARTESIAN_POINT ( 'NONE',  ( -105.3570736234661780, 5.598654528085804216, 7.705886871421366635 ) ) ;
#56851 = CARTESIAN_POINT ( 'NONE',  ( -82.94292637653380496, 0.000000000000000000, 9.524999999999991473 ) ) ;
#56852 =( LENGTH_UNIT ( ) NAMED_UNIT ( * ) SI_UNIT ( .MILLI., .METRE. ) );
#56853 = EDGE_LOOP ( 'NONE', ( #12419, #41558, #68622, #53191 ) ) ;
#56854 = DIRECTION ( 'NONE',  ( -0.000000000000000000, -1.000000000000000000, -0.000000000000000000 ) ) ;
#56855 = DIRECTION ( 'NONE',  ( 1.000000000000000000, 0.000000000000000000, 0.000000000000000000 ) ) ;
#56857 = DIRECTION ( 'NONE',  ( 0.000000000000000000, 0.000000000000000000, 1.000000000000000000 ) ) ;
#56856 = DIRECTION ( 'NONE',  ( 1.000000000000000000, -0.000000000000000000, 0.000000000000000000 ) ) ;
#56858 = FACE_OUTER_BOUND ( 'NONE', #19023, .T. ) ;
#56859 = CARTESIAN_POINT ( 'NONE',  ( -153.8049999999999784, -8.437984349512085203, 5.166775262442717831E-16 ) ) ;
#56860 = CARTESIAN_POINT ( 'NONE',  ( -148.1929263765338192, -10.01517768586948698, 6.132527647946031529E-16 ) ) ;
#56861 = EDGE_CURVE ( 'NONE', #13067, #36987, #12676, .T. ) ;
#56862 = CARTESIAN_POINT ( 'NONE',  ( -163.1949999999999648, 8.437984349512085203, -1.550032578732815448E-15 ) ) ;
#56863 = AXIS2_PLACEMENT_3D ( 'NONE', #54807, #6617, #60777 ) ;
#56864 = CARTESIAN_POINT ( 'NONE',  ( -146.6949999999999932, -8.437984349512086979, 5.166775262442717831E-16 ) ) ;
#56865 = ORIENTED_EDGE ( 'NONE', *, *, #66785, .T. ) ;
#56866 = CARTESIAN_POINT ( 'NONE',  ( -8.701243704650558186, 2.929003814506410119, 0.1702817813269568992 ) ) ;
#56867 = CYLINDRICAL_SURFACE ( 'NONE', #54753, 9.524999999999991473 ) ;
#56868 = ADVANCED_FACE ( 'NONE', ( #18327 ), #33185, .F. ) ;
#56869 = CARTESIAN_POINT ( 'NONE',  ( -62.00499999999999545, 6.826472737025116366, 4.959722759717898555 ) ) ;
#56870 = DIRECTION ( 'NONE',  ( -0.000000000000000000, -0.000000000000000000, -1.000000000000000000 ) ) ;
#56871 = CYLINDRICAL_SURFACE ( 'NONE', #17940, 2.499999999999998668 ) ;
#56872 = CIRCLE ( 'NONE', #68131, 6.999999999999997335 ) ;
#56873 = EDGE_CURVE ( 'NONE', #64020, #55574, #6365, .T. ) ;
#56874 = CARTESIAN_POINT ( 'NONE',  ( -58.64499999999998892, 4.716976649647091513, -6.492361379858946790 ) ) ;
#56875 = CARTESIAN_POINT ( 'NONE',  ( 9.058813317711338797, 157.9549999999999841, -2.943386871421372675 ) ) ;
#56876 = CARTESIAN_POINT ( 'NONE',  ( 3.999798566743339556, 49.09558629977726696, 2.000000000000000000 ) ) ;
#56877 = CIRCLE ( 'NONE', #33275, 1.000000000000000888 ) ;
#56878 = B_SPLINE_CURVE_WITH_KNOTS ( 'NONE', 3,
 ( #30045, #8952, #13877, #45232, #25124, #66659 ),
 .UNSPECIFIED., .F., .F.,
 ( 4, 2, 4 ),
 ( 0.004189585287972442777, 0.006269578072783818512, 0.008349570857595195114 ),
 .UNSPECIFIED. ) ;
#56879 = DIRECTION ( 'NONE',  ( -0.000000000000000000, -0.000000000000000000, -1.000000000000000000 ) ) ;
#56880 = PLANE ( 'NONE',  #43873 ) ;
#56881 = CARTESIAN_POINT ( 'NONE',  ( 40.99999999999998579, 108.0000000000000000, 3.000000000000000000 ) ) ;
#56882 = EDGE_CURVE ( 'NONE', #21141, #38604, #25319, .T. ) ;
#56883 = FILL_AREA_STYLE_COLOUR ( '', #1229 ) ;
#56884 =( NAMED_UNIT ( * ) PLANE_ANGLE_UNIT ( ) SI_UNIT ( $, .RADIAN. ) );
#56885 = PRESENTATION_STYLE_ASSIGNMENT (( #14674 ) ) ;
#56886 = ORIENTED_EDGE ( 'NONE', *, *, #35192, .T. ) ;
#56887 = VERTEX_POINT ( 'NONE', #19340 ) ;
#56888 = SURFACE_STYLE_FILL_AREA ( #61784 ) ;
#56889 = FACE_OUTER_BOUND ( 'NONE', #52031, .T. ) ;
#56890 = SURFACE_SIDE_STYLE ('',( #13264 ) ) ;
#56891 = PLANE ( 'NONE',  #61114 ) ;
#56892 = ORIENTED_EDGE ( 'NONE', *, *, #28016, .F. ) ;
#56893 = ORIENTED_EDGE ( 'NONE', *, *, #63526, .T. ) ;
#56894 = VECTOR ( 'NONE', #37161, 1000.000000000000000 ) ;
#56895 = SURFACE_STYLE_FILL_AREA ( #61792 ) ;
#56896 = DIRECTION ( 'NONE',  ( 0.000000000000000000, 0.000000000000000000, 1.000000000000000000 ) ) ;
#56897 = ORIENTED_EDGE ( 'NONE', *, *, #67686, .F. ) ;
#56898 = CARTESIAN_POINT ( 'NONE',  ( -60.00000000000000000, -2.024042244987997205E-14, 9.500000000000000000 ) ) ;
#56899 = CARTESIAN_POINT ( 'NONE',  ( -0.7098155475105580869, 7.000000000000003553, 0.02753250691854559548 ) ) ;
#56900 =( GEOMETRIC_REPRESENTATION_CONTEXT ( 3 ) GLOBAL_UNCERTAINTY_ASSIGNED_CONTEXT ( ( #59500 ) ) GLOBAL_UNIT_ASSIGNED_CONTEXT ( ( #18231, #60431, #18897 ) ) REPRESENTATION_CONTEXT ( 'NONE', 'WORKASPACE' ) );
#56901 = VERTEX_POINT ( 'NONE', #41527 ) ;
#56902 = STYLED_ITEM ( 'NONE', ( #2797 ), #50161 ) ;
#56903 = PRESENTATION_STYLE_ASSIGNMENT (( #66766 ) ) ;
#56904 = DIRECTION ( 'NONE',  ( 0.000000000000000000, 0.000000000000000000, 1.000000000000000000 ) ) ;
#56905 = CARTESIAN_POINT ( 'NONE',  ( -108.4449999999999790, 0.000000000000000000, 8.024999999999991473 ) ) ;
#56906 = VERTEX_POINT ( 'NONE', #3469 ) ;
#56907 = EDGE_LOOP ( 'NONE', ( #36951, #8989, #43997 ) ) ;
#56908 = CARTESIAN_POINT ( 'NONE',  ( 6.826472737025121695, 143.4929263765338305, -4.959722759717905660 ) ) ;
#56909 = DIRECTION ( 'NONE',  ( 1.000000000000000000, -1.734723475976812222E-15, -1.926605602187847311E-15 ) ) ;
#56910 = DIRECTION ( 'NONE',  ( -1.000000000000000000, 0.000000000000000000, 0.000000000000000000 ) ) ;
#56911 = CIRCLE ( 'NONE', #36736, 16.00000000000000000 ) ;
#56912 = CARTESIAN_POINT ( 'NONE',  ( 1.000000000000000000, -60.04052944165106709, -35.50000000000000000 ) ) ;
#56913 = ORIENTED_EDGE ( 'NONE', *, *, #36089, .F. ) ;
#56914 = CARTESIAN_POINT ( 'NONE',  ( -126.0570736234661808, 0.000000000000000000, 9.524999999999991473 ) ) ;
#56915 = VERTEX_POINT ( 'NONE', #35882 ) ;
#56916 = CARTESIAN_POINT ( 'NONE',  ( 2.607480562269075985, 128.7929263765338135, -8.025000000000000355 ) ) ;
#56917 = CYLINDRICAL_SURFACE ( 'NONE', #58246, 9.524999999999991473 ) ;
#56918 =( NAMED_UNIT ( * ) PLANE_ANGLE_UNIT ( ) SI_UNIT ( $, .RADIAN. ) );
#56919 = CARTESIAN_POINT ( 'NONE',  ( -158.6070736234661922, -8.102448949553174629, 5.886773742842742685 ) ) ;
#56920 = CARTESIAN_POINT ( 'NONE',  ( -124.2549999999999955, -4.716976649647092401, 6.492361379858946790 ) ) ;
#56921 = CARTESIAN_POINT ( 'NONE',  ( -183.9999999999998863, -2.671725603995652953, 7.577260112568927397 ) ) ;
#56922 = DIRECTION ( 'NONE',  ( 1.000000000000000000, 0.000000000000000000, 0.000000000000000000 ) ) ;
#56923 = PRESENTATION_STYLE_ASSIGNMENT (( #2348 ) ) ;
#56924 = MECHANICAL_DESIGN_GEOMETRIC_PRESENTATION_REPRESENTATION (  '', ( #61419 ), #64810 ) ;
#56925 = DIRECTION ( 'NONE',  ( -1.000000000000000000, -1.224646799147353454E-16, 0.000000000000000000 ) ) ;
#56926 = PRESENTATION_STYLE_ASSIGNMENT (( #8406 ) ) ;
#56927 = CARTESIAN_POINT ( 'NONE',  ( -6.826472737025120807, 120.9929263765338021, 4.959722759717906548 ) ) ;
#56928 = ORIENTED_EDGE ( 'NONE', *, *, #5331, .F. ) ;
#56929 = ORIENTED_EDGE ( 'NONE', *, *, #9081, .F. ) ;
#56930 = CARTESIAN_POINT ( 'NONE',  ( -41.49999999999998579, 108.0000000000000000, -3.000000000000000444 ) ) ;
#56931 = DIRECTION ( 'NONE',  ( 1.000000000000000000, 0.000000000000000000, 0.000000000000000000 ) ) ;
#56932 = CARTESIAN_POINT ( 'NONE',  ( 9.250000000000003553, 27.74999999999998934, 4.000000000000000000 ) ) ;
#56933 = CARTESIAN_POINT ( 'NONE',  ( 74.65811388300841145, 19.88603796100278487, 6.000000000000000888 ) ) ;
#56934 = ORIENTED_EDGE ( 'NONE', *, *, #38171, .F. ) ;
#56935 = DIRECTION ( 'NONE',  ( -0.000000000000000000, -0.000000000000000000, -1.000000000000000000 ) ) ;
#56936 = CARTESIAN_POINT ( 'NONE',  ( -176.6049999999999898, 6.826472737025113702, -4.959722759717902107 ) ) ;
#56937 = DIRECTION ( 'NONE',  ( 0.000000000000000000, 1.000000000000000000, 0.000000000000000000 ) ) ;
#56938 = EDGE_CURVE ( 'NONE', #835, #28382, #67192, .T. ) ;
#56939 = CARTESIAN_POINT ( 'NONE',  ( -55.25707362346615525, 5.598654528085800663, -7.705886871421367523 ) ) ;
#56940 = CARTESIAN_POINT ( 'NONE',  ( -172.7950000000000159, 2.607480562269069324, -8.024999999999993250 ) ) ;
#56941 = CARTESIAN_POINT ( 'NONE',  ( 40.78947368421051323, 108.1536491499103505, 3.157942443983134506 ) ) ;
#56942 = ORIENTED_EDGE ( 'NONE', *, *, #886, .F. ) ;
#56943 = CARTESIAN_POINT ( 'NONE',  ( 2.999999999999994671, 5.000000000000000000, -24.00402776293822527 ) ) ;
#56944 = SURFACE_STYLE_FILL_AREA ( #35501 ) ;
#56945 = CARTESIAN_POINT ( 'NONE',  ( -92.15499999999998693, 7.632228543268600340, 2.479861379858949277 ) ) ;
#56946 = SURFACE_STYLE_USAGE ( .BOTH. , #52395 ) ;
#56947 = VECTOR ( 'NONE', #24638, 1000.000000000000000 ) ;
#56948 = EDGE_CURVE ( 'NONE', #33026, #46607, #25345, .T. ) ;
#56949 = CARTESIAN_POINT ( 'NONE',  ( -89.54499999999998749, -7.632228543268600340, -2.479861379858950166 ) ) ;
#56950 = CARTESIAN_POINT ( 'NONE',  ( -9.058813317711337021, 126.1549999999999869, -2.943386871421374895 ) ) ;
#56951 = B_SPLINE_CURVE_WITH_KNOTS ( 'NONE', 3,
 ( #39717, #40075, #61463, #8386, #23494, #66416, #18233, #17565, #43476, #48383, #52348, #26845 ),
 .UNSPECIFIED., .F., .F.,
 ( 4, 2, 2, 2, 2, 4 ),
 ( 0.004228563614865340353, 0.004757664776855344800, 0.005286765938845350114, 0.005551316519840357976, 0.005815867100835366704, 0.006344968262825391968 ),
 .UNSPECIFIED. ) ;
#56952 = PRESENTATION_LAYER_ASSIGNMENT (  '', '', ( #32242 ) ) ;
#56953 = CARTESIAN_POINT ( 'NONE',  ( -66.29500000000000171, -2.607480562269069768, 8.024999999999991473 ) ) ;
#56954 = EDGE_CURVE ( 'NONE', #57180, #27282, #68591, .T. ) ;
#56955 = CARTESIAN_POINT ( 'NONE',  ( -75.48275862068965125, 63.99167409976910648, 9.500000000000001776 ) ) ;
#56956 = STYLED_ITEM ( 'NONE', ( #65985 ), #50394 ) ;
#56957 = CARTESIAN_POINT ( 'NONE',  ( 16.00000000000001776, 42.00000000000000000, 34.68999999999999062 ) ) ;
#56958 = ADVANCED_FACE ( 'NONE', ( #29557 ), #67904, .F. ) ;
#56959 = DIRECTION ( 'NONE',  ( 1.000000000000000000, 0.000000000000000000, 0.000000000000000000 ) ) ;
#56960 = DIRECTION ( 'NONE',  ( 0.000000000000000000, 0.3420201433256693790, -0.9396926207859082059 ) ) ;
#56961 = ORIENTED_EDGE ( 'NONE', *, *, #65044, .T. ) ;
#56962 = EDGE_CURVE ( 'NONE', #19166, #14403, #13726, .T. ) ;
#56963 = CARTESIAN_POINT ( 'NONE',  ( -110.5429263765337993, 9.058813317711329915, 2.943386871421369566 ) ) ;
#56964 =( BOUNDED_CURVE ( )  B_SPLINE_CURVE ( 2, ( #17464, #64221, #1180, #27611, #5455, #21663, #26906, #16763, #22714, #6179, #49129 ),
 .UNSPECIFIED., .F., .F. ) 
 B_SPLINE_CURVE_WITH_KNOTS ( ( 3, 2, 2, 2, 2, 3 ),
 ( 0.5978260869565077407, 0.5999999999999858780, 0.6021739130434641263, 0.6043478260869422636, 0.6065217391304206229, 0.6086956521738987602 ),
 .UNSPECIFIED. ) 
 CURVE ( )  GEOMETRIC_REPRESENTATION_ITEM ( )  RATIONAL_B_SPLINE_CURVE ( ( 1.000000000000314859, 0.9510565162948385609, 1.000000000000000000, 0.9510565162951535312, 1.000000000000000000, 0.9510565162951535312, 1.000000000000000000, 0.9510565162951535312, 1.000000000000000000, 0.9510565162954759399, 0.9999999999996775912 ) ) 
 REPRESENTATION_ITEM ( '' )  );
#56965 = CARTESIAN_POINT ( 'NONE',  ( -125.9949999999999903, -6.826472737025115478, 4.959722759717900331 ) ) ;
#56966 = CARTESIAN_POINT ( 'NONE',  ( -4.041451884327381450, 7.000000000000006217, 1.082903768654761345 ) ) ;
#56967 = CARTESIAN_POINT ( 'NONE',  ( -15.98999599679679839, 147.4999999999999716, 9.500000000000000000 ) ) ;
#56968 = DIRECTION ( 'NONE',  ( 0.000000000000000000, 0.000000000000000000, 1.000000000000000000 ) ) ;
#56969 = ORIENTED_EDGE ( 'NONE', *, *, #39727, .F. ) ;
#56970 = ORIENTED_EDGE ( 'NONE', *, *, #49349, .F. ) ;
#56971 = CARTESIAN_POINT ( 'NONE',  ( -62.54292637653379927, 9.058813317711329915, 2.943386871421369566 ) ) ;
#56972 = CARTESIAN_POINT ( 'NONE',  ( 0.000000000000000000, 146.9429263765338192, -8.025000000000000355 ) ) ;
#56973 = CARTESIAN_POINT ( 'NONE',  ( 0.7093150608870635310, 2.499999999999996447, 7.000000000000000000 ) ) ;
#56974 = FILL_AREA_STYLE ('',( #47160 ) ) ;
#56975 = CARTESIAN_POINT ( 'NONE',  ( -7.794228634059948035, -2.500000000000000000, 4.499999999999999112 ) ) ;
#56976 = EDGE_LOOP ( 'NONE', ( #10441, #14142, #39616, #4152, #65635, #16775 ) ) ;
#56977 = CARTESIAN_POINT ( 'NONE',  ( -128.4549999999999841, 7.632228543268599452, -2.479861379858951942 ) ) ;
#56978 = ORIENTED_EDGE ( 'NONE', *, *, #29866, .T. ) ;
#56979 = CARTESIAN_POINT ( 'NONE',  ( 17.25000000000000711, 25.24999999999998224, -3.750000000000000000 ) ) ;
#56980 = CARTESIAN_POINT ( 'NONE',  ( -127.2570736234661695, 5.598654528085800663, -7.705886871421367523 ) ) ;
#56981 = ORIENTED_EDGE ( 'NONE', *, *, #53319, .T. ) ;
#56982 = FACE_OUTER_BOUND ( 'NONE', #16190, .T. ) ;
#56983 = LINE ( 'NONE', #51363, #14146 ) ;
#56984 = ORIENTED_EDGE ( 'NONE', *, *, #35447, .F. ) ;
#56985 = DIRECTION ( 'NONE',  ( -0.000000000000000000, -0.000000000000000000, 1.000000000000000000 ) ) ;
#56986 =( BOUNDED_CURVE ( )  B_SPLINE_CURVE ( 3, ( #69454, #31806, #26180, #21241 ),
 .UNSPECIFIED., .F., .F. ) 
 B_SPLINE_CURVE_WITH_KNOTS ( ( 4, 4 ),
 ( 4.712388980384689674, 6.283185307179586232 ),
 .UNSPECIFIED. ) 
 CURVE ( )  GEOMETRIC_REPRESENTATION_ITEM ( )  RATIONAL_B_SPLINE_CURVE ( ( 1.000000000000000000, 0.8047378541243649375, 0.8047378541243649375, 1.000000000000000000 ) ) 
 REPRESENTATION_ITEM ( '' )  );
#56987 = CARTESIAN_POINT ( 'NONE',  ( -5.598654528085808657, 140.6449999999999818, 7.705886871421373741 ) ) ;
#56988 = SURFACE_SIDE_STYLE ('',( #19700 ) ) ;
#56989 = ORIENTED_EDGE ( 'NONE', *, *, #30460, .T. ) ;
#56990 = DIRECTION ( 'NONE',  ( 1.000000000000000000, 0.000000000000000000, 0.000000000000000000 ) ) ;
#56991 = CARTESIAN_POINT ( 'NONE',  ( -8.102448949553179958, 135.6049999999999613, 5.886773742842747126 ) ) ;
#56992 = CARTESIAN_POINT ( 'NONE',  ( -48.35499999999998266, -4.716976649647093289, -6.492361379858945902 ) ) ;
#56993 = VERTEX_POINT ( 'NONE', #62259 ) ;
#56994 = CARTESIAN_POINT ( 'NONE',  ( 7.632228543268607446, 119.0429263765338135, 2.479861379858954606 ) ) ;
#56995 = CARTESIAN_POINT ( 'NONE',  ( 0.000000000000000000, 0.000000000000000000, 1.000000000000000000 ) ) ;
#56996 = DIRECTION ( 'NONE',  ( 1.000000000000000000, 0.000000000000000000, 0.000000000000000000 ) ) ;
#56997 = AXIS2_PLACEMENT_3D ( 'NONE', #14707, #35107, #35806 ) ;
#56998 = PRESENTATION_LAYER_ASSIGNMENT (  '', '', ( #10945 ) ) ;
#56999 = PLANE ( 'NONE',  #35121 ) ;
#57000 = AXIS2_PLACEMENT_3D ( 'NONE', #32681, #5252, #26698 ) ;
#57001 = VERTEX_POINT ( 'NONE', #46841 ) ;
#57002 = CARTESIAN_POINT ( 'NONE',  ( 53.24999999999999289, 27.74999999999998579, 4.000000000000000000 ) ) ;
#57003 = ORIENTED_EDGE ( 'NONE', *, *, #42088, .F. ) ;
#57004 = CARTESIAN_POINT ( 'NONE',  ( -12.72792206135785698, 115.4999999999999574, 10.50000000000000000 ) ) ;
#57005 = FILL_AREA_STYLE ('',( #4199 ) ) ;
#57006 = DIRECTION ( 'NONE',  ( 0.000000000000000000, -1.000000000000000000, 0.000000000000000000 ) ) ;
#57007 = CARTESIAN_POINT ( 'NONE',  ( -156.0550000000000068, -9.827790563157499189E-16, -8.024999999999991473 ) ) ;
#57008 = VERTEX_POINT ( 'NONE', #68247 ) ;
#57009 = DIRECTION ( 'NONE',  ( 0.7833176619561811327, 0.6216216216216278179, 4.313366480807235014E-15 ) ) ;
#57010 = SURFACE_STYLE_FILL_AREA ( #56308 ) ;
#57011 = CARTESIAN_POINT ( 'NONE',  ( -4.716976649647098618, 152.2570736234661695, 6.492361379858953008 ) ) ;
#57012 = CARTESIAN_POINT ( 'NONE',  ( 75.00000000000000000, 19.83714805418752292, 6.873786395979866626 ) ) ;
#57013 = CARTESIAN_POINT ( 'NONE',  ( 39.74999999999999289, 18.74999999999997868, -3.750000000000000000 ) ) ;
#57014 = VERTEX_POINT ( 'NONE', #14087 ) ;
#57015 = AXIS2_PLACEMENT_3D ( 'NONE', #15379, #47393, #11083 ) ;
#57016 = CARTESIAN_POINT ( 'NONE',  ( -130.5570736234661808, -1.166476076187852838E-15, -9.524999999999991473 ) ) ;
#57017 = ORIENTED_EDGE ( 'NONE', *, *, #33077, .F. ) ;
#57018 = CARTESIAN_POINT ( 'NONE',  ( -46.64499999999998892, 4.716976649647091513, -6.492361379858946790 ) ) ;
#57019 = AXIS2_PLACEMENT_3D ( 'NONE', #26010, #59069, #43307 ) ;
#57020 = CARTESIAN_POINT ( 'NONE',  ( -79.10499999999998977, -6.826472737025115478, 4.959722759717900331 ) ) ;
#57021 = ORIENTED_EDGE ( 'NONE', *, *, #1698, .F. ) ;
#57022 = SURFACE_STYLE_FILL_AREA ( #68281 ) ;
#57023 = EDGE_CURVE ( 'NONE', #6192, #59896, #20028, .T. ) ;
#57024 = CARTESIAN_POINT ( 'NONE',  ( -124.0429263765337993, -9.058813317711329915, -2.943386871421370898 ) ) ;
#57025 = FACE_OUTER_BOUND ( 'NONE', #18735, .T. ) ;
#57027 = EDGE_CURVE ( 'NONE', #16746, #50108, #30961, .T. ) ;
#57026 = ORIENTED_EDGE ( 'NONE', *, *, #30962, .T. ) ;
#57028 = CARTESIAN_POINT ( 'NONE',  ( -75.00000000000000000, 9.657020704707399261, -6.241538579429665390 ) ) ;
#57029 = CARTESIAN_POINT ( 'NONE',  ( -4.041451884327381450, 7.000000000000006217, 1.082903768654761345 ) ) ;
#57030 = SURFACE_STYLE_USAGE ( .BOTH. , #45491 ) ;
#57032 = LINE ( 'NONE', #18711, #4442 ) ;
#57031 = CARTESIAN_POINT ( 'NONE',  ( 7.500000000000000000, 9.184850993605147944E-16, 0.2499999999999924227 ) ) ;
#57033 = CARTESIAN_POINT ( 'NONE',  ( 9.058813317711338797, 138.8449999999999989, -2.943386871421372675 ) ) ;
#57034 = CARTESIAN_POINT ( 'NONE',  ( -100.0450000000000017, 7.632228543268600340, 2.479861379858949277 ) ) ;
#57035 = ADVANCED_FACE ( 'NONE', ( #9518 ), #56646, .T. ) ;
#57036 = FILL_AREA_STYLE_COLOUR ( '', #18429 ) ;
#57037 = DIRECTION ( 'NONE',  ( 1.156482317317866302E-16, -1.000000000000000000, 1.712231188808094873E-15 ) ) ;
#57038 = CARTESIAN_POINT ( 'NONE',  ( -2.607480562268991608, 145.2929263765338419, 8.025000000000060751 ) ) ;
#57039 = ORIENTED_EDGE ( 'NONE', *, *, #66005, .F. ) ;
#57040 = AXIS2_PLACEMENT_3D ( 'NONE', #27327, #40889, #52483 ) ;
#57041 = EDGE_CURVE ( 'NONE', #35366, #31048, #32318, .T. ) ;
#57042 = CARTESIAN_POINT ( 'NONE',  ( -142.6429263765338078, -5.598654528085801552, 7.705886871421367523 ) ) ;
#57043 = DIRECTION ( 'NONE',  ( -0.000000000000000000, 1.000000000000000000, -0.000000000000000000 ) ) ;
#57044 = CARTESIAN_POINT ( 'NONE',  ( -152.6949999999999932, -8.437984349512085203, 5.166775262442717831E-16 ) ) ;
#57045 = CIRCLE ( 'NONE', #32330, 13.99999999999999822 ) ;
#57046 = DIRECTION ( 'NONE',  ( 0.000000000000000000, 0.000000000000000000, -1.000000000000000000 ) ) ;
#57047 = EDGE_LOOP ( 'NONE', ( #32076, #55349, #66749 ) ) ;
#57048 = VECTOR ( 'NONE', #7987, 1000.000000000000000 ) ;
#57049 = FACE_OUTER_BOUND ( 'NONE', #65712, .T. ) ;
#57050 = ORIENTED_EDGE ( 'NONE', *, *, #42798, .F. ) ;
#57051 = SURFACE_SIDE_STYLE ('',( #35613 ) ) ;
#57052 = CARTESIAN_POINT ( 'NONE',  ( -44.99999999999999289, 8.411230060885010573, 6.233452521073827413 ) ) ;
#57053 = CARTESIAN_POINT ( 'NONE',  ( 1.000000000000000000, 1.000000000000000222, 3.000000000000000000 ) ) ;
#57054 = VECTOR ( 'NONE', #22610, 1000.000000000000000 ) ;
#57055 =( NAMED_UNIT ( * ) SI_UNIT ( $, .STERADIAN. ) SOLID_ANGLE_UNIT ( ) );
#57056 = AXIS2_PLACEMENT_3D ( 'NONE', #14992, #68430, #40677 ) ;
#57057 = ORIENTED_EDGE ( 'NONE', *, *, #1863, .F. ) ;
#57058 = CARTESIAN_POINT ( 'NONE',  ( -164.1550000000000011, 7.632228543268600340, 2.479861379858949277 ) ) ;
#57059 = ORIENTED_EDGE ( 'NONE', *, *, #67266, .F. ) ;
#57060 = CARTESIAN_POINT ( 'NONE',  ( -24.00000000000000000, 0.000000000000000000, 4.000000000000000000 ) ) ;
#57061 = FACE_OUTER_BOUND ( 'NONE', #34395, .T. ) ;
#57062 = VERTEX_POINT ( 'NONE', #64696 ) ;
#57063 = DIRECTION ( 'NONE',  ( -1.000000000000000000, 0.000000000000000000, 0.000000000000000000 ) ) ;
#57064 = CARTESIAN_POINT ( 'NONE',  ( -74.75000000000000000, -4.000000000000000000, 7.000000000000001776 ) ) ;
#57065 = CARTESIAN_POINT ( 'NONE',  ( 8.102448949553181734, 111.3949999999999818, 5.886773742842750679 ) ) ;
#57066 = EDGE_CURVE ( 'NONE', #67453, #28073, #19763, .T. ) ;
#57067 = ORIENTED_EDGE ( 'NONE', *, *, #3402, .F. ) ;
#57068 = LINE ( 'NONE', #46920, #22960 ) ;
#57069 = CARTESIAN_POINT ( 'NONE',  ( -5.598654528085806881, 113.8549999999999898, -7.705886871421374629 ) ) ;
#57070 = CARTESIAN_POINT ( 'NONE',  ( -73.40500000000000114, -2.607480562269069768, 8.024999999999991473 ) ) ;
#57071 = ORIENTED_EDGE ( 'NONE', *, *, #40055, .F. ) ;
#57072 = CARTESIAN_POINT ( 'NONE',  ( -3.094860106618434248, 135.9050000000000011, 9.525000000000000355 ) ) ;
#57073 =( LENGTH_UNIT ( ) NAMED_UNIT ( * ) SI_UNIT ( .MILLI., .METRE. ) );
#57074 = DIRECTION ( 'NONE',  ( 1.000000000000000000, 0.000000000000000000, 0.000000000000000000 ) ) ;
#57075 = CARTESIAN_POINT ( 'NONE',  ( -40.99999999999998579, 107.7459666924148394, 3.000000000000000000 ) ) ;
#57076 = DIRECTION ( 'NONE',  ( -0.000000000000000000, -1.000000000000000000, -0.000000000000000000 ) ) ;
#57077 = VERTEX_POINT ( 'NONE', #10878 ) ;
#57078 =( LENGTH_UNIT ( ) NAMED_UNIT ( * ) SI_UNIT ( .MILLI., .METRE. ) );
#57079 = DIRECTION ( 'NONE',  ( 0.000000000000000000, 1.000000000000000000, -0.000000000000000000 ) ) ;
#57080 = CARTESIAN_POINT ( 'NONE',  ( -57.14499999999997470, -4.716976649647092401, 6.492361379858946790 ) ) ;
#57081 = ORIENTED_EDGE ( 'NONE', *, *, #26347, .F. ) ;
#57082 = CARTESIAN_POINT ( 'NONE',  ( 7.968833018235900845, 111.2897112741109567, 3.588351662842293788 ) ) ;
#57083 =( BOUNDED_CURVE ( )  B_SPLINE_CURVE ( 2, ( #36867, #4440, #58280, #48120, #31888, #9423, #37219, #41800, #4092, #63221, #10108 ),
 .UNSPECIFIED., .F., .F. ) 
 B_SPLINE_CURVE_WITH_KNOTS ( ( 3, 2, 2, 2, 2, 3 ),
 ( 0.7173913043478260532, 0.7195652173913043015, 0.7217391304347826608, 0.7239130434782609091, 0.7260869565217391575, 0.7282608695652174058 ),
 .UNSPECIFIED. ) 
 CURVE ( )  GEOMETRIC_REPRESENTATION_ITEM ( )  RATIONAL_B_SPLINE_CURVE ( ( 1.000000000000000000, 0.9510565162951535312, 1.000000000000000000, 0.9510565162951535312, 1.000000000000000000, 0.9510565162951535312, 1.000000000000000000, 0.9510565162951535312, 1.000000000000000000, 0.9510565162951535312, 1.000000000000000000 ) ) 
 REPRESENTATION_ITEM ( '' )  );
#57084 = DIRECTION ( 'NONE',  ( 0.000000000000000000, 1.350863103983176297E-16, 1.000000000000000000 ) ) ;
#57085 = CARTESIAN_POINT ( 'NONE',  ( -45.00000000000000000, 8.162286782231383597, -6.987283332039737616 ) ) ;
#57086 = SURFACE_SIDE_STYLE ('',( #68348 ) ) ;
#57087 = EDGE_LOOP ( 'NONE', ( #20794, #10664, #35568, #942 ) ) ;
#57088 = DIRECTION ( 'NONE',  ( -0.000000000000000000, -1.000000000000000000, -0.000000000000000000 ) ) ;
#57089 = ORIENTED_EDGE ( 'NONE', *, *, #61237, .F. ) ;
#57090 = AXIS2_PLACEMENT_3D ( 'NONE', #27487, #2, #5682 ) ;
#57091 = EDGE_CURVE ( 'NONE', #28673, #66441, #60910, .T. ) ;
#57092 = CARTESIAN_POINT ( 'NONE',  ( -109.1050000000000040, -6.826472737025115478, 4.959722759717900331 ) ) ;
#57093 = ORIENTED_EDGE ( 'NONE', *, *, #8825, .F. ) ;
#57094 = ADVANCED_FACE ( 'NONE', ( #5926 ), #33233, .F. ) ;
#57095 = SURFACE_STYLE_USAGE ( .BOTH. , #47999 ) ;
#57096 = CARTESIAN_POINT ( 'NONE',  ( 23.49527607712185073, 27.44009427658185984, 27.19000446309344809 ) ) ;
#57097 = CARTESIAN_POINT ( 'NONE',  ( -141.2070736234661581, 3.094860106618433360, 9.524999999999991473 ) ) ;
#57098 = SURFACE_SIDE_STYLE ('',( #35660 ) ) ;
#57099 = CARTESIAN_POINT ( 'NONE',  ( 5.598654528085809545, 145.1450000000000102, -7.705886871421373741 ) ) ;
#57100 = CARTESIAN_POINT ( 'NONE',  ( -77.45707362346617231, -9.058813317711329915, 2.943386871421371787 ) ) ;
#57101 = EDGE_CURVE ( 'NONE', #56449, #43029, #36956, .T. ) ;
#57102 = DIRECTION ( 'NONE',  ( -1.000000000000000000, -0.000000000000000000, -0.000000000000000000 ) ) ;
#57103 = ORIENTED_EDGE ( 'NONE', *, *, #33153, .F. ) ;
#57104 = LINE ( 'NONE', #8926, #65304 ) ;
#57105 = CARTESIAN_POINT ( 'NONE',  ( -19.99962819189825680, -11.99984508003516304, 0.3398326153005359340 ) ) ;
#57106 = CARTESIAN_POINT ( 'NONE',  ( 7.632228543268607446, 120.1570736234661609, 2.479861379858954606 ) ) ;
#57107 = CARTESIAN_POINT ( 'NONE',  ( -125.7550000000000097, 4.716976649647091513, -6.492361379858946790 ) ) ;
#57108 = CARTESIAN_POINT ( 'NONE',  ( -181.9429263765338192, 0.000000000000000000, 9.524999999999991473 ) ) ;
#57109 =( NAMED_UNIT ( * ) PLANE_ANGLE_UNIT ( ) SI_UNIT ( $, .RADIAN. ) );
#57110 = CARTESIAN_POINT ( 'NONE',  ( -121.4949999999999761, 6.826472737025113702, -4.959722759717902107 ) ) ;
#57111 = EDGE_CURVE ( 'NONE', #52223, #67044, #69185, .T. ) ;
#57112 = CARTESIAN_POINT ( 'NONE',  ( -115.1949999999999932, 8.437984349512086979, -1.550032578732815448E-15 ) ) ;
#57113 = DIRECTION ( 'NONE',  ( 0.000000000000000000, 0.000000000000000000, -1.000000000000000000 ) ) ;
#57114 = ORIENTED_EDGE ( 'NONE', *, *, #50920, .F. ) ;
#57115 = PRESENTATION_STYLE_ASSIGNMENT (( #46262 ) ) ;
#57116 = DIRECTION ( 'NONE',  ( 0.6216216216216191581, 0.7833176619561879050, 0.000000000000000000 ) ) ;
#57117 = AXIS2_PLACEMENT_3D ( 'NONE', #21471, #20795, #52815 ) ;
#57118 = EDGE_CURVE ( 'NONE', #30231, #22278, #54558, .T. ) ;
#57119 = CARTESIAN_POINT ( 'NONE',  ( -168.8929263765337794, -8.102448949553172852, -5.886773742842741797 ) ) ;
#57120 = CARTESIAN_POINT ( 'NONE',  ( -181.6450000000000102, 4.716976649647091513, -6.492361379858946790 ) ) ;
#57121 = AXIS2_PLACEMENT_3D ( 'NONE', #50711, #47465, #10133 ) ;
#57122 = TOROIDAL_SURFACE ( 'NONE', #58243, 1.000000000000000000, 0.5000000000000000000 ) ;
#57123 = DIRECTION ( 'NONE',  ( 0.000000000000000000, 0.000000000000000000, -1.000000000000000000 ) ) ;
#57124 = CARTESIAN_POINT ( 'NONE',  ( 96.10348817448819148, 5.000000000000000000, 27.38099488609881149 ) ) ;
#57125 = VERTEX_POINT ( 'NONE', #12233 ) ;
#57126 = CARTESIAN_POINT ( 'NONE',  ( -83.09292637653381064, 3.094860106618433360, 9.524999999999991473 ) ) ;
#57127 = AXIS2_PLACEMENT_3D ( 'NONE', #19261, #62528, #40768 ) ;
#57128 = FILL_AREA_STYLE ('',( #2584 ) ) ;
#57129 = DIRECTION ( 'NONE',  ( 1.000000000000000000, 0.000000000000000000, 0.000000000000000000 ) ) ;
#57130 = COLOUR_RGB ( '', 0.31764706, 0.68627451, 0.89019608) ;
#57131 = SURFACE_STYLE_USAGE ( .BOTH. , #24422 ) ;
#57132 = EDGE_LOOP ( 'NONE', ( #5651, #55469, #2503, #7334 ) ) ;
#57133 = CARTESIAN_POINT ( 'NONE',  ( -195.0000000000000000, 1.166476076187852838E-15, -9.524999999999991473 ) ) ;
#57134 = CARTESIAN_POINT ( 'NONE',  ( -71.74137931034479720, 63.10081643261027295, -10.00000000000000000 ) ) ;
#57135 = PRESENTATION_STYLE_ASSIGNMENT (( #4006 ) ) ;
#57136 = ORIENTED_EDGE ( 'NONE', *, *, #22408, .T. ) ;
#57137 = CARTESIAN_POINT ( 'NONE',  ( -103.7929263765348225, -3.094860106601490024, 9.525000000012299850 ) ) ;
#57138 = AXIS2_PLACEMENT_3D ( 'NONE', #41, #64830, #44123 ) ;
#57139 = CARTESIAN_POINT ( 'NONE',  ( 4.716976649647099507, 129.7570736234661695, -6.492361379858953008 ) ) ;
#57140 =( LENGTH_UNIT ( ) NAMED_UNIT ( * ) SI_UNIT ( .MILLI., .METRE. ) );
#57141 = EDGE_CURVE ( 'NONE', #10038, #29168, #24230, .T. ) ;
#57142 = ORIENTED_EDGE ( 'NONE', *, *, #24584, .F. ) ;
#57143 = CARTESIAN_POINT ( 'NONE',  ( -104.4549999999999983, 7.632228543268599452, -2.479861379858951942 ) ) ;
#57144 = VECTOR ( 'NONE', #58662, 1000.000000000000000 ) ;
#57145 = CARTESIAN_POINT ( 'NONE',  ( 0.000000000000000000, 2.000000000000000444, 0.000000000000000000 ) ) ;
#57146 = ORIENTED_EDGE ( 'NONE', *, *, #26347, .T. ) ;
#57147 = SURFACE_STYLE_FILL_AREA ( #51201 ) ;
#57148 = DIRECTION ( 'NONE',  ( 0.000000000000000000, 0.000000000000000000, 1.000000000000000000 ) ) ;
#57149 = CARTESIAN_POINT ( 'NONE',  ( -74.99999999999998579, 50.00000000000000000, 6.500000000000000000 ) ) ;
#57150 = FILL_AREA_STYLE ('',( #36793 ) ) ;
#57151 = ORIENTED_EDGE ( 'NONE', *, *, #60488, .T. ) ;
#57152 = CARTESIAN_POINT ( 'NONE',  ( 10.99999999999999645, 11.99999999999999289, 3.500000000000004885 ) ) ;
#57153 = CARTESIAN_POINT ( 'NONE',  ( -84.59499999999998465, 2.607480562269073321, 8.024999999999991473 ) ) ;
#57154 = ORIENTED_EDGE ( 'NONE', *, *, #1927, .F. ) ;
#57155 = PRESENTATION_STYLE_ASSIGNMENT (( #58212 ) ) ;
#57156 = ADVANCED_FACE ( 'NONE', ( #55511 ), #54465, .F. ) ;
#57157 =( NAMED_UNIT ( * ) SI_UNIT ( $, .STERADIAN. ) SOLID_ANGLE_UNIT ( ) );
#57158 = AXIS2_PLACEMENT_3D ( 'NONE', #29334, #23373, #38301 ) ;
#57159 = UNCERTAINTY_MEASURE_WITH_UNIT (LENGTH_MEASURE( 1.000000000000000082E-05 ), #57173, 'distance_accuracy_value', 'NONE');
#57160 = ORIENTED_EDGE ( 'NONE', *, *, #21858, .F. ) ;
#57161 =( LENGTH_UNIT ( ) NAMED_UNIT ( * ) SI_UNIT ( .MILLI., .METRE. ) );
#57162 = EDGE_CURVE ( 'NONE', #54309, #60087, #47910, .T. ) ;
#57163 = DIRECTION ( 'NONE',  ( -0.000000000000000000, -0.000000000000000000, -1.000000000000000000 ) ) ;
#57164 = CARTESIAN_POINT ( 'NONE',  ( 12.72792206135785698, 115.4999999999999574, 10.50000000000000000 ) ) ;
#57165 = VERTEX_POINT ( 'NONE', #11558 ) ;
#57166 = EDGE_CURVE ( 'NONE', #65417, #17573, #918, .T. ) ;
#57167 = ADVANCED_BREP_SHAPE_REPRESENTATION ( '', ( #3590, #42840 ), #2196 ) ;
#57168 = ORIENTED_EDGE ( 'NONE', *, *, #28016, .T. ) ;
#57169 = PRESENTATION_STYLE_ASSIGNMENT (( #67385 ) ) ;
#57170 = CARTESIAN_POINT ( 'NONE',  ( -9.827790563157511022E-16, 122.5570736234661524, 8.025000000000000355 ) ) ;
#57171 = CARTESIAN_POINT ( 'NONE',  ( 10.00000000000001776, 17.78868675966041835, -1.300977106640437060E-15 ) ) ;
#57172 = CARTESIAN_POINT ( 'NONE',  ( -170.7570736234661695, -5.598654528085801552, 7.705886871421367523 ) ) ;
#57173 =( LENGTH_UNIT ( ) NAMED_UNIT ( * ) SI_UNIT ( .MILLI., .METRE. ) );
#57174 = CARTESIAN_POINT ( 'NONE',  ( 65.00000000000000000, 2.409368300552961372E-15, 6.999999999999988454 ) ) ;
#57175 = AXIS2_PLACEMENT_3D ( 'NONE', #16728, #65225, #58567 ) ;
#57176 = CARTESIAN_POINT ( 'NONE',  ( -104.9070736234661751, -3.094860106618429807, 9.524999999999991473 ) ) ;
#57177 = CARTESIAN_POINT ( 'NONE',  ( 16.75000000000000711, 25.24999999999998224, 4.000000000000000000 ) ) ;
#57178 = EDGE_CURVE ( 'NONE', #4180, #28025, #52388, .T. ) ;
#57179 = DIRECTION ( 'NONE',  ( 1.000000000000000000, 0.000000000000000000, 0.000000000000000000 ) ) ;
#57180 = VERTEX_POINT ( 'NONE', #7335 ) ;
#57181 = STYLED_ITEM ( 'NONE', ( #54532 ), #51390 ) ;
#57182 = FILL_AREA_STYLE ('',( #51570 ) ) ;
#57183 = DIRECTION ( 'NONE',  ( 0.000000000000000000, 0.000000000000000000, 1.000000000000000000 ) ) ;
#57184 = ADVANCED_FACE ( 'NONE', ( #60093 ), #49558, .T. ) ;
#57186 = LINE ( 'NONE', #19895, #7732 ) ;
#57185 = DIRECTION ( 'NONE',  ( 0.000000000000000000, -0.000000000000000000, -1.000000000000000000 ) ) ;
#57187 = DIRECTION ( 'NONE',  ( 0.000000000000000000, 0.000000000000000000, 1.000000000000000000 ) ) ;
#57188 = CARTESIAN_POINT ( 'NONE',  ( -151.1049999999999613, -6.826472737025115478, 4.959722759717900331 ) ) ;
#57189 = CARTESIAN_POINT ( 'NONE',  ( -8.035490232227735063, 111.7463764333768097, 2.031712422923528383 ) ) ;
#57190 = CARTESIAN_POINT ( 'NONE',  ( -152.2450000000000045, -4.716976649647093289, -6.492361379858945902 ) ) ;
#57191 = PRESENTATION_LAYER_ASSIGNMENT (  '', '', ( #54963 ) ) ;
#57192 = CARTESIAN_POINT ( 'NONE',  ( -143.5449999999999875, -7.632228543268600340, -2.479861379858950166 ) ) ;
#57193 = EDGE_LOOP ( 'NONE', ( #2242, #23858, #44677, #30358, #49591, #33284, #32856, #32309 ) ) ;
#57194 = CARTESIAN_POINT ( 'NONE',  ( 30.99999999999999289, 5.000000000000000000, -24.00402776293822171 ) ) ;
#57195 =( NAMED_UNIT ( * ) SI_UNIT ( $, .STERADIAN. ) SOLID_ANGLE_UNIT ( ) );
#57196 = DIRECTION ( 'NONE',  ( -0.000000000000000000, -0.000000000000000000, -1.000000000000000000 ) ) ;
#57197 = UNCERTAINTY_MEASURE_WITH_UNIT (LENGTH_MEASURE( 1.000000000000000082E-05 ), #62497, 'distance_accuracy_value', 'NONE');
#57198 = CARTESIAN_POINT ( 'NONE',  ( -60.65499999999998693, -7.632228543268600340, -2.479861379858950166 ) ) ;
#57199 = CIRCLE ( 'NONE', #54969, 4.999999999999997335 ) ;
#57200 = CARTESIAN_POINT ( 'NONE',  ( -61.94499999999998607, -9.827790563157499189E-16, -8.024999999999991473 ) ) ;
#57201 = CARTESIAN_POINT ( 'NONE',  ( 10.01517768586949231, 160.8049999999999216, 1.839758294383810543E-15 ) ) ;
#57202 = EDGE_CURVE ( 'NONE', #54282, #54365, #35496, .T. ) ;
#57203 = CARTESIAN_POINT ( 'NONE',  ( 71.50000000000000000, 14.49137674618942562, -10.00000000000000000 ) ) ;
#57204 = DIRECTION ( 'NONE',  ( 0.000000000000000000, 0.000000000000000000, 1.000000000000000000 ) ) ;
#57205 = EDGE_CURVE ( 'NONE', #69157, #24621, #7430, .T. ) ;
#57206 = AXIS2_PLACEMENT_3D ( 'NONE', #12164, #18157, #39639 ) ;
#57207 = UNCERTAINTY_MEASURE_WITH_UNIT (LENGTH_MEASURE( 1.000000000000000082E-05 ), #30997, 'distance_accuracy_value', 'NONE');
#57208 =( LENGTH_UNIT ( ) NAMED_UNIT ( * ) SI_UNIT ( .MILLI., .METRE. ) );
#57209 = CARTESIAN_POINT ( 'NONE',  ( 0.000000000000000000, 145.0570736234661524, -8.025000000000000355 ) ) ;
#57210 = VECTOR ( 'NONE', #50133, 1000.000000000000000 ) ;
#57211 = CARTESIAN_POINT ( 'NONE',  ( 45.50000000000000000, 1.797044900979284448E-15, -6.999999999999999112 ) ) ;
#57212 = CARTESIAN_POINT ( 'NONE',  ( -177.7429263765338021, -5.598654528085803328, -7.705886871421366635 ) ) ;
#57213 =( GEOMETRIC_REPRESENTATION_CONTEXT ( 3 ) GLOBAL_UNCERTAINTY_ASSIGNED_CONTEXT ( ( #24981 ) ) GLOBAL_UNIT_ASSIGNED_CONTEXT ( ( #50719, #1058, #18371 ) ) REPRESENTATION_CONTEXT ( 'NONE', 'WORKASPACE' ) );
#57214 = PRESENTATION_STYLE_ASSIGNMENT (( #35772 ) ) ;
#57215 = VECTOR ( 'NONE', #8257, 1000.000000000000000 ) ;
#57216 = DIRECTION ( 'NONE',  ( -1.000000000000000000, 0.000000000000000000, 0.000000000000000000 ) ) ;
#57217 = EDGE_LOOP ( 'NONE', ( #38420, #18071, #5249, #35371 ) ) ;
#57218 = STYLED_ITEM ( 'NONE', ( #3309 ), #10598 ) ;
#57219 = ORIENTED_EDGE ( 'NONE', *, *, #31051, .T. ) ;
#57220 =( NAMED_UNIT ( * ) PLANE_ANGLE_UNIT ( ) SI_UNIT ( $, .RADIAN. ) );
#57221 = VECTOR ( 'NONE', #38148, 1000.000000000000114 ) ;
#57223 = AXIS2_PLACEMENT_3D ( 'NONE', #66979, #39224, #12097 ) ;
#57222 = FILL_AREA_STYLE_COLOUR ( '', #45082 ) ;
#57224 = PRESENTATION_LAYER_ASSIGNMENT (  '', '', ( #69585 ) ) ;
#57225 = AXIS2_PLACEMENT_3D ( 'NONE', #5764, #48753, #452 ) ;
#57226 =( NAMED_UNIT ( * ) PLANE_ANGLE_UNIT ( ) SI_UNIT ( $, .RADIAN. ) );
#57227 = CARTESIAN_POINT ( 'NONE',  ( 74.50000000000000000, 3.473944261090200865E-15, 9.500000000000000000 ) ) ;
#57228 = ORIENTED_EDGE ( 'NONE', *, *, #29644, .F. ) ;
#57229 = VERTEX_POINT ( 'NONE', #60767 ) ;
#57230 = SURFACE_STYLE_USAGE ( .BOTH. , #46745 ) ;
#57231 = EDGE_LOOP ( 'NONE', ( #39625, #42861, #58355, #10304 ) ) ;
#57232 = CARTESIAN_POINT ( 'NONE',  ( 3.094860106618431583, 115.2049999999999983, 9.525000000000000355 ) ) ;
#57233 = LINE ( 'NONE', #13626, #4020 ) ;
#57234 = ORIENTED_EDGE ( 'NONE', *, *, #28096, .T. ) ;
#57235 = EDGE_CURVE ( 'NONE', #21322, #54480, #23145, .T. ) ;
#57236 = PRESENTATION_LAYER_ASSIGNMENT (  '', '', ( #23545 ) ) ;
#57237 = LINE ( 'NONE', #2321, #18201 ) ;
#57238 = CARTESIAN_POINT ( 'NONE',  ( -108.7449999999999903, 4.716976649647094177, 6.492361379858945902 ) ) ;
#57239 = ORIENTED_EDGE ( 'NONE', *, *, #57355, .F. ) ;
#57240 = CIRCLE ( 'NONE', #52751, 0.2500000000000002220 ) ;
#57241 = CYLINDRICAL_SURFACE ( 'NONE', #62510, 3.100000000000005418 ) ;
#57242 = FACE_OUTER_BOUND ( 'NONE', #68151, .T. ) ;
#57243 = EDGE_CURVE ( 'NONE', #16376, #8059, #22124, .T. ) ;
#57244 =( NAMED_UNIT ( * ) PLANE_ANGLE_UNIT ( ) SI_UNIT ( $, .RADIAN. ) );
#57245 = VERTEX_POINT ( 'NONE', #44999 ) ;
#57246 = CARTESIAN_POINT ( 'NONE',  ( -8.437984349512095861, 144.6929263765337907, -5.166775262442723748E-16 ) ) ;
#57247 = PLANE ( 'NONE',  #31271 ) ;
#57248 = DIRECTION ( 'NONE',  ( -0.000000000000000000, -0.000000000000000000, -1.000000000000000000 ) ) ;
#57249 = EDGE_CURVE ( 'NONE', #6919, #32327, #43618, .T. ) ;
#57250 = SURFACE_STYLE_FILL_AREA ( #68513 ) ;
#57251 = ORIENTED_EDGE ( 'NONE', *, *, #21523, .T. ) ;
#57252 = SURFACE_STYLE_USAGE ( .BOTH. , #61470 ) ;
#57253 = ORIENTED_EDGE ( 'NONE', *, *, #19994, .T. ) ;
#57254 = DIRECTION ( 'NONE',  ( -0.000000000000000000, -1.000000000000000000, 0.000000000000000000 ) ) ;
#57255 = FACE_OUTER_BOUND ( 'NONE', #42251, .T. ) ;
#57256 = CARTESIAN_POINT ( 'NONE',  ( -141.1429263765338078, 5.598654528085800663, -7.705886871421367523 ) ) ;
#57257 = CARTESIAN_POINT ( 'NONE',  ( 17.25000000000000711, 25.24999999999998224, 4.000000000000000000 ) ) ;
#57258 = CARTESIAN_POINT ( 'NONE',  ( -123.5049999999999955, -6.826472737025115478, -4.959722759717899443 ) ) ;
#57259 = AXIS2_PLACEMENT_3D ( 'NONE', #64942, #43893, #7262 ) ;
#57260 = VECTOR ( 'NONE', #66892, 1000.000000000000000 ) ;
#57261 = CYLINDRICAL_SURFACE ( 'NONE', #28710, 0.5000000000000004441 ) ;
#57262 = AXIS2_PLACEMENT_3D ( 'NONE', #69338, #21130, #4599 ) ;
#57263 = CARTESIAN_POINT ( 'NONE',  ( -74.08841717987164088, 9.415467456214850372, 6.077850184675972933 ) ) ;
#57264 = CARTESIAN_POINT ( 'NONE',  ( 27.99999999999999645, 0.000000000000000000, -72.00402776293822171 ) ) ;
#57265 = DIRECTION ( 'NONE',  ( 0.000000000000000000, 0.000000000000000000, -1.000000000000000000 ) ) ;
#57266 = ORIENTED_EDGE ( 'NONE', *, *, #11129, .F. ) ;
#57267 = EDGE_LOOP ( 'NONE', ( #4947, #53950, #12920 ) ) ;
#57268 = CARTESIAN_POINT ( 'NONE',  ( -11.33578643762689708, 3.244476573706588632E-16, 19.41421356237309581 ) ) ;
#57269 = FILL_AREA_STYLE_COLOUR ( '', #50053 ) ;
#57270 = EDGE_CURVE ( 'NONE', #27592, #3932, #17537, .T. ) ;
#57271 = CARTESIAN_POINT ( 'NONE',  ( 6.759171781091399822, -2.392512705203733603, 2.292771058063876488 ) ) ;
#57272 =( LENGTH_UNIT ( ) NAMED_UNIT ( * ) SI_UNIT ( .MILLI., .METRE. ) );
#57273 = ORIENTED_EDGE ( 'NONE', *, *, #10042, .T. ) ;
#57274 = SURFACE_STYLE_FILL_AREA ( #25945 ) ;
#57275 = CARTESIAN_POINT ( 'NONE',  ( -183.2050000000000125, -2.607480562269071545, -8.024999999999991473 ) ) ;
#57276 = CARTESIAN_POINT ( 'NONE',  ( 60.00000000000000000, -2.024042244987997205E-14, 10.00000000000000000 ) ) ;
#57277 = VECTOR ( 'NONE', #40818, 1000.000000000000000 ) ;
#57278 = CARTESIAN_POINT ( 'NONE',  ( -53.30707362346616662, -10.01517768586948698, 6.132527647946031529E-16 ) ) ;
#57279 = AXIS2_PLACEMENT_3D ( 'NONE', #54190, #60846, #27778 ) ;
#57280 = CARTESIAN_POINT ( 'NONE',  ( -179.6949999999999932, -8.437984349512086979, 5.166775262442717831E-16 ) ) ;
#57281 = CIRCLE ( 'NONE', #36012, 10.00000000000000178 ) ;
#57282 = ORIENTED_EDGE ( 'NONE', *, *, #3371, .F. ) ;
#57283 = SURFACE_STYLE_FILL_AREA ( #15110 ) ;
#57284 = SURFACE_STYLE_USAGE ( .BOTH. , #41480 ) ;
#57285 = CARTESIAN_POINT ( 'NONE',  ( -88.85499999999998977, 4.716976649647094177, 6.492361379858945902 ) ) ;
#57286 = CARTESIAN_POINT ( 'NONE',  ( -41.49999999999998579, 99.99999999999998579, 3.000000000000000000 ) ) ;
#57287 = PRESENTATION_STYLE_ASSIGNMENT (( #9471 ) ) ;
#57288 = CIRCLE ( 'NONE', #67422, 0.2500000000000002220 ) ;
#57289 = DIRECTION ( 'NONE',  ( 0.000000000000000000, -0.1048768571002353378, 0.9944852160011111719 ) ) ;
#57290 = CARTESIAN_POINT ( 'NONE',  ( -86.99499999999997613, -6.826472737025113702, 4.959722759717902107 ) ) ;
#57291 = CARTESIAN_POINT ( 'NONE',  ( 9.058813317711337021, 127.6549999999999869, 2.943386871421375783 ) ) ;
#57292 = CARTESIAN_POINT ( 'NONE',  ( -70.49499999999996191, 6.826472737025113702, -4.959722759717902107 ) ) ;
#57293 = CARTESIAN_POINT ( 'NONE',  ( 71.50000000000000000, 14.49137674618942562, -7.000000000000000000 ) ) ;
#57294 = CIRCLE ( 'NONE', #14630, 1.000000000000000888 ) ;
#57295 = CARTESIAN_POINT ( 'NONE',  ( 3.999798566743339556, 49.09558629977726696, -2.000000000000000000 ) ) ;
#57296 = DIRECTION ( 'NONE',  ( -0.000000000000000000, -1.000000000000000000, -0.000000000000000000 ) ) ;
#57297 = EDGE_CURVE ( 'NONE', #23279, #17642, #32125, .T. ) ;
#57298 = UNCERTAINTY_MEASURE_WITH_UNIT (LENGTH_MEASURE( 1.000000000000000082E-05 ), #219, 'distance_accuracy_value', 'NONE');
#57299 = AXIS2_PLACEMENT_3D ( 'NONE', #16248, #15890, #37371 ) ;
#57300 = CARTESIAN_POINT ( 'NONE',  ( 1.000000000000000000, 36.74999999999999289, 3.750000000000000000 ) ) ;
#57301 = CARTESIAN_POINT ( 'NONE',  ( -48.44292637653380496, -1.166476076187852838E-15, -9.524999999999991473 ) ) ;
#57302 = ORIENTED_EDGE ( 'NONE', *, *, #19442, .F. ) ;
#57303 = CARTESIAN_POINT ( 'NONE',  ( -101.6929263765337907, 10.01517768586948698, -1.839758294383808571E-15 ) ) ;
#57304 = CARTESIAN_POINT ( 'NONE',  ( -126.1450000000000102, -4.716976649647092401, 6.492361379858946790 ) ) ;
#57305 = FILL_AREA_STYLE_COLOUR ( '', #23540 ) ;
#57306 = MECHANICAL_DESIGN_GEOMETRIC_PRESENTATION_REPRESENTATION (  '', ( #56136 ), #31484 ) ;
#57307 = CARTESIAN_POINT ( 'NONE',  ( -1.953228634907021810, 72.00000000000001421, -6.349999999999997868 ) ) ;
#57308 = CARTESIAN_POINT ( 'NONE',  ( -83.49999999999998579, 4.336808689942018722E-16, 24.00000000000000000 ) ) ;
#57309 = ORIENTED_EDGE ( 'NONE', *, *, #63776, .F. ) ;
#57310 = ORIENTED_EDGE ( 'NONE', *, *, #58427, .F. ) ;
#57311 = PRESENTATION_LAYER_ASSIGNMENT (  '', '', ( #18003 ) ) ;
#57312 = CARTESIAN_POINT ( 'NONE',  ( -62.69292637653379785, 10.01517768586948698, -1.839758294383808966E-15 ) ) ;
#57313 = AXIS2_PLACEMENT_3D ( 'NONE', #67504, #3080, #62225 ) ;
#57314 = LINE ( 'NONE', #9148, #19197 ) ;
#57315 = CARTESIAN_POINT ( 'NONE',  ( 2.755156416437879674, 1.983268963961027920, 7.000000000000000888 ) ) ;
#57316 = DIRECTION ( 'NONE',  ( 0.000000000000000000, -1.000000000000000000, 0.000000000000000000 ) ) ;
#57317 = ORIENTED_EDGE ( 'NONE', *, *, #23212, .F. ) ;
#57318 = CARTESIAN_POINT ( 'NONE',  ( -131.7549999999999955, 4.716976649647091513, -6.492361379858946790 ) ) ;
#57319 = EDGE_LOOP ( 'NONE', ( #66332, #64679, #38729 ) ) ;
#57320 = DIRECTION ( 'NONE',  ( 0.000000000000000000, 0.000000000000000000, 1.000000000000000000 ) ) ;
#57321 = CARTESIAN_POINT ( 'NONE',  ( -121.8570736234661780, -5.598654528085803328, -7.705886871421366635 ) ) ;
#57322 = ORIENTED_EDGE ( 'NONE', *, *, #45068, .T. ) ;
#57323 = CARTESIAN_POINT ( 'NONE',  ( -171.5929263765339670, -3.094860106621170281, -9.524999999998001954 ) ) ;
#57324 = FILL_AREA_STYLE ('',( #8108 ) ) ;
#57325 = VERTEX_POINT ( 'NONE', #8713 ) ;
#57326 = ADVANCED_FACE ( 'NONE', ( #36792 ), #57944, .F. ) ;
#57327 = FILL_AREA_STYLE ('',( #25652 ) ) ;
#57328 =( GEOMETRIC_REPRESENTATION_CONTEXT ( 3 ) GLOBAL_UNCERTAINTY_ASSIGNED_CONTEXT ( ( #6037 ) ) GLOBAL_UNIT_ASSIGNED_CONTEXT ( ( #21068, #15817, #37298 ) ) REPRESENTATION_CONTEXT ( 'NONE', 'WORKASPACE' ) );
#57329 = CARTESIAN_POINT ( 'NONE',  ( -3.094860106618434248, 140.7950000000000159, 9.525000000000000355 ) ) ;
#57330 =( NAMED_UNIT ( * ) PLANE_ANGLE_UNIT ( ) SI_UNIT ( $, .RADIAN. ) );
#57331 = ORIENTED_EDGE ( 'NONE', *, *, #63967, .F. ) ;
#57332 = FACE_OUTER_BOUND ( 'NONE', #44620, .T. ) ;
#57333 = CARTESIAN_POINT ( 'NONE',  ( 10.01517768586949408, 148.8050000000000068, 1.839758294383810543E-15 ) ) ;
#57334 = LINE ( 'NONE', #25325, #2384 ) ;
#57335 = AXIS2_PLACEMENT_3D ( 'NONE', #53349, #10774, #5129 ) ;
#57336 = ORIENTED_EDGE ( 'NONE', *, *, #19865, .F. ) ;
#57337 = CARTESIAN_POINT ( 'NONE',  ( 4.716976649647099507, 116.6429263765338078, -6.492361379858953008 ) ) ;
#57338 = CARTESIAN_POINT ( 'NONE',  ( 44.99999999999998579, 119.9999999999999716, -9.500000000000000000 ) ) ;
#57339 = UNCERTAINTY_MEASURE_WITH_UNIT (LENGTH_MEASURE( 1.000000000000000082E-05 ), #21327, 'distance_accuracy_value', 'NONE');
#57340 = DIRECTION ( 'NONE',  ( 0.000000000000000000, 0.000000000000000000, -1.000000000000000000 ) ) ;
#57341 = AXIS2_PLACEMENT_3D ( 'NONE', #33854, #65882, #5730 ) ;
#57342 = CYLINDRICAL_SURFACE ( 'NONE', #25462, 30.00000000000000000 ) ;
#57343 = CARTESIAN_POINT ( 'NONE',  ( -1.445602896647333671E-14, 18.74999999999994671, 4.000000000000000000 ) ) ;
#57344 = EDGE_CURVE ( 'NONE', #15724, #57165, #66930, .T. ) ;
#57345 = PLANE ( 'NONE',  #64662 ) ;
#57346 = ORIENTED_EDGE ( 'NONE', *, *, #60667, .T. ) ;
#57347 = STYLED_ITEM ( 'NONE', ( #36612 ), #17422 ) ;
#57348 = CARTESIAN_POINT ( 'NONE',  ( -6.418790567836333949, 2.882328613363593917, 0.02778322089669647138 ) ) ;
#57349 = ORIENTED_EDGE ( 'NONE', *, *, #18872, .F. ) ;
#57350 = CARTESIAN_POINT ( 'NONE',  ( -60.29292637653380638, 3.094860106618428031, -9.524999999999993250 ) ) ;
#57351 = AXIS2_PLACEMENT_3D ( 'NONE', #49181, #33335, #6247 ) ;
#57352 =( NAMED_UNIT ( * ) PLANE_ANGLE_UNIT ( ) SI_UNIT ( $, .RADIAN. ) );
#57353 =( LENGTH_UNIT ( ) NAMED_UNIT ( * ) SI_UNIT ( .MILLI., .METRE. ) );
#57354 = CARTESIAN_POINT ( 'NONE',  ( -148.1049999999999898, -6.826472737025115478, 4.959722759717900331 ) ) ;
#57356 = ORIENTED_EDGE ( 'NONE', *, *, #64224, .T. ) ;
#57355 = EDGE_CURVE ( 'NONE', #51004, #54282, #46031, .T. ) ;
#57357 =( LENGTH_UNIT ( ) NAMED_UNIT ( * ) SI_UNIT ( .MILLI., .METRE. ) );
#57358 = UNCERTAINTY_MEASURE_WITH_UNIT (LENGTH_MEASURE( 1.000000000000000082E-05 ), #58122, 'distance_accuracy_value', 'NONE');
#57359 = CIRCLE ( 'NONE', #29262, 0.2500000000000002220 ) ;
#57360 = PRODUCT_DEFINITION_FORMATION_WITH_SPECIFIED_SOURCE ( 'ANY', '', #26552, .NOT_KNOWN. ) ;
#57361 = EDGE_CURVE ( 'NONE', #63234, #68810, #15413, .T. ) ;
#57362 = DIRECTION ( 'NONE',  ( -1.982541115402069054E-16, -0.000000000000000000, -1.000000000000000000 ) ) ;
#57363 = CARTESIAN_POINT ( 'NONE',  ( 74.50000000000000000, 19.30628705663858113, 6.500000000000000888 ) ) ;
#57364 = CARTESIAN_POINT ( 'NONE',  ( 2.607480562269155921, 145.5929263765338533, 8.024999999999941735 ) ) ;
#57365 = ORIENTED_EDGE ( 'NONE', *, *, #850, .T. ) ;
#57366 = STYLED_ITEM ( 'NONE', ( #68825 ), #13601 ) ;
#57367 = EDGE_LOOP ( 'NONE', ( #34046, #44434, #28918 ) ) ;
#57368 = CARTESIAN_POINT ( 'NONE',  ( -96.05707362346618083, 0.000000000000000000, 9.524999999999991473 ) ) ;
#57369 = ADVANCED_FACE ( 'NONE', ( #47347 ), #47720, .T. ) ;
#57370 = DIRECTION ( 'NONE',  ( -1.000000000000000000, 0.000000000000000000, 0.000000000000000000 ) ) ;
#57371 = CARTESIAN_POINT ( 'NONE',  ( -66.95499999999998408, -7.632228543268599452, 2.479861379858951054 ) ) ;
#57372 = VERTEX_POINT ( 'NONE', #29814 ) ;
#57373 = CARTESIAN_POINT ( 'NONE',  ( 1.000000000000000000, 42.00000000000000000, 79.00402776293826435 ) ) ;
#57374 = MECHANICAL_DESIGN_GEOMETRIC_PRESENTATION_REPRESENTATION (  '', ( #9069 ), #5625 ) ;
#57375 =( NAMED_UNIT ( * ) PLANE_ANGLE_UNIT ( ) SI_UNIT ( $, .RADIAN. ) );
#57376 = DIRECTION ( 'NONE',  ( 0.000000000000000000, 0.000000000000000000, 1.000000000000000000 ) ) ;
#57377 = EDGE_LOOP ( 'NONE', ( #39491, #9410, #17966, #43231 ) ) ;
#57378 = MECHANICAL_DESIGN_GEOMETRIC_PRESENTATION_REPRESENTATION (  '', ( #51767 ), #67450 ) ;
#57379 =( GEOMETRIC_REPRESENTATION_CONTEXT ( 3 ) GLOBAL_UNCERTAINTY_ASSIGNED_CONTEXT ( ( #61566 ) ) GLOBAL_UNIT_ASSIGNED_CONTEXT ( ( #18940, #25279, #35143 ) ) REPRESENTATION_CONTEXT ( 'NONE', 'WORKASPACE' ) );
#57380 = DIRECTION ( 'NONE',  ( -0.000000000000000000, 1.000000000000000000, -0.000000000000000000 ) ) ;
#57381 = CARTESIAN_POINT ( 'NONE',  ( -7.500000000000000000, 0.000000000000000000, 0.2499999999999924227 ) ) ;
#57382 =( BOUNDED_CURVE ( )  B_SPLINE_CURVE ( 2, ( #19052, #52160, #61976, #30653, #3917, #67615, #40561, #19418, #68316, #24339, #14860 ),
 .UNSPECIFIED., .F., .F. ) 
 B_SPLINE_CURVE_WITH_KNOTS ( ( 3, 2, 2, 2, 2, 3 ),
 ( 0.1470588235294118806, 0.1529411764705883026, 0.1588235294117646967, 0.1647058823529411464, 0.1705882352941175684, 0.1764705882352939903 ),
 .UNSPECIFIED. ) 
 CURVE ( )  GEOMETRIC_REPRESENTATION_ITEM ( )  RATIONAL_B_SPLINE_CURVE ( ( 0.9999999999999991118, 0.9510565162951544194, 1.000000000000000000, 0.9510565162951535312, 1.000000000000000000, 0.9510565162951535312, 1.000000000000000000, 0.9510565162951535312, 1.000000000000000000, 0.9510565162951546414, 0.9999999999999988898 ) ) 
 REPRESENTATION_ITEM ( '' )  );
#57384 = CARTESIAN_POINT ( 'NONE',  ( 0.000000000000000000, 2.500000000000000000, 0.000000000000000000 ) ) ;
#57383 = DIRECTION ( 'NONE',  ( -1.000000000000000000, 0.000000000000000000, 0.000000000000000000 ) ) ;
#57385 = CARTESIAN_POINT ( 'NONE',  ( 9.058813317711337021, 144.5449999999999875, 2.943386871421375783 ) ) ;
#57386 = CARTESIAN_POINT ( 'NONE',  ( -96.59499999999998465, 2.607480562269073321, 8.024999999999991473 ) ) ;
#57387 = AXIS2_PLACEMENT_3D ( 'NONE', #25814, #58884, #58527 ) ;
#57388 = DIRECTION ( 'NONE',  ( 0.000000000000000000, 0.000000000000000000, 1.000000000000000000 ) ) ;
#57389 = DIRECTION ( 'NONE',  ( 0.000000000000000000, -1.000000000000000000, 0.000000000000000000 ) ) ;
#57390 = AXIS2_PLACEMENT_3D ( 'NONE', #67717, #63123, #2303 ) ;
#57391 = UNCERTAINTY_MEASURE_WITH_UNIT (LENGTH_MEASURE( 1.000000000000000082E-05 ), #33937, 'distance_accuracy_value', 'NONE');
#57392 = CARTESIAN_POINT ( 'NONE',  ( -72.29292637653379927, 3.094860106618428031, -9.524999999999993250 ) ) ;
#57393 = ORIENTED_EDGE ( 'NONE', *, *, #57361, .T. ) ;
#57394 = CARTESIAN_POINT ( 'NONE',  ( -146.3929263765337794, 8.102448949553176405, 5.886773742842740909 ) ) ;
#57395 = CARTESIAN_POINT ( 'NONE',  ( 53.24999999999999289, 27.74999999999998579, 3.750000000000000000 ) ) ;
#57396 = CARTESIAN_POINT ( 'NONE',  ( -158.5449999999999875, -7.632228543268600340, -2.479861379858950166 ) ) ;
#57397 = STYLED_ITEM ( 'NONE', ( #51971 ), #52832 ) ;
#57398 = FILL_AREA_STYLE_COLOUR ( '', #22497 ) ;
#57399 = CARTESIAN_POINT ( 'NONE',  ( -195.0000000000000000, 0.000000000000000000, 0.000000000000000000 ) ) ;
#57400 = CARTESIAN_POINT ( 'NONE',  ( -132.8929263765337794, -8.102448949553174629, -5.886773742842741797 ) ) ;
#57401 = ORIENTED_EDGE ( 'NONE', *, *, #14299, .F. ) ;
#57402 = DIRECTION ( 'NONE',  ( -1.000000000000000000, 0.000000000000000000, 0.000000000000000000 ) ) ;
#57403 = EDGE_LOOP ( 'NONE', ( #57858, #22227, #51432 ) ) ;
#57404 =( BOUNDED_CURVE ( )  B_SPLINE_CURVE ( 2, ( #51299, #45369, #12606, #50602, #55531, #3040, #55874, #39387, #13293, #8035, #61152 ),
 .UNSPECIFIED., .F., .F. ) 
 B_SPLINE_CURVE_WITH_KNOTS ( ( 3, 2, 2, 2, 2, 3 ),
 ( 0.5882352941176473005, 0.5941176470588236391, 0.5999999999999999778, 0.6058823529411763165, 0.6117647058823527662, 0.6176470588235291048 ),
 .UNSPECIFIED. ) 
 CURVE ( )  GEOMETRIC_REPRESENTATION_ITEM ( )  RATIONAL_B_SPLINE_CURVE ( ( 0.9999999999999981126, 0.9510565162951554186, 1.000000000000000000, 0.9510565162951535312, 1.000000000000000000, 0.9510565162951535312, 1.000000000000000000, 0.9510565162951535312, 1.000000000000000000, 0.9510565162951563067, 0.9999999999999972244 ) ) 
 REPRESENTATION_ITEM ( '' )  );
#57405 = VECTOR ( 'NONE', #22021, 1000.000000000000000 ) ;
#57406 = CARTESIAN_POINT ( 'NONE',  ( -15.48999599679679662, 146.4999999999999716, 9.500000000000000000 ) ) ;
#57407 = LINE ( 'NONE', #56349, #67460 ) ;
#57408 = CARTESIAN_POINT ( 'NONE',  ( 67.50000000000000000, 1.797044900979284448E-15, 12.00000000000000000 ) ) ;
#57409 = CARTESIAN_POINT ( 'NONE',  ( -59.44836694140673927, -8.499999999999992895, 0.9166795111384334893 ) ) ;
#57410 = VERTEX_POINT ( 'NONE', #62160 ) ;
#57411 = CARTESIAN_POINT ( 'NONE',  ( -155.9049999999999727, 2.607480562269069324, -8.024999999999993250 ) ) ;
#57412 = ORIENTED_EDGE ( 'NONE', *, *, #24142, .T. ) ;
#57413 = CARTESIAN_POINT ( 'NONE',  ( -74.50000000000000000, 9.708372675170620525, -6.500000000000000000 ) ) ;
#57414 = DIRECTION ( 'NONE',  ( -0.000000000000000000, -1.000000000000000000, -0.000000000000000000 ) ) ;
#57415 = ORIENTED_EDGE ( 'NONE', *, *, #22559, .T. ) ;
#57416 = ADVANCED_FACE ( 'NONE', ( #51280 ), #36695, .F. ) ;
#57417 = AXIS2_PLACEMENT_3D ( 'NONE', #4321, #31778, #25806 ) ;
#57418 = FACE_OUTER_BOUND ( 'NONE', #27053, .T. ) ;
#57419 = CARTESIAN_POINT ( 'NONE',  ( 23.21231517720797655, 117.4999999999999716, -7.500000000000000000 ) ) ;
#57420 = CARTESIAN_POINT ( 'NONE',  ( 9.058813317711338797, 111.8449999999999847, -2.943386871421372675 ) ) ;
#57421 = EDGE_CURVE ( 'NONE', #51968, #57077, #17590, .T. ) ;
#57422 = ORIENTED_EDGE ( 'NONE', *, *, #63152, .F. ) ;
#57423 = CARTESIAN_POINT ( 'NONE',  ( -10.01517768586949408, 123.3049999999999784, -6.132527647946036459E-16 ) ) ;
#57424 = CIRCLE ( 'NONE', #27066, 0.2500000000000002220 ) ;
#57425 = CARTESIAN_POINT ( 'NONE',  ( -78.65499999999998693, -7.632228543268600340, -2.479861379858950166 ) ) ;
#57426 = DIRECTION ( 'NONE',  ( 1.000000000000000000, 0.000000000000000000, 0.000000000000000000 ) ) ;
#57427 = ORIENTED_EDGE ( 'NONE', *, *, #64505, .F. ) ;
#57428 = CARTESIAN_POINT ( 'NONE',  ( -8.102448949553181734, 138.6049999999999329, 5.886773742842747126 ) ) ;
#57429 = UNCERTAINTY_MEASURE_WITH_UNIT (LENGTH_MEASURE( 1.000000000000000082E-05 ), #66831, 'distance_accuracy_value', 'NONE');
#57430 = SURFACE_STYLE_FILL_AREA ( #8891 ) ;
#57431 = EDGE_CURVE ( 'NONE', #51630, #11647, #69119, .T. ) ;
#57432 = DIRECTION ( 'NONE',  ( 0.000000000000000000, 0.000000000000000000, 1.000000000000000000 ) ) ;
#57433 = MECHANICAL_DESIGN_GEOMETRIC_PRESENTATION_REPRESENTATION (  '', ( #30433 ), #45122 ) ;
#57434 = FILL_AREA_STYLE_COLOUR ( '', #2370 ) ;
#57435 = EDGE_CURVE ( 'NONE', #31294, #62143, #63814, .T. ) ;
#57436 = CIRCLE ( 'NONE', #27075, 0.5000000000000004441 ) ;
#57437 = EDGE_CURVE ( 'NONE', #68501, #65417, #10710, .T. ) ;
#57438 = LINE ( 'NONE', #46223, #19366 ) ;
#57439 = VERTEX_POINT ( 'NONE', #60278 ) ;
#57440 = FACE_OUTER_BOUND ( 'NONE', #37476, .T. ) ;
#57441 = CARTESIAN_POINT ( 'NONE',  ( -181.7050000000000125, 2.607480562269073321, 8.024999999999991473 ) ) ;
#57443 = ORIENTED_EDGE ( 'NONE', *, *, #39961, .T. ) ;
#57442 = PRESENTATION_LAYER_ASSIGNMENT (  '', '', ( #5740 ) ) ;
#57444 = CARTESIAN_POINT ( 'NONE',  ( 32.00000000000000000, 42.24290439782119932, 45.14575947096723496 ) ) ;
#57445 = CARTESIAN_POINT ( 'NONE',  ( -176.1570736234662036, -9.058813317711329915, -2.943386871421370898 ) ) ;
#57446 = EDGE_CURVE ( 'NONE', #62287, #1278, #50019, .T. ) ;
#57447 = DIRECTION ( 'NONE',  ( 0.000000000000000000, 0.000000000000000000, 1.000000000000000000 ) ) ;
#57448 = VERTEX_POINT ( 'NONE', #59215 ) ;
#57449 = CYLINDRICAL_SURFACE ( 'NONE', #32166, 0.2500000000000002220 ) ;
#57450 = AXIS2_PLACEMENT_3D ( 'NONE', #55037, #27606, #49124 ) ;
#57451 = ORIENTED_EDGE ( 'NONE', *, *, #42648, .T. ) ;
#57452 = CARTESIAN_POINT ( 'NONE',  ( -98.90500000000000114, 2.607480562269068880, -8.024999999999993250 ) ) ;
#57453 = EDGE_LOOP ( 'NONE', ( #68066, #30470, #43090, #59230 ) ) ;
#57454 = AXIS2_PLACEMENT_3D ( 'NONE', #23104, #14525, #61059 ) ;
#57455 = CARTESIAN_POINT ( 'NONE',  ( -136.4070736234661751, 3.094860106618428031, -9.524999999999993250 ) ) ;
#57456 =( NAMED_UNIT ( * ) SI_UNIT ( $, .STERADIAN. ) SOLID_ANGLE_UNIT ( ) );
#57457 = CARTESIAN_POINT ( 'NONE',  ( 71.49999999999998579, 64.07124727947029896, -7.500000000000000000 ) ) ;
#57458 = CARTESIAN_POINT ( 'NONE',  ( -74.15707362346617515, -9.058813317711329915, -2.943386871421370898 ) ) ;
#57459 = PRESENTATION_LAYER_ASSIGNMENT (  '', '', ( #39654 ) ) ;
#57460 = ORIENTED_EDGE ( 'NONE', *, *, #10027, .T. ) ;
#57461 = DIRECTION ( 'NONE',  ( -1.000000000000000000, 0.000000000000000000, -0.000000000000000000 ) ) ;
#57462 = CARTESIAN_POINT ( 'NONE',  ( -18.30189000360816465, -11.39540925085623968, 3.768464141822855495 ) ) ;
#57463 = CONICAL_SURFACE ( 'NONE', #34964, 8.524999999999977263, 0.7853981633974552734 ) ;
#57464 = SURFACE_STYLE_FILL_AREA ( #4304 ) ;
#57465 = CARTESIAN_POINT ( 'NONE',  ( -121.1050000000000040, -6.826472737025115478, 4.959722759717900331 ) ) ;
#57466 = CARTESIAN_POINT ( 'NONE',  ( -8.102448949553181734, 121.8949999999999818, -5.886773742842749790 ) ) ;
#57467 = CARTESIAN_POINT ( 'NONE',  ( -127.1949999999999932, 8.437984349512085203, -1.550032578732815448E-15 ) ) ;
#57468 =( NAMED_UNIT ( * ) SI_UNIT ( $, .STERADIAN. ) SOLID_ANGLE_UNIT ( ) );
#57469 = ORIENTED_EDGE ( 'NONE', *, *, #66827, .T. ) ;
#57470 = EDGE_CURVE ( 'NONE', #26721, #56578, #2900, .T. ) ;
#57471 = FACE_OUTER_BOUND ( 'NONE', #4280, .T. ) ;
#57472 = ORIENTED_EDGE ( 'NONE', *, *, #5019, .T. ) ;
#57474 = VECTOR ( 'NONE', #7622, 1000.000000000000000 ) ;
#57473 = DIRECTION ( 'NONE',  ( 1.000000000000000000, 0.000000000000000000, 0.000000000000000000 ) ) ;
#57475 = CARTESIAN_POINT ( 'NONE',  ( -167.6929263765338476, 10.01517768586948698, -1.839758294383808571E-15 ) ) ;
#57476 =( NAMED_UNIT ( * ) PLANE_ANGLE_UNIT ( ) SI_UNIT ( $, .RADIAN. ) );
#57477 = CARTESIAN_POINT ( 'NONE',  ( -181.4950000000000045, 6.826472737025113702, -4.959722759717902107 ) ) ;
#57478 = CIRCLE ( 'NONE', #67579, 5.500000000000005329 ) ;
#57479 = CARTESIAN_POINT ( 'NONE',  ( -44.99678646488361977, 9.646512454965742833, -3.411134130722746072 ) ) ;
#57480 = FACE_OUTER_BOUND ( 'NONE', #56011, .T. ) ;
#57481 = CARTESIAN_POINT ( 'NONE',  ( -15.00000000000000000, 8.000000000000000000, -4.000000000000000000 ) ) ;
#57482 = ORIENTED_EDGE ( 'NONE', *, *, #44257, .F. ) ;
#57483 = STYLED_ITEM ( 'NONE', ( #10883 ), #35444 ) ;
#57484 = CARTESIAN_POINT ( 'NONE',  ( -82.04292637653379927, -9.058813317711329915, -2.943386871421370898 ) ) ;
#57485 = CARTESIAN_POINT ( 'NONE',  ( -53.42422250819203100, -9.981287739266411663, -3.026606198070554754 ) ) ;
#57486 = CARTESIAN_POINT ( 'NONE',  ( -166.6429263765338078, -5.598654528085801552, 7.705886871421367523 ) ) ;
#57487 = PRESENTATION_LAYER_ASSIGNMENT (  '', '', ( #55212 ) ) ;
#57488 = FILL_AREA_STYLE_COLOUR ( '', #50567 ) ;
#57489 = SURFACE_STYLE_USAGE ( .BOTH. , #24763 ) ;
#57490 = FACE_OUTER_BOUND ( 'NONE', #69130, .T. ) ;
#57491 = CIRCLE ( 'NONE', #38470, 0.5000000000000004441 ) ;
#57492 = DIRECTION ( 'NONE',  ( 1.000000000000000000, 0.000000000000000000, 0.000000000000000000 ) ) ;
#57493 = EDGE_CURVE ( 'NONE', #10363, #8139, #66832, .T. ) ;
#57494 = VERTEX_POINT ( 'NONE', #44155 ) ;
#57495 = STYLED_ITEM ( 'NONE', ( #37437 ), #18292 ) ;
#57496 = CARTESIAN_POINT ( 'NONE',  ( 6.062177826491070398, 3.500000000000002665, 0.000000000000000000 ) ) ;
#57497 = DIRECTION ( 'NONE',  ( 0.000000000000000000, 1.000000000000000000, 0.000000000000000000 ) ) ;
#57498 = ORIENTED_EDGE ( 'NONE', *, *, #8498, .F. ) ;
#57499 = CARTESIAN_POINT ( 'NONE',  ( -103.0429263765337993, -9.058813317711329915, -2.943386871421370898 ) ) ;
#57500 = FACE_OUTER_BOUND ( 'NONE', #20769, .T. ) ;
#57501 = CARTESIAN_POINT ( 'NONE',  ( -4.716976649647098618, 134.2570736234661695, 6.492361379858953008 ) ) ;
#57502 = FACE_OUTER_BOUND ( 'NONE', #8281, .T. ) ;
#57503 = EDGE_CURVE ( 'NONE', #35999, #17121, #69453, .T. ) ;
#57504 =( BOUNDED_CURVE ( )  B_SPLINE_CURVE ( 2, ( #54739, #17163, #38981, #539, #21715, #16481, #862, #43908, #5502, #11850, #10481 ),
 .UNSPECIFIED., .F., .F. ) 
 B_SPLINE_CURVE_WITH_KNOTS ( ( 3, 2, 2, 2, 2, 3 ),
 ( 0.4999999999999881206, 0.5021739130434663689, 0.5043478260869445062, 0.5065217391304227545, 0.5086956521739008918, 0.5108695652173792512 ),
 .UNSPECIFIED. ) 
 CURVE ( )  GEOMETRIC_REPRESENTATION_ITEM ( )  RATIONAL_B_SPLINE_CURVE ( ( 1.000000000000267342, 0.9510565162948860785, 1.000000000000000000, 0.9510565162951535312, 1.000000000000000000, 0.9510565162951535312, 1.000000000000000000, 0.9510565162951535312, 1.000000000000000000, 0.9510565162954259799, 0.9999999999997275513 ) ) 
 REPRESENTATION_ITEM ( '' )  );
#57505 = AXIS2_PLACEMENT_3D ( 'NONE', #28424, #29490, #55535 ) ;
#57506 = EDGE_LOOP ( 'NONE', ( #8366, #58430, #6294, #55851 ) ) ;
#57507 = CARTESIAN_POINT ( 'NONE',  ( -104.0049999999999670, 6.826472737025115478, 4.959722759717899443 ) ) ;
#57508 = VECTOR ( 'NONE', #42005, 1000.000000000000000 ) ;
#57509 = ORIENTED_EDGE ( 'NONE', *, *, #17214, .T. ) ;
#57510 = DIRECTION ( 'NONE',  ( 0.000000000000000000, 0.000000000000000000, 1.000000000000000000 ) ) ;
#57511 = PRESENTATION_STYLE_ASSIGNMENT (( #47004 ) ) ;
#57512 = DIRECTION ( 'NONE',  ( 0.000000000000000000, 0.000000000000000000, -1.000000000000000000 ) ) ;
#57513 = CARTESIAN_POINT ( 'NONE',  ( 44.99999999999998579, 119.9999999999999716, 7.000000000000000000 ) ) ;
#57514 = EDGE_CURVE ( 'NONE', #26708, #65395, #45668, .T. ) ;
#57515 = VERTEX_POINT ( 'NONE', #48735 ) ;
#57516 = CARTESIAN_POINT ( 'NONE',  ( 7.766391886667110889, 0.5482146608018589884, 0.7663918866669823249 ) ) ;
#57517 = CARTESIAN_POINT ( 'NONE',  ( -68.39499999999999602, -6.826472737025115478, -4.959722759717899443 ) ) ;
#57518 = VERTEX_POINT ( 'NONE', #439 ) ;
#57519 = MECHANICAL_DESIGN_GEOMETRIC_PRESENTATION_REPRESENTATION (  '', ( #54140 ), #58668 ) ;
#57520 =( LENGTH_UNIT ( ) NAMED_UNIT ( * ) SI_UNIT ( .MILLI., .METRE. ) );
#57521 = SURFACE_STYLE_USAGE ( .BOTH. , #56472 ) ;
#57522 = EDGE_CURVE ( 'NONE', #61983, #11976, #27884, .T. ) ;
#57523 = VERTEX_POINT ( 'NONE', #43474 ) ;
#57524 = DIRECTION ( 'NONE',  ( -0.000000000000000000, -1.000000000000000000, -0.000000000000000000 ) ) ;
#57525 = CARTESIAN_POINT ( 'NONE',  ( -195.0000000000000000, 0.000000000000000000, 0.000000000000000000 ) ) ;
#57526 = SURFACE_SIDE_STYLE ('',( #50864 ) ) ;
#57527 = FILL_AREA_STYLE ('',( #36466 ) ) ;
#57528 = VERTEX_POINT ( 'NONE', #21967 ) ;
#57529 = PRESENTATION_LAYER_ASSIGNMENT (  '', '', ( #19303 ) ) ;
#57530 = DIRECTION ( 'NONE',  ( 0.000000000000000000, 0.000000000000000000, -1.000000000000000000 ) ) ;
#57531 = ORIENTED_EDGE ( 'NONE', *, *, #24751, .F. ) ;
#57532 = SURFACE_SIDE_STYLE ('',( #24803 ) ) ;
#57533 = DIRECTION ( 'NONE',  ( 0.8753987966739757987, 0.000000000000000000, -0.4834014344018390252 ) ) ;
#57534 = CARTESIAN_POINT ( 'NONE',  ( -40.82991390394946762, 108.1252238755516828, 3.311222316328668036 ) ) ;
#57535 = CARTESIAN_POINT ( 'NONE',  ( -167.6070736234661638, -8.102448949553172852, 5.886773742842742685 ) ) ;
#57536 = AXIS2_PLACEMENT_3D ( 'NONE', #33212, #23007, #51130 ) ;
#57537 = CARTESIAN_POINT ( 'NONE',  ( -9.058813317711337021, 119.0449999999999875, -2.943386871421374895 ) ) ;
#57538 = CARTESIAN_POINT ( 'NONE',  ( -100.5570736234661808, -1.166476076187852838E-15, -9.524999999999991473 ) ) ;
#57539 = PRESENTATION_LAYER_ASSIGNMENT (  '', '', ( #48599 ) ) ;
#57540 = FILL_AREA_STYLE ('',( #20240 ) ) ;
#57541 = FACE_OUTER_BOUND ( 'NONE', #8977, .T. ) ;
#57542 = EDGE_LOOP ( 'NONE', ( #6516, #253, #37103, #67847 ) ) ;
#57543 = CARTESIAN_POINT ( 'NONE',  ( -106.1070736234661638, 8.102448949553172852, -5.886773742842744461 ) ) ;
#57544 = DIRECTION ( 'NONE',  ( -1.000000000000000000, -0.000000000000000000, -0.000000000000000000 ) ) ;
#57545 = DIRECTION ( 'NONE',  ( 1.000000000000000000, 0.000000000000000000, 0.000000000000000000 ) ) ;
#57546 = CARTESIAN_POINT ( 'NONE',  ( -148.5550000000000068, 0.000000000000000000, 8.024999999999991473 ) ) ;
#57547 = CARTESIAN_POINT ( 'NONE',  ( 72.49999999999998579, 64.07124727947029896, -9.500000000000000000 ) ) ;
#57548 = CARTESIAN_POINT ( 'NONE',  ( -8.468615938765699624, 111.5588028509683198, -0.3477567820242795649 ) ) ;
#57549 = CIRCLE ( 'NONE', #66544, 18.50000000000000355 ) ;
#57550 = CARTESIAN_POINT ( 'NONE',  ( -153.1450000000000102, -4.716976649647092401, 6.492361379858946790 ) ) ;
#57551 = CARTESIAN_POINT ( 'NONE',  ( -144.8949999999999818, 6.826472737025115478, 4.959722759717899443 ) ) ;
#57552 = ORIENTED_EDGE ( 'NONE', *, *, #21781, .T. ) ;
#57553 = EDGE_CURVE ( 'NONE', #20590, #6919, #27249, .T. ) ;
#57554 = CARTESIAN_POINT ( 'NONE',  ( -181.2570736234661979, 5.598654528085800663, -7.705886871421367523 ) ) ;
#57555 = STYLED_ITEM ( 'NONE', ( #22670 ), #25491 ) ;
#57556 = SURFACE_STYLE_USAGE ( .BOTH. , #14652 ) ;
#57557 = DIRECTION ( 'NONE',  ( -1.000000000000000000, 0.000000000000000000, 0.000000000000000000 ) ) ;
#57558 = CARTESIAN_POINT ( 'NONE',  ( -59.45499999999997698, 7.632228543268599452, -2.479861379858951942 ) ) ;
#57559 = CIRCLE ( 'NONE', #36136, 14.00000000000000533 ) ;
#57560 = CARTESIAN_POINT ( 'NONE',  ( -153.5070736234661979, 8.102448949553176405, 5.886773742842740909 ) ) ;
#57561 = CARTESIAN_POINT ( 'NONE',  ( -64.04499999999998749, 7.632228543268600340, 2.479861379858949277 ) ) ;
#57562 = CARTESIAN_POINT ( 'NONE',  ( -8.102448949553181734, 153.0050000000000239, -5.886773742842749790 ) ) ;
#57563 = CARTESIAN_POINT ( 'NONE',  ( 57.74999999999998579, 30.74999999999999289, -3.750000000000000000 ) ) ;
#57564 = AXIS2_PLACEMENT_3D ( 'NONE', #43273, #26999, #59043 ) ;
#57565 = DIRECTION ( 'NONE',  ( -0.000000000000000000, -1.000000000000000000, -0.000000000000000000 ) ) ;
#57566 =( NAMED_UNIT ( * ) SI_UNIT ( $, .STERADIAN. ) SOLID_ANGLE_UNIT ( ) );
#57567 = VECTOR ( 'NONE', #49224, 1000.000000000000000 ) ;
#57568 = ADVANCED_FACE ( 'NONE', ( #6121 ), #32024, .T. ) ;
#57569 = LINE ( 'NONE', #45671, #35918 ) ;
#57570 = CARTESIAN_POINT ( 'NONE',  ( -178.6429263765338078, -5.598654528085801552, 7.705886871421367523 ) ) ;
#57571 = ADVANCED_FACE ( 'NONE', ( #1112 ), #53288, .F. ) ;
#57572 = PRESENTATION_STYLE_ASSIGNMENT (( #4416 ) ) ;
#57573 = EDGE_CURVE ( 'NONE', #65761, #45031, #51128, .T. ) ;
#57574 = PRESENTATION_LAYER_ASSIGNMENT (  '', '', ( #38551 ) ) ;
#57575 = CARTESIAN_POINT ( 'NONE',  ( -34.99999999999992895, 112.9999999999999858, 9.500000000000000000 ) ) ;
#57576 = ORIENTED_EDGE ( 'NONE', *, *, #49886, .T. ) ;
#57577 = ORIENTED_EDGE ( 'NONE', *, *, #60947, .F. ) ;
#57578 =( NAMED_UNIT ( * ) PLANE_ANGLE_UNIT ( ) SI_UNIT ( $, .RADIAN. ) );
#57579 = PRESENTATION_LAYER_ASSIGNMENT (  '', '', ( #10442 ) ) ;
#57580 = DIRECTION ( 'NONE',  ( 1.000000000000000000, 0.000000000000000000, 0.000000000000000000 ) ) ;
#57581 = VECTOR ( 'NONE', #12012, 1000.000000000000000 ) ;
#57582 = EDGE_CURVE ( 'NONE', #10638, #43189, #63602, .T. ) ;
#57583 = CARTESIAN_POINT ( 'NONE',  ( -20.99026508940074010, 114.7786387612191703, 10.00000000000000000 ) ) ;
#57584 = CARTESIAN_POINT ( 'NONE',  ( 22.70977904271739334, 24.88203576750890988, -27.31717988970180500 ) ) ;
#57585 = CARTESIAN_POINT ( 'NONE',  ( -76.55707362346616662, -1.166476076187852838E-15, -9.524999999999991473 ) ) ;
#57586 = ADVANCED_FACE ( 'NONE', ( #2522 ), #24279, .F. ) ;
#57587 = EDGE_LOOP ( 'NONE', ( #29336, #47964, #69123, #30416 ) ) ;
#57588 = ORIENTED_EDGE ( 'NONE', *, *, #26363, .F. ) ;
#57589 = AXIS2_PLACEMENT_3D ( 'NONE', #48470, #49149, #17814 ) ;
#57590 = DIRECTION ( 'NONE',  ( -0.000000000000000000, -0.000000000000000000, 1.000000000000000000 ) ) ;
#57591 = FILL_AREA_STYLE_COLOUR ( '', #32001 ) ;
#57592 = CIRCLE ( 'NONE', #67735, 5.000000000000000888 ) ;
#57593 = ORIENTED_EDGE ( 'NONE', *, *, #9785, .F. ) ;
#57594 = CARTESIAN_POINT ( 'NONE',  ( -3.094860106618434248, 114.9049999999999727, 9.525000000000000355 ) ) ;
#57595 = DIRECTION ( 'NONE',  ( 1.000000000000000000, -0.000000000000000000, 0.000000000000000000 ) ) ;
#57596 = CARTESIAN_POINT ( 'NONE',  ( 71.50000000000000000, 35.92875272052971525, -7.500000000000000000 ) ) ;
#57597 = CONICAL_SURFACE ( 'NONE', #56433, 5.499999999999976907, 0.7853981633974309595 ) ;
#57598 = EDGE_CURVE ( 'NONE', #9072, #1577, #63452, .T. ) ;
#57599 = CARTESIAN_POINT ( 'NONE',  ( -111.7449999999999903, 4.716976649647094177, 6.492361379858945902 ) ) ;
#57600 = VERTEX_POINT ( 'NONE', #18063 ) ;
#57601 = VECTOR ( 'NONE', #63684, 1000.000000000000000 ) ;
#57602 = PRESENTATION_STYLE_ASSIGNMENT (( #19948 ) ) ;
#57603 = SURFACE_SIDE_STYLE ('',( #42177 ) ) ;
#57604 = DIRECTION ( 'NONE',  ( -1.000000000000000000, 0.000000000000000000, 0.000000000000000000 ) ) ;
#57605 = ORIENTED_EDGE ( 'NONE', *, *, #62353, .F. ) ;
#57606 = CARTESIAN_POINT ( 'NONE',  ( 6.826472737025119919, 154.8929263765338362, 4.959722759717908325 ) ) ;
#57607 = PRESENTATION_LAYER_ASSIGNMENT (  '', '', ( #22764 ) ) ;
#57608 = SURFACE_STYLE_FILL_AREA ( #21011 ) ;
#57609 = FILL_AREA_STYLE ('',( #3035 ) ) ;
#57610 = ORIENTED_EDGE ( 'NONE', *, *, #46555, .T. ) ;
#57611 = CARTESIAN_POINT ( 'NONE',  ( 19.89974874213240597, 115.4999999999999574, -10.00000000000000000 ) ) ;
#57612 = ORIENTED_EDGE ( 'NONE', *, *, #51155, .T. ) ;
#57613 = CARTESIAN_POINT ( 'NONE',  ( 20.04013953308945162, 115.4999999999999432, 10.00000000000000000 ) ) ;
#57614 = CARTESIAN_POINT ( 'NONE',  ( -4.041451884327381450, -7.000000000000002665, 7.500000000000000000 ) ) ;
#57615 = CARTESIAN_POINT ( 'NONE',  ( -60.00000000000000000, -2.024042244987997205E-14, -6.000000000000000000 ) ) ;
#57616 = FACE_OUTER_BOUND ( 'NONE', #59206, .T. ) ;
#57618 = CARTESIAN_POINT ( 'NONE',  ( -122.0049999999999670, 6.826472737025116366, 4.959722759717898555 ) ) ;
#57617 = COLOUR_RGB ( '', 0.08235294, 0.09019608, 0.10196078) ;
#57619 = CARTESIAN_POINT ( 'NONE',  ( -24.21231517720798010, 113.4999999999999858, -7.500000000000000000 ) ) ;
#57620 = EDGE_CURVE ( 'NONE', #320, #6729, #34242, .T. ) ;
#57621 = CYLINDRICAL_SURFACE ( 'NONE', #55226, 0.2500000000000002220 ) ;
#57622 = DIRECTION ( 'NONE',  ( -0.000000000000000000, -1.000000000000000000, -0.000000000000000000 ) ) ;
#57623 = CIRCLE ( 'NONE', #28405, 0.5000000000000004441 ) ;
#57624 = CARTESIAN_POINT ( 'NONE',  ( -74.50000000000000000, 7.768687147774684831, 6.500000000000000000 ) ) ;
#57625 = CYLINDRICAL_SURFACE ( 'NONE', #19316, 0.5000000000000004441 ) ;
#57626 = CARTESIAN_POINT ( 'NONE',  ( 35.99999999999999289, 0.000000000000000000, -72.00402776293825013 ) ) ;
#57627 = ORIENTED_EDGE ( 'NONE', *, *, #59481, .T. ) ;
#57628 = ORIENTED_EDGE ( 'NONE', *, *, #41423, .F. ) ;
#57629 = FACE_OUTER_BOUND ( 'NONE', #9199, .T. ) ;
#57630 = CARTESIAN_POINT ( 'NONE',  ( 61.74999999999998579, 30.74999999999999289, -4.000000000000000000 ) ) ;
#57631 = CARTESIAN_POINT ( 'NONE',  ( 10.39230484541326582, 2.500000000000000000, 0.000000000000000000 ) ) ;
#57632 = ORIENTED_EDGE ( 'NONE', *, *, #4264, .T. ) ;
#57633 = CARTESIAN_POINT ( 'NONE',  ( 62.24999999999998579, 31.24999999999999289, -4.000000000000000000 ) ) ;
#57634 = CARTESIAN_POINT ( 'NONE',  ( -177.0549999999999784, -9.827790563157499189E-16, -8.024999999999991473 ) ) ;
#57635 =( GEOMETRIC_REPRESENTATION_CONTEXT ( 3 ) GLOBAL_UNCERTAINTY_ASSIGNED_CONTEXT ( ( #12412 ) ) GLOBAL_UNIT_ASSIGNED_CONTEXT ( ( #24972, #57330, #58369 ) ) REPRESENTATION_CONTEXT ( 'NONE', 'WORKASPACE' ) );
#57636 = FILL_AREA_STYLE ('',( #46792 ) ) ;
#57637 = CARTESIAN_POINT ( 'NONE',  ( -49.10707362346617089, 8.102448949553171076, -5.886773742842744461 ) ) ;
#57638 = CARTESIAN_POINT ( 'NONE',  ( -174.7449999999999761, 4.716976649647094177, 6.492361379858945902 ) ) ;
#57639 = CARTESIAN_POINT ( 'NONE',  ( 3.749999999999999556, 34.24999999999998579, 3.750000000000000000 ) ) ;
#57640 = ORIENTED_EDGE ( 'NONE', *, *, #10492, .F. ) ;
#57641 = AXIS2_PLACEMENT_3D ( 'NONE', #18242, #22840, #54812 ) ;
#57642 = FILL_AREA_STYLE ('',( #30530 ) ) ;
#57643 = CARTESIAN_POINT ( 'NONE',  ( -88.25499999999998124, -4.716976649647092401, 6.492361379858946790 ) ) ;
#57644 = CARTESIAN_POINT ( 'NONE',  ( 9.270114131632642085, 154.5000000000000284, -2.232057404141062573 ) ) ;
#57645 = DIRECTION ( 'NONE',  ( 0.000000000000000000, 0.000000000000000000, -1.000000000000000000 ) ) ;
#57646 = SURFACE_STYLE_FILL_AREA ( #9472 ) ;
#57647 = VECTOR ( 'NONE', #34837, 1000.000000000000000 ) ;
#57648 = PRESENTATION_LAYER_ASSIGNMENT (  '', '', ( #18342 ) ) ;
#57649 = CARTESIAN_POINT ( 'NONE',  ( -86.24499999999999034, -4.716976649647093289, -6.492361379858945902 ) ) ;
#57650 = CARTESIAN_POINT ( 'NONE',  ( -1.166476076187854022E-15, 124.0549999999999784, 9.525000000000000355 ) ) ;
#57651 = CARTESIAN_POINT ( 'NONE',  ( -64.34499999999998465, 7.632228543268599452, -2.479861379858951942 ) ) ;
#57652 = VECTOR ( 'NONE', #39235, 1000.000000000000000 ) ;
#57653 = CARTESIAN_POINT ( 'NONE',  ( 20.40217977176331843, 114.8427411095148329, -10.33293932795019465 ) ) ;
#57654 = DIRECTION ( 'NONE',  ( 0.000000000000000000, 0.000000000000000000, 1.000000000000000000 ) ) ;
#57655 = DIRECTION ( 'NONE',  ( -1.000000000000000000, 0.000000000000000000, 0.000000000000000000 ) ) ;
#57656 =( GEOMETRIC_REPRESENTATION_CONTEXT ( 3 ) GLOBAL_UNCERTAINTY_ASSIGNED_CONTEXT ( ( #25750 ) ) GLOBAL_UNIT_ASSIGNED_CONTEXT ( ( #56227, #7697, #1687 ) ) REPRESENTATION_CONTEXT ( 'NONE', 'WORKASPACE' ) );
#57657 = FACE_OUTER_BOUND ( 'NONE', #26269, .T. ) ;
#57658 = SPHERICAL_SURFACE ( 'NONE', #46159, 0.5000000000000000000 ) ;
#57659 = VERTEX_POINT ( 'NONE', #50422 ) ;
#57660 = EDGE_CURVE ( 'NONE', #2398, #45832, #1474, .T. ) ;
#57661 = CARTESIAN_POINT ( 'NONE',  ( -108.7429263765338021, -5.598654528085803328, -7.705886871421366635 ) ) ;
#57662 = CARTESIAN_POINT ( 'NONE',  ( -129.2949999999999875, -2.607480562269069768, 8.024999999999991473 ) ) ;
#57663 = EDGE_CURVE ( 'NONE', #52777, #40754, #66599, .T. ) ;
#57665 = FACE_OUTER_BOUND ( 'NONE', #50587, .T. ) ;
#57664 = CARTESIAN_POINT ( 'NONE',  ( -25.00000000000000000, 1.000000000000000000, -4.000000000000000000 ) ) ;
#57666 = FACE_OUTER_BOUND ( 'NONE', #22330, .T. ) ;
#57667 = ORIENTED_EDGE ( 'NONE', *, *, #21374, .F. ) ;
#57669 = ORIENTED_EDGE ( 'NONE', *, *, #42075, .F. ) ;
#57668 = AXIS2_PLACEMENT_3D ( 'NONE', #64680, #49541, #11893 ) ;
#57670 = SURFACE_STYLE_FILL_AREA ( #15810 ) ;
#57671 = CARTESIAN_POINT ( 'NONE',  ( 16.75000000000000711, 25.24999999999998224, 3.750000000000000000 ) ) ;
#57672 = APPLICATION_CONTEXT ( 'automotive_design' ) ;
#57673 = COLOUR_RGB ( '', 0.72549020, 0.75294118, 0.79215686) ;
#57674 = FILL_AREA_STYLE ('',( #36249 ) ) ;
#57675 = CARTESIAN_POINT ( 'NONE',  ( -41.84210526315788314, 107.2928455055531600, -4.000000000000000000 ) ) ;
#57676 = DIRECTION ( 'NONE',  ( -1.000000000000000000, -0.000000000000000000, -0.000000000000000000 ) ) ;
#57677 = ADVANCED_FACE ( 'NONE', ( #67292 ), #55697, .F. ) ;
#57678 = ORIENTED_EDGE ( 'NONE', *, *, #53199, .T. ) ;
#57679 = CARTESIAN_POINT ( 'NONE',  ( -126.2049999999999841, -2.607480562269071545, -8.024999999999991473 ) ) ;
#57680 = VERTEX_POINT ( 'NONE', #24029 ) ;
#57681 = LINE ( 'NONE', #8103, #19589 ) ;
#57682 = CARTESIAN_POINT ( 'NONE',  ( -120.8070736234661666, 10.01517768586948698, -1.839758294383808571E-15 ) ) ;
#57683 = AXIS2_PLACEMENT_3D ( 'NONE', #14577, #18803, #13520 ) ;
#57684 = VERTEX_POINT ( 'NONE', #60598 ) ;
#57685 =( LENGTH_UNIT ( ) NAMED_UNIT ( * ) SI_UNIT ( .MILLI., .METRE. ) );
#57686 = CARTESIAN_POINT ( 'NONE',  ( 48.50000000000000000, 14.49137674618942562, 9.500000000000000000 ) ) ;
#57687 = EDGE_LOOP ( 'NONE', ( #14493, #46915, #9726, #45634 ) ) ;
#57688 = STYLED_ITEM ( 'NONE', ( #55532 ), #36502 ) ;
#57689 = DIRECTION ( 'NONE',  ( 1.000000000000000000, 0.000000000000000000, 0.000000000000000000 ) ) ;
#57690 = CARTESIAN_POINT ( 'NONE',  ( 5.598654528085809545, 148.1450000000000102, -7.705886871421373741 ) ) ;
#57691 = CONICAL_SURFACE ( 'NONE', #20627, 7.000000000000000888, 0.7853981633974500554 ) ;
#57692 = ORIENTED_EDGE ( 'NONE', *, *, #28505, .F. ) ;
#57693 = CARTESIAN_POINT ( 'NONE',  ( 8.102448949553179958, 145.5049999999999670, 5.886773742842750679 ) ) ;
#57694 = FACE_OUTER_BOUND ( 'NONE', #15590, .T. ) ;
#57695 = FILL_AREA_STYLE_COLOUR ( '', #68910 ) ;
#57696 = VECTOR ( 'NONE', #22113, 1000.000000000000000 ) ;
#57697 = VERTEX_POINT ( 'NONE', #18417 ) ;
#57698 = CARTESIAN_POINT ( 'NONE',  ( 8.437984349512095861, 125.1929263765338192, 1.550032578732817026E-15 ) ) ;
#57699 = CARTESIAN_POINT ( 'NONE',  ( 45.00000000000000000, 10.00000000017111468, 6.065867531378962063 ) ) ;
#57700 = CIRCLE ( 'NONE', #16199, 16.00000000000000000 ) ;
#57701 = VECTOR ( 'NONE', #18875, 1000.000000000000000 ) ;
#57702 = SPHERICAL_SURFACE ( 'NONE', #63541, 0.2500000000000000000 ) ;
#57703 = EDGE_CURVE ( 'NONE', #62431, #13981, #44605, .T. ) ;
#57704 = VERTEX_POINT ( 'NONE', #23332 ) ;
#57705 = CARTESIAN_POINT ( 'NONE',  ( 41.00754902350322340, 107.7352920524769502, 3.098114188008662673 ) ) ;
#57706 = ORIENTED_EDGE ( 'NONE', *, *, #7480, .T. ) ;
#57707 = CARTESIAN_POINT ( 'NONE',  ( -62.54292637653379927, 9.058813317711329915, 2.943386871421369566 ) ) ;
#57708 = DIRECTION ( 'NONE',  ( 0.000000000000000000, 1.000000000000000000, -0.000000000000000000 ) ) ;
#57709 = SURFACE_STYLE_USAGE ( .BOTH. , #62962 ) ;
#57710 = CARTESIAN_POINT ( 'NONE',  ( -149.1549999999999727, 7.632228543268600340, 2.479861379858949277 ) ) ;
#57711 = VERTEX_POINT ( 'NONE', #52529 ) ;
#57712 = ADVANCED_FACE ( 'NONE', ( #62683 ), #53369, .F. ) ;
#57713 = DIRECTION ( 'NONE',  ( 0.000000000000000000, -1.000000000000000000, 0.000000000000000000 ) ) ;
#57714 =( BOUNDED_CURVE ( )  B_SPLINE_CURVE ( 2, ( #60915, #3167, #55656, #13421, #46177, #34889, #51086, #24657, #66193, #18717, #45501 ),
 .UNSPECIFIED., .F., .F. ) 
 B_SPLINE_CURVE_WITH_KNOTS ( ( 3, 2, 2, 2, 2, 3 ),
 ( 0.6195652173912897798, 0.6217391304347680281, 0.6239130434782461654, 0.6260869565217245247, 0.6282608695652026620, 0.6304347826086809103 ),
 .UNSPECIFIED. ) 
 CURVE ( )  GEOMETRIC_REPRESENTATION_ITEM ( )  RATIONAL_B_SPLINE_CURVE ( ( 1.000000000000327516, 0.9510565162948261264, 1.000000000000000000, 0.9510565162951535312, 1.000000000000000000, 0.9510565162951535312, 1.000000000000000000, 0.9510565162951535312, 1.000000000000000000, 0.9510565162954859320, 0.9999999999996675992 ) ) 
 REPRESENTATION_ITEM ( '' )  );
#57715 = CARTESIAN_POINT ( 'NONE',  ( 0.000000000000000000, 111.9999999999999858, -8.025000000000000355 ) ) ;
#57716 = CARTESIAN_POINT ( 'NONE',  ( -17.75000000000000711, 30.99999999999999289, -3.750000000000000000 ) ) ;
#57717 = CARTESIAN_POINT ( 'NONE',  ( 16.75000000000000711, 27.74999999999998224, -4.000000000000000000 ) ) ;
#57718 = CARTESIAN_POINT ( 'NONE',  ( -34.99999999999992895, 113.4999999999999858, -7.000000000000000000 ) ) ;
#57719 = ORIENTED_EDGE ( 'NONE', *, *, #46446, .T. ) ;
#57720 = ORIENTED_EDGE ( 'NONE', *, *, #16967, .F. ) ;
#57721 = CARTESIAN_POINT ( 'NONE',  ( 8.000000000000035527, 0.000000000000000000, -77.00402776293825013 ) ) ;
#57722 = DIRECTION ( 'NONE',  ( -0.7071067811865451302, 8.659560562354903276E-17, 0.7071067811865500152 ) ) ;
#57724 = CARTESIAN_POINT ( 'NONE',  ( -69.20499999999998408, -2.607480562269071545, -8.024999999999991473 ) ) ;
#57723 = VECTOR ( 'NONE', #3679, 1000.000000000000000 ) ;
#57725 = ORIENTED_EDGE ( 'NONE', *, *, #25475, .F. ) ;
#57726 = CARTESIAN_POINT ( 'NONE',  ( -48.00000000000000000, 99.99999999999992895, 9.500000000000000000 ) ) ;
#57727 = DIRECTION ( 'NONE',  ( -0.000000000000000000, -1.000000000000000000, 0.000000000000000000 ) ) ;
#57728 = B_SPLINE_CURVE_WITH_KNOTS ( 'NONE', 3,
 ( #19262, #7676, #3760, #51644, #29112, #3400, #62530, #24893, #56208, #50954 ),
 .UNSPECIFIED., .F., .F.,
 ( 4, 2, 2, 2, 4 ),
 ( 0.000000000000000000, 0.0002942714429691380704, 0.0005885428859382761408, 0.0008828143289074142112, 0.001177085771876552282 ),
 .UNSPECIFIED. ) ;
#57729 = STYLED_ITEM ( 'NONE', ( #18878 ), #48321 ) ;
#57730 = AXIS2_PLACEMENT_3D ( 'NONE', #55846, #56531, #50926 ) ;
#57731 = CARTESIAN_POINT ( 'NONE',  ( -90.50707362346618368, 8.102448949553176405, 5.886773742842740909 ) ) ;
#57732 = DIRECTION ( 'NONE',  ( -0.000000000000000000, -1.000000000000000000, -0.000000000000000000 ) ) ;
#57733 = VERTEX_POINT ( 'NONE', #51822 ) ;
#57734 =( GEOMETRIC_REPRESENTATION_CONTEXT ( 3 ) GLOBAL_UNCERTAINTY_ASSIGNED_CONTEXT ( ( #42464 ) ) GLOBAL_UNIT_ASSIGNED_CONTEXT ( ( #39838, #52111, #19369 ) ) REPRESENTATION_CONTEXT ( 'NONE', 'WORKASPACE' ) );
#57735 =( LENGTH_UNIT ( ) NAMED_UNIT ( * ) SI_UNIT ( .MILLI., .METRE. ) );
#57736 = CARTESIAN_POINT ( 'NONE',  ( 0.000000000000000000, 0.000000000000000000, 0.000000000000000000 ) ) ;
#57737 = DIRECTION ( 'NONE',  ( 0.000000000000000000, 0.000000000000000000, 1.000000000000000000 ) ) ;
#57738 = AXIS2_PLACEMENT_3D ( 'NONE', #69685, #42327, #15228 ) ;
#57739 = CARTESIAN_POINT ( 'NONE',  ( 3.094860106618435136, 148.2949999999999307, -9.525000000000000355 ) ) ;
#57740 = CARTESIAN_POINT ( 'NONE',  ( -93.59499999999997044, 2.607480562269073321, 8.024999999999991473 ) ) ;
#57741 = EDGE_CURVE ( 'NONE', #27592, #16561, #64145, .T. ) ;
#57742 = DIRECTION ( 'NONE',  ( -0.000000000000000000, 0.3420201433256630508, 0.9396926207859105373 ) ) ;
#57743 = AXIS2_PLACEMENT_3D ( 'NONE', #27301, #16806, #38280 ) ;
#57744 = CARTESIAN_POINT ( 'NONE',  ( 11.00000000000001599, 42.74314482547740113, 27.71473342867655987 ) ) ;
#57745 = CARTESIAN_POINT ( 'NONE',  ( -41.25890975875731215, 107.3519676386824671, -3.442113426143909027 ) ) ;
#57746 = ORIENTED_EDGE ( 'NONE', *, *, #46261, .F. ) ;
#57747 = CARTESIAN_POINT ( 'NONE',  ( -136.0429263765338135, -9.058813317711329915, -2.943386871421370898 ) ) ;
#57748 = AXIS2_PLACEMENT_3D ( 'NONE', #29246, #65245, #50728 ) ;
#57749 =( NAMED_UNIT ( * ) PLANE_ANGLE_UNIT ( ) SI_UNIT ( $, .RADIAN. ) );
#57750 = CARTESIAN_POINT ( 'NONE',  ( -33.26911838175604430, -9.395153070120809247, -2.525443329778700008 ) ) ;
#57751 = CARTESIAN_POINT ( 'NONE',  ( -154.3449999999999704, 7.632228543268599452, -2.479861379858951942 ) ) ;
#57752 = SURFACE_SIDE_STYLE ('',( #56432 ) ) ;
#57753 = STYLED_ITEM ( 'NONE', ( #8543 ), #30249 ) ;
#57754 = EDGE_CURVE ( 'NONE', #3926, #14977, #14511, .T. ) ;
#57755 = DIRECTION ( 'NONE',  ( -1.000000000000000000, 0.000000000000000000, 0.000000000000000000 ) ) ;
#57756 = CARTESIAN_POINT ( 'NONE',  ( -63.05707362346617373, 0.000000000000000000, 9.524999999999991473 ) ) ;
#57757 = CARTESIAN_POINT ( 'NONE',  ( 26.00000000000001776, 15.00000000000000000, -29.68999999999999417 ) ) ;
#57758 = ORIENTED_EDGE ( 'NONE', *, *, #1638, .F. ) ;
#57759 = CARTESIAN_POINT ( 'NONE',  ( 15.98999599679679839, 146.4999999999999716, -7.000000000000000000 ) ) ;
#57761 = ORIENTED_EDGE ( 'NONE', *, *, #60487, .F. ) ;
#57760 = COLOUR_RGB ( '', 0.09019608, 0.27058824, 0.51372549) ;
#57762 = EDGE_CURVE ( 'NONE', #57325, #61698, #10681, .T. ) ;
#57763 = CARTESIAN_POINT ( 'NONE',  ( 5.705565085145809512, -2.472216779103305395, 4.117671386636410524 ) ) ;
#57764 = COLOUR_RGB ( '', 0.72549020, 0.75294118, 0.79215686) ;
#57765 = AXIS2_PLACEMENT_3D ( 'NONE', #8223, #28938, #25086 ) ;
#57766 = DIRECTION ( 'NONE',  ( 0.000000000000000000, 0.000000000000000000, -1.000000000000000000 ) ) ;
#57767 = CARTESIAN_POINT ( 'NONE',  ( -44.99999999999964473, 8.706976341191598578, 5.725845108613464518 ) ) ;
#57768 = CARTESIAN_POINT ( 'NONE',  ( 57.00000000000000000, 0.000000000000000000, 79.00402776293826435 ) ) ;
#57769 = EDGE_CURVE ( 'NONE', #33888, #50928, #50062, .T. ) ;
#57770 = ORIENTED_EDGE ( 'NONE', *, *, #8587, .T. ) ;
#57771 = CARTESIAN_POINT ( 'NONE',  ( -153.5049999999999670, -6.826472737025113702, -4.959722759717900331 ) ) ;
#57772 = CIRCLE ( 'NONE', #33004, 1.000000000000000000 ) ;
#57773 = EDGE_LOOP ( 'NONE', ( #14119, #14243, #25465, #9942 ) ) ;
#57774 = LINE ( 'NONE', #20829, #26776 ) ;
#57775 = FACE_OUTER_BOUND ( 'NONE', #23174, .T. ) ;
#57776 = EDGE_LOOP ( 'NONE', ( #18851, #41833, #62624, #30658 ) ) ;
#57777 = CIRCLE ( 'NONE', #27412, 0.5000000000000004441 ) ;
#57778 = DIRECTION ( 'NONE',  ( 0.000000000000000000, 0.000000000000000000, -1.000000000000000000 ) ) ;
#57779 = CARTESIAN_POINT ( 'NONE',  ( 62.24999999999998579, 0.000000000000000000, 3.750000000000000000 ) ) ;
#57780 = CARTESIAN_POINT ( 'NONE',  ( 5.598654528085805993, 117.2449999999999903, 7.705886871421374629 ) ) ;
#57781 = EDGE_LOOP ( 'NONE', ( #47615, #24187, #33515, #1059 ) ) ;
#57782 = CARTESIAN_POINT ( 'NONE',  ( -57.74292637653380211, -5.598654528085803328, -7.705886871421366635 ) ) ;
#57783 = CARTESIAN_POINT ( 'NONE',  ( 5.598654528085809545, 125.2549999999999812, -7.705886871421373741 ) ) ;
#57784 = CARTESIAN_POINT ( 'NONE',  ( -74.00499999999996703, 6.826472737025115478, 4.959722759717899443 ) ) ;
#57785 = LINE ( 'NONE', #51453, #37511 ) ;
#57786 = ORIENTED_EDGE ( 'NONE', *, *, #9237, .F. ) ;
#57787 = CARTESIAN_POINT ( 'NONE',  ( -9.058813317711337021, 135.1550000000000011, -2.943386871421374895 ) ) ;
#57788 = CARTESIAN_POINT ( 'NONE',  ( -13.75000000000000533, 30.99999999999999289, -3.750000000000000000 ) ) ;
#57789 = CARTESIAN_POINT ( 'NONE',  ( -15.48999599679679662, 117.9999999999999716, -7.500000000000000000 ) ) ;
#57790 = ORIENTED_EDGE ( 'NONE', *, *, #39279, .T. ) ;
#57791 = CARTESIAN_POINT ( 'NONE',  ( -55.00000000000000000, -2.024042244987997205E-14, -11.50000000000000355 ) ) ;
#57793 = FILL_AREA_STYLE ('',( #30681 ) ) ;
#57792 = VECTOR ( 'NONE', #39573, 1000.000000000000000 ) ;
#57794 = LINE ( 'NONE', #4278, #57508 ) ;
#57795 = CARTESIAN_POINT ( 'NONE',  ( -182.7549999999999955, 4.716976649647091513, -6.492361379858946790 ) ) ;
#57796 = ORIENTED_EDGE ( 'NONE', *, *, #59797, .F. ) ;
#57797 = CARTESIAN_POINT ( 'NONE',  ( 10.00000000000001954, 43.00000000000000000, 45.61250543006183733 ) ) ;
#57798 =( GEOMETRIC_REPRESENTATION_CONTEXT ( 3 ) GLOBAL_UNCERTAINTY_ASSIGNED_CONTEXT ( ( #44718 ) ) GLOBAL_UNIT_ASSIGNED_CONTEXT ( ( #9193, #67223, #50114 ) ) REPRESENTATION_CONTEXT ( 'NONE', 'WORKASPACE' ) );
#57799 = CARTESIAN_POINT ( 'NONE',  ( -72.50000000000001421, 14.49137674618942562, -10.00000000000000000 ) ) ;
#57800 = VECTOR ( 'NONE', #63275, 1000.000000000000000 ) ;
#57801 = FILL_AREA_STYLE ('',( #37778 ) ) ;
#57802 = ORIENTED_EDGE ( 'NONE', *, *, #27445, .T. ) ;
#57803 = DIRECTION ( 'NONE',  ( 0.000000000000000000, 1.000000000000000000, -0.000000000000000000 ) ) ;
#57804 = EDGE_LOOP ( 'NONE', ( #35075, #38560, #51620, #69469 ) ) ;
#57805 = CARTESIAN_POINT ( 'NONE',  ( -0.3545099074454303167, -7.000000000000004441, -2.440407800158045118E-14 ) ) ;
#57806 = AXIS2_PLACEMENT_3D ( 'NONE', #16940, #55230, #27784 ) ;
#57807 =( NAMED_UNIT ( * ) SI_UNIT ( $, .STERADIAN. ) SOLID_ANGLE_UNIT ( ) );
#57808 = CARTESIAN_POINT ( 'NONE',  ( -96.80499999999999261, -8.437984349512085203, 5.166775262442717831E-16 ) ) ;
#57809 = ORIENTED_EDGE ( 'NONE', *, *, #64732, .F. ) ;
#57810 =( NAMED_UNIT ( * ) SI_UNIT ( $, .STERADIAN. ) SOLID_ANGLE_UNIT ( ) );
#57811 = DIRECTION ( 'NONE',  ( 1.000000000000000000, 0.000000000000000000, 0.000000000000000000 ) ) ;
#57812 = CARTESIAN_POINT ( 'NONE',  ( -130.2570736234661695, 5.598654528085800663, -7.705886871421367523 ) ) ;
#57813 = CARTESIAN_POINT ( 'NONE',  ( 5.598654528085809545, 154.1449999999999818, -7.705886871421373741 ) ) ;
#57814 = CARTESIAN_POINT ( 'NONE',  ( -75.80707362346616662, 10.01517768586948698, -1.839758294383808571E-15 ) ) ;
#57815 = AXIS2_PLACEMENT_3D ( 'NONE', #45215, #6156, #44536 ) ;
#57816 = CIRCLE ( 'NONE', #55538, 0.5000000000000004441 ) ;
#57817 = DIRECTION ( 'NONE',  ( 1.000000000000000000, 7.709882115452468306E-16, 0.000000000000000000 ) ) ;
#57818 = ORIENTED_EDGE ( 'NONE', *, *, #27467, .T. ) ;
#57819 = CARTESIAN_POINT ( 'NONE',  ( -15.65737470746391580, -10.92375055806530071, 4.967564989580693258 ) ) ;
#57821 = SPHERICAL_SURFACE ( 'NONE', #20123, 0.5000000000000000000 ) ;
#57820 = LINE ( 'NONE', #4679, #67289 ) ;
#57822 = VECTOR ( 'NONE', #23623, 1000.000000000000000 ) ;
#57823 = CARTESIAN_POINT ( 'NONE',  ( -107.3049999999999784, 8.437984349512085203, -1.550032578732815448E-15 ) ) ;
#57824 = CARTESIAN_POINT ( 'NONE',  ( -9.058813317711338797, 119.3449999999999989, 2.943386871421373563 ) ) ;
#57825 = CARTESIAN_POINT ( 'NONE',  ( -123.2949999999999875, -2.607480562269069768, 8.024999999999991473 ) ) ;
#57826 = ADVANCED_FACE ( 'NONE', ( #8896 ), #45574, .T. ) ;
#57827 = AXIS2_PLACEMENT_3D ( 'NONE', #40480, #35874, #56639 ) ;
#57828 = CIRCLE ( 'NONE', #38734, 0.2500000000000002220 ) ;
#57829 = CARTESIAN_POINT ( 'NONE',  ( -111.8070736234661666, 10.01517768586948698, -1.839758294383808966E-15 ) ) ;
#57830 = ADVANCED_FACE ( 'NONE', ( #30320 ), #37768, .F. ) ;
#57831 = PRESENTATION_STYLE_ASSIGNMENT (( #36413 ) ) ;
#57832 = CARTESIAN_POINT ( 'NONE',  ( 29.00000000000000000, 42.00000000000000000, -80.00402776293826435 ) ) ;
#57833 = ORIENTED_EDGE ( 'NONE', *, *, #25803, .T. ) ;
#57834 = CARTESIAN_POINT ( 'NONE',  ( -167.9070736234663457, -3.094860106615454853, 9.525000000002153300 ) ) ;
#57835 = CARTESIAN_POINT ( 'NONE',  ( -166.9429263765337907, 0.000000000000000000, 9.524999999999991473 ) ) ;
#57836 = FILL_AREA_STYLE_COLOUR ( '', #66851 ) ;
#57837 = AXIS2_PLACEMENT_3D ( 'NONE', #39190, #44142, #1460 ) ;
#57838 = MECHANICAL_DESIGN_GEOMETRIC_PRESENTATION_REPRESENTATION (  '', ( #50016 ), #34223 ) ;
#57839 = EDGE_CURVE ( 'NONE', #9072, #20368, #64788, .T. ) ;
#57840 = PLANE ( 'NONE',  #9610 ) ;
#57841 = EDGE_CURVE ( 'NONE', #69641, #28845, #16338, .T. ) ;
#57842 = AXIS2_PLACEMENT_3D ( 'NONE', #20570, #42086, #40748 ) ;
#57843 = B_SPLINE_CURVE_WITH_KNOTS ( 'NONE', 3,
 ( #37317, #10545, #31984, #5239, #26682, #66414, #8019, #66772, #40073, #61804 ),
 .UNSPECIFIED., .F., .F.,
 ( 4, 2, 2, 2, 4 ),
 ( 0.009262909725840906203, 0.01194559479670475113, 0.01328693733213667447, 0.01395760859985263613, 0.01462827986756859780 ),
 .UNSPECIFIED. ) ;
#57844 = CARTESIAN_POINT ( 'NONE',  ( -20.58910881788679603, 114.8399099445016276, -10.00000000000000355 ) ) ;
#57845 = PRESENTATION_LAYER_ASSIGNMENT (  '', '', ( #18519 ) ) ;
#57846 = CARTESIAN_POINT ( 'NONE',  ( -54.73148258177910463, -9.107254030097815090, -2.000000000000000000 ) ) ;
#57847 = ORIENTED_EDGE ( 'NONE', *, *, #19442, .T. ) ;
#57848 = ADVANCED_FACE ( 'NONE', ( #5333, #37421, #32088 ), #4997, .F. ) ;
#57849 = CARTESIAN_POINT ( 'NONE',  ( -89.39292637653377938, 8.102448949553176405, 5.886773742842740909 ) ) ;
#57850 = AXIS2_PLACEMENT_3D ( 'NONE', #9604, #56735, #35629 ) ;
#57851 = CARTESIAN_POINT ( 'NONE',  ( -166.3429263765337964, -9.058813317711329915, 2.943386871421371787 ) ) ;
#57852 = EDGE_CURVE ( 'NONE', #14977, #59828, #8488, .T. ) ;
#57853 = AXIS2_PLACEMENT_3D ( 'NONE', #47401, #35766, #3347 ) ;
#57854 = CARTESIAN_POINT ( 'NONE',  ( 6.826472737025119919, 151.8929263765337510, 4.959722759717908325 ) ) ;
#57855 = CARTESIAN_POINT ( 'NONE',  ( 30.99999999999999289, 5.000000000000000000, -24.00402776293822171 ) ) ;
#57856 = DIRECTION ( 'NONE',  ( -0.000000000000000000, -1.000000000000000000, -0.000000000000000000 ) ) ;
#57857 = CARTESIAN_POINT ( 'NONE',  ( -178.5549999999999784, 0.000000000000000000, 8.024999999999991473 ) ) ;
#57858 = ORIENTED_EDGE ( 'NONE', *, *, #12007, .T. ) ;
#57859 = DIRECTION ( 'NONE',  ( 0.000000000000000000, 0.000000000000000000, 1.000000000000000000 ) ) ;
#57860 = CARTESIAN_POINT ( 'NONE',  ( 0.04677136509298115974, 68.99999999999998579, 12.50000000000000000 ) ) ;
#57861 = CARTESIAN_POINT ( 'NONE',  ( -24.00000000000000355, 37.00000000000000000, -3.750000000000000000 ) ) ;
#57862 = ORIENTED_EDGE ( 'NONE', *, *, #64729, .F. ) ;
#57863 = CARTESIAN_POINT ( 'NONE',  ( -102.5929263765348338, -3.094860106635640928, -9.524999999987485921 ) ) ;
#57864 = CARTESIAN_POINT ( 'NONE',  ( -34.99999999999992895, 113.4999999999999858, -7.500000000000000000 ) ) ;
#57865 = CARTESIAN_POINT ( 'NONE',  ( 7.632228543268607446, 144.1570736234661751, 2.479861379858954606 ) ) ;
#57866 = CARTESIAN_POINT ( 'NONE',  ( 10.00000000000001954, 42.00000000000000000, -35.50000000000000000 ) ) ;
#57867 = AXIS2_PLACEMENT_3D ( 'NONE', #40097, #29129, #55180 ) ;
#57868 = ORIENTED_EDGE ( 'NONE', *, *, #59394, .F. ) ;
#57869 = CARTESIAN_POINT ( 'NONE',  ( -101.9070736234671841, -3.094860106601623695, 9.525000000012200374 ) ) ;
#57870 = CARTESIAN_POINT ( 'NONE',  ( -99.05499999999999261, -9.827790563157499189E-16, -8.024999999999991473 ) ) ;
#57871 = B_SPLINE_CURVE_WITH_KNOTS ( 'NONE', 3,
 ( #54912, #44094, #33155, #6740, #49682, #39150 ),
 .UNSPECIFIED., .F., .F.,
 ( 4, 2, 4 ),
 ( 0.005386537104126977275, 0.008060814333094816833, 0.01073509156206265552 ),
 .UNSPECIFIED. ) ;
#57872 = VERTEX_POINT ( 'NONE', #37059 ) ;
#57873 = CARTESIAN_POINT ( 'NONE',  ( 5.196152422706628471, -1.107695154586738173, -9.000000000000005329 ) ) ;
#57874 = AXIS2_PLACEMENT_3D ( 'NONE', #43157, #46072, #40793 ) ;
#57875 = FILL_AREA_STYLE ('',( #15658 ) ) ;
#57876 = DIRECTION ( 'NONE',  ( -0.000000000000000000, -0.000000000000000000, 1.000000000000000000 ) ) ;
#57877 = STYLED_ITEM ( 'NONE', ( #13622 ), #49130 ) ;
#57878 = ORIENTED_EDGE ( 'NONE', *, *, #45263, .F. ) ;
#57879 = DIRECTION ( 'NONE',  ( 1.000000000000000000, 0.000000000000000000, 0.000000000000000000 ) ) ;
#57880 = CARTESIAN_POINT ( 'NONE',  ( -75.59499999999998465, 2.607480562269073321, 8.024999999999991473 ) ) ;
#57881 = ORIENTED_EDGE ( 'NONE', *, *, #28726, .T. ) ;
#57882 = DIRECTION ( 'NONE',  ( 0.000000000000000000, 0.000000000000000000, 1.000000000000000000 ) ) ;
#57883 = CARTESIAN_POINT ( 'NONE',  ( -120.8070736234661666, 10.01517768586948698, -1.839758294383808966E-15 ) ) ;
#57884 = UNCERTAINTY_MEASURE_WITH_UNIT (LENGTH_MEASURE( 1.000000000000000082E-05 ), #60377, 'distance_accuracy_value', 'NONE');
#57885 = ORIENTED_EDGE ( 'NONE', *, *, #45145, .T. ) ;
#57886 = CARTESIAN_POINT ( 'NONE',  ( -195.0000000000000000, 7.499999999999984901, 0.000000000000000000 ) ) ;
#57887 = CARTESIAN_POINT ( 'NONE',  ( 7.899999999999995914, 11.99999999999999289, 4.000000000000000000 ) ) ;
#57888 = DIRECTION ( 'NONE',  ( 0.000000000000000000, 0.000000000000000000, -1.000000000000000000 ) ) ;
#57889 = LINE ( 'NONE', #62782, #63785 ) ;
#57890 = ORIENTED_EDGE ( 'NONE', *, *, #53238, .T. ) ;
#57891 = AXIS2_PLACEMENT_3D ( 'NONE', #39132, #12335, #66157 ) ;
#57892 = EDGE_LOOP ( 'NONE', ( #52166, #23600, #38421, #54711 ) ) ;
#57893 = PLANE ( 'NONE',  #59362 ) ;
#57894 = FACE_OUTER_BOUND ( 'NONE', #14573, .T. ) ;
#57895 = CARTESIAN_POINT ( 'NONE',  ( -41.26950967128010461, 107.7917145016473910, 3.849034857644454188 ) ) ;
#57896 = CARTESIAN_POINT ( 'NONE',  ( -170.0070736234661410, -8.102448949553172852, -5.886773742842741797 ) ) ;
#57897 = CARTESIAN_POINT ( 'NONE',  ( -9.058813317711338797, 122.3449999999999847, 2.943386871421373563 ) ) ;
#57898 = VECTOR ( 'NONE', #44747, 1000.000000000000000 ) ;
#57899 = CARTESIAN_POINT ( 'NONE',  ( -106.1070736234661638, 8.102448949553171076, -5.886773742842744461 ) ) ;
#57900 = CARTESIAN_POINT ( 'NONE',  ( 2.607480562269082647, 112.5929263765338106, 8.024999999999993250 ) ) ;
#57901 = VECTOR ( 'NONE', #3264, 1000.000000000000000 ) ;
#57902 = SURFACE_STYLE_USAGE ( .BOTH. , #20241 ) ;
#57903 = VERTEX_POINT ( 'NONE', #26452 ) ;
#57904 = SURFACE_SIDE_STYLE ('',( #25518 ) ) ;
#57906 = CARTESIAN_POINT ( 'NONE',  ( -115.5570736234661808, -1.166476076187852838E-15, -9.524999999999991473 ) ) ;
#57905 = CYLINDRICAL_SURFACE ( 'NONE', #63812, 9.524999999999991473 ) ;
#57907 = SURFACE_STYLE_USAGE ( .BOTH. , #13939 ) ;
#57908 = CARTESIAN_POINT ( 'NONE',  ( -138.8050000000000068, -8.437984349512085203, 5.166775262442717831E-16 ) ) ;
#57909 = EDGE_CURVE ( 'NONE', #9284, #66764, #5094, .T. ) ;
#57910 = SURFACE_SIDE_STYLE ('',( #62804 ) ) ;
#57911 = CARTESIAN_POINT ( 'NONE',  ( -150.8950000000000102, 6.826472737025116366, 4.959722759717898555 ) ) ;
#57912 = EDGE_CURVE ( 'NONE', #27898, #44763, #56783, .T. ) ;
#57913 = CARTESIAN_POINT ( 'NONE',  ( -148.9449999999999932, -9.827790563157499189E-16, -8.024999999999991473 ) ) ;
#57914 = ORIENTED_EDGE ( 'NONE', *, *, #13220, .T. ) ;
#57915 = B_SPLINE_CURVE_WITH_KNOTS ( 'NONE', 3,
 ( #3723, #3360, #20638, #57941, #46367, #51263, #3008, #46007, #19927 ),
 .UNSPECIFIED., .F., .F.,
 ( 4, 2, 1, 2, 4 ),
 ( 0.01084732271231145413, 0.01152005980350376095, 0.01219279689469606777, 0.01353827107708068141, 0.01622921944184991042 ),
 .UNSPECIFIED. ) ;
#57916 = EDGE_CURVE ( 'NONE', #25674, #2846, #3927, .T. ) ;
#57917 = CARTESIAN_POINT ( 'NONE',  ( -5.196152422706636465, 1.107695154586737063, 9.000000000000001776 ) ) ;
#57918 =( GEOMETRIC_REPRESENTATION_CONTEXT ( 3 ) GLOBAL_UNCERTAINTY_ASSIGNED_CONTEXT ( ( #3862 ) ) GLOBAL_UNIT_ASSIGNED_CONTEXT ( ( #13227, #1922, #7284 ) ) REPRESENTATION_CONTEXT ( 'NONE', 'WORKASPACE' ) );
#57919 = FILL_AREA_STYLE ('',( #21289 ) ) ;
#57920 = DIRECTION ( 'NONE',  ( 0.000000000000000000, 0.000000000000000000, 1.000000000000000000 ) ) ;
#57921 = UNCERTAINTY_MEASURE_WITH_UNIT (LENGTH_MEASURE( 1.000000000000000082E-05 ), #61028, 'distance_accuracy_value', 'NONE');
#57922 = CARTESIAN_POINT ( 'NONE',  ( -62.15499999999998693, 7.632228543268600340, 2.479861379858949277 ) ) ;
#57923 = SURFACE_SIDE_STYLE ('',( #4066 ) ) ;
#57924 = AXIS2_PLACEMENT_3D ( 'NONE', #23041, #49432, #11428 ) ;
#57925 = CARTESIAN_POINT ( 'NONE',  ( -65.54499999999998749, -7.632228543268600340, -2.479861379858950166 ) ) ;
#57926 = CARTESIAN_POINT ( 'NONE',  ( -5.598654528085806881, 152.8549999999999898, -7.705886871421374629 ) ) ;
#57927 = EDGE_CURVE ( 'NONE', #48746, #25674, #37751, .T. ) ;
#57928 = AXIS2_PLACEMENT_3D ( 'NONE', #53286, #63813, #48046 ) ;
#57929 = STYLED_ITEM ( 'NONE', ( #66351 ), #5388 ) ;
#57930 = SURFACE_SIDE_STYLE ('',( #63192 ) ) ;
#57931 = UNCERTAINTY_MEASURE_WITH_UNIT (LENGTH_MEASURE( 1.000000000000000082E-05 ), #35758, 'distance_accuracy_value', 'NONE');
#57932 = DIRECTION ( 'NONE',  ( 1.786087863151539797E-17, -1.942890293094023946E-16, -1.000000000000000000 ) ) ;
#57933 = SURFACE_STYLE_FILL_AREA ( #29432 ) ;
#57934 = ADVANCED_FACE ( 'NONE', ( #65116 ), #21890, .F. ) ;
#57935 = CARTESIAN_POINT ( 'NONE',  ( -82.40707362346617515, 3.094860106618428031, -9.524999999999993250 ) ) ;
#57936 = CARTESIAN_POINT ( 'NONE',  ( -177.8929263765338078, -8.102448949553174629, -5.886773742842741797 ) ) ;
#57937 = AXIS2_PLACEMENT_3D ( 'NONE', #57686, #31976, #64333 ) ;
#57938 = DIRECTION ( 'NONE',  ( 0.000000000000000000, 0.000000000000000000, -1.000000000000000000 ) ) ;
#57939 = CARTESIAN_POINT ( 'NONE',  ( -29.67263558057812389, -7.738202242605012771, -0.6497364857716234621 ) ) ;
#57940 = VECTOR ( 'NONE', #37677, 1000.000000000000000 ) ;
#57941 = CARTESIAN_POINT ( 'NONE',  ( -0.9109038252169214811, -2.456844516558468694, -9.000000000000003553 ) ) ;
#57942 = VERTEX_POINT ( 'NONE', #59855 ) ;
#57943 = VERTEX_POINT ( 'NONE', #33136 ) ;
#57945 = CARTESIAN_POINT ( 'NONE',  ( -44.99999999999998579, 119.9999999999999716, 9.500000000000000000 ) ) ;
#57944 = TOROIDAL_SURFACE ( 'NONE', #27580, 14.49999999999999822, 0.5000000000000000000 ) ;
#57946 = AXIS2_PLACEMENT_3D ( 'NONE', #17010, #39874, #61278 ) ;
#57947 = CARTESIAN_POINT ( 'NONE',  ( -20.06856914206998610, 114.9886858359306814, 10.44306996520268527 ) ) ;
#57948 = SPHERICAL_SURFACE ( 'NONE', #40679, 0.2500000000000000000 ) ;
#57949 =( NAMED_UNIT ( * ) PLANE_ANGLE_UNIT ( ) SI_UNIT ( $, .RADIAN. ) );
#57950 = ORIENTED_EDGE ( 'NONE', *, *, #47302, .T. ) ;
#57951 = ORIENTED_EDGE ( 'NONE', *, *, #5769, .F. ) ;
#57952 = CARTESIAN_POINT ( 'NONE',  ( 9.250000000000003553, 27.99999999999998934, -3.750000000000000000 ) ) ;
#57953 = SURFACE_SIDE_STYLE ('',( #10451 ) ) ;
#57954 = ORIENTED_EDGE ( 'NONE', *, *, #4506, .F. ) ;
#57955 = CARTESIAN_POINT ( 'NONE',  ( -1.166476076187854022E-15, 121.0549999999999784, 9.525000000000000355 ) ) ;
#57956 = DIRECTION ( 'NONE',  ( 0.000000000000000000, 0.000000000000000000, -1.000000000000000000 ) ) ;
#57957 = CARTESIAN_POINT ( 'NONE',  ( 12.25000000000000533, 28.24999999999998224, 3.750000000000000000 ) ) ;
#57958 = FACE_OUTER_BOUND ( 'NONE', #15045, .T. ) ;
#57959 = CARTESIAN_POINT ( 'NONE',  ( -102.4449999999999932, 0.000000000000000000, 8.024999999999991473 ) ) ;
#57960 = ORIENTED_EDGE ( 'NONE', *, *, #33913, .F. ) ;
#57961 = EDGE_CURVE ( 'NONE', #38966, #25423, #27810, .T. ) ;
#57962 = CARTESIAN_POINT ( 'NONE',  ( -52.94292637653380496, 0.000000000000000000, 9.524999999999991473 ) ) ;
#57963 = ORIENTED_EDGE ( 'NONE', *, *, #35763, .F. ) ;
#57964 = CARTESIAN_POINT ( 'NONE',  ( 7.632228543268608334, 152.3429263765338249, -2.479861379858951942 ) ) ;
#57965 = CYLINDRICAL_SURFACE ( 'NONE', #41418, 0.5000000000000004441 ) ;
#57966 = MECHANICAL_DESIGN_GEOMETRIC_PRESENTATION_REPRESENTATION (  '', ( #5120 ), #4001 ) ;
#57967 = DIRECTION ( 'NONE',  ( 0.000000000000000000, 0.000000000000000000, -1.000000000000000000 ) ) ;
#57968 =( NAMED_UNIT ( * ) PLANE_ANGLE_UNIT ( ) SI_UNIT ( $, .RADIAN. ) );
#57969 = ORIENTED_EDGE ( 'NONE', *, *, #64148, .F. ) ;
#57970 = CARTESIAN_POINT ( 'NONE',  ( 20.22778885548742522, 114.9430298377684210, -10.39013442403998866 ) ) ;
#57971 = ORIENTED_EDGE ( 'NONE', *, *, #42385, .T. ) ;
#57972 = AXIS2_PLACEMENT_3D ( 'NONE', #10206, #43308, #10551 ) ;
#57973 = CARTESIAN_POINT ( 'NONE',  ( 48.50000000000000000, 99.99999999999992895, 7.500000000000000000 ) ) ;
#57974 = CARTESIAN_POINT ( 'NONE',  ( -140.2429263765338021, 5.598654528085804216, 7.705886871421366635 ) ) ;
#57975 = CARTESIAN_POINT ( 'NONE',  ( -33.41404910821478325, -9.512283121613517523, 3.449313401996988215 ) ) ;
#57976 = CIRCLE ( 'NONE', #54594, 0.5000000000000004441 ) ;
#57977 = SURFACE_STYLE_FILL_AREA ( #13655 ) ;
#57978 = PRESENTATION_STYLE_ASSIGNMENT (( #29116 ) ) ;
#57979 = SURFACE_STYLE_USAGE ( .BOTH. , #10476 ) ;
#57980 = CARTESIAN_POINT ( 'NONE',  ( -4.750000000000002665, 22.24999999999998579, 3.750000000000000000 ) ) ;
#57981 = CARTESIAN_POINT ( 'NONE',  ( -183.0000000000000284, -1.154738647139537111, 9.454745033939424559 ) ) ;
#57982 = SURFACE_SIDE_STYLE ('',( #41131 ) ) ;
#57983 = CARTESIAN_POINT ( 'NONE',  ( 98.00000000000000000, 14.00000000000000000, 0.000000000000000000 ) ) ;
#57984 = ORIENTED_EDGE ( 'NONE', *, *, #68140, .T. ) ;
#57985 = ORIENTED_EDGE ( 'NONE', *, *, #59554, .T. ) ;
#57986 =( LENGTH_UNIT ( ) NAMED_UNIT ( * ) SI_UNIT ( .MILLI., .METRE. ) );
#57987 = CARTESIAN_POINT ( 'NONE',  ( 4.000000000000002665, 42.00000000000000000, 0.000000000000000000 ) ) ;
#57988 = CARTESIAN_POINT ( 'NONE',  ( -182.5429263765337851, 9.058813317711329915, 2.943386871421369566 ) ) ;
#57989 = ADVANCED_FACE ( 'NONE', ( #7441 ), #60521, .F. ) ;
#57990 = DIRECTION ( 'NONE',  ( 0.000000000000000000, 1.000000000000000000, -0.000000000000000000 ) ) ;
#57992 = ORIENTED_EDGE ( 'NONE', *, *, #40482, .T. ) ;
#57991 = VECTOR ( 'NONE', #21077, 1000.000000000000000 ) ;
#57993 = CARTESIAN_POINT ( 'NONE',  ( -154.9429263765338192, 0.000000000000000000, 9.524999999999991473 ) ) ;
#57994 = CARTESIAN_POINT ( 'NONE',  ( -176.7549999999999955, 4.716976649647091513, -6.492361379858946790 ) ) ;
#57995 = ADVANCED_FACE ( 'NONE', ( #2800 ), #1689, .F. ) ;
#57996 = LINE ( 'NONE', #62886, #32999 ) ;
#57997 = DIRECTION ( 'NONE',  ( -1.000000000000000000, 0.000000000000000000, 0.000000000000000000 ) ) ;
#57998 = CARTESIAN_POINT ( 'NONE',  ( -179.5450000000000159, -7.632228543268600340, -2.479861379858950166 ) ) ;
#57999 = VECTOR ( 'NONE', #58487, 1000.000000000000000 ) ;
#58000 = CARTESIAN_POINT ( 'NONE',  ( -173.8449999999999989, -7.632228543268599452, 2.479861379858951054 ) ) ;
#58001 =( GEOMETRIC_REPRESENTATION_CONTEXT ( 3 ) GLOBAL_UNCERTAINTY_ASSIGNED_CONTEXT ( ( #22883 ) ) GLOBAL_UNIT_ASSIGNED_CONTEXT ( ( #50936, #58548, #67107 ) ) REPRESENTATION_CONTEXT ( 'NONE', 'WORKASPACE' ) );
#58002 = VERTEX_POINT ( 'NONE', #23599 ) ;
#58003 =( NAMED_UNIT ( * ) SI_UNIT ( $, .STERADIAN. ) SOLID_ANGLE_UNIT ( ) );
#58004 = EDGE_CURVE ( 'NONE', #63980, #54030, #65831, .T. ) ;
#58005 = CARTESIAN_POINT ( 'NONE',  ( -5.196152422706636465, -1.107695154586737063, 9.000000000000001776 ) ) ;
#58006 = CARTESIAN_POINT ( 'NONE',  ( -54.35505119478604286, -9.142989783843194829, -2.885398154219640965 ) ) ;
#58007 = CARTESIAN_POINT ( 'NONE',  ( -95.90500000000000114, 2.607480562269068880, -8.024999999999993250 ) ) ;
#58008 = DIRECTION ( 'NONE',  ( 0.000000000000000000, 1.000000000000000000, -0.000000000000000000 ) ) ;
#58009 = DIRECTION ( 'NONE',  ( 0.000000000000000000, 0.000000000000000000, -1.000000000000000000 ) ) ;
#58010 = PRESENTATION_STYLE_ASSIGNMENT (( #47124 ) ) ;
#58011 = EDGE_CURVE ( 'NONE', #61698, #68819, #17329, .T. ) ;
#58012 = CARTESIAN_POINT ( 'NONE',  ( -93.29499999999998749, -2.607480562269069768, 8.024999999999991473 ) ) ;
#58013 = CARTESIAN_POINT ( 'NONE',  ( -3.094860106618432471, 128.7049999999999841, -9.525000000000000355 ) ) ;
#58014 = CARTESIAN_POINT ( 'NONE',  ( -68.09499999999998465, -2.607480562269071545, -8.024999999999991473 ) ) ;
#58015 = DIRECTION ( 'NONE',  ( -1.000000000000000000, 0.000000000000000000, 0.000000000000000000 ) ) ;
#58016 = EDGE_CURVE ( 'NONE', #41095, #4575, #2802, .T. ) ;
#58017 = CARTESIAN_POINT ( 'NONE',  ( 3.728548500389071485, -7.000000000000003553, 0.9264520766856032541 ) ) ;
#58018 = DIRECTION ( 'NONE',  ( -1.000000000000000000, 0.000000000000000000, 0.000000000000000000 ) ) ;
#58019 = UNCERTAINTY_MEASURE_WITH_UNIT (LENGTH_MEASURE( 1.000000000000000082E-05 ), #44649, 'distance_accuracy_value', 'NONE');
#58020 = FACE_OUTER_BOUND ( 'NONE', #21827, .T. ) ;
#58021 = ORIENTED_EDGE ( 'NONE', *, *, #20239, .T. ) ;
#58022 = ADVANCED_FACE ( 'NONE', ( #17663 ), #7760, .F. ) ;
#58023 = DIRECTION ( 'NONE',  ( 0.2831056412805232902, 0.9590887320134375837, 0.000000000000000000 ) ) ;
#58024 = DIRECTION ( 'NONE',  ( 0.000000000000000000, 0.000000000000000000, -1.000000000000000000 ) ) ;
#58025 = VECTOR ( 'NONE', #46036, 1000.000000000000000 ) ;
#58026 = DIRECTION ( 'NONE',  ( 1.000000000000000000, -0.000000000000000000, 0.000000000000000000 ) ) ;
#58027 = DIRECTION ( 'NONE',  ( -0.9704308468600219006, -0.2413793103448194921, -0.000000000000000000 ) ) ;
#58028 = ORIENTED_EDGE ( 'NONE', *, *, #66467, .F. ) ;
#58029 = ORIENTED_EDGE ( 'NONE', *, *, #68149, .T. ) ;
#58030 = CARTESIAN_POINT ( 'NONE',  ( -45.57139843939562240, 8.073466093857248893, -6.500000000000084377 ) ) ;
#58031 =( BOUNDED_CURVE ( )  B_SPLINE_CURVE ( 2, ( #53559, #69395, #5344, #15268, #25771, #10990, #14907, #42367, #63751, #10313, #26114 ),
 .UNSPECIFIED., .F., .F. ) 
 B_SPLINE_CURVE_WITH_KNOTS ( ( 3, 2, 2, 2, 2, 3 ),
 ( 0.3913043478260777031, 0.3934782608695558959, 0.3956521739130340887, 0.3978260869565122815, 0.3999999999999905298, 0.4021739130434687226 ),
 .UNSPECIFIED. ) 
 CURVE ( )  GEOMETRIC_REPRESENTATION_ITEM ( )  RATIONAL_B_SPLINE_CURVE ( ( 1.000000000000208722, 0.9510565162949448093, 1.000000000000000000, 0.9510565162951535312, 1.000000000000000000, 0.9510565162951535312, 1.000000000000000000, 0.9510565162951535312, 1.000000000000000000, 0.9510565162953684704, 0.9999999999997850608 ) ) 
 REPRESENTATION_ITEM ( '' )  );
#58032 = UNCERTAINTY_MEASURE_WITH_UNIT (LENGTH_MEASURE( 1.000000000000000082E-05 ), #51349, 'distance_accuracy_value', 'NONE');
#58033 = FACE_OUTER_BOUND ( 'NONE', #10907, .T. ) ;
#58034 =( NAMED_UNIT ( * ) PLANE_ANGLE_UNIT ( ) SI_UNIT ( $, .RADIAN. ) );
#58035 = DIRECTION ( 'NONE',  ( 0.000000000000000000, 0.000000000000000000, -1.000000000000000000 ) ) ;
#58036 = LINE ( 'NONE', #47877, #12755 ) ;
#58037 = VERTEX_POINT ( 'NONE', #28516 ) ;
#58038 = CARTESIAN_POINT ( 'NONE',  ( -126.0550000000000068, -9.827790563157499189E-16, -8.024999999999991473 ) ) ;
#58039 = EDGE_LOOP ( 'NONE', ( #64720, #66046, #28771, #24183 ) ) ;
#58040 = DIRECTION ( 'NONE',  ( -1.000000000000000000, 1.541976423090494529E-14, 0.000000000000000000 ) ) ;
#58041 = STYLED_ITEM ( 'NONE', ( #59488 ), #40379 ) ;
#58042 = CARTESIAN_POINT ( 'NONE',  ( 20.99028635741426640, 114.7785533247281933, -10.00000000000000000 ) ) ;
#58043 = ORIENTED_EDGE ( 'NONE', *, *, #15888, .T. ) ;
#58044 = CARTESIAN_POINT ( 'NONE',  ( 23.71231517720798010, 113.4999999999999858, 7.000000000000000000 ) ) ;
#58045 = ORIENTED_EDGE ( 'NONE', *, *, #2746, .F. ) ;
#58046 = DIRECTION ( 'NONE',  ( 1.000000000000000000, 0.000000000000000000, 0.000000000000000000 ) ) ;
#58047 = CARTESIAN_POINT ( 'NONE',  ( -9.058813317711337021, 146.0449999999999875, -2.943386871421374895 ) ) ;
#58048 = CARTESIAN_POINT ( 'NONE',  ( 48.50000000000000000, 21.99999999999998579, 3.750000000000000000 ) ) ;
#58049 = ADVANCED_FACE ( 'NONE', ( #28862 ), #50017, .T. ) ;
#58050 = ORIENTED_EDGE ( 'NONE', *, *, #46482, .F. ) ;
#58051 = CARTESIAN_POINT ( 'NONE',  ( -3.094860106618432471, 149.7049999999999557, -9.525000000000000355 ) ) ;
#58052 = SURFACE_STYLE_USAGE ( .BOTH. , #24977 ) ;
#58053 = ORIENTED_EDGE ( 'NONE', *, *, #2822, .T. ) ;
#58054 = CARTESIAN_POINT ( 'NONE',  ( 4.716976649647096842, 121.7429263765338163, 6.492361379858953896 ) ) ;
#58055 = LINE ( 'NONE', #9862, #43557 ) ;
#58056 = UNCERTAINTY_MEASURE_WITH_UNIT (LENGTH_MEASURE( 1.000000000000000082E-05 ), #8196, 'distance_accuracy_value', 'NONE');
#58057 = CARTESIAN_POINT ( 'NONE',  ( -46.85707362346616378, -5.598654528085803328, -7.705886871421366635 ) ) ;
#58058 = CARTESIAN_POINT ( 'NONE',  ( 45.65811388300841855, 10.21937129433612235, 6.000000000000000888 ) ) ;
#58059 = CARTESIAN_POINT ( 'NONE',  ( 44.25000000000000000, 0.000000000000000000, 3.750000000000000000 ) ) ;
#58060 = DIRECTION ( 'NONE',  ( 0.000000000000000000, -0.000000000000000000, 1.000000000000000000 ) ) ;
#58061 = EDGE_LOOP ( 'NONE', ( #56290, #42253, #27170, #68010 ) ) ;
#58062 = CARTESIAN_POINT ( 'NONE',  ( -40.78947368421051323, 108.1536491499103505, -3.000000000000000444 ) ) ;
#58063 = ORIENTED_EDGE ( 'NONE', *, *, #18505, .T. ) ;
#58064 = CARTESIAN_POINT ( 'NONE',  ( -55.04292637653379927, -9.058813317711329915, -2.943386871421370898 ) ) ;
#58065 = DIRECTION ( 'NONE',  ( -1.000000000000000000, 0.000000000000000000, 0.000000000000000000 ) ) ;
#58066 = CARTESIAN_POINT ( 'NONE',  ( -152.3050000000000068, 8.437984349512085203, -1.550032578732815448E-15 ) ) ;
#58067 = VERTEX_POINT ( 'NONE', #23263 ) ;
#58068 = CARTESIAN_POINT ( 'NONE',  ( 15.98999599679679839, 117.4999999999999716, -9.500000000000000000 ) ) ;
#58069 = UNCERTAINTY_MEASURE_WITH_UNIT (LENGTH_MEASURE( 1.000000000000000082E-05 ), #39270, 'distance_accuracy_value', 'NONE');
#58070 = EDGE_CURVE ( 'NONE', #6981, #37694, #515, .T. ) ;
#58071 = CARTESIAN_POINT ( 'NONE',  ( -45.99999999999998579, 0.000000000000000000, 0.000000000000000000 ) ) ;
#58072 = CARTESIAN_POINT ( 'NONE',  ( -52.18882097621168725, -9.718525487687024622, 4.712719346062894665 ) ) ;
#58073 = CARTESIAN_POINT ( 'NONE',  ( 74.59716837049619187, 19.66257108179090096, 6.399833413891846234 ) ) ;
#58074 = DIRECTION ( 'NONE',  ( 0.000000000000000000, -6.938893903907222067E-15, 1.000000000000000000 ) ) ;
#58075 = ORIENTED_EDGE ( 'NONE', *, *, #49255, .T. ) ;
#58076 = ORIENTED_EDGE ( 'NONE', *, *, #21871, .F. ) ;
#58077 = CARTESIAN_POINT ( 'NONE',  ( -75.50000000000000000, -8.499999999999991118, 21.00000000000000000 ) ) ;
#58078 = PRESENTATION_LAYER_ASSIGNMENT (  '', '', ( #9766 ) ) ;
#58079 = PRESENTATION_STYLE_ASSIGNMENT (( #53803 ) ) ;
#58080 = ADVANCED_FACE ( 'NONE', ( #66879 ), #12691, .F. ) ;
#58081 = CARTESIAN_POINT ( 'NONE',  ( -70.85499999999998977, 4.716976649647094177, 6.492361379858945902 ) ) ;
#58082 = ORIENTED_EDGE ( 'NONE', *, *, #26984, .F. ) ;
#58083 = ADVANCED_FACE ( 'NONE', ( #40162 ), #61556, .F. ) ;
#58085 = AXIS2_PLACEMENT_3D ( 'NONE', #68342, #45623, #67039 ) ;
#58084 = CARTESIAN_POINT ( 'NONE',  ( 34.99999999999999289, 146.4999999999999716, 7.500000000000000000 ) ) ;
#58086 =( GEOMETRIC_REPRESENTATION_CONTEXT ( 3 ) GLOBAL_UNCERTAINTY_ASSIGNED_CONTEXT ( ( #67964 ) ) GLOBAL_UNIT_ASSIGNED_CONTEXT ( ( #50689, #29568, #41207 ) ) REPRESENTATION_CONTEXT ( 'NONE', 'WORKASPACE' ) );
#58087 = DIRECTION ( 'NONE',  ( 0.000000000000000000, 0.000000000000000000, 1.000000000000000000 ) ) ;
#58088 = DIRECTION ( 'NONE',  ( 1.000000000000000000, 0.000000000000000000, 0.000000000000000000 ) ) ;
#58089 = VERTEX_POINT ( 'NONE', #9177 ) ;
#58090 = EDGE_CURVE ( 'NONE', #22128, #21243, #58523, .T. ) ;
#58091 = DIRECTION ( 'NONE',  ( -0.000000000000000000, -0.000000000000000000, -1.000000000000000000 ) ) ;
#58092 = SURFACE_STYLE_USAGE ( .BOTH. , #4950 ) ;
#58093 = EDGE_CURVE ( 'NONE', #44784, #23681, #42226, .T. ) ;
#58094 = STYLED_ITEM ( 'NONE', ( #20036 ), #40798 ) ;
#58095 = CARTESIAN_POINT ( 'NONE',  ( 0.000000000000000000, 148.4449999999999932, -9.525000000000000355 ) ) ;
#58096 = CARTESIAN_POINT ( 'NONE',  ( -101.5449999999999875, -7.632228543268600340, -2.479861379858950166 ) ) ;
#58097 = DIRECTION ( 'NONE',  ( -1.156482317317870344E-15, -1.000000000000000000, 0.000000000000000000 ) ) ;
#58098 = DIRECTION ( 'NONE',  ( 1.000000000000000000, -9.122956858292678705E-34, -1.300977106640434891E-16 ) ) ;
#58099 = UNCERTAINTY_MEASURE_WITH_UNIT (LENGTH_MEASURE( 1.000000000000000082E-05 ), #44153, 'distance_accuracy_value', 'NONE');
#58100 = CARTESIAN_POINT ( 'NONE',  ( 72.50000000000000000, 1.797044900979284448E-15, -9.500000000000000000 ) ) ;
#58101 = ORIENTED_EDGE ( 'NONE', *, *, #2917, .T. ) ;
#58102 = CARTESIAN_POINT ( 'NONE',  ( -134.3929263765338078, 8.102448949553176405, 5.886773742842740909 ) ) ;
#58103 = PRESENTATION_STYLE_ASSIGNMENT (( #36324 ) ) ;
#58104 = CARTESIAN_POINT ( 'NONE',  ( 22.50000000000000711, 36.75000000000000000, 3.750000000000000000 ) ) ;
#58105 = CARTESIAN_POINT ( 'NONE',  ( -160.0449999999999875, 7.632228543268600340, 2.479861379858949277 ) ) ;
#58106 = EDGE_CURVE ( 'NONE', #53591, #62231, #53465, .T. ) ;
#58107 = FILL_AREA_STYLE ('',( #36689 ) ) ;
#58108 = LINE ( 'NONE', #57757, #41738 ) ;
#58109 = ORIENTED_EDGE ( 'NONE', *, *, #2216, .F. ) ;
#58110 = ORIENTED_EDGE ( 'NONE', *, *, #63058, .T. ) ;
#58111 = ADVANCED_FACE ( 'NONE', ( #45786 ), #57702, .T. ) ;
#58112 = B_SPLINE_CURVE_WITH_KNOTS ( 'NONE', 3,
 ( #25586, #51306, #41463, #13660, #35123, #19635, #9097, #67474 ),
 .UNSPECIFIED., .F., .F.,
 ( 4, 2, 2, 4 ),
 ( 0.000000000000000000, 0.0002394028614865243657, 0.0004788057229730487314, 0.0009576114459460974629 ),
 .UNSPECIFIED. ) ;
#58113 = CARTESIAN_POINT ( 'NONE',  ( 5.356721384544673725, -2.367558512213880473, 4.721886399977921478 ) ) ;
#58114 =( NAMED_UNIT ( * ) PLANE_ANGLE_UNIT ( ) SI_UNIT ( $, .RADIAN. ) );
#58115 = CARTESIAN_POINT ( 'NONE',  ( -45.00000000000000000, 8.442834901059519837, 5.542315673751926575 ) ) ;
#58116 = CARTESIAN_POINT ( 'NONE',  ( -110.1570736234661751, -9.058813317711329915, -2.943386871421370898 ) ) ;
#58117 = CARTESIAN_POINT ( 'NONE',  ( 9.000000000000003553, 27.74999999999998934, 3.750000000000000000 ) ) ;
#58118 = VERTEX_POINT ( 'NONE', #46855 ) ;
#58119 = CARTESIAN_POINT ( 'NONE',  ( -153.8049999999999784, -8.437984349512086979, 5.166775262442717831E-16 ) ) ;
#58120 = MECHANICAL_DESIGN_GEOMETRIC_PRESENTATION_REPRESENTATION (  '', ( #26646 ), #51379 ) ;
#58121 = VERTEX_POINT ( 'NONE', #14103 ) ;
#58122 =( LENGTH_UNIT ( ) NAMED_UNIT ( * ) SI_UNIT ( .MILLI., .METRE. ) );
#58123 = PRESENTATION_STYLE_ASSIGNMENT (( #36705 ) ) ;
#58124 = ORIENTED_EDGE ( 'NONE', *, *, #35594, .F. ) ;
#58125 = CARTESIAN_POINT ( 'NONE',  ( -1.166476076187854022E-15, 119.9449999999999790, 9.525000000000000355 ) ) ;
#58126 =( BOUNDED_CURVE ( )  B_SPLINE_CURVE ( 3, ( #40731, #42149, #63201, #4421 ),
 .UNSPECIFIED., .F., .F. ) 
 B_SPLINE_CURVE_WITH_KNOTS ( ( 4, 4 ),
 ( 3.141592653589793116, 4.712388980384689674 ),
 .UNSPECIFIED. ) 
 CURVE ( )  GEOMETRIC_REPRESENTATION_ITEM ( )  RATIONAL_B_SPLINE_CURVE ( ( 1.000000000000000000, 0.8047378541243649375, 0.8047378541243649375, 1.000000000000000000 ) ) 
 REPRESENTATION_ITEM ( '' )  );
#58127 = ORIENTED_EDGE ( 'NONE', *, *, #28963, .F. ) ;
#58128 = DIRECTION ( 'NONE',  ( 0.000000000000000000, -1.000000000000000000, 0.000000000000000000 ) ) ;
#58129 = CARTESIAN_POINT ( 'NONE',  ( -8.102448949553179958, 117.6049999999999898, 5.886773742842747126 ) ) ;
#58130 = CARTESIAN_POINT ( 'NONE',  ( -62.75499999999998835, 4.716976649647091513, -6.492361379858946790 ) ) ;
#58131 =( NAMED_UNIT ( * ) PLANE_ANGLE_UNIT ( ) SI_UNIT ( $, .RADIAN. ) );
#58132 = ORIENTED_EDGE ( 'NONE', *, *, #4, .T. ) ;
#58133 = CARTESIAN_POINT ( 'NONE',  ( -5.598654528085808657, 147.7549999999999955, 7.705886871421373741 ) ) ;
#58134 = UNCERTAINTY_MEASURE_WITH_UNIT (LENGTH_MEASURE( 1.000000000000000082E-05 ), #5623, 'distance_accuracy_value', 'NONE');
#58135 = FACE_OUTER_BOUND ( 'NONE', #20729, .T. ) ;
#58136 = STYLED_ITEM ( 'NONE', ( #61917 ), #40879 ) ;
#58137 = FILL_AREA_STYLE ('',( #37420 ) ) ;
#58138 = EDGE_CURVE ( 'NONE', #19090, #19777, #30593, .T. ) ;
#58139 = VERTEX_POINT ( 'NONE', #68260 ) ;
#58140 = FACE_OUTER_BOUND ( 'NONE', #52436, .T. ) ;
#58141 = CARTESIAN_POINT ( 'NONE',  ( -195.0000000000000000, 0.000000000000000000, 9.524999999999991473 ) ) ;
#58142 = CARTESIAN_POINT ( 'NONE',  ( -176.9050000000000011, 2.607480562269068880, -8.024999999999993250 ) ) ;
#58143 = ORIENTED_EDGE ( 'NONE', *, *, #32988, .F. ) ;
#58144 = CARTESIAN_POINT ( 'NONE',  ( 31.14385391401492598, 43.00000000000000711, 45.61250543006183022 ) ) ;
#58145 = DIRECTION ( 'NONE',  ( 1.000000000000000000, 0.000000000000000000, -1.300977106640434891E-16 ) ) ;
#58146 = EDGE_CURVE ( 'NONE', #38350, #41509, #34327, .T. ) ;
#58147 = DIRECTION ( 'NONE',  ( 0.000000000000000000, 0.000000000000000000, 1.000000000000000000 ) ) ;
#58148 = ORIENTED_EDGE ( 'NONE', *, *, #29859, .F. ) ;
#58149 = CARTESIAN_POINT ( 'NONE',  ( 4.250000000000001776, 22.24999999999998579, -3.750000000000000000 ) ) ;
#58150 = SURFACE_SIDE_STYLE ('',( #15266 ) ) ;
#58151 = VERTEX_POINT ( 'NONE', #3125 ) ;
#58152 = CYLINDRICAL_SURFACE ( 'NONE', #39550, 3.000000000000000444 ) ;
#58154 = ADVANCED_FACE ( 'NONE', ( #31285 ), #30236, .F. ) ;
#58153 = SURFACE_STYLE_FILL_AREA ( #21546 ) ;
#58155 = CARTESIAN_POINT ( 'NONE',  ( -95.90500000000000114, 2.607480562269068880, -8.024999999999993250 ) ) ;
#58156 = ORIENTED_EDGE ( 'NONE', *, *, #16908, .F. ) ;
#58157 = CARTESIAN_POINT ( 'NONE',  ( -48.81081081081080697, 14.09971791521132900, -9.500000000000000000 ) ) ;
#58158 = CARTESIAN_POINT ( 'NONE',  ( -128.4570736234661865, -9.058813317711329915, 2.943386871421371787 ) ) ;
#58159 = CARTESIAN_POINT ( 'NONE',  ( 3.094860106618435136, 148.2949999999999591, -9.525000000000000355 ) ) ;
#58160 = CARTESIAN_POINT ( 'NONE',  ( -70.85707362346617799, -5.598654528085803328, -7.705886871421366635 ) ) ;
#58161 = STYLED_ITEM ( 'NONE', ( #30984 ), #66905 ) ;
#58162 = ORIENTED_EDGE ( 'NONE', *, *, #47197, .T. ) ;
#58163 = DIRECTION ( 'NONE',  ( -1.000000000000000000, 0.000000000000000000, 0.000000000000000000 ) ) ;
#58164 = STYLED_ITEM ( 'NONE', ( #62175 ), #58471 ) ;
#58165 = COLOUR_RGB ( '', 0.40784314, 0.44705882, 0.49803922) ;
#58166 = EDGE_CURVE ( 'NONE', #23317, #34747, #69180, .T. ) ;
#58167 = CARTESIAN_POINT ( 'NONE',  ( -112.5549999999999926, 0.000000000000000000, 8.024999999999991473 ) ) ;
#58168 = FILL_AREA_STYLE ('',( #14924 ) ) ;
#58169 = CARTESIAN_POINT ( 'NONE',  ( 0.000000000000000000, 115.4449999999999932, -9.525000000000000355 ) ) ;
#58170 = CARTESIAN_POINT ( 'NONE',  ( -122.0949999999999847, -2.607480562269071545, -8.024999999999991473 ) ) ;
#58171 =( GEOMETRIC_REPRESENTATION_CONTEXT ( 3 ) GLOBAL_UNCERTAINTY_ASSIGNED_CONTEXT ( ( #58748 ) ) GLOBAL_UNIT_ASSIGNED_CONTEXT ( ( #25205, #18866, #29794 ) ) REPRESENTATION_CONTEXT ( 'NONE', 'WORKASPACE' ) );
#58172 = CARTESIAN_POINT ( 'NONE',  ( 31.00000000000000355, 42.47058823529412308, -74.11764705882353610 ) ) ;
#58173 = PLANE ( 'NONE',  #67204 ) ;
#58174 = ORIENTED_EDGE ( 'NONE', *, *, #39727, .T. ) ;
#58175 = CARTESIAN_POINT ( 'NONE',  ( -162.5929263765337964, -3.094860106618431139, -9.524999999999991473 ) ) ;
#58176 = SURFACE_SIDE_STYLE ('',( #52571 ) ) ;
#58177 = CARTESIAN_POINT ( 'NONE',  ( 9.984889265949533410, -0.7056644834263142707, 0.9848892659495224189 ) ) ;
#58178 = PLANE ( 'NONE',  #21995 ) ;
#58179 = CARTESIAN_POINT ( 'NONE',  ( -20.55683252178218723, 114.6388620567782084, -10.28289609742943078 ) ) ;
#58180 = CARTESIAN_POINT ( 'NONE',  ( -53.46164564159121113, -9.867047122144169791, -3.272593290840572600 ) ) ;
#58181 = FACE_OUTER_BOUND ( 'NONE', #29240, .T. ) ;
#58182 = ORIENTED_EDGE ( 'NONE', *, *, #17131, .T. ) ;
#58183 = CARTESIAN_POINT ( 'NONE',  ( -76.79292637653379927, -3.094860106618429807, 9.524999999999991473 ) ) ;
#58184 = DIRECTION ( 'NONE',  ( 0.000000000000000000, 0.000000000000000000, 1.000000000000000000 ) ) ;
#58185 = CARTESIAN_POINT ( 'NONE',  ( -74.08452722063037754, 9.430195807687216103, 6.000000000000000888 ) ) ;
#58186 = DIRECTION ( 'NONE',  ( -0.000000000000000000, 0.000000000000000000, -1.000000000000000000 ) ) ;
#58187 = CARTESIAN_POINT ( 'NONE',  ( -177.5049999999999670, -6.826472737025113702, -4.959722759717900331 ) ) ;
#58188 = ORIENTED_EDGE ( 'NONE', *, *, #32984, .F. ) ;
#58189 = DIRECTION ( 'NONE',  ( -8.673617379884040402E-17, 0.000000000000000000, -1.000000000000000000 ) ) ;
#58190 = CARTESIAN_POINT ( 'NONE',  ( -9.827790563157511022E-16, 137.5570736234661808, 8.025000000000000355 ) ) ;
#58191 = CARTESIAN_POINT ( 'NONE',  ( -105.4429263765338050, -1.166476076187852838E-15, -9.524999999999991473 ) ) ;
#58192 = ORIENTED_EDGE ( 'NONE', *, *, #51295, .F. ) ;
#58193 = CARTESIAN_POINT ( 'NONE',  ( -110.6929263765338050, 10.01517768586948698, -1.839758294383808966E-15 ) ) ;
#58194 = CARTESIAN_POINT ( 'NONE',  ( 54.99999999999999289, 2.409368300552961372E-15, -12.00000000000000000 ) ) ;
#58195 = CARTESIAN_POINT ( 'NONE',  ( 8.437984349512095861, 141.3070736234661524, 1.550032578732817026E-15 ) ) ;
#58196 = ORIENTED_EDGE ( 'NONE', *, *, #12485, .F. ) ;
#58197 = AXIS2_PLACEMENT_3D ( 'NONE', #3339, #51945, #41406 ) ;
#58198 = CARTESIAN_POINT ( 'NONE',  ( -4.250000000000001776, 22.24999999999998579, 4.000000000000000000 ) ) ;
#58199 = CARTESIAN_POINT ( 'NONE',  ( -93.35499999999998977, -4.716976649647093289, -6.492361379858945902 ) ) ;
#58200 = UNCERTAINTY_MEASURE_WITH_UNIT (LENGTH_MEASURE( 1.000000000000000082E-05 ), #13019, 'distance_accuracy_value', 'NONE');
#58201 = MECHANICAL_DESIGN_GEOMETRIC_PRESENTATION_REPRESENTATION (  '', ( #51426 ), #62647 ) ;
#58202 = ORIENTED_EDGE ( 'NONE', *, *, #35110, .F. ) ;
#58203 = CIRCLE ( 'NONE', #39106, 5.000000000000004441 ) ;
#58204 = LINE ( 'NONE', #58901, #27555 ) ;
#58205 = FACE_OUTER_BOUND ( 'NONE', #16261, .T. ) ;
#58206 = DIRECTION ( 'NONE',  ( 0.000000000000000000, 1.000000000000000000, 0.000000000000000000 ) ) ;
#58207 = ADVANCED_FACE ( 'NONE', ( #63320 ), #57345, .F. ) ;
#58208 = EDGE_LOOP ( 'NONE', ( #64692, #8193 ) ) ;
#58209 = CARTESIAN_POINT ( 'NONE',  ( -129.0570736234661808, 0.000000000000000000, 9.524999999999991473 ) ) ;
#58210 = CARTESIAN_POINT ( 'NONE',  ( -74.39499999999999602, -6.826472737025115478, -4.959722759717899443 ) ) ;
#58211 = ORIENTED_EDGE ( 'NONE', *, *, #23434, .T. ) ;
#58212 = SURFACE_STYLE_USAGE ( .BOTH. , #26536 ) ;
#58213 = SURFACE_STYLE_FILL_AREA ( #21611 ) ;
#58214 = CARTESIAN_POINT ( 'NONE',  ( -125.1570736234661751, -9.058813317711329915, -2.943386871421370898 ) ) ;
#58215 = ORIENTED_EDGE ( 'NONE', *, *, #67853, .T. ) ;
#58216 = FACE_OUTER_BOUND ( 'NONE', #9588, .T. ) ;
#58217 = CARTESIAN_POINT ( 'NONE',  ( 52.75000000000000000, 25.24999999999998579, 3.750000000000000000 ) ) ;
#58218 = MECHANICAL_DESIGN_GEOMETRIC_PRESENTATION_REPRESENTATION (  '', ( #33507 ), #1946 ) ;
#58219 = CARTESIAN_POINT ( 'NONE',  ( 86.21825843581743243, 0.000000000000000000, -39.83014742847162637 ) ) ;
#58221 = EDGE_CURVE ( 'NONE', #4254, #51004, #29920, .T. ) ;
#58220 = FACE_OUTER_BOUND ( 'NONE', #1654, .T. ) ;
#58222 = EDGE_LOOP ( 'NONE', ( #3177, #24298, #40291, #27259, #2594 ) ) ;
#58223 = EDGE_CURVE ( 'NONE', #68534, #1034, #14148, .T. ) ;
#58224 = ORIENTED_EDGE ( 'NONE', *, *, #69683, .F. ) ;
#58225 =( NAMED_UNIT ( * ) PLANE_ANGLE_UNIT ( ) SI_UNIT ( $, .RADIAN. ) );
#58226 = DIRECTION ( 'NONE',  ( -0.4834014344018414677, 0.000000000000000000, -0.8753987966739744664 ) ) ;
#58227 = SURFACE_STYLE_FILL_AREA ( #47745 ) ;
#58228 = CARTESIAN_POINT ( 'NONE',  ( -159.2070736234661297, 3.094860106618433360, 9.524999999999991473 ) ) ;
#58229 = ADVANCED_FACE ( 'NONE', ( #10554 ), #16202, .T. ) ;
#58230 = CARTESIAN_POINT ( 'NONE',  ( 3.094860106618431583, 120.0949999999999847, 9.525000000000000355 ) ) ;
#58231 = CARTESIAN_POINT ( 'NONE',  ( -102.9570736234661723, 9.058813317711329915, -2.943386871421373119 ) ) ;
#58232 = EDGE_CURVE ( 'NONE', #65858, #61027, #47901, .T. ) ;
#58233 = DIRECTION ( 'NONE',  ( -1.000000000000000000, -0.000000000000000000, -0.000000000000000000 ) ) ;
#58234 = ORIENTED_EDGE ( 'NONE', *, *, #68020, .F. ) ;
#58235 = CARTESIAN_POINT ( 'NONE',  ( -106.9429263765337907, 0.000000000000000000, 9.524999999999991473 ) ) ;
#58237 = CARTESIAN_POINT ( 'NONE',  ( 66.49999999999998579, 34.24999999999999289, 3.750000000000000000 ) ) ;
#58236 = DIRECTION ( 'NONE',  ( 1.000000000000000000, 0.000000000000000000, 0.000000000000000000 ) ) ;
#58238 = CARTESIAN_POINT ( 'NONE',  ( -71.18918918918917882, 14.09971791521133255, 7.000000000000000000 ) ) ;
#58239 = EDGE_CURVE ( 'NONE', #67189, #47061, #53125, .T. ) ;
#58240 = CARTESIAN_POINT ( 'NONE',  ( -141.0549999999999784, -9.827790563157499189E-16, -8.024999999999991473 ) ) ;
#58241 = FACE_OUTER_BOUND ( 'NONE', #24496, .T. ) ;
#58242 = CARTESIAN_POINT ( 'NONE',  ( -150.5949999999999989, 2.607480562269073321, 8.024999999999991473 ) ) ;
#58243 = AXIS2_PLACEMENT_3D ( 'NONE', #36351, #14867, #58454 ) ;
#58244 = CARTESIAN_POINT ( 'NONE',  ( -140.9949999999999761, -6.826472737025113702, 4.959722759717902107 ) ) ;
#58245 = ORIENTED_EDGE ( 'NONE', *, *, #36998, .T. ) ;
#58246 = AXIS2_PLACEMENT_3D ( 'NONE', #68180, #19624, #20315 ) ;
#58247 = CARTESIAN_POINT ( 'NONE',  ( -180.3570736234661638, 5.598654528085804216, 7.705886871421366635 ) ) ;
#58248 = CARTESIAN_POINT ( 'NONE',  ( 20.74545326270968459, 149.7621816065244218, -9.931116503619028535 ) ) ;
#58249 = CARTESIAN_POINT ( 'NONE',  ( -52.55499999999999261, 0.000000000000000000, 8.024999999999991473 ) ) ;
#58250 = MECHANICAL_DESIGN_GEOMETRIC_PRESENTATION_REPRESENTATION (  '', ( #20017 ), #27880 ) ;
#58251 = CARTESIAN_POINT ( 'NONE',  ( -10.01517768586949231, 153.3050000000000068, -6.132527647946036459E-16 ) ) ;
#58252 = CARTESIAN_POINT ( 'NONE',  ( -52.79292637653378506, -3.094860106618429807, 9.524999999999991473 ) ) ;
#58253 =( NAMED_UNIT ( * ) PLANE_ANGLE_UNIT ( ) SI_UNIT ( $, .RADIAN. ) );
#58254 = VECTOR ( 'NONE', #31417, 1000.000000000000000 ) ;
#58255 = CARTESIAN_POINT ( 'NONE',  ( -6.898093598910797652, -2.361802048420727385, 6.052151411320861207 ) ) ;
#58256 = DIRECTION ( 'NONE',  ( -0.6920792929596435439, 2.191136493437615848E-16, 0.7218214822630869554 ) ) ;
#58257 = STYLED_ITEM ( 'NONE', ( #3033 ), #953 ) ;
#58258 = DIRECTION ( 'NONE',  ( 0.000000000000000000, 0.000000000000000000, 1.000000000000000000 ) ) ;
#58259 = CARTESIAN_POINT ( 'NONE',  ( -82.55707362346618083, -1.166476076187852838E-15, -9.524999999999991473 ) ) ;
#58260 = DIRECTION ( 'NONE',  ( 0.000000000000000000, 0.000000000000000000, 1.000000000000000000 ) ) ;
#58261 = COLOUR_RGB ( '', 0.72549020, 0.75294118, 0.79215686) ;
#58262 = DIRECTION ( 'NONE',  ( -0.000000000000000000, -1.000000000000000000, -0.000000000000000000 ) ) ;
#58263 = CARTESIAN_POINT ( 'NONE',  ( -79.94292637653380496, 0.000000000000000000, 9.524999999999991473 ) ) ;
#58264 = SURFACE_SIDE_STYLE ('',( #59274 ) ) ;
#58265 = EDGE_LOOP ( 'NONE', ( #40173, #53108, #58188, #61459 ) ) ;
#58266 = ORIENTED_EDGE ( 'NONE', *, *, #14455, .T. ) ;
#58267 = DIRECTION ( 'NONE',  ( -0.7071067811865451302, 0.000000000000000000, -0.7071067811865500152 ) ) ;
#58268 = CARTESIAN_POINT ( 'NONE',  ( 7.632228543268608334, 117.4570736234661581, -2.479861379858951942 ) ) ;
#58269 = CIRCLE ( 'NONE', #25722, 18.00000000000000355 ) ;
#58270 = CARTESIAN_POINT ( 'NONE',  ( 35.99999999999999289, 5.000000000000000000, -29.00402776293825724 ) ) ;
#58271 = FACE_OUTER_BOUND ( 'NONE', #2738, .T. ) ;
#58272 = CARTESIAN_POINT ( 'NONE',  ( -76.85707362346616378, -5.598654528085803328, -7.705886871421366635 ) ) ;
#58273 = ORIENTED_EDGE ( 'NONE', *, *, #65103, .T. ) ;
#58275 = ORIENTED_EDGE ( 'NONE', *, *, #64901, .F. ) ;
#58274 = AXIS2_PLACEMENT_3D ( 'NONE', #66176, #2092, #23618 ) ;
#58276 = DIRECTION ( 'NONE',  ( -1.000000000000000000, -0.000000000000000000, -0.000000000000000000 ) ) ;
#58277 = CARTESIAN_POINT ( 'NONE',  ( -20.74545326270968459, 149.7621816065244218, 9.931116503619028535 ) ) ;
#58278 = ORIENTED_EDGE ( 'NONE', *, *, #12870, .T. ) ;
#58279 = CARTESIAN_POINT ( 'NONE',  ( 9.058813317711337021, 121.6549999999999869, 2.943386871421375783 ) ) ;
#58280 = CARTESIAN_POINT ( 'NONE',  ( -85.64292637653379359, -5.598654528085801552, 7.705886871421367523 ) ) ;
#58281 = PLANE ( 'NONE',  #59168 ) ;
#58282 = EDGE_CURVE ( 'NONE', #61550, #65886, #59075, .T. ) ;
#58283 = AXIS2_PLACEMENT_3D ( 'NONE', #59023, #1603, #38299 ) ;
#58284 = DIRECTION ( 'NONE',  ( 1.000000000000000000, 0.000000000000000000, 0.000000000000000000 ) ) ;
#58285 = CARTESIAN_POINT ( 'NONE',  ( -103.4949999999999761, 6.826472737025113702, -4.959722759717902107 ) ) ;
#58286 = ORIENTED_EDGE ( 'NONE', *, *, #7955, .T. ) ;
#58287 = CIRCLE ( 'NONE', #52680, 4.999999999999997335 ) ;
#58288 = ADVANCED_FACE ( 'NONE', ( #16547 ), #42274, .T. ) ;
#58289 = CARTESIAN_POINT ( 'NONE',  ( 5.806870487293831928, 153.9760667166096084, -6.889211357469143593 ) ) ;
#58290 = ORIENTED_EDGE ( 'NONE', *, *, #60241, .T. ) ;
#58291 = CARTESIAN_POINT ( 'NONE',  ( -2.607480562269075097, 157.2929263765338135, 8.025000000000000355 ) ) ;
#58292 =( NAMED_UNIT ( * ) PLANE_ANGLE_UNIT ( ) SI_UNIT ( $, .RADIAN. ) );
#58293 = ADVANCED_FACE ( 'NONE', ( #64353 ), #32123, .T. ) ;
#58294 = AXIS2_PLACEMENT_3D ( 'NONE', #5031, #26482, #48008 ) ;
#58295 = PRESENTATION_STYLE_ASSIGNMENT (( #41116 ) ) ;
#58296 = CARTESIAN_POINT ( 'NONE',  ( -20.94636006565341191, 149.9999999999999716, -9.500000000000000000 ) ) ;
#58297 = DIRECTION ( 'NONE',  ( 1.000000000000000000, 3.011817513800517074E-33, -1.300977106640435384E-16 ) ) ;
#58298 = EDGE_CURVE ( 'NONE', #34398, #36960, #11877, .T. ) ;
#58299 = ORIENTED_EDGE ( 'NONE', *, *, #4379, .F. ) ;
#58300 = CARTESIAN_POINT ( 'NONE',  ( -14.98999599679679662, 117.9999999999999716, 9.500000000000000000 ) ) ;
#58301 = FACE_OUTER_BOUND ( 'NONE', #9264, .T. ) ;
#58303 = MECHANICAL_DESIGN_GEOMETRIC_PRESENTATION_REPRESENTATION (  '', ( #42578 ), #67295 ) ;
#58302 = CARTESIAN_POINT ( 'NONE',  ( -33.66753869681811295, -9.718525487688960851, 3.069079019093872152 ) ) ;
#58304 = DIRECTION ( 'NONE',  ( 0.000000000000000000, 0.000000000000000000, -1.000000000000000000 ) ) ;
#58305 = STYLED_ITEM ( 'NONE', ( #17925 ), #19772 ) ;
#58306 = DIRECTION ( 'NONE',  ( 0.000000000000000000, 0.000000000000000000, 1.000000000000000000 ) ) ;
#58307 = CARTESIAN_POINT ( 'NONE',  ( -74.20353070810536167, 8.974048487541153918, 6.364280603494544941 ) ) ;
#58308 = ADVANCED_FACE ( 'NONE', ( #33045 ), #263, .T. ) ;
#58309 = DIRECTION ( 'NONE',  ( 0.7071067811865352493, 0.000000000000000000, 0.7071067811865597852 ) ) ;
#58310 = LINE ( 'NONE', #47464, #18048 ) ;
#58311 = CARTESIAN_POINT ( 'NONE',  ( -58.75000000000000000, -4.000000000000000000, 18.10000000000000497 ) ) ;
#58312 = VERTEX_POINT ( 'NONE', #33711 ) ;
#58313 = AXIS2_PLACEMENT_3D ( 'NONE', #47840, #16137, #37957 ) ;
#58314 = VERTEX_POINT ( 'NONE', #17241 ) ;
#58315 = SURFACE_STYLE_USAGE ( .BOTH. , #47108 ) ;
#58316 = DIRECTION ( 'NONE',  ( 0.000000000000000000, 0.000000000000000000, 1.000000000000000000 ) ) ;
#58317 = LINE ( 'NONE', #5508, #42476 ) ;
#58318 = VERTEX_POINT ( 'NONE', #55869 ) ;
#58319 = CARTESIAN_POINT ( 'NONE',  ( -169.5549999999999784, 0.000000000000000000, 8.024999999999991473 ) ) ;
#58320 = CARTESIAN_POINT ( 'NONE',  ( -15.75000000000000000, 4.336808689942018722E-16, 20.00000000000000000 ) ) ;
#58321 = CARTESIAN_POINT ( 'NONE',  ( -181.6450000000000102, 4.716976649647091513, -6.492361379858946790 ) ) ;
#58322 = CARTESIAN_POINT ( 'NONE',  ( -166.1949999999999932, 8.437984349512086979, -1.550032578732815448E-15 ) ) ;
#58323 = ORIENTED_EDGE ( 'NONE', *, *, #67094, .T. ) ;
#58324 = CARTESIAN_POINT ( 'NONE',  ( 10.00000000000001954, 42.00000000000000000, -35.50000000000000000 ) ) ;
#58325 =( NAMED_UNIT ( * ) PLANE_ANGLE_UNIT ( ) SI_UNIT ( $, .RADIAN. ) );
#58326 = CARTESIAN_POINT ( 'NONE',  ( -14.83546612668997433, 10.90871211463571022, -5.000000000000001776 ) ) ;
#58327 = CARTESIAN_POINT ( 'NONE',  ( -83.00499999999995282, 6.826472737025116366, 4.959722759717898555 ) ) ;
#58328 = CARTESIAN_POINT ( 'NONE',  ( 34.99999999999999289, 99.99999999999998579, -9.500000000000000000 ) ) ;
#58329 = CARTESIAN_POINT ( 'NONE',  ( -168.0570736234661808, 0.000000000000000000, 9.524999999999991473 ) ) ;
#58330 =( LENGTH_UNIT ( ) NAMED_UNIT ( * ) SI_UNIT ( .MILLI., .METRE. ) );
#58331 = AXIS2_PLACEMENT_3D ( 'NONE', #21996, #32190, #42447 ) ;
#58332 = CARTESIAN_POINT ( 'NONE',  ( -94.94499999999999318, -9.827790563157499189E-16, -8.024999999999991473 ) ) ;
#58333 = CARTESIAN_POINT ( 'NONE',  ( -5.598654528085808657, 126.7549999999999812, 7.705886871421373741 ) ) ;
#58334 = DIRECTION ( 'NONE',  ( 0.000000000000000000, 0.000000000000000000, -1.000000000000000000 ) ) ;
#58335 = AXIS2_PLACEMENT_3D ( 'NONE', #38620, #48472, #55074 ) ;
#58336 = CARTESIAN_POINT ( 'NONE',  ( 8.082903768654761123, 2.500000000000000000, 9.511133375893962597E-16 ) ) ;
#58337 = AXIS2_PLACEMENT_3D ( 'NONE', #5731, #10358, #58885 ) ;
#58338 = STYLED_ITEM ( 'NONE', ( #16649 ), #4931 ) ;
#58339 = EDGE_CURVE ( 'NONE', #14152, #44124, #65734, .T. ) ;
#58340 = AXIS2_PLACEMENT_3D ( 'NONE', #17717, #50404, #38853 ) ;
#58341 = ORIENTED_EDGE ( 'NONE', *, *, #67674, .F. ) ;
#58342 = CARTESIAN_POINT ( 'NONE',  ( -4.250000000000001776, 22.24999999999998579, 3.750000000000000000 ) ) ;
#58343 =( NAMED_UNIT ( * ) PLANE_ANGLE_UNIT ( ) SI_UNIT ( $, .RADIAN. ) );
#58345 = CARTESIAN_POINT ( 'NONE',  ( -195.0000000000000000, 1.166476076187852838E-15, -9.524999999999991473 ) ) ;
#58344 = DIRECTION ( 'NONE',  ( 0.000000000000000000, -1.000000000000000000, 0.000000000000000000 ) ) ;
#58346 = CARTESIAN_POINT ( 'NONE',  ( -17.41962728626436530, -0.1139526552317604857, 2.000000000000000000 ) ) ;
#58347 = ORIENTED_EDGE ( 'NONE', *, *, #66978, .F. ) ;
#58348 =( GEOMETRIC_REPRESENTATION_CONTEXT ( 3 ) GLOBAL_UNCERTAINTY_ASSIGNED_CONTEXT ( ( #17254 ) ) GLOBAL_UNIT_ASSIGNED_CONTEXT ( ( #58853, #54249, #64478 ) ) REPRESENTATION_CONTEXT ( 'NONE', 'WORKASPACE' ) );
#58349 = EDGE_LOOP ( 'NONE', ( #25799, #29074, #37071, #42016 ) ) ;
#58350 = DIRECTION ( 'NONE',  ( -1.000000000000000000, 0.000000000000000000, 0.000000000000000000 ) ) ;
#58351 = MECHANICAL_DESIGN_GEOMETRIC_PRESENTATION_REPRESENTATION (  '', ( #66226 ), #25763 ) ;
#58352 = CARTESIAN_POINT ( 'NONE',  ( -7.632228543268608334, 147.8429263765338249, 2.479861379858952830 ) ) ;
#58353 = PRESENTATION_STYLE_ASSIGNMENT (( #15479 ) ) ;
#58354 = AXIS2_PLACEMENT_3D ( 'NONE', #10413, #5434, #52637 ) ;
#58355 = ORIENTED_EDGE ( 'NONE', *, *, #49800, .F. ) ;
#58356 = CARTESIAN_POINT ( 'NONE',  ( -124.5549999999999926, 0.000000000000000000, 8.024999999999991473 ) ) ;
#58358 = EDGE_CURVE ( 'NONE', #31013, #53539, #51206, .T. ) ;
#58357 = ORIENTED_EDGE ( 'NONE', *, *, #67281, .T. ) ;
#58359 = CARTESIAN_POINT ( 'NONE',  ( -137.7570736234661695, -5.598654528085801552, 7.705886871421367523 ) ) ;
#58360 = CARTESIAN_POINT ( 'NONE',  ( 4.716976649647099507, 129.7570736234661695, -6.492361379858953008 ) ) ;
#58361 = EDGE_CURVE ( 'NONE', #41081, #3021, #55161, .T. ) ;
#58362 = ORIENTED_EDGE ( 'NONE', *, *, #34871, .F. ) ;
#58363 = SURFACE_STYLE_USAGE ( .BOTH. , #47525 ) ;
#58364 = DIRECTION ( 'NONE',  ( -0.000000000000000000, 1.000000000000000000, -0.000000000000000000 ) ) ;
#58365 = ORIENTED_EDGE ( 'NONE', *, *, #28585, .F. ) ;
#58366 =( GEOMETRIC_REPRESENTATION_CONTEXT ( 3 ) GLOBAL_UNCERTAINTY_ASSIGNED_CONTEXT ( ( #61391 ) ) GLOBAL_UNIT_ASSIGNED_CONTEXT ( ( #60699, #1216, #38961 ) ) REPRESENTATION_CONTEXT ( 'NONE', 'WORKASPACE' ) );
#58367 = CIRCLE ( 'NONE', #61704, 26.99999999999999645 ) ;
#58368 = CARTESIAN_POINT ( 'NONE',  ( -3.094860106618434248, 149.7949999999999875, 9.525000000000000355 ) ) ;
#58369 =( NAMED_UNIT ( * ) SI_UNIT ( $, .STERADIAN. ) SOLID_ANGLE_UNIT ( ) );
#58370 = EDGE_CURVE ( 'NONE', #21095, #55864, #39043, .T. ) ;
#58371 = ORIENTED_EDGE ( 'NONE', *, *, #31270, .T. ) ;
#58372 = DIRECTION ( 'NONE',  ( -1.000000000000000000, 0.000000000000000000, 0.000000000000000000 ) ) ;
#58373 = CARTESIAN_POINT ( 'NONE',  ( -8.102448949553179958, 153.6049999999999898, 5.886773742842747126 ) ) ;
#58374 = CARTESIAN_POINT ( 'NONE',  ( -136.4070736234667720, 3.094860106608949835, -9.525000000006881962 ) ) ;
#58375 = VECTOR ( 'NONE', #32365, 1000.000000000000000 ) ;
#58376 = LINE ( 'NONE', #38001, #29618 ) ;
#58377 = EDGE_LOOP ( 'NONE', ( #13290, #50238, #50670 ) ) ;
#58378 = CARTESIAN_POINT ( 'NONE',  ( -8.437984349512095861, 123.6929263765338192, -5.166775262442723748E-16 ) ) ;
#58379 = DIRECTION ( 'NONE',  ( -1.000000000000000000, 0.000000000000000000, 0.000000000000000000 ) ) ;
#58380 = DIRECTION ( 'NONE',  ( -0.000000000000000000, -0.000000000000000000, -1.000000000000000000 ) ) ;
#58381 = PRESENTATION_STYLE_ASSIGNMENT (( #20401 ) ) ;
#58382 = SURFACE_SIDE_STYLE ('',( #47544 ) ) ;
#58383 = EDGE_LOOP ( 'NONE', ( #45222, #21133, #3015 ) ) ;
#58384 = DIRECTION ( 'NONE',  ( -1.156482317317873451E-16, -1.000000000000000000, 0.000000000000000000 ) ) ;
#58385 = ADVANCED_FACE ( 'NONE', ( #66422 ), #66783, .F. ) ;
#58386 = EDGE_LOOP ( 'NONE', ( #56625, #45440, #59866, #13031 ) ) ;
#58387 = CARTESIAN_POINT ( 'NONE',  ( -55.94292637653380496, 0.000000000000000000, 9.524999999999991473 ) ) ;
#58388 = MECHANICAL_DESIGN_GEOMETRIC_PRESENTATION_REPRESENTATION (  '', ( #43818 ), #68485 ) ;
#58389 = PLANE ( 'NONE',  #17703 ) ;
#58390 = DIRECTION ( 'NONE',  ( 0.000000000000000000, 0.000000000000000000, -1.000000000000000000 ) ) ;
#58391 = CARTESIAN_POINT ( 'NONE',  ( -153.5049999999999670, -6.826472737025115478, -4.959722759717899443 ) ) ;
#58392 =( GEOMETRIC_REPRESENTATION_CONTEXT ( 3 ) GLOBAL_UNCERTAINTY_ASSIGNED_CONTEXT ( ( #23595 ) ) GLOBAL_UNIT_ASSIGNED_CONTEXT ( ( #58794, #32060, #11289 ) ) REPRESENTATION_CONTEXT ( 'NONE', 'WORKASPACE' ) );
#58393 =( NAMED_UNIT ( * ) PLANE_ANGLE_UNIT ( ) SI_UNIT ( $, .RADIAN. ) );
#58394 = CARTESIAN_POINT ( 'NONE',  ( -6.062177826491072175, -3.499999999999998668, 0.000000000000000000 ) ) ;
#58396 = EDGE_CURVE ( 'NONE', #60291, #47340, #52326, .T. ) ;
#58395 = TOROIDAL_SURFACE ( 'NONE', #28026, 26.49999999999999645, 0.5000000000000000000 ) ;
#58397 = PRESENTATION_STYLE_ASSIGNMENT (( #63672 ) ) ;
#58398 = FILL_AREA_STYLE_COLOUR ( '', #67405 ) ;
#58399 = DIRECTION ( 'NONE',  ( 0.000000000000000000, -1.000000000000000000, 0.000000000000000000 ) ) ;
#58400 = VERTEX_POINT ( 'NONE', #34415 ) ;
#58401 = STYLED_ITEM ( 'NONE', ( #52056 ), #51511 ) ;
#58402 = VERTEX_POINT ( 'NONE', #65393 ) ;
#58403 = FACE_OUTER_BOUND ( 'NONE', #50762, .T. ) ;
#58404 = DIRECTION ( 'NONE',  ( 0.000000000000000000, 0.000000000000000000, 1.000000000000000000 ) ) ;
#58405 = CARTESIAN_POINT ( 'NONE',  ( -70.70499999999996987, 2.607480562269073321, 8.024999999999991473 ) ) ;
#58406 = ORIENTED_EDGE ( 'NONE', *, *, #60215, .F. ) ;
#58407 = DIRECTION ( 'NONE',  ( 1.000000000000000000, 2.168404344971008868E-16, 0.000000000000000000 ) ) ;
#58408 = PLANE ( 'NONE',  #34845 ) ;
#58409 = DIRECTION ( 'NONE',  ( -1.000000000000000000, 0.000000000000000000, 0.000000000000000000 ) ) ;
#58410 = DIRECTION ( 'NONE',  ( -0.3420201433256663814, 0.9396926207859092051, 0.000000000000000000 ) ) ;
#58411 = CARTESIAN_POINT ( 'NONE',  ( 98.00000000000000000, 16.00000000000000000, 12.50000000000000178 ) ) ;
#58412 = AXIS2_PLACEMENT_3D ( 'NONE', #52825, #69000, #48615 ) ;
#58413 = VERTEX_POINT ( 'NONE', #22482 ) ;
#58414 = CYLINDRICAL_SURFACE ( 'NONE', #60469, 0.2500000000000002220 ) ;
#58415 = CARTESIAN_POINT ( 'NONE',  ( 1.804495846578303864, 51.08602766979955589, -7.112547338523483198 ) ) ;
#58416 = CARTESIAN_POINT ( 'NONE',  ( -71.18918918918917882, 14.09971791521133255, 9.500000000000000000 ) ) ;
#58417 = VECTOR ( 'NONE', #4307, 1000.000000000000000 ) ;
#58419 = CARTESIAN_POINT ( 'NONE',  ( -74.50000000000000000, -2.208799022165584366E-14, -10.00000000000000000 ) ) ;
#58418 = LINE ( 'NONE', #68637, #18856 ) ;
#58420 = CARTESIAN_POINT ( 'NONE',  ( -121.6449999999999960, 4.716976649647091513, -6.492361379858946790 ) ) ;
#58421 = CARTESIAN_POINT ( 'NONE',  ( 5.598654528085809545, 145.1450000000000102, -7.705886871421373741 ) ) ;
#58422 = CARTESIAN_POINT ( 'NONE',  ( -84.59499999999998465, 2.607480562269073321, 8.024999999999991473 ) ) ;
#58423 = DIRECTION ( 'NONE',  ( -0.000000000000000000, -0.000000000000000000, 1.000000000000000000 ) ) ;
#58424 = VECTOR ( 'NONE', #6813, 1000.000000000000114 ) ;
#58425 = PRESENTATION_LAYER_ASSIGNMENT (  '', '', ( #19083 ) ) ;
#58426 =( BOUNDED_CURVE ( )  B_SPLINE_CURVE ( 2, ( #53956, #10721, #47356, #21248, #26538, #59223, #58214, #53300, #14984, #63494, #31460 ),
 .UNSPECIFIED., .F., .F. ) 
 B_SPLINE_CURVE_WITH_KNOTS ( ( 3, 2, 2, 2, 2, 3 ),
 ( 0.4130434782608597977, 0.4152173913043379905, 0.4173913043478162388, 0.4195652173912944871, 0.4217391304347727354, 0.4239130434782509282 ),
 .UNSPECIFIED. ) 
 CURVE ( )  GEOMETRIC_REPRESENTATION_ITEM ( )  RATIONAL_B_SPLINE_CURVE ( ( 1.000000000000220046, 0.9510565162949335960, 1.000000000000000000, 0.9510565162951535312, 1.000000000000000000, 0.9510565162951535312, 1.000000000000000000, 0.9510565162951535312, 1.000000000000000000, 0.9510565162953772411, 0.9999999999997762901 ) ) 
 REPRESENTATION_ITEM ( '' )  );
#58427 = EDGE_CURVE ( 'NONE', #61023, #60866, #9654, .T. ) ;
#58428 = CYLINDRICAL_SURFACE ( 'NONE', #51689, 0.5000000000000004441 ) ;
#58430 = ORIENTED_EDGE ( 'NONE', *, *, #53298, .T. ) ;
#58429 = CIRCLE ( 'NONE', #53939, 5.000000000000004441 ) ;
#58431 = CARTESIAN_POINT ( 'NONE',  ( -136.6429263765338078, -5.598654528085801552, 7.705886871421367523 ) ) ;
#58432 = LINE ( 'NONE', #53172, #1716 ) ;
#58433 = CARTESIAN_POINT ( 'NONE',  ( -157.9449999999999932, -9.827790563157499189E-16, -8.024999999999991473 ) ) ;
#58434 = SURFACE_STYLE_FILL_AREA ( #21848 ) ;
#58435 = AXIS2_PLACEMENT_3D ( 'NONE', #49598, #43332, #7016 ) ;
#58436 = DIRECTION ( 'NONE',  ( 1.000000000000000000, 0.000000000000000000, 0.000000000000000000 ) ) ;
#58437 = EDGE_LOOP ( 'NONE', ( #13062, #12093, #18891, #44836 ) ) ;
#58438 = ORIENTED_EDGE ( 'NONE', *, *, #19549, .F. ) ;
#58439 =( GEOMETRIC_REPRESENTATION_CONTEXT ( 3 ) GLOBAL_UNCERTAINTY_ASSIGNED_CONTEXT ( ( #59489 ) ) GLOBAL_UNIT_ASSIGNED_CONTEXT ( ( #5556, #37652, #54104 ) ) REPRESENTATION_CONTEXT ( 'NONE', 'WORKASPACE' ) );
#58440 = DIRECTION ( 'NONE',  ( 0.000000000000000000, 0.000000000000000000, 1.000000000000000000 ) ) ;
#58441 = PRODUCT_RELATED_PRODUCT_CATEGORY ( 'part', '', ( #32768 ) ) ;
#58442 = EDGE_CURVE ( 'NONE', #28999, #40918, #53994, .T. ) ;
#58443 = VECTOR ( 'NONE', #51260, 1000.000000000000000 ) ;
#58444 = EDGE_CURVE ( 'NONE', #60451, #17311, #5301, .T. ) ;
#58445 = CARTESIAN_POINT ( 'NONE',  ( -9.827790563157511022E-16, 118.4429263765338192, 8.025000000000000355 ) ) ;
#58446 = CARTESIAN_POINT ( 'NONE',  ( -6.062177826491072175, -3.499999999999998668, 0.000000000000000000 ) ) ;
#58447 = CARTESIAN_POINT ( 'NONE',  ( -59.39292637653377938, 8.102448949553176405, 5.886773742842740909 ) ) ;
#58448 =( GEOMETRIC_REPRESENTATION_CONTEXT ( 3 ) GLOBAL_UNCERTAINTY_ASSIGNED_CONTEXT ( ( #68646 ) ) GLOBAL_UNIT_ASSIGNED_CONTEXT ( ( #67084, #56517, #3001 ) ) REPRESENTATION_CONTEXT ( 'NONE', 'WORKASPACE' ) );
#58449 = VERTEX_POINT ( 'NONE', #13289 ) ;
#58450 = CARTESIAN_POINT ( 'NONE',  ( -154.7049999999999841, 2.607480562269072433, 8.024999999999991473 ) ) ;
#58451 = ADVANCED_FACE ( 'NONE', ( #1982 ), #17899, .T. ) ;
#58452 = EDGE_CURVE ( 'NONE', #29727, #60346, #8693, .T. ) ;
#58453 = ORIENTED_EDGE ( 'NONE', *, *, #63772, .T. ) ;
#58454 = DIRECTION ( 'NONE',  ( 0.000000000000000000, 0.000000000000000000, 1.000000000000000000 ) ) ;
#58455 = DIRECTION ( 'NONE',  ( -1.000000000000000000, 0.000000000000000000, 0.000000000000000000 ) ) ;
#58456 = ORIENTED_EDGE ( 'NONE', *, *, #69275, .F. ) ;
#58457 = AXIS2_PLACEMENT_3D ( 'NONE', #2767, #19320, #36240 ) ;
#58458 = AXIS2_PLACEMENT_3D ( 'NONE', #22521, #38741, #22171 ) ;
#58459 = LINE ( 'NONE', #10282, #24132 ) ;
#58460 = CARTESIAN_POINT ( 'NONE',  ( 5.598654528085805993, 123.2449999999999903, 7.705886871421374629 ) ) ;
#58461 = DIRECTION ( 'NONE',  ( -1.000000000000000000, 0.000000000000000000, 0.000000000000000000 ) ) ;
#58462 = ORIENTED_EDGE ( 'NONE', *, *, #63368, .F. ) ;
#58464 = EDGE_CURVE ( 'NONE', #68782, #49817, #67134, .T. ) ;
#58463 = CARTESIAN_POINT ( 'NONE',  ( -8.102448949553179958, 123.0049999999999955, -5.886773742842749790 ) ) ;
#58465 = CARTESIAN_POINT ( 'NONE',  ( -64.40499999999998693, -2.607480562269069768, 8.024999999999991473 ) ) ;
#58466 = CARTESIAN_POINT ( 'NONE',  ( -60.00000000000000000, -2.024042244987997205E-14, 6.999999999999995559 ) ) ;
#58467 = ORIENTED_EDGE ( 'NONE', *, *, #59974, .T. ) ;
#58468 = CARTESIAN_POINT ( 'NONE',  ( 9.058813317711338797, 151.9550000000000125, -2.943386871421372675 ) ) ;
#58469 = AXIS2_PLACEMENT_3D ( 'NONE', #14298, #63185, #15026 ) ;
#58470 = SURFACE_STYLE_FILL_AREA ( #8893 ) ;
#58471 = ADVANCED_FACE ( 'NONE', ( #1305 ), #7578, .F. ) ;
#58472 = CARTESIAN_POINT ( 'NONE',  ( 20.71462257042833599, 114.4999999999999574, 10.00000000000000000 ) ) ;
#58473 = DIRECTION ( 'NONE',  ( 0.000000000000000000, 1.000000000000000000, 0.000000000000000000 ) ) ;
#58474 = CARTESIAN_POINT ( 'NONE',  ( 44.99999999999998579, 119.9999999999999716, 7.500000000000000000 ) ) ;
#58475 = ORIENTED_EDGE ( 'NONE', *, *, #48343, .F. ) ;
#58476 = SURFACE_SIDE_STYLE ('',( #26778 ) ) ;
#58478 = CARTESIAN_POINT ( 'NONE',  ( -183.0550000000000068, -9.827790563157499189E-16, -8.024999999999991473 ) ) ;
#58477 = VECTOR ( 'NONE', #10480, 1000.000000000000000 ) ;
#58479 = ORIENTED_EDGE ( 'NONE', *, *, #4944, .F. ) ;
#58480 = DIRECTION ( 'NONE',  ( -7.816271194327172234E-17, -0.000000000000000000, -1.000000000000000000 ) ) ;
#58481 = FILL_AREA_STYLE_COLOUR ( '', #15550 ) ;
#58482 = PRESENTATION_LAYER_ASSIGNMENT (  '', '', ( #9075 ) ) ;
#58483 = AXIS2_PLACEMENT_3D ( 'NONE', #50721, #3887, #29602 ) ;
#58484 = CARTESIAN_POINT ( 'NONE',  ( 28.00000000000002842, 43.00000000000000000, 79.00402776293826435 ) ) ;
#58485 = VERTEX_POINT ( 'NONE', #44336 ) ;
#58486 = SURFACE_SIDE_STYLE ('',( #48669 ) ) ;
#58487 = DIRECTION ( 'NONE',  ( -1.000000000000000000, -0.000000000000000000, -0.000000000000000000 ) ) ;
#58488 = ORIENTED_EDGE ( 'NONE', *, *, #4174, .T. ) ;
#58489 = DIRECTION ( 'NONE',  ( -0.000000000000000000, -0.000000000000000000, -1.000000000000000000 ) ) ;
#58490 = CARTESIAN_POINT ( 'NONE',  ( -98.30499999999997840, 8.437984349512085203, -1.550032578732815448E-15 ) ) ;
#58491 = ORIENTED_EDGE ( 'NONE', *, *, #53084, .F. ) ;
#58492 = MECHANICAL_DESIGN_GEOMETRIC_PRESENTATION_REPRESENTATION (  '', ( #29245 ), #32659 ) ;
#58493 = CARTESIAN_POINT ( 'NONE',  ( -134.3070736234661240, -10.01517768586948698, 6.132527647946031529E-16 ) ) ;
#58494 = EDGE_CURVE ( 'NONE', #9170, #29261, #61483, .T. ) ;
#58495 =( NAMED_UNIT ( * ) PLANE_ANGLE_UNIT ( ) SI_UNIT ( $, .RADIAN. ) );
#58496 = CARTESIAN_POINT ( 'NONE',  ( -5.598654528085808657, 149.6450000000000102, 7.705886871421373741 ) ) ;
#58497 = CARTESIAN_POINT ( 'NONE',  ( -62.00707362346618368, -8.102448949553172852, -5.886773742842741797 ) ) ;
#58498 = TOROIDAL_SURFACE ( 'NONE', #36179, 0.5000000000000000000, 0.2500000000000000000 ) ;
#58499 = CARTESIAN_POINT ( 'NONE',  ( -71.75000000000000000, -0.9999999999999995559, 24.00000000000000000 ) ) ;
#58500 = EDGE_LOOP ( 'NONE', ( #5565, #13866, #11491, #4891 ) ) ;
#58501 =( NAMED_UNIT ( * ) PLANE_ANGLE_UNIT ( ) SI_UNIT ( $, .RADIAN. ) );
#58502 = AXIS2_PLACEMENT_3D ( 'NONE', #58883, #16350, #36433 ) ;
#58503 = CYLINDRICAL_SURFACE ( 'NONE', #41514, 5.000000000000004441 ) ;
#58504 = DIRECTION ( 'NONE',  ( -1.000000000000000000, -0.000000000000000000, -0.000000000000000000 ) ) ;
#58505 = CARTESIAN_POINT ( 'NONE',  ( -113.7549999999999955, 4.716976649647091513, -6.492361379858946790 ) ) ;
#58506 = CARTESIAN_POINT ( 'NONE',  ( 5.598654528085809545, 121.1449999999999818, -7.705886871421373741 ) ) ;
#58507 = CARTESIAN_POINT ( 'NONE',  ( -127.7949999999999875, 2.607480562269068880, -8.024999999999993250 ) ) ;
#58508 = COLOUR_RGB ( '', 0.31764706, 0.68627451, 0.89019608) ;
#58509 = CONICAL_SURFACE ( 'NONE', #22558, 8.025000000000000355, 0.7853981633974491672 ) ;
#58510 = ORIENTED_EDGE ( 'NONE', *, *, #29451, .T. ) ;
#58511 = CARTESIAN_POINT ( 'NONE',  ( -160.6429263765338362, -5.598654528085801552, 7.705886871421367523 ) ) ;
#58512 = SHAPE_REPRESENTATION_RELATIONSHIP ( 'NONE' , 'NONE' ,  #14155, #6101 ) ;
#58513 = COLOUR_RGB ( '', 0.72549020, 0.75294118, 0.79215686) ;
#58514 = DIRECTION ( 'NONE',  ( 1.300977106640434891E-16, 0.000000000000000000, 1.000000000000000000 ) ) ;
#58515 = DIRECTION ( 'NONE',  ( -1.000000000000000000, -0.000000000000000000, -0.000000000000000000 ) ) ;
#58516 = DIRECTION ( 'NONE',  ( -1.000000000000000000, 0.000000000000000000, -0.000000000000000000 ) ) ;
#58517 =( LENGTH_UNIT ( ) NAMED_UNIT ( * ) SI_UNIT ( .MILLI., .METRE. ) );
#58518 = SURFACE_STYLE_USAGE ( .BOTH. , #25464 ) ;
#58519 = EDGE_LOOP ( 'NONE', ( #37583, #58988, #20103, #60795 ) ) ;
#58520 = CIRCLE ( 'NONE', #18104, 0.2500000000000002220 ) ;
#58521 = CARTESIAN_POINT ( 'NONE',  ( -71.84292637653381064, 9.058813317711329915, -2.943386871421373119 ) ) ;
#58522 = CARTESIAN_POINT ( 'NONE',  ( 71.49999999999998579, 64.07124727947029896, 7.500000000000000000 ) ) ;
#58523 =( BOUNDED_CURVE ( )  B_SPLINE_CURVE ( 3, ( #52783, #52101, #14799, #36639 ),
 .UNSPECIFIED., .F., .F. ) 
 B_SPLINE_CURVE_WITH_KNOTS ( ( 4, 4 ),
 ( 1.570796326794896558, 3.141592653589793116 ),
 .UNSPECIFIED. ) 
 CURVE ( )  GEOMETRIC_REPRESENTATION_ITEM ( )  RATIONAL_B_SPLINE_CURVE ( ( 1.000000000000000000, 0.8047378541243649375, 0.8047378541243649375, 1.000000000000000000 ) ) 
 REPRESENTATION_ITEM ( '' )  );
#58524 = AXIS2_PLACEMENT_3D ( 'NONE', #23250, #28848, #34487 ) ;
#58525 = ADVANCED_FACE ( 'NONE', ( #67822, #29478 ), #52355, .T. ) ;
#58526 = DIRECTION ( 'NONE',  ( 0.000000000000000000, 0.000000000000000000, -1.000000000000000000 ) ) ;
#58527 = DIRECTION ( 'NONE',  ( 0.000000000000000000, 0.000000000000000000, -1.000000000000000000 ) ) ;
#58528 = DIRECTION ( 'NONE',  ( 0.6402681315062906942, 0.000000000000000000, -0.7681514953298230752 ) ) ;
#58529 = CARTESIAN_POINT ( 'NONE',  ( -181.1049999999999898, -6.826472737025113702, 4.959722759717902107 ) ) ;
#58530 = EDGE_CURVE ( 'NONE', #11115, #47453, #51293, .T. ) ;
#58531 = ORIENTED_EDGE ( 'NONE', *, *, #36259, .T. ) ;
#58532 = PRESENTATION_STYLE_ASSIGNMENT (( #16689 ) ) ;
#58533 = MECHANICAL_DESIGN_GEOMETRIC_PRESENTATION_REPRESENTATION (  '', ( #2317 ), #68692 ) ;
#58534 = DIRECTION ( 'NONE',  ( 1.000000000000000000, -0.000000000000000000, 0.000000000000000000 ) ) ;
#58535 = DIRECTION ( 'NONE',  ( -0.000000000000000000, 1.000000000000000000, -0.000000000000000000 ) ) ;
#58536 = AXIS2_PLACEMENT_3D ( 'NONE', #60497, #8704, #62145 ) ;
#58537 = DIRECTION ( 'NONE',  ( 1.000000000000000000, 0.000000000000000000, 0.000000000000000000 ) ) ;
#58538 = CARTESIAN_POINT ( 'NONE',  ( 6.826472737025119919, 141.0070736234661695, 4.959722759717908325 ) ) ;
#58539 = STYLED_ITEM ( 'NONE', ( #48878 ), #53616 ) ;
#58540 = VERTEX_POINT ( 'NONE', #19954 ) ;
#58541 = CARTESIAN_POINT ( 'NONE',  ( 2.999999999999993339, 0.000000000000000000, 24.00402776293822882 ) ) ;
#58542 = CARTESIAN_POINT ( 'NONE',  ( -89.30499999999997840, 8.437984349512086979, -1.550032578732815448E-15 ) ) ;
#58543 = AXIS2_PLACEMENT_3D ( 'NONE', #47245, #20464, #41968 ) ;
#58544 = EDGE_LOOP ( 'NONE', ( #26035, #18601, #29160, #14321 ) ) ;
#58545 = CARTESIAN_POINT ( 'NONE',  ( 1.802043943559349604, -2.359472279213374435, -9.000000000000007105 ) ) ;
#58546 = EDGE_CURVE ( 'NONE', #41012, #8636, #3392, .T. ) ;
#58547 = CARTESIAN_POINT ( 'NONE',  ( 6.826472737025119919, 142.8929263765338078, 4.959722759717908325 ) ) ;
#58548 =( NAMED_UNIT ( * ) PLANE_ANGLE_UNIT ( ) SI_UNIT ( $, .RADIAN. ) );
#58549 = CARTESIAN_POINT ( 'NONE',  ( 28.58578643762690419, 34.36176364315825538, -80.00402776293826435 ) ) ;
#58550 = ORIENTED_EDGE ( 'NONE', *, *, #52216, .T. ) ;
#58551 = CYLINDRICAL_SURFACE ( 'NONE', #27210, 1.000000000000000888 ) ;
#58552 = CARTESIAN_POINT ( 'NONE',  ( -72.14499999999998181, -4.716976649647092401, 6.492361379858946790 ) ) ;
#58553 = ORIENTED_EDGE ( 'NONE', *, *, #48686, .T. ) ;
#58554 = MECHANICAL_DESIGN_GEOMETRIC_PRESENTATION_REPRESENTATION (  '', ( #15902 ), #54074 ) ;
#58555 = CARTESIAN_POINT ( 'NONE',  ( -9.827790563157511022E-16, 142.4429263765338192, 8.025000000000000355 ) ) ;
#58556 = DIRECTION ( 'NONE',  ( -0.000000000000000000, -0.000000000000000000, 1.000000000000000000 ) ) ;
#58557 = FILL_AREA_STYLE_COLOUR ( '', #46558 ) ;
#58558 = EDGE_LOOP ( 'NONE', ( #41436, #39234, #64917, #49936 ) ) ;
#58559 = FILL_AREA_STYLE ('',( #37150 ) ) ;
#58560 = CARTESIAN_POINT ( 'NONE',  ( -21.02379604162863913, 110.4999999999999858, -10.50000000000000000 ) ) ;
#58561 = COLOUR_RGB ( '', 0.40784314, 0.44705882, 0.49803922) ;
#58562 = VECTOR ( 'NONE', #35573, 1000.000000000000000 ) ;
#58563 =( NAMED_UNIT ( * ) SI_UNIT ( $, .STERADIAN. ) SOLID_ANGLE_UNIT ( ) );
#58564 = VERTEX_POINT ( 'NONE', #29826 ) ;
#58565 = DIRECTION ( 'NONE',  ( 0.000000000000000000, 0.000000000000000000, 1.000000000000000000 ) ) ;
#58566 = ORIENTED_EDGE ( 'NONE', *, *, #19941, .T. ) ;
#58567 = DIRECTION ( 'NONE',  ( 0.000000000000000000, 0.000000000000000000, 1.000000000000000000 ) ) ;
#58568 = DIRECTION ( 'NONE',  ( 1.387778780781445676E-15, 0.000000000000000000, 1.000000000000000000 ) ) ;
#58569 = DIRECTION ( 'NONE',  ( -0.000000000000000000, 1.000000000000000000, -0.000000000000000000 ) ) ;
#58570 = CARTESIAN_POINT ( 'NONE',  ( -160.1070736234661922, 8.102448949553171076, -5.886773742842744461 ) ) ;
#58571 = PRESENTATION_LAYER_ASSIGNMENT (  '', '', ( #23721 ) ) ;
#58572 = EDGE_CURVE ( 'NONE', #39293, #35271, #4106, .T. ) ;
#58573 = CARTESIAN_POINT ( 'NONE',  ( -1.166476076187854022E-15, 122.9449999999999790, 9.525000000000000355 ) ) ;
#58574 = CARTESIAN_POINT ( 'NONE',  ( -93.50707362346618368, 8.102448949553176405, 5.886773742842740909 ) ) ;
#58575 = STYLED_ITEM ( 'NONE', ( #64607 ), #45568 ) ;
#58576 = STYLED_ITEM ( 'NONE', ( #66020 ), #12527 ) ;
#58577 = PRODUCT_DEFINITION_SHAPE ( 'NONE', 'NONE',  #53296 ) ;
#58578 = ORIENTED_EDGE ( 'NONE', *, *, #31765, .F. ) ;
#58580 = CIRCLE ( 'NONE', #55201, 0.2500000000000002220 ) ;
#58579 = DIRECTION ( 'NONE',  ( -1.000000000000000000, 0.000000000000000000, 0.000000000000000000 ) ) ;
#58581 = CARTESIAN_POINT ( 'NONE',  ( -6.826472737025120807, 131.1070736234661638, 4.959722759717906548 ) ) ;
#58582 = CARTESIAN_POINT ( 'NONE',  ( -144.3549999999999898, -4.716976649647093289, -6.492361379858945902 ) ) ;
#58583 = SURFACE_STYLE_FILL_AREA ( #16408 ) ;
#58584 = FACE_OUTER_BOUND ( 'NONE', #41798, .T. ) ;
#58585 = AXIS2_PLACEMENT_3D ( 'NONE', #68233, #47514, #68931 ) ;
#58586 = CARTESIAN_POINT ( 'NONE',  ( -155.3950000000000102, -6.826472737025115478, -4.959722759717899443 ) ) ;
#58587 = CARTESIAN_POINT ( 'NONE',  ( -140.0949999999999989, -2.607480562269071545, -8.024999999999991473 ) ) ;
#58588 = VECTOR ( 'NONE', #59647, 1000.000000000000000 ) ;
#58589 = EDGE_LOOP ( 'NONE', ( #64766, #43294, #31639, #29272 ) ) ;
#58590 = DIRECTION ( 'NONE',  ( 1.000000000000000000, -0.000000000000000000, -0.000000000000000000 ) ) ;
#58591 = APPLICATION_CONTEXT ( 'automotive_design' ) ;
#58592 = DIRECTION ( 'NONE',  ( 0.000000000000000000, 1.000000000000000000, 0.000000000000000000 ) ) ;
#58593 = FILL_AREA_STYLE ('',( #15701 ) ) ;
#58594 = UNCERTAINTY_MEASURE_WITH_UNIT (LENGTH_MEASURE( 1.000000000000000082E-05 ), #4162, 'distance_accuracy_value', 'NONE');
#58595 = CARTESIAN_POINT ( 'NONE',  ( -57.95499999999997698, -7.632228543268599452, 2.479861379858951054 ) ) ;
#58596 = CARTESIAN_POINT ( 'NONE',  ( -43.75000000000000000, 0.000000000000000000, 0.000000000000000000 ) ) ;
#58597 = CARTESIAN_POINT ( 'NONE',  ( 0.000000000000000000, 87.30187232391182306, 0.000000000000000000 ) ) ;
#58598 = STYLED_ITEM ( 'NONE', ( #17345 ), #18369 ) ;
#58599 = ADVANCED_FACE ( 'NONE', ( #14339 ), #46762, .T. ) ;
#58600 = DIRECTION ( 'NONE',  ( -1.000000000000000000, 0.000000000000000000, 0.000000000000000000 ) ) ;
#58601 = UNCERTAINTY_MEASURE_WITH_UNIT (LENGTH_MEASURE( 1.000000000000000082E-05 ), #50971, 'distance_accuracy_value', 'NONE');
#58602 = DIRECTION ( 'NONE',  ( 1.110223024625156540E-16, -0.3711537444790456441, 0.9285714285714283811 ) ) ;
#58603 = STYLED_ITEM ( 'NONE', ( #32004 ), #25107 ) ;
#58604 = CARTESIAN_POINT ( 'NONE',  ( -88.70707362346615810, -3.094860106618431139, -9.524999999999991473 ) ) ;
#58605 = DIRECTION ( 'NONE',  ( 0.000000000000000000, 0.000000000000000000, 1.000000000000000000 ) ) ;
#58606 = CIRCLE ( 'NONE', #26067, 0.2500000000000002220 ) ;
#58607 = DIRECTION ( 'NONE',  ( -1.000000000000000000, -5.782411586589331015E-16, 0.000000000000000000 ) ) ;
#58608 = EDGE_CURVE ( 'NONE', #51568, #65703, #58643, .T. ) ;
#58609 = DIRECTION ( 'NONE',  ( 1.000000000000000000, 0.000000000000000000, 0.000000000000000000 ) ) ;
#58610 = DIRECTION ( 'NONE',  ( 0.000000000000000000, 1.000000000000000000, 0.000000000000000000 ) ) ;
#58611 = FACE_OUTER_BOUND ( 'NONE', #66818, .T. ) ;
#58612 = ORIENTED_EDGE ( 'NONE', *, *, #40737, .T. ) ;
#58613 =( NAMED_UNIT ( * ) PLANE_ANGLE_UNIT ( ) SI_UNIT ( $, .RADIAN. ) );
#58614 = AXIS2_PLACEMENT_3D ( 'NONE', #9141, #31244, #35528 ) ;
#58615 = ADVANCED_FACE ( 'NONE', ( #36551 ), #526, .F. ) ;
#58616 = B_SPLINE_CURVE_WITH_KNOTS ( 'NONE', 3,
 ( #19490, #40994, #62411, #8268, #35692, #7900, #29346, #46637 ),
 .UNSPECIFIED., .F., .F.,
 ( 4, 2, 2, 4 ),
 ( 0.008439684080927939078, 0.009486163742497470339, 0.01053264340406700160, 0.01262560272720606412 ),
 .UNSPECIFIED. ) ;
#58617 = CARTESIAN_POINT ( 'NONE',  ( 0.000000000000000000, 118.0570736234661524, -8.025000000000000355 ) ) ;
#58618 = AXIS2_PLACEMENT_3D ( 'NONE', #48047, #15334, #10028 ) ;
#58619 = ADVANCED_FACE ( 'NONE', ( #31193 ), #4454, .F. ) ;
#58620 = AXIS2_PLACEMENT_3D ( 'NONE', #66651, #18465, #51497 ) ;
#58621 = CARTESIAN_POINT ( 'NONE',  ( -20.56511377093078252, 115.3174848394179435, 10.00000000000000000 ) ) ;
#58622 = AXIS2_PLACEMENT_3D ( 'NONE', #64933, #44236, #6892 ) ;
#58623 =( NAMED_UNIT ( * ) PLANE_ANGLE_UNIT ( ) SI_UNIT ( $, .RADIAN. ) );
#58624 = ORIENTED_EDGE ( 'NONE', *, *, #16163, .F. ) ;
#58625 = AXIS2_PLACEMENT_3D ( 'NONE', #11694, #23626, #38484 ) ;
#58626 = EDGE_LOOP ( 'NONE', ( #1920, #68842, #5005, #35789 ) ) ;
#58627 = CARTESIAN_POINT ( 'NONE',  ( -15.98999599679679839, 117.9999999999999716, -7.500000000000000000 ) ) ;
#58628 = EDGE_CURVE ( 'NONE', #24120, #18515, #4189, .T. ) ;
#58629 = PLANE ( 'NONE',  #41023 ) ;
#58630 = EDGE_LOOP ( 'NONE', ( #69385, #11024, #69359, #37384 ) ) ;
#58631 = CARTESIAN_POINT ( 'NONE',  ( -3.094860106618432471, 119.7049999999999983, -9.525000000000000355 ) ) ;
#58632 = CARTESIAN_POINT ( 'NONE',  ( 5.196152422706628471, 1.107695154586738173, -9.000000000000005329 ) ) ;
#58633 = PRESENTATION_LAYER_ASSIGNMENT (  '', '', ( #9241 ) ) ;
#58634 = PRESENTATION_LAYER_ASSIGNMENT (  '', '', ( #57483 ) ) ;
#58635 = CARTESIAN_POINT ( 'NONE',  ( 59.00000000000000000, 11.99999999999999822, 4.000000000000000000 ) ) ;
#58636 = CARTESIAN_POINT ( 'NONE',  ( -100.4949999999999761, 6.826472737025113702, -4.959722759717902107 ) ) ;
#58637 = ORIENTED_EDGE ( 'NONE', *, *, #39976, .F. ) ;
#58638 = CARTESIAN_POINT ( 'NONE',  ( 3.151604648985912416, 154.2021441917068216, -8.710059496740715446 ) ) ;
#58639 = CARTESIAN_POINT ( 'NONE',  ( -140.1570736234661751, -9.058813317711329915, -2.943386871421370898 ) ) ;
#58640 = ORIENTED_EDGE ( 'NONE', *, *, #27479, .F. ) ;
#58641 = CARTESIAN_POINT ( 'NONE',  ( -2.607480562269073765, 150.0929263765338533, -8.025000000000000355 ) ) ;
#58642 = CARTESIAN_POINT ( 'NONE',  ( 7.335726704534224041, 2.464278740834329184, 5.294148637306918204 ) ) ;
#58643 = LINE ( 'NONE', #15079, #6418 ) ;
#58644 = CIRCLE ( 'NONE', #14890, 0.5000000000000004441 ) ;
#58645 = CARTESIAN_POINT ( 'NONE',  ( 20.57648122633967347, 114.5694469452588038, -10.27659575647942169 ) ) ;
#58646 = ORIENTED_EDGE ( 'NONE', *, *, #45789, .T. ) ;
#58647 = DIRECTION ( 'NONE',  ( 1.000000000000000000, 0.000000000000000000, 0.000000000000000000 ) ) ;
#58648 = FACE_OUTER_BOUND ( 'NONE', #39563, .T. ) ;
#58649 = AXIS2_PLACEMENT_3D ( 'NONE', #35310, #45201, #34261 ) ;
#58650 = DIRECTION ( 'NONE',  ( -1.000000000000000000, 0.000000000000000000, 0.000000000000000000 ) ) ;
#58651 = DIRECTION ( 'NONE',  ( 0.000000000000000000, -1.000000000000000000, 0.000000000000000000 ) ) ;
#58652 = CARTESIAN_POINT ( 'NONE',  ( -15.75000000000000000, -0.9999999999999995559, 20.00000000000000000 ) ) ;
#58653 = DIRECTION ( 'NONE',  ( 0.000000000000000000, 0.000000000000000000, -1.000000000000000000 ) ) ;
#58654 = VERTEX_POINT ( 'NONE', #37237 ) ;
#58655 = EDGE_LOOP ( 'NONE', ( #11549, #43379, #64516, #49680 ) ) ;
#58656 = CARTESIAN_POINT ( 'NONE',  ( -20.71231517720798010, 149.9999999999999716, -10.00000000000000000 ) ) ;
#58657 = CYLINDRICAL_SURFACE ( 'NONE', #54758, 5.000000000000004441 ) ;
#58658 = PRESENTATION_STYLE_ASSIGNMENT (( #196 ) ) ;
#58659 = VERTEX_POINT ( 'NONE', #53383 ) ;
#58660 = CARTESIAN_POINT ( 'NONE',  ( -173.6049999999999898, 6.826472737025113702, -4.959722759717902107 ) ) ;
#58661 = DIRECTION ( 'NONE',  ( -0.000000000000000000, -0.000000000000000000, 1.000000000000000000 ) ) ;
#58662 = DIRECTION ( 'NONE',  ( 0.000000000000000000, 0.000000000000000000, -1.000000000000000000 ) ) ;
#58663 = CARTESIAN_POINT ( 'NONE',  ( -181.3449999999999989, 7.632228543268599452, -2.479861379858951942 ) ) ;
#58664 = AXIS2_PLACEMENT_3D ( 'NONE', #37644, #45332, #66383 ) ;
#58665 = CARTESIAN_POINT ( 'NONE',  ( -171.8949999999999534, 6.826472737025115478, 4.959722759717899443 ) ) ;
#58666 = EDGE_LOOP ( 'NONE', ( #47915, #11759, #40878 ) ) ;
#58667 = DIRECTION ( 'NONE',  ( -0.000000000000000000, -0.000000000000000000, -1.000000000000000000 ) ) ;
#58668 =( GEOMETRIC_REPRESENTATION_CONTEXT ( 3 ) GLOBAL_UNCERTAINTY_ASSIGNED_CONTEXT ( ( #64900 ) ) GLOBAL_UNIT_ASSIGNED_CONTEXT ( ( #9615, #31370, #10296 ) ) REPRESENTATION_CONTEXT ( 'NONE', 'WORKASPACE' ) );
#58669 = CARTESIAN_POINT ( 'NONE',  ( -53.18756747357285519, -10.02680648607945102, -3.500000000000002220 ) ) ;
#58670 = CARTESIAN_POINT ( 'NONE',  ( -84.65500000000000114, -7.632228543268600340, -2.479861379858950166 ) ) ;
#58671 = FACE_OUTER_BOUND ( 'NONE', #3009, .T. ) ;
#58672 = TOROIDAL_SURFACE ( 'NONE', #2433, 17.50000000000000000, 0.5000000000000000000 ) ;
#58673 = CARTESIAN_POINT ( 'NONE',  ( -75.01595440434799400, 35.98078654237776419, -9.636386880385824583 ) ) ;
#58674 = CARTESIAN_POINT ( 'NONE',  ( -79.94499999999999318, -9.827790563157499189E-16, -8.024999999999991473 ) ) ;
#58675 = CARTESIAN_POINT ( 'NONE',  ( 3.094860106618431583, 136.2049999999999557, 9.525000000000000355 ) ) ;
#58676 = CIRCLE ( 'NONE', #17191, 0.2500000000000002220 ) ;
#58677 = DIRECTION ( 'NONE',  ( 0.000000000000000000, 0.6691306063588591257, -0.7431448254773933559 ) ) ;
#58678 = EDGE_CURVE ( 'NONE', #38619, #46060, #40194, .T. ) ;
#58679 = CARTESIAN_POINT ( 'NONE',  ( -171.2070736234663570, 3.094860106620802132, 9.524999999998270184 ) ) ;
#58680 = PRODUCT_DEFINITION_SHAPE ( 'NONE', 'NONE',  #69706 ) ;
#58681 = VECTOR ( 'NONE', #48126, 1000.000000000000000 ) ;
#58682 = DIRECTION ( 'NONE',  ( 0.000000000000000000, 0.000000000000000000, 1.000000000000000000 ) ) ;
#58683 = UNCERTAINTY_MEASURE_WITH_UNIT (LENGTH_MEASURE( 1.000000000000000082E-05 ), #52363, 'distance_accuracy_value', 'NONE');
#58684 = EDGE_CURVE ( 'NONE', #16390, #60144, #46648, .T. ) ;
#58685 = PRESENTATION_LAYER_ASSIGNMENT (  '', '', ( #38508 ) ) ;
#58686 = DIRECTION ( 'NONE',  ( 0.000000000000000000, 0.000000000000000000, 1.000000000000000000 ) ) ;
#58687 = ADVANCED_FACE ( 'NONE', ( #172 ), #55442, .T. ) ;
#58688 = ORIENTED_EDGE ( 'NONE', *, *, #8726, .F. ) ;
#58689 = VECTOR ( 'NONE', #14000, 1000.000000000000000 ) ;
#58690 = FACE_OUTER_BOUND ( 'NONE', #62445, .T. ) ;
#58691 = EDGE_CURVE ( 'NONE', #10058, #35167, #69355, .T. ) ;
#58692 =( GEOMETRIC_REPRESENTATION_CONTEXT ( 3 ) GLOBAL_UNCERTAINTY_ASSIGNED_CONTEXT ( ( #32085 ) ) GLOBAL_UNIT_ASSIGNED_CONTEXT ( ( #6399, #50717, #60900 ) ) REPRESENTATION_CONTEXT ( 'NONE', 'WORKASPACE' ) );
#58693 = ADVANCED_FACE ( 'NONE', ( #27643 ), #33305, .T. ) ;
#58694 = AXIS2_PLACEMENT_3D ( 'NONE', #59007, #26624, #64277 ) ;
#58695 = EDGE_CURVE ( 'NONE', #37203, #52477, #55076, .T. ) ;
#58697 = SURFACE_STYLE_USAGE ( .BOTH. , #26998 ) ;
#58696 = LINE ( 'NONE', #43271, #38660 ) ;
#58698 = CARTESIAN_POINT ( 'NONE',  ( -8.437984349512095861, 136.8070736234661808, -5.166775262442723748E-16 ) ) ;
#58699 = ORIENTED_EDGE ( 'NONE', *, *, #60899, .T. ) ;
#58700 = VERTEX_POINT ( 'NONE', #65650 ) ;
#58701 = SURFACE_SIDE_STYLE ('',( #57670 ) ) ;
#58702 = EDGE_CURVE ( 'NONE', #38934, #53965, #29981, .T. ) ;
#58703 =( GEOMETRIC_REPRESENTATION_CONTEXT ( 3 ) GLOBAL_UNCERTAINTY_ASSIGNED_CONTEXT ( ( #30757 ) ) GLOBAL_UNIT_ASSIGNED_CONTEXT ( ( #51067, #66543, #34522 ) ) REPRESENTATION_CONTEXT ( 'NONE', 'WORKASPACE' ) );
#58704 = ADVANCED_FACE ( 'NONE', ( #1906 ), #38274, .T. ) ;
#58705 = VECTOR ( 'NONE', #26927, 1000.000000000000000 ) ;
#58706 =( LENGTH_UNIT ( ) NAMED_UNIT ( * ) SI_UNIT ( .MILLI., .METRE. ) );
#58707 = FACE_OUTER_BOUND ( 'NONE', #10649, .T. ) ;
#58708 = SURFACE_STYLE_FILL_AREA ( #65000 ) ;
#58709 = CARTESIAN_POINT ( 'NONE',  ( 7.632228543268608334, 140.3429263765338249, -2.479861379858951942 ) ) ;
#58710 = VERTEX_POINT ( 'NONE', #22749 ) ;
#58712 = B_SPLINE_CURVE_WITH_KNOTS ( 'NONE', 3,
 ( #15380, #48087, #68127, #68460, #58248, #10072, #69161, #20967 ),
 .UNSPECIFIED., .F., .F.,
 ( 4, 2, 2, 4 ),
 ( 0.000000000000000000, 0.0004110476197876519158, 0.0006165714296814797440, 0.0008220952395753075180 ),
 .UNSPECIFIED. ) ;
#58711 = CARTESIAN_POINT ( 'NONE',  ( -120.3549999999999898, -4.716976649647093289, -6.492361379858945902 ) ) ;
#58713 = ORIENTED_EDGE ( 'NONE', *, *, #61075, .T. ) ;
#58714 = CARTESIAN_POINT ( 'NONE',  ( -137.9070736234667436, -3.094860106609220285, 9.525000000006683010 ) ) ;
#58715 =( NAMED_UNIT ( * ) PLANE_ANGLE_UNIT ( ) SI_UNIT ( $, .RADIAN. ) );
#58716 = VERTEX_POINT ( 'NONE', #17818 ) ;
#58717 =( NAMED_UNIT ( * ) PLANE_ANGLE_UNIT ( ) SI_UNIT ( $, .RADIAN. ) );
#58718 = DIRECTION ( 'NONE',  ( 1.000000000000000000, 0.000000000000000000, 0.000000000000000000 ) ) ;
#58719 = ORIENTED_EDGE ( 'NONE', *, *, #44618, .F. ) ;
#58720 =( NAMED_UNIT ( * ) SI_UNIT ( $, .STERADIAN. ) SOLID_ANGLE_UNIT ( ) );
#58721 = CARTESIAN_POINT ( 'NONE',  ( -5.598654528085808657, 149.6450000000000102, 7.705886871421373741 ) ) ;
#58722 = SURFACE_STYLE_FILL_AREA ( #63651 ) ;
#58723 = ORIENTED_EDGE ( 'NONE', *, *, #66305, .T. ) ;
#58724 = AXIS2_PLACEMENT_3D ( 'NONE', #18681, #29571, #66877 ) ;
#58725 = FACE_OUTER_BOUND ( 'NONE', #44989, .T. ) ;
#58726 = CARTESIAN_POINT ( 'NONE',  ( 9.058813317711337021, 145.6549999999999727, 2.943386871421375783 ) ) ;
#58727 = CARTESIAN_POINT ( 'NONE',  ( -135.9570736234661865, 9.058813317711329915, -2.943386871421373119 ) ) ;
#58728 = CARTESIAN_POINT ( 'NONE',  ( -130.0429263765338135, -9.058813317711329915, -2.943386871421370898 ) ) ;
#58729 = ORIENTED_EDGE ( 'NONE', *, *, #50987, .T. ) ;
#58730 = CARTESIAN_POINT ( 'NONE',  ( 7.632228543268607446, 122.0429263765338135, 2.479861379858954606 ) ) ;
#58731 = LINE ( 'NONE', #44670, #39079 ) ;
#58732 = UNCERTAINTY_MEASURE_WITH_UNIT (LENGTH_MEASURE( 1.000000000000000082E-05 ), #28654, 'distance_accuracy_value', 'NONE');
#58733 = CARTESIAN_POINT ( 'NONE',  ( -47.71347897792733761, -13.42724224818812040, 0.9185643661977238583 ) ) ;
#58734 = DIRECTION ( 'NONE',  ( 1.000000000000000000, 0.000000000000000000, -0.000000000000000000 ) ) ;
#58736 = CLOSED_SHELL ( 'NONE', ( #68551, #13584, #21316, #63851, #32799, #36477, #10190, #46507, #69261, #48321, #51534, #22015, #66640, #15754, #42644, #10110, #23236, #48453, #31854, #37626, #43504, #12899, #24383, #3197, #23057, #17692, #21188, #14808, #20414, #17443, #49889, #25659, #9057, #60130, #33588, #1385, #69042, #5852, #13966, #50144, #32479, #48817, #25726, #9473, #43661, #17422, #29309, #25798, #47383, #37898, #58619, #9068, #65596, #48973, #57035, #23739, #56478, #43186, #27294, #22745, #5776, #19692, #2613, #20903, #67535, #52676, #62726, #3109, #45142, #34932, #19793, #29078, #57571, #43263, #7960, #28790, #27374, #15066, #23760, #51434, #17664, #46922, #37537, #62457, #22725, #40275, #52134, #11833, #22800, #51812, #61877, #732, #13575, #8539, #69613, #24852, #5862, #7177, #15209, #62484, #959, #59214, #66381, #67261, #35265, #31599, #62816, #22304, #46275, #4500, #25491, #33355, #8923, #7361, #58704, #28748, #30249, #58599, #13842, #12013, #51194, #87, #18292, #16864, #48340, #33625, #68252, #45568, #26213, #35453, #53990, #50834, #15826, #44200, #61803, #15305, #17272, #49528, #22003, #7259, #46516, #9331, #413, #12291, #69187, #54771, #46912, #1191, #14500, #52832, #10344, #16349, #34621, #25220, #61678, #31604, #8127, #44851, #63878, #25107, #54231, #34703, #35614, #55468, #2820, #54665, #18531, #33429, #16655, #62279, #11186, #51411, #1461, #3494, #31034, #19990, #56868, #26993, #8754, #8442, #1111, #67420, #66698, #19852, #45798, #25963, #41344, #58971, #68163, #59718, #45663, #20977, #55765, #4039, #64946, #20668, #41887, #38953, #11347, #21041, #46200, #17817, #62157, #12423, #12452, #34175, #53463, #69178, #18149, #2245, #44302, #34550, #38644, #65509, #45224, #61675, #16682, #15907, #2839, #8523, #27529, #48348, #10844, #23705, #18116, #9839, #34243, #15583, #60579, #50424, #49411, #67510, #41731, #65333, #51101, #38079, #5139, #22907, #42953, #45982, #1027, #4931, #56294, #19538, #53652, #45241, #31262, #30408, #17773, #60351, #60805, #14878 ) ) ;
#58735 = DIRECTION ( 'NONE',  ( -1.000000000000000000, 0.000000000000000000, 0.000000000000000000 ) ) ;
#58737 = EDGE_LOOP ( 'NONE', ( #45074, #56714, #68889, #35102, #61652, #43466 ) ) ;
#58738 =( GEOMETRIC_REPRESENTATION_CONTEXT ( 3 ) GLOBAL_UNCERTAINTY_ASSIGNED_CONTEXT ( ( #27190 ) ) GLOBAL_UNIT_ASSIGNED_CONTEXT ( ( #43620, #27372, #59749 ) ) REPRESENTATION_CONTEXT ( 'NONE', 'WORKASPACE' ) );
#58739 = FACE_OUTER_BOUND ( 'NONE', #2676, .T. ) ;
#58740 = EDGE_LOOP ( 'NONE', ( #65134, #16220, #55971, #47880 ) ) ;
#58741 = CARTESIAN_POINT ( 'NONE',  ( -57.59292637653379643, -3.094860106618431139, -9.524999999999991473 ) ) ;
#58742 = CARTESIAN_POINT ( 'NONE',  ( -74.99999999999998579, 50.00000000000000000, -6.500000000000000000 ) ) ;
#58743 = CARTESIAN_POINT ( 'NONE',  ( -6.938426666069068993, 1.982292489777645272, 0.2088670156639333142 ) ) ;
#58744 = CARTESIAN_POINT ( 'NONE',  ( -147.6549999999999727, -7.632228543268600340, -2.479861379858950166 ) ) ;
#58745 = AXIS2_PLACEMENT_3D ( 'NONE', #46935, #10302, #20125 ) ;
#58746 = DIRECTION ( 'NONE',  ( 1.000000000000000000, 0.000000000000000000, 0.000000000000000000 ) ) ;
#58747 = CYLINDRICAL_SURFACE ( 'NONE', #64219, 0.5000000000000004441 ) ;
#58748 = UNCERTAINTY_MEASURE_WITH_UNIT (LENGTH_MEASURE( 1.000000000000000082E-05 ), #25205, 'distance_accuracy_value', 'NONE');
#58749 = EDGE_CURVE ( 'NONE', #40244, #31294, #19033, .T. ) ;
#58750 =( GEOMETRIC_REPRESENTATION_CONTEXT ( 3 ) GLOBAL_UNCERTAINTY_ASSIGNED_CONTEXT ( ( #48955 ) ) GLOBAL_UNIT_ASSIGNED_CONTEXT ( ( #51460, #3946, #14183 ) ) REPRESENTATION_CONTEXT ( 'NONE', 'WORKASPACE' ) );
#58751 =( NAMED_UNIT ( * ) PLANE_ANGLE_UNIT ( ) SI_UNIT ( $, .RADIAN. ) );
#58752 = ORIENTED_EDGE ( 'NONE', *, *, #24456, .T. ) ;
#58753 = ORIENTED_EDGE ( 'NONE', *, *, #48692, .T. ) ;
#58754 = DIRECTION ( 'NONE',  ( 0.000000000000000000, -1.000000000000000000, 0.000000000000000000 ) ) ;
#58755 = TOROIDAL_SURFACE ( 'NONE', #11536, 7.499999999999998224, 0.5000000000000000000 ) ;
#58756 = CARTESIAN_POINT ( 'NONE',  ( 75.83633811589984930, 14.00000000000000000, 66.72655454856716517 ) ) ;
#58757 = CARTESIAN_POINT ( 'NONE',  ( -65.30499999999999261, 8.437984349512085203, -1.550032578732815448E-15 ) ) ;
#58758 = ORIENTED_EDGE ( 'NONE', *, *, #39344, .T. ) ;
#58759 = DIRECTION ( 'NONE',  ( 0.000000000000000000, -0.000000000000000000, -1.000000000000000000 ) ) ;
#58760 = CONICAL_SURFACE ( 'NONE', #40808, 7.000000000000000888, 0.7853981633974500554 ) ;
#58761 = FILL_AREA_STYLE ('',( #32026 ) ) ;
#58762 = CARTESIAN_POINT ( 'NONE',  ( -127.9429263765338192, 0.000000000000000000, 9.524999999999991473 ) ) ;
#58763 = ORIENTED_EDGE ( 'NONE', *, *, #50176, .T. ) ;
#58764 = CIRCLE ( 'NONE', #61003, 0.2500000000000002220 ) ;
#58765 = CARTESIAN_POINT ( 'NONE',  ( 3.046771365092978190, 72.00000000000001421, 6.349999999999997868 ) ) ;
#58766 = CARTESIAN_POINT ( 'NONE',  ( -12.72792206135785698, 149.9999999999999716, 10.00000000000000000 ) ) ;
#58767 = SURFACE_SIDE_STYLE ('',( #21474 ) ) ;
#58768 = CARTESIAN_POINT ( 'NONE',  ( 8.437984349512095861, 126.3070736234661524, 1.550032578732816828E-15 ) ) ;
#58769 = EDGE_CURVE ( 'NONE', #46816, #29086, #63283, .T. ) ;
#58770 = CARTESIAN_POINT ( 'NONE',  ( -110.0949999999999704, -2.607480562269071545, -8.024999999999991473 ) ) ;
#58771 = CARTESIAN_POINT ( 'NONE',  ( -9.058813317711338797, 146.3449999999999989, 2.943386871421373563 ) ) ;
#58772 = CARTESIAN_POINT ( 'NONE',  ( -85.94499999999999318, -9.827790563157499189E-16, -8.024999999999991473 ) ) ;
#58773 = CARTESIAN_POINT ( 'NONE',  ( -195.0000000000000000, 0.000000000000000000, 9.524999999999991473 ) ) ;
#58774 = CIRCLE ( 'NONE', #53215, 0.2500000000000002220 ) ;
#58775 = CIRCLE ( 'NONE', #5986, 5.000000000000004441 ) ;
#58776 = PLANE ( 'NONE',  #59517 ) ;
#58777 = UNCERTAINTY_MEASURE_WITH_UNIT (LENGTH_MEASURE( 1.000000000000000082E-05 ), #24762, 'distance_accuracy_value', 'NONE');
#58778 = EDGE_CURVE ( 'NONE', #57229, #20856, #56102, .T. ) ;
#58779 = DIRECTION ( 'NONE',  ( 0.000000000000000000, -0.000000000000000000, 1.000000000000000000 ) ) ;
#58780 = ORIENTED_EDGE ( 'NONE', *, *, #46357, .T. ) ;
#58781 = CARTESIAN_POINT ( 'NONE',  ( -135.8929263765338362, -8.102448949553172852, -5.886773742842741797 ) ) ;
#58782 = LINE ( 'NONE', #14847, #24197 ) ;
#58783 = CARTESIAN_POINT ( 'NONE',  ( -145.4949999999999477, 6.826472737025113702, -4.959722759717902107 ) ) ;
#58784 = CARTESIAN_POINT ( 'NONE',  ( 52.75000000000000000, 24.74999999999998224, -4.000000000000000000 ) ) ;
#58785 = EDGE_CURVE ( 'NONE', #20552, #48146, #14534, .T. ) ;
#58786 = CARTESIAN_POINT ( 'NONE',  ( -67.25707362346616947, 5.598654528085800663, -7.705886871421367523 ) ) ;
#58787 =( NAMED_UNIT ( * ) PLANE_ANGLE_UNIT ( ) SI_UNIT ( $, .RADIAN. ) );
#58788 = ORIENTED_EDGE ( 'NONE', *, *, #21282, .T. ) ;
#58789 = EDGE_LOOP ( 'NONE', ( #47998, #37655, #62463, #46022, #53285 ) ) ;
#58790 = PRESENTATION_LAYER_ASSIGNMENT (  '', '', ( #10494 ) ) ;
#58791 = CARTESIAN_POINT ( 'NONE',  ( 27.99999999999998224, 5.000000000000000000, 72.00402776293822171 ) ) ;
#58792 = EDGE_CURVE ( 'NONE', #22827, #42596, #3198, .T. ) ;
#58793 = CARTESIAN_POINT ( 'NONE',  ( -45.00000000000000000, 8.681192140609645946, 5.652915417256442865 ) ) ;
#58794 =( LENGTH_UNIT ( ) NAMED_UNIT ( * ) SI_UNIT ( .MILLI., .METRE. ) );
#58795 = DIRECTION ( 'NONE',  ( 0.000000000000000000, -0.000000000000000000, -1.000000000000000000 ) ) ;
#58796 = VECTOR ( 'NONE', #38449, 1000.000000000000000 ) ;
#58797 = DIRECTION ( 'NONE',  ( 0.000000000000000000, 0.000000000000000000, 1.000000000000000000 ) ) ;
#58798 = EDGE_LOOP ( 'NONE', ( #38237, #19677, #40579, #28826 ) ) ;
#58799 = CARTESIAN_POINT ( 'NONE',  ( -148.7049999999999841, 2.607480562269072433, 8.024999999999991473 ) ) ;
#58800 = AXIS2_PLACEMENT_3D ( 'NONE', #45394, #23209, #1333 ) ;
#58801 = VERTEX_POINT ( 'NONE', #50525 ) ;
#58802 = FILL_AREA_STYLE ('',( #37396 ) ) ;
#58803 = CARTESIAN_POINT ( 'NONE',  ( -142.2570736234661695, 5.598654528085800663, -7.705886871421367523 ) ) ;
#58804 = ORIENTED_EDGE ( 'NONE', *, *, #7948, .T. ) ;
#58805 = DIRECTION ( 'NONE',  ( -0.000000000000000000, -0.000000000000000000, 1.000000000000000000 ) ) ;
#58806 = CARTESIAN_POINT ( 'NONE',  ( -1.166476076187854022E-15, 122.9449999999999790, 9.525000000000000355 ) ) ;
#58807 = CARTESIAN_POINT ( 'NONE',  ( 75.00000000000000000, -2.215169945516535778E-14, 10.00000000000000000 ) ) ;
#58808 = STYLED_ITEM ( 'NONE', ( #29048 ), #26656 ) ;
#58809 = VERTEX_POINT ( 'NONE', #13210 ) ;
#58810 =( GEOMETRIC_REPRESENTATION_CONTEXT ( 3 ) GLOBAL_UNCERTAINTY_ASSIGNED_CONTEXT ( ( #65839 ) ) GLOBAL_UNIT_ASSIGNED_CONTEXT ( ( #55583, #63199, #30827 ) ) REPRESENTATION_CONTEXT ( 'NONE', 'WORKASPACE' ) );
#58811 = DIRECTION ( 'NONE',  ( 1.000000000000000000, -0.000000000000000000, -0.000000000000000000 ) ) ;
#58812 = CARTESIAN_POINT ( 'NONE',  ( -9.058813317711337021, 117.1549999999999869, -2.943386871421374895 ) ) ;
#58813 = CARTESIAN_POINT ( 'NONE',  ( -66.80499999999999261, -8.437984349512086979, 5.166775262442717831E-16 ) ) ;
#58814 = CARTESIAN_POINT ( 'NONE',  ( -116.6949999999999790, -8.437984349512085203, 5.166775262442717831E-16 ) ) ;
#58815 = CARTESIAN_POINT ( 'NONE',  ( -41.27334858134337026, 107.3315027881082528, -3.464507624620943638 ) ) ;
#58816 = ORIENTED_EDGE ( 'NONE', *, *, #25244, .F. ) ;
#58817 = CARTESIAN_POINT ( 'NONE',  ( -5.598654528085806881, 143.8549999999999898, -7.705886871421374629 ) ) ;
#58818 = UNCERTAINTY_MEASURE_WITH_UNIT (LENGTH_MEASURE( 1.000000000000000082E-05 ), #53224, 'distance_accuracy_value', 'NONE');
#58819 = CARTESIAN_POINT ( 'NONE',  ( -65.49999999999998579, 50.00000000000000000, -10.49999999999999822 ) ) ;
#58820 = AXIS2_PLACEMENT_3D ( 'NONE', #65551, #33539, #7161 ) ;
#58821 = DIRECTION ( 'NONE',  ( 0.000000000000000000, -1.000000000000000000, 0.000000000000000000 ) ) ;
#58822 = FACE_OUTER_BOUND ( 'NONE', #981, .T. ) ;
#58823 = VERTEX_POINT ( 'NONE', #56120 ) ;
#58824 = COLOUR_RGB ( '', 0.40784314, 0.44705882, 0.49803922) ;
#58825 = FILL_AREA_STYLE ('',( #14895 ) ) ;
#58826 = CARTESIAN_POINT ( 'NONE',  ( -183.6549999999999727, -7.632228543268600340, -2.479861379858950166 ) ) ;
#58827 = ORIENTED_EDGE ( 'NONE', *, *, #57421, .T. ) ;
#58828 = FILL_AREA_STYLE ('',( #27132 ) ) ;
#58829 = EDGE_CURVE ( 'NONE', #18515, #57001, #40633, .T. ) ;
#58830 =( GEOMETRIC_REPRESENTATION_CONTEXT ( 3 ) GLOBAL_UNCERTAINTY_ASSIGNED_CONTEXT ( ( #63522 ) ) GLOBAL_UNIT_ASSIGNED_CONTEXT ( ( #170, #44844, #32252 ) ) REPRESENTATION_CONTEXT ( 'NONE', 'WORKASPACE' ) );
#58831 =( LENGTH_UNIT ( ) NAMED_UNIT ( * ) SI_UNIT ( .MILLI., .METRE. ) );
#58832 = MECHANICAL_DESIGN_GEOMETRIC_PRESENTATION_REPRESENTATION (  '', ( #28468 ), #37545 ) ;
#58833 = SURFACE_SIDE_STYLE ('',( #44439 ) ) ;
#58834 = ORIENTED_EDGE ( 'NONE', *, *, #21949, .F. ) ;
#58835 = CARTESIAN_POINT ( 'NONE',  ( 22.99999999999995381, 0.000000000000000000, 32.00402776293825724 ) ) ;
#58836 = CARTESIAN_POINT ( 'NONE',  ( -96.50499999999998124, -6.826472737025115478, -4.959722759717899443 ) ) ;
#58838 = ORIENTED_EDGE ( 'NONE', *, *, #28569, .F. ) ;
#58837 = AXIS2_PLACEMENT_3D ( 'NONE', #45833, #61972, #37386 ) ;
#58839 = LINE ( 'NONE', #48677, #18294 ) ;
#58840 =( NAMED_UNIT ( * ) PLANE_ANGLE_UNIT ( ) SI_UNIT ( $, .RADIAN. ) );
#58841 = CARTESIAN_POINT ( 'NONE',  ( -132.0570736234661808, 0.000000000000000000, 9.524999999999991473 ) ) ;
#58842 = AXIS2_PLACEMENT_3D ( 'NONE', #40410, #66790, #8397 ) ;
#58843 =( BOUNDED_CURVE ( )  B_SPLINE_CURVE ( 2, ( #66221, #39888, #18045, #65540, #60262, #6785, #54283, #60584, #61293, #28919, #12401 ),
 .UNSPECIFIED., .F., .F. ) 
 B_SPLINE_CURVE_WITH_KNOTS ( ( 3, 2, 2, 2, 2, 3 ),
 ( 0.5217391304347702707, 0.5239130434782484080, 0.5260869565217266564, 0.5282608695652047937, 0.5304347826086831530, 0.5326086956521612903 ),
 .UNSPECIFIED. ) 
 CURVE ( )  GEOMETRIC_REPRESENTATION_ITEM ( )  RATIONAL_B_SPLINE_CURVE ( ( 1.000000000000277556, 0.9510565162948760864, 1.000000000000000000, 0.9510565162951535312, 1.000000000000000000, 0.9510565162951535312, 1.000000000000000000, 0.9510565162951535312, 1.000000000000000000, 0.9510565162954385254, 0.9999999999997150057 ) ) 
 REPRESENTATION_ITEM ( '' )  );
#58844 = CARTESIAN_POINT ( 'NONE',  ( -9.827790563157511022E-16, 143.5570736234661524, 8.025000000000000355 ) ) ;
#58845 = CARTESIAN_POINT ( 'NONE',  ( 0.000000000000000000, 148.4449999999999932, -9.525000000000000355 ) ) ;
#58846 = CARTESIAN_POINT ( 'NONE',  ( -66.35707362346616378, 5.598654528085804216, 7.705886871421366635 ) ) ;
#58847 = VECTOR ( 'NONE', #24530, 1000.000000000000000 ) ;
#58848 = CARTESIAN_POINT ( 'NONE',  ( -79.94292637653380496, 0.000000000000000000, 9.524999999999991473 ) ) ;
#58849 = AXIS2_PLACEMENT_3D ( 'NONE', #52822, #15542, #69337 ) ;
#58850 = ORIENTED_EDGE ( 'NONE', *, *, #21157, .T. ) ;
#58851 = CARTESIAN_POINT ( 'NONE',  ( -5.196152422706633800, -9.000000000000005329, 7.500000000000000000 ) ) ;
#58853 =( LENGTH_UNIT ( ) NAMED_UNIT ( * ) SI_UNIT ( .MILLI., .METRE. ) );
#58852 = CYLINDRICAL_SURFACE ( 'NONE', #56024, 12.50000000000000178 ) ;
#58854 = CIRCLE ( 'NONE', #27334, 0.5000000000000004441 ) ;
#58855 = B_SPLINE_CURVE_WITH_KNOTS ( 'NONE', 3,
 ( #2828, #56693, #25362, #45814, #36311, #14133 ),
 .UNSPECIFIED., .F., .F.,
 ( 4, 2, 4 ),
 ( 4.336808689942017736E-19, 0.001189544056195996052, 0.002379088112391991670 ),
 .UNSPECIFIED. ) ;
#58856 = EDGE_CURVE ( 'NONE', #41095, #10826, #35730, .T. ) ;
#58857 = AXIS2_PLACEMENT_3D ( 'NONE', #38320, #33006, #38673 ) ;
#58858 = CARTESIAN_POINT ( 'NONE',  ( -113.6049999999999898, 6.826472737025113702, -4.959722759717902107 ) ) ;
#58859 = EDGE_CURVE ( 'NONE', #4364, #60894, #58367, .T. ) ;
#58860 = CARTESIAN_POINT ( 'NONE',  ( 5.598654528085805993, 123.2449999999999903, 7.705886871421374629 ) ) ;
#58861 = CARTESIAN_POINT ( 'NONE',  ( -115.7949999999999875, 2.607480562269068880, -8.024999999999993250 ) ) ;
#58862 = FACE_OUTER_BOUND ( 'NONE', #64859, .T. ) ;
#58863 = AXIS2_PLACEMENT_3D ( 'NONE', #31840, #53329, #27235 ) ;
#58865 = CARTESIAN_POINT ( 'NONE',  ( -153.3570736234661922, 5.598654528085804216, 7.705886871421366635 ) ) ;
#58864 = FACE_OUTER_BOUND ( 'NONE', #19751, .T. ) ;
#58866 = CIRCLE ( 'NONE', #63375, 0.5000000000000004441 ) ;
#58867 = EDGE_CURVE ( 'NONE', #58564, #58968, #10079, .T. ) ;
#58868 = ORIENTED_EDGE ( 'NONE', *, *, #17969, .T. ) ;
#58869 = CARTESIAN_POINT ( 'NONE',  ( -158.2429263765338021, 5.598654528085804216, 7.705886871421366635 ) ) ;
#58870 = CARTESIAN_POINT ( 'NONE',  ( -173.5450000000000159, -7.632228543268600340, -2.479861379858950166 ) ) ;
#58871 = ADVANCED_FACE ( 'NONE', ( #30080 ), #40321, .T. ) ;
#58872 = AXIS2_PLACEMENT_3D ( 'NONE', #184, #4116, #37246 ) ;
#58873 = CARTESIAN_POINT ( 'NONE',  ( 62.24999999999998579, 31.24999999999999289, 4.000000000000000000 ) ) ;
#58874 = ADVANCED_FACE ( 'NONE', ( #24123 ), #46317, .F. ) ;
#58875 = PRESENTATION_LAYER_ASSIGNMENT (  '', '', ( #10580 ) ) ;
#58876 = CARTESIAN_POINT ( 'NONE',  ( 0.000000000000000000, 0.000000000000000000, 0.000000000000000000 ) ) ;
#58877 = CARTESIAN_POINT ( 'NONE',  ( -70.75000000000000000, -4.000000000000000000, 24.00000000000000000 ) ) ;
#58878 = ORIENTED_EDGE ( 'NONE', *, *, #7588, .T. ) ;
#58879 = CARTESIAN_POINT ( 'NONE',  ( -79.64292637653380780, -5.598654528085801552, 7.705886871421367523 ) ) ;
#58880 = CARTESIAN_POINT ( 'NONE',  ( -71.74137931034479720, 63.10081643261027295, 10.00000000000000000 ) ) ;
#58881 =( NAMED_UNIT ( * ) PLANE_ANGLE_UNIT ( ) SI_UNIT ( $, .RADIAN. ) );
#58882 = EDGE_CURVE ( 'NONE', #32302, #20280, #51216, .T. ) ;
#58883 = CARTESIAN_POINT ( 'NONE',  ( 74.99999999999998579, 50.00000000000000000, -7.500000000000000000 ) ) ;
#58884 = DIRECTION ( 'NONE',  ( 1.000000000000000000, 0.000000000000000000, 0.000000000000000000 ) ) ;
#58885 = DIRECTION ( 'NONE',  ( 0.000000000000000000, 0.000000000000000000, 1.000000000000000000 ) ) ;
#58886 = CARTESIAN_POINT ( 'NONE',  ( -180.6550000000000011, -7.632228543268600340, -2.479861379858950166 ) ) ;
#58887 = CIRCLE ( 'NONE', #44372, 0.5000000000000004441 ) ;
#58888 = ORIENTED_EDGE ( 'NONE', *, *, #29136, .F. ) ;
#58889 = CARTESIAN_POINT ( 'NONE',  ( -4.000000000000000000, -3.499999999999999556, 24.00000000000000000 ) ) ;
#58890 = SURFACE_STYLE_FILL_AREA ( #16692 ) ;
#58891 = AXIS2_PLACEMENT_3D ( 'NONE', #19540, #25172, #36091 ) ;
#58892 = CARTESIAN_POINT ( 'NONE',  ( 0.000000000000000000, 0.000000000000000000, 0.7500000000000000000 ) ) ;
#58893 = CARTESIAN_POINT ( 'NONE',  ( -8.437984349512095861, 142.8070736234661808, -5.166775262442723748E-16 ) ) ;
#58894 = MECHANICAL_DESIGN_GEOMETRIC_PRESENTATION_REPRESENTATION (  '', ( #6064 ), #45429 ) ;
#58895 = TOROIDAL_SURFACE ( 'NONE', #64515, 1.000000000000000000, 0.5000000000000000000 ) ;
#58896 = ORIENTED_EDGE ( 'NONE', *, *, #54905, .T. ) ;
#58897 = CARTESIAN_POINT ( 'NONE',  ( -31.83594241490679622, -8.712327904965905034, -1.102500065259914619 ) ) ;
#58898 = CARTESIAN_POINT ( 'NONE',  ( -89.00499999999998124, 6.826472737025115478, 4.959722759717899443 ) ) ;
#58899 = UNCERTAINTY_MEASURE_WITH_UNIT (LENGTH_MEASURE( 1.000000000000000082E-05 ), #3012, 'distance_accuracy_value', 'NONE');
#58900 = VERTEX_POINT ( 'NONE', #13921 ) ;
#58901 = CARTESIAN_POINT ( 'NONE',  ( -23.21231517720797655, 112.9999999999999858, 10.00000000000000000 ) ) ;
#58902 = CARTESIAN_POINT ( 'NONE',  ( 15.00000000000000000, 8.000000000000000000, -4.000000000000000000 ) ) ;
#58903 = FILL_AREA_STYLE_COLOUR ( '', #36538 ) ;
#58904 = SURFACE_STYLE_FILL_AREA ( #32859 ) ;
#58905 = DIRECTION ( 'NONE',  ( -1.000000000000000000, 0.000000000000000000, 0.000000000000000000 ) ) ;
#58906 = VERTEX_POINT ( 'NONE', #41035 ) ;
#58907 = DIRECTION ( 'NONE',  ( 1.000000000000000000, 0.000000000000000000, 0.000000000000000000 ) ) ;
#58908 = CARTESIAN_POINT ( 'NONE',  ( -69.14499999999998181, -4.716976649647092401, 6.492361379858946790 ) ) ;
#58909 = ORIENTED_EDGE ( 'NONE', *, *, #24694, .T. ) ;
#58910 = LINE ( 'NONE', #26851, #48564 ) ;
#58911 = AXIS2_PLACEMENT_3D ( 'NONE', #55734, #33917, #50458 ) ;
#58912 = EDGE_CURVE ( 'NONE', #5399, #15891, #35881, .T. ) ;
#58913 = MECHANICAL_DESIGN_GEOMETRIC_PRESENTATION_REPRESENTATION (  '', ( #64537 ), #13962 ) ;
#58914 = CARTESIAN_POINT ( 'NONE',  ( -48.50000000000000000, 14.49137674618942562, 9.500000000000000000 ) ) ;
#58915 = CARTESIAN_POINT ( 'NONE',  ( -71.99999999999998579, 119.9999999999997868, 7.000000000000000000 ) ) ;
#58916 = ORIENTED_EDGE ( 'NONE', *, *, #4708, .T. ) ;
#58917 =( NAMED_UNIT ( * ) SI_UNIT ( $, .STERADIAN. ) SOLID_ANGLE_UNIT ( ) );
#58918 = CARTESIAN_POINT ( 'NONE',  ( 16.00000000000001776, 42.00000000000000000, -29.68999999999999417 ) ) ;
#58919 = AXIS2_PLACEMENT_3D ( 'NONE', #55642, #67232, #18708 ) ;
#58920 = CARTESIAN_POINT ( 'NONE',  ( 72.00000000000000000, 35.92875272052971525, -10.00000000000000000 ) ) ;
#58921 = CARTESIAN_POINT ( 'NONE',  ( -122.4549999999999983, 7.632228543268599452, -2.479861379858951942 ) ) ;
#58922 = VERTEX_POINT ( 'NONE', #30413 ) ;
#58923 = ORIENTED_EDGE ( 'NONE', *, *, #24779, .T. ) ;
#58924 = DIRECTION ( 'NONE',  ( 0.000000000000000000, 0.000000000000000000, -1.000000000000000000 ) ) ;
#58925 = DIRECTION ( 'NONE',  ( -0.000000000000000000, -0.000000000000000000, 1.000000000000000000 ) ) ;
#58926 = COLOUR_RGB ( '', 0.31764706, 0.68627451, 0.89019608) ;
#58927 = COLOUR_RGB ( '', 0.40784314, 0.44705882, 0.49803922) ;
#58928 = CARTESIAN_POINT ( 'NONE',  ( -163.5570736234661524, -1.166476076187852838E-15, -9.524999999999991473 ) ) ;
#58929 = CARTESIAN_POINT ( 'NONE',  ( 5.598654528085805993, 123.2449999999999903, 7.705886871421374629 ) ) ;
#58930 = CARTESIAN_POINT ( 'NONE',  ( -92.75707362346618368, -5.598654528085801552, 7.705886871421367523 ) ) ;
#58931 = EDGE_CURVE ( 'NONE', #4102, #29672, #51915, .T. ) ;
#58932 = DIRECTION ( 'NONE',  ( -0.000000000000000000, 1.000000000000000000, -0.000000000000000000 ) ) ;
#58933 = ORIENTED_EDGE ( 'NONE', *, *, #62902, .F. ) ;
#58934 = ADVANCED_FACE ( 'NONE', ( #39999 ), #19878, .F. ) ;
#58935 = DIRECTION ( 'NONE',  ( -0.000000000000000000, 1.000000000000000000, -0.000000000000000000 ) ) ;
#58936 = CARTESIAN_POINT ( 'NONE',  ( -7.794228634059947147, 2.500000000000000000, -4.500000000000000000 ) ) ;
#58937 = ADVANCED_FACE ( 'NONE', ( #31118 ), #64179, .F. ) ;
#58938 = VECTOR ( 'NONE', #42067, 1000.000000000000000 ) ;
#58939 = CARTESIAN_POINT ( 'NONE',  ( -140.6050000000000182, 6.826472737025113702, -4.959722759717902107 ) ) ;
#58940 = ADVANCED_FACE ( 'NONE', ( #69133 ), #36465, .F. ) ;
#58941 = CYLINDRICAL_SURFACE ( 'NONE', #67349, 1.000000000000000000 ) ;
#58942 =( NAMED_UNIT ( * ) PLANE_ANGLE_UNIT ( ) SI_UNIT ( $, .RADIAN. ) );
#58943 = CARTESIAN_POINT ( 'NONE',  ( -147.4449999999999932, 0.000000000000000000, 8.024999999999991473 ) ) ;
#58944 = CARTESIAN_POINT ( 'NONE',  ( -135.1449999999999818, -4.716976649647092401, 6.492361379858946790 ) ) ;
#58945 = ORIENTED_EDGE ( 'NONE', *, *, #11718, .F. ) ;
#58946 =( BOUNDED_SURFACE ( )  B_SPLINE_SURFACE ( 3, 2, ( 
 ( #16383, #1130, #55968 ),
 ( #13397, #29585, #43808 ),
 ( #23961, #56310, #21982 ),
 ( #13060, #38546, #34515 ),
 ( #49087, #11755, #774 ),
 ( #24304, #18696, #54661 ) ),
 .UNSPECIFIED., .F., .F., .F. ) 
 B_SPLINE_SURFACE_WITH_KNOTS ( ( 4, 2, 4 ),
 ( 3, 3 ),
 ( 1.570796326794896558, 2.356194490192344837, 3.141592653589793116 ),
 ( 0.000000000000000000, 1.000000000000000000 ),
 .UNSPECIFIED. ) 
 GEOMETRIC_REPRESENTATION_ITEM ( )  RATIONAL_B_SPLINE_SURFACE ( (
 ( 1.000000000000000000, 0.7071067811865523467, 1.000000000000000000),
 ( 1.000000000000000000, 0.6778979487215957001, 1.000000000000000000),
 ( 1.000000000000000000, 0.6465434225954497238, 1.000000000000000000),
 ( 1.000000000000000000, 0.5995650817090790730, 1.000000000000000000),
 ( 1.000000000000000000, 0.5843845446918550790, 1.000000000000000000),
 ( 1.000000000000000000, 0.5847102846637692863, 1.000000000000000000) ) ) 
 REPRESENTATION_ITEM ( '' )  SURFACE ( )  );
#58947 = CARTESIAN_POINT ( 'NONE',  ( 44.58498124287053344, 10.41703377194147073, -3.499556662980365829 ) ) ;
#58948 = CARTESIAN_POINT ( 'NONE',  ( -76.55707362346616662, -1.166476076187852838E-15, -9.524999999999991473 ) ) ;
#58949 = CARTESIAN_POINT ( 'NONE',  ( -52.25499999999999545, -4.716976649647092401, 6.492361379858946790 ) ) ;
#58950 = CARTESIAN_POINT ( 'NONE',  ( -15.48999599679679662, 117.9999999999999716, -7.000000000000000000 ) ) ;
#58951 = EDGE_CURVE ( 'NONE', #43499, #46838, #42711, .T. ) ;
#58952 = CARTESIAN_POINT ( 'NONE',  ( -138.4429263765337907, -1.166476076187852838E-15, -9.524999999999991473 ) ) ;
#58953 = CARTESIAN_POINT ( 'NONE',  ( -51.44292637653380496, -1.166476076187852838E-15, -9.524999999999991473 ) ) ;
#58954 = DIRECTION ( 'NONE',  ( -0.000000000000000000, 1.000000000000000000, -0.000000000000000000 ) ) ;
#58955 = CARTESIAN_POINT ( 'NONE',  ( -106.7929263765337851, -3.094860106618429807, 9.524999999999991473 ) ) ;
#58956 = DIRECTION ( 'NONE',  ( -1.103071622995683091E-16, 0.9242245927363028635, 0.3818493186865932199 ) ) ;
#58957 =( GEOMETRIC_REPRESENTATION_CONTEXT ( 3 ) GLOBAL_UNCERTAINTY_ASSIGNED_CONTEXT ( ( #50417 ) ) GLOBAL_UNIT_ASSIGNED_CONTEXT ( ( #52037, #24924, #63268 ) ) REPRESENTATION_CONTEXT ( 'NONE', 'WORKASPACE' ) );
#58958 = PLANE ( 'NONE',  #14738 ) ;
#58959 = AXIS2_PLACEMENT_3D ( 'NONE', #27652, #534, #6223 ) ;
#58960 = LINE ( 'NONE', #47773, #52844 ) ;
#58961 = PRESENTATION_STYLE_ASSIGNMENT (( #10434 ) ) ;
#58962 = AXIS2_PLACEMENT_3D ( 'NONE', #16411, #24558, #64200 ) ;
#58963 = FACE_OUTER_BOUND ( 'NONE', #34083, .T. ) ;
#58964 = EDGE_CURVE ( 'NONE', #40506, #2776, #15711, .T. ) ;
#58965 = DIRECTION ( 'NONE',  ( 0.000000000000000000, 0.000000000000000000, 1.000000000000000000 ) ) ;
#58966 = CARTESIAN_POINT ( 'NONE',  ( -60.00000000000000000, -2.024042244987997205E-14, -6.500000000000000000 ) ) ;
#58968 = VERTEX_POINT ( 'NONE', #58219 ) ;
#58967 = VECTOR ( 'NONE', #46379, 1000.000000000000114 ) ;
#58969 = CARTESIAN_POINT ( 'NONE',  ( 15.48999599679679662, 146.9999999999999716, 7.000000000000000000 ) ) ;
#58970 = STYLED_ITEM ( 'NONE', ( #61304 ), #6072 ) ;
#58971 = ADVANCED_FACE ( 'NONE', ( #53962 ), #20146, .T. ) ;
#58972 = CARTESIAN_POINT ( 'NONE',  ( -7.632228543268607446, 109.6570736234661609, -2.479861379858953718 ) ) ;
#58973 = AXIS2_PLACEMENT_3D ( 'NONE', #44255, #55795, #66343 ) ;
#58974 = ORIENTED_EDGE ( 'NONE', *, *, #5273, .T. ) ;
#58975 = ORIENTED_EDGE ( 'NONE', *, *, #2497, .F. ) ;
#58976 = CARTESIAN_POINT ( 'NONE',  ( 6.062177826491067734, -2.500000000000000000, 3.500000000000000000 ) ) ;
#58977 = CARTESIAN_POINT ( 'NONE',  ( -20.76401515593078884, 149.8168068008927492, 9.892342186632994583 ) ) ;
#58978 = VERTEX_POINT ( 'NONE', #26857 ) ;
#58979 = CARTESIAN_POINT ( 'NONE',  ( -5.598654528085808657, 129.7549999999999955, 7.705886871421373741 ) ) ;
#58980 = FILL_AREA_STYLE_COLOUR ( '', #53510 ) ;
#58981 = SURFACE_STYLE_FILL_AREA ( #31539 ) ;
#58982 = PRESENTATION_LAYER_ASSIGNMENT (  '', '', ( #42326 ) ) ;
#58983 = CARTESIAN_POINT ( 'NONE',  ( -98.99499999999997613, -6.826472737025115478, 4.959722759717900331 ) ) ;
#58984 = EDGE_LOOP ( 'NONE', ( #56178, #27985, #42834, #4810 ) ) ;
#58985 = DIRECTION ( 'NONE',  ( 0.000000000000000000, 0.000000000000000000, -1.000000000000000000 ) ) ;
#58986 =( NAMED_UNIT ( * ) SI_UNIT ( $, .STERADIAN. ) SOLID_ANGLE_UNIT ( ) );
#58987 = AXIS2_PLACEMENT_3D ( 'NONE', #28368, #39678, #61767 ) ;
#58988 = ORIENTED_EDGE ( 'NONE', *, *, #30114, .F. ) ;
#58989 = CARTESIAN_POINT ( 'NONE',  ( 0.000000000000000000, 152.9429263765338192, -8.025000000000000355 ) ) ;
#58990 = CARTESIAN_POINT ( 'NONE',  ( -74.99999999999998579, 64.49137674618943095, -9.500000000000000000 ) ) ;
#58991 = DIRECTION ( 'NONE',  ( -1.189524669241239855E-16, -1.000000000000000000, 0.000000000000000000 ) ) ;
#58992 = SURFACE_SIDE_STYLE ('',( #69539 ) ) ;
#58993 = ADVANCED_FACE ( 'NONE', ( #64543 ), #58946, .T. ) ;
#58994 = CARTESIAN_POINT ( 'NONE',  ( -1.011095968855053334E-15, -8.500000000000000000, 3.000000000000000000 ) ) ;
#58995 = EDGE_LOOP ( 'NONE', ( #43024, #51603, #65462, #3282 ) ) ;
#58996 = LINE ( 'NONE', #65309, #59638 ) ;
#58997 = CARTESIAN_POINT ( 'NONE',  ( 0.000000000000000000, 2.299999999999999822, 0.000000000000000000 ) ) ;
#58998 = CARTESIAN_POINT ( 'NONE',  ( 74.89452121010485541, 13.00000000000000178, 66.39042820928573008 ) ) ;
#58999 = PRESENTATION_STYLE_ASSIGNMENT (( #57979 ) ) ;
#59000 = MECHANICAL_DESIGN_GEOMETRIC_PRESENTATION_REPRESENTATION (  '', ( #68015 ), #42246 ) ;
#59001 = EDGE_CURVE ( 'NONE', #66131, #13709, #22313, .T. ) ;
#59002 = FACE_OUTER_BOUND ( 'NONE', #44194, .T. ) ;
#59003 = LINE ( 'NONE', #63588, #65187 ) ;
#59004 = CARTESIAN_POINT ( 'NONE',  ( -5.038399427696178101, 153.9194349410952043, 7.410012812680824013 ) ) ;
#59005 = VERTEX_POINT ( 'NONE', #65218 ) ;
#59006 = ORIENTED_EDGE ( 'NONE', *, *, #6435, .T. ) ;
#59007 = CARTESIAN_POINT ( 'NONE',  ( 0.000000000000000000, 50.00000000000000000, 60.00000000000000000 ) ) ;
#59008 = DIRECTION ( 'NONE',  ( 0.000000000000000000, 1.000000000000000000, 0.000000000000000000 ) ) ;
#59009 = CARTESIAN_POINT ( 'NONE',  ( -15.75000000000000000, -0.9999999999999995559, 19.00000000000000000 ) ) ;
#59011 = FACE_OUTER_BOUND ( 'NONE', #17900, .T. ) ;
#59010 = VECTOR ( 'NONE', #22690, 1000.000000000000000 ) ;
#59012 = VERTEX_POINT ( 'NONE', #33223 ) ;
#59013 = CARTESIAN_POINT ( 'NONE',  ( -47.50000000000000000, 13.41640786499872284, 9.500000000000000000 ) ) ;
#59014 = EDGE_CURVE ( 'NONE', #50552, #17866, #22666, .T. ) ;
#59015 = CARTESIAN_POINT ( 'NONE',  ( -171.6550000000000011, -7.632228543268600340, -2.479861379858950166 ) ) ;
#59016 = CARTESIAN_POINT ( 'NONE',  ( 61.99999999999998579, 31.24999999999999289, -3.750000000000000000 ) ) ;
#59017 = CARTESIAN_POINT ( 'NONE',  ( -148.4070736234666015, 3.094860106611302619, -9.525000000005171330 ) ) ;
#59018 = CARTESIAN_POINT ( 'NONE',  ( -173.8449999999999989, -7.632228543268599452, 2.479861379858951054 ) ) ;
#59019 =( GEOMETRIC_REPRESENTATION_CONTEXT ( 3 ) GLOBAL_UNCERTAINTY_ASSIGNED_CONTEXT ( ( #15023 ) ) GLOBAL_UNIT_ASSIGNED_CONTEXT ( ( #594, #43612, #59741 ) ) REPRESENTATION_CONTEXT ( 'NONE', 'WORKASPACE' ) );
#59020 = VECTOR ( 'NONE', #5869, 1000.000000000000000 ) ;
#59021 = CARTESIAN_POINT ( 'NONE',  ( -165.5949999999999420, 2.607480562269072433, 8.024999999999991473 ) ) ;
#59022 = VERTEX_POINT ( 'NONE', #49407 ) ;
#59023 = CARTESIAN_POINT ( 'NONE',  ( -195.0000000000000000, 0.000000000000000000, 0.000000000000000000 ) ) ;
#59024 = CARTESIAN_POINT ( 'NONE',  ( -4.750000000000002665, 24.74999999999998579, 3.750000000000000000 ) ) ;
#59025 = LINE ( 'NONE', #47482, #47326 ) ;
#59026 = CARTESIAN_POINT ( 'NONE',  ( -84.50499999999999545, -6.826472737025115478, -4.959722759717899443 ) ) ;
#59027 = CARTESIAN_POINT ( 'NONE',  ( 0.000000000000000000, 42.00000000000000000, -36.49999999999999289 ) ) ;
#59028 = LINE ( 'NONE', #53734, #62915 ) ;
#59029 = CARTESIAN_POINT ( 'NONE',  ( -74.49999999999998579, 36.50926243676796190, -10.00000000000000000 ) ) ;
#59030 = EDGE_CURVE ( 'NONE', #13725, #51712, #66535, .T. ) ;
#59031 = CARTESIAN_POINT ( 'NONE',  ( -83.24499999999999034, -4.716976649647093289, -6.492361379858945902 ) ) ;
#59032 = CARTESIAN_POINT ( 'NONE',  ( 9.058813317711338797, 139.9549999999999841, -2.943386871421372675 ) ) ;
#59033 = MECHANICAL_DESIGN_GEOMETRIC_PRESENTATION_REPRESENTATION (  '', ( #68044 ), #23087 ) ;
#59034 = LINE ( 'NONE', #16152, #64043 ) ;
#59035 = DIRECTION ( 'NONE',  ( -0.000000000000000000, 0.000000000000000000, -1.000000000000000000 ) ) ;
#59036 = AXIS2_PLACEMENT_3D ( 'NONE', #48640, #37753, #64069 ) ;
#59037 = PRESENTATION_STYLE_ASSIGNMENT (( #32631 ) ) ;
#59038 = VERTEX_POINT ( 'NONE', #18356 ) ;
#59039 = CIRCLE ( 'NONE', #44477, 0.4999999999999991118 ) ;
#59040 = DIRECTION ( 'NONE',  ( 0.7071067811865549002, 8.659560562355021605E-17, -0.7071067811865402453 ) ) ;
#59041 =( NAMED_UNIT ( * ) SI_UNIT ( $, .STERADIAN. ) SOLID_ANGLE_UNIT ( ) );
#59042 =( LENGTH_UNIT ( ) NAMED_UNIT ( * ) SI_UNIT ( .MILLI., .METRE. ) );
#59043 = DIRECTION ( 'NONE',  ( 0.000000000000000000, 0.000000000000000000, 1.000000000000000000 ) ) ;
#59044 = ORIENTED_EDGE ( 'NONE', *, *, #16095, .T. ) ;
#59045 = ORIENTED_EDGE ( 'NONE', *, *, #8369, .T. ) ;
#59046 = DIRECTION ( 'NONE',  ( -0.000000000000000000, -0.000000000000000000, 1.000000000000000000 ) ) ;
#59047 = CARTESIAN_POINT ( 'NONE',  ( -174.2070736234663570, 3.094860106620215046, 9.524999999998700062 ) ) ;
#59048 = CARTESIAN_POINT ( 'NONE',  ( -4.716976649647098618, 148.1429263765338078, 6.492361379858953008 ) ) ;
#59049 = CYLINDRICAL_SURFACE ( 'NONE', #59934, 8.025000000000000355 ) ;
#59050 = ORIENTED_EDGE ( 'NONE', *, *, #50219, .F. ) ;
#59051 = CARTESIAN_POINT ( 'NONE',  ( -115.8549999999999898, 4.716976649647094177, 6.492361379858945902 ) ) ;
#59052 = EDGE_LOOP ( 'NONE', ( #53001, #61170, #24043, #56304, #39640 ) ) ;
#59053 = DIRECTION ( 'NONE',  ( 1.300977106640434891E-16, -0.000000000000000000, 1.000000000000000000 ) ) ;
#59054 = CARTESIAN_POINT ( 'NONE',  ( 74.65811388300841145, 19.88603796100278487, 6.000000000000000888 ) ) ;
#59055 = ORIENTED_EDGE ( 'NONE', *, *, #6581, .T. ) ;
#59056 = SPHERICAL_SURFACE ( 'NONE', #9996, 0.5000000000000000000 ) ;
#59057 = CARTESIAN_POINT ( 'NONE',  ( -60.00000000000000000, -2.024042244987997205E-14, 12.00000000000000000 ) ) ;
#59058 = VERTEX_POINT ( 'NONE', #17067 ) ;
#59059 = AXIS2_PLACEMENT_3D ( 'NONE', #53363, #37578, #20289 ) ;
#59060 = TOROIDAL_SURFACE ( 'NONE', #28718, 0.5000000000000000000, 0.2500000000000000000 ) ;
#59061 = CARTESIAN_POINT ( 'NONE',  ( 7.794228634059945371, 2.500000000000000000, 4.500000000000000888 ) ) ;
#59062 = CARTESIAN_POINT ( 'NONE',  ( -9.058813317711338797, 155.3449999999999704, 2.943386871421373563 ) ) ;
#59063 = DIRECTION ( 'NONE',  ( -0.000000000000000000, -1.000000000000000000, -0.000000000000000000 ) ) ;
#59064 = EDGE_LOOP ( 'NONE', ( #48624, #1214, #68938, #19701 ) ) ;
#59065 = FILL_AREA_STYLE ('',( #11916 ) ) ;
#59066 = CARTESIAN_POINT ( 'NONE',  ( -181.9429263765338192, 0.000000000000000000, 9.524999999999991473 ) ) ;
#59067 = VERTEX_POINT ( 'NONE', #59938 ) ;
#59068 = CARTESIAN_POINT ( 'NONE',  ( 7.632228543268607446, 125.0429263765337993, 2.479861379858954606 ) ) ;
#59069 = DIRECTION ( 'NONE',  ( 0.8660254037844387076, 0.000000000000000000, -0.5000000000000000000 ) ) ;
#59070 = DIRECTION ( 'NONE',  ( -1.000000000000000000, 0.000000000000000000, 0.000000000000000000 ) ) ;
#59071 = FILL_AREA_STYLE ('',( #5940 ) ) ;
#59072 = CIRCLE ( 'NONE', #12976, 4.999999999999997335 ) ;
#59073 = SURFACE_STYLE_USAGE ( .BOTH. , #68960 ) ;
#59074 = VERTEX_POINT ( 'NONE', #5763 ) ;
#59075 = CIRCLE ( 'NONE', #2845, 1.000000000000000888 ) ;
#59076 = EDGE_CURVE ( 'NONE', #8197, #21622, #32543, .T. ) ;
#59077 = CARTESIAN_POINT ( 'NONE',  ( 5.365183871890743639, -4.707228941936128841, 0.1074872947962652175 ) ) ;
#59078 = ORIENTED_EDGE ( 'NONE', *, *, #48807, .T. ) ;
#59079 = CARTESIAN_POINT ( 'NONE',  ( -53.24292637653380211, 5.598654528085804216, 7.705886871421366635 ) ) ;
#59080 = AXIS2_PLACEMENT_3D ( 'NONE', #31047, #41298, #69056 ) ;
#59081 = DIRECTION ( 'NONE',  ( 0.000000000000000000, 0.000000000000000000, 1.000000000000000000 ) ) ;
#59082 = DIRECTION ( 'NONE',  ( 0.000000000000000000, 0.000000000000000000, 1.000000000000000000 ) ) ;
#59083 = CARTESIAN_POINT ( 'NONE',  ( -143.4550000000000125, 7.632228543268599452, -2.479861379858951942 ) ) ;
#59084 = CARTESIAN_POINT ( 'NONE',  ( -176.0070736234661695, -8.102448949553174629, -5.886773742842741797 ) ) ;
#59085 = DIRECTION ( 'NONE',  ( 0.000000000000000000, 0.000000000000000000, 1.000000000000000000 ) ) ;
#59086 = AXIS2_PLACEMENT_3D ( 'NONE', #10541, #31978, #53452 ) ;
#59087 = CARTESIAN_POINT ( 'NONE',  ( 7.000000000000017764, 43.00000000000000000, -28.00000000000000000 ) ) ;
#59088 = FACE_OUTER_BOUND ( 'NONE', #66938, .T. ) ;
#59089 = ORIENTED_EDGE ( 'NONE', *, *, #39111, .F. ) ;
#59090 = EDGE_CURVE ( 'NONE', #34430, #44609, #6138, .T. ) ;
#59091 = VERTEX_POINT ( 'NONE', #16722 ) ;
#59092 = CARTESIAN_POINT ( 'NONE',  ( -56.90499999999998693, 2.607480562269068880, -8.024999999999993250 ) ) ;
#59093 = ORIENTED_EDGE ( 'NONE', *, *, #6267, .F. ) ;
#59094 = LINE ( 'NONE', #4580, #24724 ) ;
#59095 = EDGE_CURVE ( 'NONE', #67644, #13443, #7776, .T. ) ;
#59096 = SURFACE_SIDE_STYLE ('',( #6314 ) ) ;
#59097 = DIRECTION ( 'NONE',  ( 0.000000000000000000, 1.000000000000000000, 0.000000000000000000 ) ) ;
#59098 = ADVANCED_FACE ( 'NONE', ( #34860 ), #4206, .F. ) ;
#59099 = EDGE_CURVE ( 'NONE', #1731, #46991, #38185, .T. ) ;
#59100 = FACE_OUTER_BOUND ( 'NONE', #69427, .T. ) ;
#59101 = CARTESIAN_POINT ( 'NONE',  ( -129.4429263765338192, -1.166476076187852838E-15, -9.524999999999991473 ) ) ;
#59102 = ORIENTED_EDGE ( 'NONE', *, *, #47560, .T. ) ;
#59103 = VECTOR ( 'NONE', #61524, 1000.000000000000000 ) ;
#59104 = ADVANCED_FACE ( 'NONE', ( #47200 ), #62973, .F. ) ;
#59105 = CARTESIAN_POINT ( 'NONE',  ( 6.826472737025121695, 126.6070736234661496, -4.959722759717905660 ) ) ;
#59106 = CARTESIAN_POINT ( 'NONE',  ( -111.8949999999999960, 6.826472737025115478, 4.959722759717899443 ) ) ;
#59107 = CARTESIAN_POINT ( 'NONE',  ( -3.094860106618432471, 157.5949999999999989, -9.525000000000000355 ) ) ;
#59108 = CARTESIAN_POINT ( 'NONE',  ( -84.89499999999996760, 6.826472737025116366, 4.959722759717898555 ) ) ;
#59109 = SURFACE_STYLE_FILL_AREA ( #44377 ) ;
#59110 = CARTESIAN_POINT ( 'NONE',  ( -195.0000000000000000, 0.000000000000000000, 0.000000000000000000 ) ) ;
#59111 = DIRECTION ( 'NONE',  ( 0.000000000000000000, 0.000000000000000000, 1.000000000000000000 ) ) ;
#59112 = DIRECTION ( 'NONE',  ( 0.000000000000000000, 0.000000000000000000, 1.000000000000000000 ) ) ;
#59113 = VERTEX_POINT ( 'NONE', #9884 ) ;
#59114 = CARTESIAN_POINT ( 'NONE',  ( -137.5429263765338135, 9.058813317711329915, 2.943386871421369566 ) ) ;
#59115 = CARTESIAN_POINT ( 'NONE',  ( -150.8950000000000102, 6.826472737025116366, 4.959722759717898555 ) ) ;
#59116 = AXIS2_PLACEMENT_3D ( 'NONE', #12231, #44658, #39365 ) ;
#59117 = CARTESIAN_POINT ( 'NONE',  ( -67.55707362346618083, -1.166476076187852838E-15, -9.524999999999991473 ) ) ;
#59118 = ORIENTED_EDGE ( 'NONE', *, *, #61376, .F. ) ;
#59119 = EDGE_LOOP ( 'NONE', ( #47019, #32664, #39486, #33727 ) ) ;
#59120 = SURFACE_STYLE_USAGE ( .BOTH. , #26071 ) ;
#59121 = FILL_AREA_STYLE ('',( #28384 ) ) ;
#59122 = CARTESIAN_POINT ( 'NONE',  ( -45.70684385664927163, 8.620779964796652095, 6.438673729884040853 ) ) ;
#59123 = SURFACE_STYLE_FILL_AREA ( #54195 ) ;
#59124 = CARTESIAN_POINT ( 'NONE',  ( -151.3429263765337964, -9.058813317711329915, 2.943386871421371787 ) ) ;
#59125 = ORIENTED_EDGE ( 'NONE', *, *, #14449, .T. ) ;
#59126 = CARTESIAN_POINT ( 'NONE',  ( -146.6049999999999898, 6.826472737025113702, -4.959722759717902107 ) ) ;
#59127 = ORIENTED_EDGE ( 'NONE', *, *, #18109, .F. ) ;
#59128 = FILL_AREA_STYLE_COLOUR ( '', #27870 ) ;
#59129 = CARTESIAN_POINT ( 'NONE',  ( -142.1070736234661638, 8.102448949553172852, -5.886773742842744461 ) ) ;
#59130 = ORIENTED_EDGE ( 'NONE', *, *, #55098, .T. ) ;
#59131 = CARTESIAN_POINT ( 'NONE',  ( 3.000000000000030198, 38.70020753820971748, 89.00000000000000000 ) ) ;
#59132 = DIRECTION ( 'NONE',  ( -0.000000000000000000, 1.000000000000000000, -0.000000000000000000 ) ) ;
#59133 = CARTESIAN_POINT ( 'NONE',  ( -8.102448949553181734, 118.8949999999999676, -5.886773742842749790 ) ) ;
#59134 = CARTESIAN_POINT ( 'NONE',  ( -4.000000000000000000, 4.336808689942018722E-16, 24.00000000000000000 ) ) ;
#59135 = ORIENTED_EDGE ( 'NONE', *, *, #30476, .T. ) ;
#59136 = DIRECTION ( 'NONE',  ( 1.000000000000000000, 1.601283208593975100E-14, 0.000000000000000000 ) ) ;
#59137 = CARTESIAN_POINT ( 'NONE',  ( 5.598654528085805993, 133.3549999999999898, 7.705886871421374629 ) ) ;
#59138 = CARTESIAN_POINT ( 'NONE',  ( -65.45499999999998408, 7.632228543268599452, -2.479861379858951942 ) ) ;
#59139 = CARTESIAN_POINT ( 'NONE',  ( -124.1950000000000074, 8.437984349512085203, -1.550032578732815448E-15 ) ) ;
#59140 = ORIENTED_EDGE ( 'NONE', *, *, #20702, .T. ) ;
#59141 = CARTESIAN_POINT ( 'NONE',  ( -5.598654528085808657, 144.7549999999999955, 7.705886871421373741 ) ) ;
#59142 =( NAMED_UNIT ( * ) SI_UNIT ( $, .STERADIAN. ) SOLID_ANGLE_UNIT ( ) );
#59143 = AXIS2_PLACEMENT_3D ( 'NONE', #36092, #42443, #52625 ) ;
#59144 = DIRECTION ( 'NONE',  ( 1.000000000000000000, -0.000000000000000000, 0.000000000000000000 ) ) ;
#59145 = CARTESIAN_POINT ( 'NONE',  ( 92.41620014002536720, 5.000000000000000000, -24.00402776293825369 ) ) ;
#59146 = AXIS2_PLACEMENT_3D ( 'NONE', #21787, #38699, #22474 ) ;
#59147 = EDGE_CURVE ( 'NONE', #38125, #56906, #46449, .T. ) ;
#59148 = LINE ( 'NONE', #26454, #35140 ) ;
#59149 = CIRCLE ( 'NONE', #68162, 30.00000000000000000 ) ;
#59150 = ORIENTED_EDGE ( 'NONE', *, *, #44925, .F. ) ;
#59151 = DIRECTION ( 'NONE',  ( -1.000000000000000000, 0.000000000000000000, 0.000000000000000000 ) ) ;
#59152 = CARTESIAN_POINT ( 'NONE',  ( -168.3550000000000182, -4.716976649647093289, -6.492361379858945902 ) ) ;
#59153 = ORIENTED_EDGE ( 'NONE', *, *, #13098, .F. ) ;
#59154 = DIRECTION ( 'NONE',  ( 0.000000000000000000, 0.000000000000000000, 1.000000000000000000 ) ) ;
#59155 = EDGE_CURVE ( 'NONE', #38116, #62934, #35915, .T. ) ;
#59156 = DIRECTION ( 'NONE',  ( 0.000000000000000000, 0.000000000000000000, 1.000000000000000000 ) ) ;
#59157 = DIRECTION ( 'NONE',  ( 0.000000000000000000, 1.000000000000000000, 0.000000000000000000 ) ) ;
#59158 = ORIENTED_EDGE ( 'NONE', *, *, #26578, .T. ) ;
#59159 =( NAMED_UNIT ( * ) PLANE_ANGLE_UNIT ( ) SI_UNIT ( $, .RADIAN. ) );
#59160 = CARTESIAN_POINT ( 'NONE',  ( -190.0000000000000000, 0.000000000000000000, 0.000000000000000000 ) ) ;
#59161 = CARTESIAN_POINT ( 'NONE',  ( -84.35499999999998977, -4.716976649647093289, -6.492361379858945902 ) ) ;
#59162 = VERTEX_POINT ( 'NONE', #9548 ) ;
#59163 =( NAMED_UNIT ( * ) SI_UNIT ( $, .STERADIAN. ) SOLID_ANGLE_UNIT ( ) );
#59164 = EDGE_CURVE ( 'NONE', #35564, #59936, #14116, .T. ) ;
#59165 = DIRECTION ( 'NONE',  ( -0.000000000000000000, -1.000000000000000000, -0.000000000000000000 ) ) ;
#59166 = SURFACE_STYLE_USAGE ( .BOTH. , #11687 ) ;
#59167 = CARTESIAN_POINT ( 'NONE',  ( -62.45707362346617231, -9.058813317711329915, 2.943386871421371787 ) ) ;
#59168 = AXIS2_PLACEMENT_3D ( 'NONE', #514, #27633, #65977 ) ;
#59169 = ADVANCED_FACE ( 'NONE', ( #14437 ), #66110, .T. ) ;
#59170 = CARTESIAN_POINT ( 'NONE',  ( 22.00000000000000355, 42.47058823529412308, -74.11764705882353610 ) ) ;
#59171 = EDGE_LOOP ( 'NONE', ( #1507, #15393, #34221, #31600 ) ) ;
#59172 = DIRECTION ( 'NONE',  ( 1.000000000000000000, 0.000000000000000000, -4.625929269271505635E-16 ) ) ;
#59174 = CYLINDRICAL_SURFACE ( 'NONE', #39256, 0.5000000000000004441 ) ;
#59173 = LINE ( 'NONE', #59877, #54910 ) ;
#59175 = CARTESIAN_POINT ( 'NONE',  ( -111.5049999999999955, -6.826472737025115478, -4.959722759717899443 ) ) ;
#59176 = CARTESIAN_POINT ( 'NONE',  ( -9.058813317711337021, 125.0449999999999875, -2.943386871421374895 ) ) ;
#59177 = CARTESIAN_POINT ( 'NONE',  ( -117.7449999999999903, 4.716976649647094177, 6.492361379858945902 ) ) ;
#59178 =( NAMED_UNIT ( * ) PLANE_ANGLE_UNIT ( ) SI_UNIT ( $, .RADIAN. ) );
#59179 = FILL_AREA_STYLE ('',( #37808 ) ) ;
#59180 = CARTESIAN_POINT ( 'NONE',  ( -166.3429263765337964, -9.058813317711329915, 2.943386871421371787 ) ) ;
#59181 = CARTESIAN_POINT ( 'NONE',  ( -178.6450000000000102, 4.716976649647091513, -6.492361379858946790 ) ) ;
#59182 = EDGE_CURVE ( 'NONE', #30209, #10224, #2151, .T. ) ;
#59183 = CIRCLE ( 'NONE', #51334, 1.000000000000000888 ) ;
#59184 = DIRECTION ( 'NONE',  ( -1.000000000000000000, 0.000000000000000000, 0.000000000000000000 ) ) ;
#59185 = CARTESIAN_POINT ( 'NONE',  ( -47.71347897792735182, -13.42724224818811862, 0.9185643661977266339 ) ) ;
#59186 = DIRECTION ( 'NONE',  ( -0.9704308468600219006, 0.2413793103448194921, 0.000000000000000000 ) ) ;
#59187 = DIRECTION ( 'NONE',  ( 0.000000000000000000, 0.000000000000000000, 1.000000000000000000 ) ) ;
#59188 = ORIENTED_EDGE ( 'NONE', *, *, #66382, .T. ) ;
#59189 = CARTESIAN_POINT ( 'NONE',  ( -77.09292637653378222, 3.094860106618433360, 9.524999999999991473 ) ) ;
#59190 = CARTESIAN_POINT ( 'NONE',  ( 3.851859888774471706E-31, -8.500000000000000000, 24.00000000000000000 ) ) ;
#59191 = DIRECTION ( 'NONE',  ( 1.000000000000000000, 0.000000000000000000, -1.300977106640435137E-16 ) ) ;
#59192 = ADVANCED_FACE ( 'NONE', ( #59780 ), #34677, .F. ) ;
#59193 = FILL_AREA_STYLE_COLOUR ( '', #69689 ) ;
#59195 = SURFACE_STYLE_FILL_AREA ( #27177 ) ;
#59194 =( BOUNDED_CURVE ( )  B_SPLINE_CURVE ( 2, ( #15231, #62335, #61977, #35261, #51437, #67616, #4247, #46907, #35617, #19419, #40916 ),
 .UNSPECIFIED., .F., .F. ) 
 B_SPLINE_CURVE_WITH_KNOTS ( ( 3, 2, 2, 2, 2, 3 ),
 ( 0.06521739130434635323, 0.06739130434782455992, 0.06956521739130278048, 0.07173913043478098717, 0.07391304347825920773, 0.07608695652173741442 ),
 .UNSPECIFIED. ) 
 CURVE ( )  GEOMETRIC_REPRESENTATION_ITEM ( )  RATIONAL_B_SPLINE_CURVE ( ( 1.000000000000033085, 0.9510565162951203355, 1.000000000000000000, 0.9510565162951535312, 1.000000000000000000, 0.9510565162951535312, 1.000000000000000000, 0.9510565162951535312, 1.000000000000000000, 0.9510565162951922780, 0.9999999999999612532 ) ) 
 REPRESENTATION_ITEM ( '' )  );
#59196 = DIRECTION ( 'NONE',  ( -0.000000000000000000, 1.000000000000000000, 0.000000000000000000 ) ) ;
#59197 = CIRCLE ( 'NONE', #62626, 14.49999999999999822 ) ;
#59198 = CARTESIAN_POINT ( 'NONE',  ( -177.6550000000000011, -7.632228543268600340, -2.479861379858950166 ) ) ;
#59199 = EDGE_LOOP ( 'NONE', ( #42186, #63687, #44656, #10787, #30124, #50968, #11891, #31483, #69268, #14809 ) ) ;
#59200 = CYLINDRICAL_SURFACE ( 'NONE', #8942, 4.999999999999997335 ) ;
#59201 =( LENGTH_UNIT ( ) NAMED_UNIT ( * ) SI_UNIT ( .MILLI., .METRE. ) );
#59202 = DIRECTION ( 'NONE',  ( -1.000000000000000000, -0.000000000000000000, 1.300977106640434891E-16 ) ) ;
#59203 = FILL_AREA_STYLE_COLOUR ( '', #10620 ) ;
#59204 = SURFACE_STYLE_FILL_AREA ( #43106 ) ;
#59205 = CARTESIAN_POINT ( 'NONE',  ( 2.607480562269076430, 141.9070736234661183, -8.025000000000000355 ) ) ;
#59206 = EDGE_LOOP ( 'NONE', ( #41838, #6127, #45898 ) ) ;
#59207 =( LENGTH_UNIT ( ) NAMED_UNIT ( * ) SI_UNIT ( .MILLI., .METRE. ) );
#59208 = CARTESIAN_POINT ( 'NONE',  ( -94.55499999999999261, 0.000000000000000000, 8.024999999999991473 ) ) ;
#59209 = CARTESIAN_POINT ( 'NONE',  ( 23.21231517720797655, 118.4999999999999716, -7.000000000000000000 ) ) ;
#59210 = ORIENTED_EDGE ( 'NONE', *, *, #30893, .T. ) ;
#59211 = SURFACE_STYLE_FILL_AREA ( #53613 ) ;
#59212 = EDGE_CURVE ( 'NONE', #53146, #33379, #5571, .T. ) ;
#59213 = CARTESIAN_POINT ( 'NONE',  ( -17.75000000000000355, -3.000000000000000000, 24.00000000000000000 ) ) ;
#59214 = ADVANCED_FACE ( 'NONE', ( #65410 ), #47913, .F. ) ;
#59215 = CARTESIAN_POINT ( 'NONE',  ( -90.05707362346616662, 0.000000000000000000, 9.524999999999991473 ) ) ;
#59216 = FACE_OUTER_BOUND ( 'NONE', #56212, .T. ) ;
#59217 = CARTESIAN_POINT ( 'NONE',  ( 3.542752237027638085, -1.835478060177118120, 9.000000000000003553 ) ) ;
#59218 = ORIENTED_EDGE ( 'NONE', *, *, #10087, .F. ) ;
#59219 = CARTESIAN_POINT ( 'NONE',  ( -65.24499999999999034, -4.716976649647093289, -6.492361379858945902 ) ) ;
#59220 = EDGE_LOOP ( 'NONE', ( #64334, #28133, #705, #52679 ) ) ;
#59221 = DIRECTION ( 'NONE',  ( 1.000000000000000000, 0.000000000000000000, -0.000000000000000000 ) ) ;
#59222 = ADVANCED_FACE ( 'NONE', ( #23517 ), #12259, .T. ) ;
#59223 = CARTESIAN_POINT ( 'NONE',  ( -125.3070736234661808, -10.01517768586948698, 6.132527647946031529E-16 ) ) ;
#59224 = EDGE_LOOP ( 'NONE', ( #25223, #67900, #29179, #6808 ) ) ;
#59225 = DIRECTION ( 'NONE',  ( -1.000000000000000000, 0.000000000000000000, 0.000000000000000000 ) ) ;
#59226 = EDGE_LOOP ( 'NONE', ( #59552, #26786, #6553 ) ) ;
#59227 = AXIS2_PLACEMENT_3D ( 'NONE', #28691, #43896, #2246 ) ;
#59228 = CARTESIAN_POINT ( 'NONE',  ( 26.00000000000001776, 42.00000000000000000, 29.68999999999999417 ) ) ;
#59229 = CARTESIAN_POINT ( 'NONE',  ( -123.2049999999999699, -2.607480562269071545, -8.024999999999991473 ) ) ;
#59230 = ORIENTED_EDGE ( 'NONE', *, *, #41104, .T. ) ;
#59231 = AXIS2_PLACEMENT_3D ( 'NONE', #38712, #16207, #53470 ) ;
#59232 = CARTESIAN_POINT ( 'NONE',  ( -73.34292637653381064, -9.058813317711329915, 2.943386871421371787 ) ) ;
#59233 = ORIENTED_EDGE ( 'NONE', *, *, #31688, .F. ) ;
#59234 = ADVANCED_FACE ( 'NONE', ( #44350 ), #50613, .T. ) ;
#59235 = CARTESIAN_POINT ( 'NONE',  ( -160.6429263765338362, -5.598654528085801552, 7.705886871421367523 ) ) ;
#59236 = DIRECTION ( 'NONE',  ( 0.000000000000000000, -1.000000000000000000, -0.000000000000000000 ) ) ;
#59237 = DIRECTION ( 'NONE',  ( 0.000000000000000000, 0.000000000000000000, -1.000000000000000000 ) ) ;
#59238 = CARTESIAN_POINT ( 'NONE',  ( -161.4570736234661865, -9.058813317711329915, 2.943386871421371787 ) ) ;
#59239 = PRODUCT_DEFINITION_SHAPE ( 'NONE', 'NONE',  #69714 ) ;
#59240 = CARTESIAN_POINT ( 'NONE',  ( -9.058813317711338797, 128.3449999999999989, 2.943386871421373563 ) ) ;
#59241 = CARTESIAN_POINT ( 'NONE',  ( -96.95707362346617231, 9.058813317711329915, -2.943386871421373119 ) ) ;
#59242 = EDGE_CURVE ( 'NONE', #48045, #27359, #68521, .T. ) ;
#59243 = LINE ( 'NONE', #37526, #14487 ) ;
#59244 = VERTEX_POINT ( 'NONE', #66084 ) ;
#59245 = DIRECTION ( 'NONE',  ( -1.000000000000000000, 0.000000000000000000, 0.000000000000000000 ) ) ;
#59246 = SURFACE_SIDE_STYLE ('',( #55010 ) ) ;
#59247 = FILL_AREA_STYLE_COLOUR ( '', #55685 ) ;
#59248 = VECTOR ( 'NONE', #63316, 1000.000000000000000 ) ;
#59249 = CARTESIAN_POINT ( 'NONE',  ( -135.8049999999999500, -8.437984349512085203, 5.166775262442717831E-16 ) ) ;
#59250 =( NAMED_UNIT ( * ) PLANE_ANGLE_UNIT ( ) SI_UNIT ( $, .RADIAN. ) );
#59251 = LINE ( 'NONE', #26559, #63969 ) ;
#59252 = DIRECTION ( 'NONE',  ( 0.000000000000000000, 0.000000000000000000, 1.000000000000000000 ) ) ;
#59253 = CARTESIAN_POINT ( 'NONE',  ( -144.2950000000000159, -2.607480562269069768, 8.024999999999991473 ) ) ;
#59254 = CARTESIAN_POINT ( 'NONE',  ( -141.5949999999999989, 2.607480562269072433, 8.024999999999991473 ) ) ;
#59255 = ORIENTED_EDGE ( 'NONE', *, *, #50771, .F. ) ;
#59256 = CARTESIAN_POINT ( 'NONE',  ( 44.56131952741539237, 9.853773175805059736, -3.472780323910071409 ) ) ;
#59257 = SPHERICAL_SURFACE ( 'NONE', #60362, 1.000000000000000000 ) ;
#59258 = UNCERTAINTY_MEASURE_WITH_UNIT (LENGTH_MEASURE( 1.000000000000000082E-05 ), #23074, 'distance_accuracy_value', 'NONE');
#59259 = CARTESIAN_POINT ( 'NONE',  ( -56.00499999999996703, 6.826472737025116366, 4.959722759717898555 ) ) ;
#59260 = CARTESIAN_POINT ( 'NONE',  ( 18.00000000000000711, 31.24999999999999289, 4.000000000000000000 ) ) ;
#59261 = CARTESIAN_POINT ( 'NONE',  ( -54.29499999999998749, -2.607480562269069768, 8.024999999999991473 ) ) ;
#59262 =( NAMED_UNIT ( * ) PLANE_ANGLE_UNIT ( ) SI_UNIT ( $, .RADIAN. ) );
#59263 = PRESENTATION_STYLE_ASSIGNMENT (( #64212 ) ) ;
#59264 =( LENGTH_UNIT ( ) NAMED_UNIT ( * ) SI_UNIT ( .MILLI., .METRE. ) );
#59265 = CARTESIAN_POINT ( 'NONE',  ( 22.50000000000000711, 34.24999999999999289, -3.750000000000000000 ) ) ;
#59266 = CARTESIAN_POINT ( 'NONE',  ( -105.2929263765337993, 3.094860106618428031, -9.524999999999993250 ) ) ;
#59267 = DIRECTION ( 'NONE',  ( -1.000000000000000000, -1.132643588934172738E-16, -1.473213661637684397E-17 ) ) ;
#59268 = FACE_OUTER_BOUND ( 'NONE', #39842, .T. ) ;
#59269 = EDGE_CURVE ( 'NONE', #34517, #25180, #14568, .T. ) ;
#59270 = LINE ( 'NONE', #37195, #14619 ) ;
#59271 = CIRCLE ( 'NONE', #60439, 0.2500000000000002220 ) ;
#59272 = ORIENTED_EDGE ( 'NONE', *, *, #31120, .T. ) ;
#59273 = CARTESIAN_POINT ( 'NONE',  ( -48.50000000000000000, 50.00000000000000000, 7.000000000000000000 ) ) ;
#59274 = SURFACE_STYLE_FILL_AREA ( #42480 ) ;
#59275 = ORIENTED_EDGE ( 'NONE', *, *, #15438, .T. ) ;
#59276 = CARTESIAN_POINT ( 'NONE',  ( 21.25000000000000711, 22.24999999999998224, 3.750000000000000000 ) ) ;
#59277 = VECTOR ( 'NONE', #40723, 1000.000000000000000 ) ;
#59278 = CARTESIAN_POINT ( 'NONE',  ( 7.632228543268608334, 111.4570736234661581, -2.479861379858951942 ) ) ;
#59279 = EDGE_CURVE ( 'NONE', #63065, #6283, #59909, .T. ) ;
#59280 = CARTESIAN_POINT ( 'NONE',  ( -19.89974874213240597, 114.9999999999999574, 10.00000000000001421 ) ) ;
#59281 = CARTESIAN_POINT ( 'NONE',  ( 8.437984349512095861, 138.3070736234661808, 1.550032578732816828E-15 ) ) ;
#59282 = VECTOR ( 'NONE', #1432, 1000.000000000000000 ) ;
#59283 = CARTESIAN_POINT ( 'NONE',  ( 57.24999999999999289, 27.74999999999998934, -3.750000000000000000 ) ) ;
#59284 = EDGE_LOOP ( 'NONE', ( #5251, #30919, #19957 ) ) ;
#59285 = ORIENTED_EDGE ( 'NONE', *, *, #66301, .F. ) ;
#59286 = CARTESIAN_POINT ( 'NONE',  ( -116.9070736234669994, -3.094860106604782946, 9.525000000009905321 ) ) ;
#59287 = AXIS2_PLACEMENT_3D ( 'NONE', #6499, #1175, #22710 ) ;
#59288 = DIRECTION ( 'NONE',  ( 0.000000000000000000, -1.000000000000000000, 0.000000000000000000 ) ) ;
#59289 = EDGE_CURVE ( 'NONE', #6428, #47061, #65142, .T. ) ;
#59290 = DIRECTION ( 'NONE',  ( 1.000000000000000000, 0.000000000000000000, 0.000000000000000000 ) ) ;
#59291 = VERTEX_POINT ( 'NONE', #22854 ) ;
#59292 = ADVANCED_FACE ( 'NONE', ( #13304 ), #34762, .F. ) ;
#59293 = CARTESIAN_POINT ( 'NONE',  ( 5.598654528085809545, 125.2549999999999812, -7.705886871421373741 ) ) ;
#59294 = CARTESIAN_POINT ( 'NONE',  ( 25.75000000000001066, 21.99999999999998224, -3.750000000000000000 ) ) ;
#59295 = CARTESIAN_POINT ( 'NONE',  ( -93.20707362346729496, 3.094860106636853292, 9.524999999986610177 ) ) ;
#59296 = CARTESIAN_POINT ( 'NONE',  ( 0.000000000000000000, 149.9429263765338476, -8.025000000000000355 ) ) ;
#59297 = CARTESIAN_POINT ( 'NONE',  ( -95.69499999999997897, -8.437984349512085203, 5.166775262442717831E-16 ) ) ;
#59298 = ORIENTED_EDGE ( 'NONE', *, *, #58298, .T. ) ;
#59299 = SURFACE_STYLE_USAGE ( .BOTH. , #37925 ) ;
#59300 = ADVANCED_FACE ( 'NONE', ( #3407 ), #29839, .T. ) ;
#59301 = SURFACE_STYLE_FILL_AREA ( #31896 ) ;
#59302 = ORIENTED_EDGE ( 'NONE', *, *, #30726, .F. ) ;
#59303 = CARTESIAN_POINT ( 'NONE',  ( -175.7929263765338987, -3.094860106616613926, 9.525000000001307754 ) ) ;
#59304 = FILL_AREA_STYLE ('',( #37930 ) ) ;
#59305 = ADVANCED_FACE ( 'NONE', ( #3768 ), #43905, .F. ) ;
#59306 = DIRECTION ( 'NONE',  ( 0.000000000000000000, 0.000000000000000000, -1.000000000000000000 ) ) ;
#59307 =( NAMED_UNIT ( * ) SI_UNIT ( $, .STERADIAN. ) SOLID_ANGLE_UNIT ( ) );
#59308 = VERTEX_POINT ( 'NONE', #20324 ) ;
#59309 = DIRECTION ( 'NONE',  ( 0.000000000000000000, 0.000000000000000000, 1.000000000000000000 ) ) ;
#59310 = ORIENTED_EDGE ( 'NONE', *, *, #1622, .F. ) ;
#59311 = DIRECTION ( 'NONE',  ( -1.000000000000000000, -0.000000000000000000, -0.000000000000000000 ) ) ;
#59312 = DIRECTION ( 'NONE',  ( 1.000000000000000000, 0.000000000000000000, 0.000000000000000000 ) ) ;
#59313 = FILL_AREA_STYLE_COLOUR ( '', #18729 ) ;
#59314 = MECHANICAL_DESIGN_GEOMETRIC_PRESENTATION_REPRESENTATION (  '', ( #41401 ), #25631 ) ;
#59315 = DIRECTION ( 'NONE',  ( 0.000000000000000000, 0.000000000000000000, -1.000000000000000000 ) ) ;
#59316 = CIRCLE ( 'NONE', #2024, 7.000000000000001776 ) ;
#59317 =( BOUNDED_CURVE ( )  B_SPLINE_CURVE ( 2, ( #33044, #43632, #39042, #33383, #22136, #54809, #37676, #60441, #59395, #1304, #28414 ),
 .UNSPECIFIED., .F., .F. ) 
 B_SPLINE_CURVE_WITH_KNOTS ( ( 3, 2, 2, 2, 2, 3 ),
 ( 0.5760869565217253685, 0.5782608695652036168, 0.5804347826086817541, 0.5826086956521600024, 0.5847826086956381397, 0.5869565217391164991 ),
 .UNSPECIFIED. ) 
 CURVE ( )  GEOMETRIC_REPRESENTATION_ITEM ( )  RATIONAL_B_SPLINE_CURVE ( ( 1.000000000000309974, 0.9510565162948435569, 1.000000000000000000, 0.9510565162951535312, 1.000000000000000000, 0.9510565162951535312, 1.000000000000000000, 0.9510565162951535312, 1.000000000000000000, 0.9510565162954685015, 0.9999999999996850297 ) ) 
 REPRESENTATION_ITEM ( '' )  );
#59318 = CARTESIAN_POINT ( 'NONE',  ( 7.632228543268608334, 116.3429263765338106, -2.479861379858951942 ) ) ;
#59319 = CARTESIAN_POINT ( 'NONE',  ( -6.598003871452776892, 153.8282337726623723, 5.909302594220192439 ) ) ;
#59320 = ORIENTED_EDGE ( 'NONE', *, *, #33168, .T. ) ;
#59321 = COLOUR_RGB ( '', 0.09019608, 0.27058824, 0.51372549) ;
#59322 = EDGE_LOOP ( 'NONE', ( #69022, #41713, #16132 ) ) ;
#59323 = DIRECTION ( 'NONE',  ( 0.000000000000000000, 0.000000000000000000, 1.000000000000000000 ) ) ;
#59324 = CARTESIAN_POINT ( 'NONE',  ( 48.75000000000004974, 1.127570259384924864E-13, 4.000000000000000000 ) ) ;
#59325 = CARTESIAN_POINT ( 'NONE',  ( -150.0570736234661808, 0.000000000000000000, 9.524999999999991473 ) ) ;
#59326 = CARTESIAN_POINT ( 'NONE',  ( 72.00000000000000000, 14.49137674618942562, -7.500000000000000000 ) ) ;
#59327 = ORIENTED_EDGE ( 'NONE', *, *, #33736, .T. ) ;
#59328 = SURFACE_STYLE_FILL_AREA ( #10827 ) ;
#59329 = CARTESIAN_POINT ( 'NONE',  ( -166.2549999999999955, -4.716976649647092401, 6.492361379858946790 ) ) ;
#59330 = DIRECTION ( 'NONE',  ( -1.000000000000000000, -0.000000000000000000, -0.000000000000000000 ) ) ;
#59331 = CARTESIAN_POINT ( 'NONE',  ( -148.5570736234661808, -1.166476076187852838E-15, -9.524999999999991473 ) ) ;
#59332 = CARTESIAN_POINT ( 'NONE',  ( -173.6949999999999648, -8.437984349512085203, 5.166775262442717831E-16 ) ) ;
#59333 = COLOUR_RGB ( '', 0.66274510, 0.83137255, 0.94901961) ;
#59334 = CARTESIAN_POINT ( 'NONE',  ( -167.5449999999999875, -7.632228543268600340, -2.479861379858950166 ) ) ;
#59335 = EDGE_CURVE ( 'NONE', #59464, #20746, #68575, .T. ) ;
#59336 = ORIENTED_EDGE ( 'NONE', *, *, #37482, .F. ) ;
#59337 = STYLED_ITEM ( 'NONE', ( #37234 ), #971 ) ;
#59338 = SURFACE_STYLE_FILL_AREA ( #48507 ) ;
#59339 = CARTESIAN_POINT ( 'NONE',  ( -2.243484957755116582, -2.233878551459170136, 9.000000000000005329 ) ) ;
#59340 = CARTESIAN_POINT ( 'NONE',  ( -80.90499999999995850, 2.607480562269068880, -8.024999999999993250 ) ) ;
#59341 = DIRECTION ( 'NONE',  ( -0.000000000000000000, 0.000000000000000000, 1.000000000000000000 ) ) ;
#59342 = CARTESIAN_POINT ( 'NONE',  ( -65.99999999999998579, 50.00000000000000000, 10.50000000000000000 ) ) ;
#59344 = FACE_OUTER_BOUND ( 'NONE', #10115, .T. ) ;
#59343 = PRESENTATION_LAYER_ASSIGNMENT (  '', '', ( #63871 ) ) ;
#59345 = CARTESIAN_POINT ( 'NONE',  ( -82.49499999999997613, 6.826472737025113702, -4.959722759717902107 ) ) ;
#59346 = CARTESIAN_POINT ( 'NONE',  ( -9.058813317711337021, 138.1550000000000011, -2.943386871421374895 ) ) ;
#59347 = CARTESIAN_POINT ( 'NONE',  ( -6.826472737025120807, 126.3929263765338220, -4.959722759717907437 ) ) ;
#59348 = CARTESIAN_POINT ( 'NONE',  ( 14.60000000000000142, 11.99999999999999289, -4.000000000000000000 ) ) ;
#59349 = UNCERTAINTY_MEASURE_WITH_UNIT (LENGTH_MEASURE( 1.000000000000000082E-05 ), #22062, 'distance_accuracy_value', 'NONE');
#59350 = CARTESIAN_POINT ( 'NONE',  ( -0.3558155365998603159, -2.493171897977953133, -7.000000000000004441 ) ) ;
#59351 = VERTEX_POINT ( 'NONE', #14019 ) ;
#59352 = CARTESIAN_POINT ( 'NONE',  ( 96.10348817448819148, 0.000000000000000000, 27.38099488609881149 ) ) ;
#59353 = VECTOR ( 'NONE', #53046, 1000.000000000000000 ) ;
#59354 = EDGE_CURVE ( 'NONE', #27464, #28130, #37233, .T. ) ;
#59355 = DIRECTION ( 'NONE',  ( -1.000000000000000000, 0.000000000000000000, 0.000000000000000000 ) ) ;
#59356 = CARTESIAN_POINT ( 'NONE',  ( 28.00000000000000000, 42.00000000000000000, 3.902931319921305165E-16 ) ) ;
#59357 = VERTEX_POINT ( 'NONE', #67475 ) ;
#59358 = ORIENTED_EDGE ( 'NONE', *, *, #36050, .T. ) ;
#59359 = PRESENTATION_STYLE_ASSIGNMENT (( #39351 ) ) ;
#59360 = FACE_OUTER_BOUND ( 'NONE', #32597, .T. ) ;
#59362 = AXIS2_PLACEMENT_3D ( 'NONE', #9714, #24457, #31125 ) ;
#59361 = UNCERTAINTY_MEASURE_WITH_UNIT (LENGTH_MEASURE( 1.000000000000000082E-05 ), #10081, 'distance_accuracy_value', 'NONE');
#59363 = EDGE_CURVE ( 'NONE', #66883, #41176, #7901, .T. ) ;
#59364 = SURFACE_STYLE_USAGE ( .BOTH. , #54103 ) ;
#59365 = CARTESIAN_POINT ( 'NONE',  ( -151.5570736234661808, -1.166476076187852838E-15, -9.524999999999991473 ) ) ;
#59366 = PRESENTATION_LAYER_ASSIGNMENT (  '', '', ( #66119 ) ) ;
#59367 = FACE_OUTER_BOUND ( 'NONE', #21864, .T. ) ;
#59368 = CARTESIAN_POINT ( 'NONE',  ( 32.00000000000001421, 42.00000000000000000, -36.50000000000000000 ) ) ;
#59369 = EDGE_LOOP ( 'NONE', ( #19133, #11494, #9013, #6641 ) ) ;
#59370 = CARTESIAN_POINT ( 'NONE',  ( -114.8049999999999926, -8.437984349512086979, 5.166775262442717831E-16 ) ) ;
#59371 = ORIENTED_EDGE ( 'NONE', *, *, #822, .T. ) ;
#59372 = FACE_OUTER_BOUND ( 'NONE', #19424, .T. ) ;
#59373 = DIRECTION ( 'NONE',  ( 1.000000000000000000, 0.000000000000000000, 0.000000000000000000 ) ) ;
#59374 = EDGE_CURVE ( 'NONE', #48200, #16450, #25872, .T. ) ;
#59375 = VERTEX_POINT ( 'NONE', #52015 ) ;
#59376 = FACE_OUTER_BOUND ( 'NONE', #11866, .T. ) ;
#59377 = DIRECTION ( 'NONE',  ( 0.000000000000000000, 0.000000000000000000, 1.000000000000000000 ) ) ;
#59378 = ORIENTED_EDGE ( 'NONE', *, *, #52304, .T. ) ;
#59379 = AXIS2_PLACEMENT_3D ( 'NONE', #59541, #21936, #53589 ) ;
#59380 = SURFACE_STYLE_FILL_AREA ( #27369 ) ;
#59381 = CARTESIAN_POINT ( 'NONE',  ( -8.102448949553181734, 154.8949999999999534, -5.886773742842749790 ) ) ;
#59382 =( LENGTH_UNIT ( ) NAMED_UNIT ( * ) SI_UNIT ( .MILLI., .METRE. ) );
#59383 = ORIENTED_EDGE ( 'NONE', *, *, #54468, .F. ) ;
#59384 = ORIENTED_EDGE ( 'NONE', *, *, #3307, .T. ) ;
#59385 = CARTESIAN_POINT ( 'NONE',  ( 92.41620014002536720, 5.000000000000000000, -29.00402776293825724 ) ) ;
#59386 =( LENGTH_UNIT ( ) NAMED_UNIT ( * ) SI_UNIT ( .MILLI., .METRE. ) );
#59387 = CARTESIAN_POINT ( 'NONE',  ( 31.00000000000001421, 42.00000000000000000, 36.49999999999999289 ) ) ;
#59388 = CARTESIAN_POINT ( 'NONE',  ( 74.99999999999998579, 50.00000000000000000, -7.500000000000000000 ) ) ;
#59389 = ORIENTED_EDGE ( 'NONE', *, *, #59538, .F. ) ;
#59390 = CARTESIAN_POINT ( 'NONE',  ( 2.607480562269076430, 134.7929263765338135, -8.025000000000000355 ) ) ;
#59391 = DIRECTION ( 'NONE',  ( 0.000000000000000000, 0.000000000000000000, 1.000000000000000000 ) ) ;
#59392 = CARTESIAN_POINT ( 'NONE',  ( -75.48275862068965125, 36.00832590023089352, -9.500000000000001776 ) ) ;
#59393 = AXIS2_PLACEMENT_3D ( 'NONE', #17172, #60047, #11861 ) ;
#59394 = EDGE_CURVE ( 'NONE', #57062, #10613, #10864, .T. ) ;
#59395 = CARTESIAN_POINT ( 'NONE',  ( -104.2429263765338021, 5.598654528085804216, 7.705886871421366635 ) ) ;
#59396 = CARTESIAN_POINT ( 'NONE',  ( 0.04677136509298115974, 68.99999999999998579, 2.000000000000000000 ) ) ;
#59397 = ORIENTED_EDGE ( 'NONE', *, *, #35845, .T. ) ;
#59398 = CARTESIAN_POINT ( 'NONE',  ( -74.50000000000001421, -2.220952357103124294E-14, 10.00000000000000000 ) ) ;
#59399 = ORIENTED_EDGE ( 'NONE', *, *, #55822, .T. ) ;
#59400 = CARTESIAN_POINT ( 'NONE',  ( -51.29292637653378506, 3.094860106618428031, -9.524999999999993250 ) ) ;
#59401 = CYLINDRICAL_SURFACE ( 'NONE', #60163, 9.524999999999991473 ) ;
#59402 = CARTESIAN_POINT ( 'NONE',  ( -141.5049999999999955, -6.826472737025115478, -4.959722759717899443 ) ) ;
#59403 =( NAMED_UNIT ( * ) PLANE_ANGLE_UNIT ( ) SI_UNIT ( $, .RADIAN. ) );
#59404 =( NAMED_UNIT ( * ) PLANE_ANGLE_UNIT ( ) SI_UNIT ( $, .RADIAN. ) );
#59405 = UNCERTAINTY_MEASURE_WITH_UNIT (LENGTH_MEASURE( 1.000000000000000082E-05 ), #15878, 'distance_accuracy_value', 'NONE');
#59406 = CIRCLE ( 'NONE', #29067, 5.000000000000004441 ) ;
#59407 = CARTESIAN_POINT ( 'NONE',  ( -46.46084196965908575, -13.75011736874646395, 0.8310740330500354656 ) ) ;
#59408 = CARTESIAN_POINT ( 'NONE',  ( -5.196152422706634688, 9.000000000000008882, 1.392304845413263159 ) ) ;
#59409 = CARTESIAN_POINT ( 'NONE',  ( 41.03182778381237483, 107.9802461459568832, 3.207526698639996177 ) ) ;
#59410 = VERTEX_POINT ( 'NONE', #10817 ) ;
#59411 = ORIENTED_EDGE ( 'NONE', *, *, #44370, .T. ) ;
#59412 = LINE ( 'NONE', #27406, #29416 ) ;
#59413 = CIRCLE ( 'NONE', #30187, 0.5000000000000004441 ) ;
#59414 = FACE_OUTER_BOUND ( 'NONE', #12049, .T. ) ;
#59415 = CARTESIAN_POINT ( 'NONE',  ( -59.45499999999997698, 7.632228543268599452, -2.479861379858951942 ) ) ;
#59416 = ORIENTED_EDGE ( 'NONE', *, *, #66978, .T. ) ;
#59417 =( NAMED_UNIT ( * ) PLANE_ANGLE_UNIT ( ) SI_UNIT ( $, .RADIAN. ) );
#59418 = DIRECTION ( 'NONE',  ( 0.000000000000000000, 0.000000000000000000, 1.000000000000000000 ) ) ;
#59419 = CARTESIAN_POINT ( 'NONE',  ( 9.000000000000003553, 27.99999999999998934, 4.000000000000000000 ) ) ;
#59420 = PRESENTATION_LAYER_ASSIGNMENT (  '', '', ( #57218 ) ) ;
#59421 = DIRECTION ( 'NONE',  ( 0.000000000000000000, 0.000000000000000000, 1.000000000000000000 ) ) ;
#59422 = EDGE_CURVE ( 'NONE', #8099, #40740, #48841, .T. ) ;
#59423 = DIRECTION ( 'NONE',  ( -1.000000000000000000, -2.168404344971008868E-16, 0.000000000000000000 ) ) ;
#59424 = ORIENTED_EDGE ( 'NONE', *, *, #2164, .F. ) ;
#59425 = DIRECTION ( 'NONE',  ( -1.000000000000000000, 0.000000000000000000, 0.000000000000000000 ) ) ;
#59426 = FILL_AREA_STYLE ('',( #39075 ) ) ;
#59427 = PLANE ( 'NONE',  #61207 ) ;
#59428 = SURFACE_SIDE_STYLE ('',( #38037 ) ) ;
#59429 = VECTOR ( 'NONE', #69675, 1000.000000000000000 ) ;
#59430 = SURFACE_STYLE_USAGE ( .BOTH. , #42305 ) ;
#59431 = CARTESIAN_POINT ( 'NONE',  ( -112.1949999999999932, 8.437984349512086979, -1.550032578732815448E-15 ) ) ;
#59432 = CARTESIAN_POINT ( 'NONE',  ( 0.000000000000000000, 154.4449999999999932, -9.525000000000000355 ) ) ;
#59433 = CARTESIAN_POINT ( 'NONE',  ( -83.84499999999998465, -7.632228543268599452, 2.479861379858951054 ) ) ;
#59434 = CARTESIAN_POINT ( 'NONE',  ( 0.000000000000000000, 2.000000000000000444, 3.000000000000000444 ) ) ;
#59435 = B_SPLINE_CURVE_WITH_KNOTS ( 'NONE', 3,
 ( #37884, #35495, #52030, #62210, #14036, #10754, #25275, #68199, #56941, #53648 ),
 .UNSPECIFIED., .F., .F.,
 ( 4, 2, 2, 2, 4 ),
 ( 0.000000000000000000, 0.0004658606356703475925, 0.0009317212713406951849, 0.001397581907011042832, 0.001863442542681390370 ),
 .UNSPECIFIED. ) ;
#59436 = VECTOR ( 'NONE', #64119, 1000.000000000000000 ) ;
#59437 = PRESENTATION_STYLE_ASSIGNMENT (( #4958 ) ) ;
#59438 = CARTESIAN_POINT ( 'NONE',  ( -48.50000000000000000, 14.49137674618942562, 7.500000000000000000 ) ) ;
#59439 = UNCERTAINTY_MEASURE_WITH_UNIT (LENGTH_MEASURE( 1.000000000000000082E-05 ), #38360, 'distance_accuracy_value', 'NONE');
#59440 =( GEOMETRIC_REPRESENTATION_CONTEXT ( 3 ) GLOBAL_UNCERTAINTY_ASSIGNED_CONTEXT ( ( #29356 ) ) GLOBAL_UNIT_ASSIGNED_CONTEXT ( ( #60467, #63766, #21195 ) ) REPRESENTATION_CONTEXT ( 'NONE', 'WORKASPACE' ) );
#59441 = LINE ( 'NONE', #64042, #49379 ) ;
#59442 = ORIENTED_EDGE ( 'NONE', *, *, #30649, .F. ) ;
#59443 = CARTESIAN_POINT ( 'NONE',  ( -122.3929263765337936, 8.102448949553176405, 5.886773742842740909 ) ) ;
#59444 = CARTESIAN_POINT ( 'NONE',  ( -144.7449999999999761, 4.716976649647094177, 6.492361379858945902 ) ) ;
#59445 = DIRECTION ( 'NONE',  ( 0.000000000000000000, 0.000000000000000000, 1.000000000000000000 ) ) ;
#59446 = CIRCLE ( 'NONE', #51695, 4.000000000000000000 ) ;
#59447 = EDGE_CURVE ( 'NONE', #50360, #35826, #53395, .T. ) ;
#59448 = CARTESIAN_POINT ( 'NONE',  ( 15.98999599679679839, 146.9999999999999716, -7.500000000000000000 ) ) ;
#59449 = CARTESIAN_POINT ( 'NONE',  ( 4.000000000000030198, 42.00000000000000000, 0.000000000000000000 ) ) ;
#59450 = EDGE_LOOP ( 'NONE', ( #3372, #18684, #9098, #50134 ) ) ;
#59451 = VERTEX_POINT ( 'NONE', #31564 ) ;
#59452 = STYLED_ITEM ( 'NONE', ( #8649 ), #1177 ) ;
#59453 = AXIS2_PLACEMENT_3D ( 'NONE', #32177, #21617, #43133 ) ;
#59454 = DIRECTION ( 'NONE',  ( -1.000000000000000000, -0.000000000000000000, -0.000000000000000000 ) ) ;
#59455 = DIRECTION ( 'NONE',  ( -0.000000000000000000, -1.000000000000000000, -0.000000000000000000 ) ) ;
#59456 = CARTESIAN_POINT ( 'NONE',  ( -35.25000000000000000, 4.336808689942018722E-16, -5.099999999999999645 ) ) ;
#59457 = FACE_OUTER_BOUND ( 'NONE', #40016, .T. ) ;
#59458 = CARTESIAN_POINT ( 'NONE',  ( 0.000000000000000000, 0.9999999999999991118, -79.00402776293826435 ) ) ;
#59459 = CARTESIAN_POINT ( 'NONE',  ( -116.5429263765338135, 9.058813317711329915, 2.943386871421369566 ) ) ;
#59460 =( GEOMETRIC_REPRESENTATION_CONTEXT ( 3 ) GLOBAL_UNCERTAINTY_ASSIGNED_CONTEXT ( ( #31990 ) ) GLOBAL_UNIT_ASSIGNED_CONTEXT ( ( #38482, #16316, #5700 ) ) REPRESENTATION_CONTEXT ( 'NONE', 'WORKASPACE' ) );
#59461 = DIRECTION ( 'NONE',  ( 0.000000000000000000, 0.000000000000000000, -1.000000000000000000 ) ) ;
#59462 = ORIENTED_EDGE ( 'NONE', *, *, #15758, .F. ) ;
#59463 = CARTESIAN_POINT ( 'NONE',  ( -142.4050000000000011, -2.607480562269069768, 8.024999999999991473 ) ) ;
#59464 = VERTEX_POINT ( 'NONE', #53711 ) ;
#59465 = EDGE_CURVE ( 'NONE', #40918, #50571, #49114, .T. ) ;
#59466 = EDGE_LOOP ( 'NONE', ( #66581, #17995, #17844, #65457 ) ) ;
#59467 = DIRECTION ( 'NONE',  ( 0.000000000000000000, 0.000000000000000000, 1.000000000000000000 ) ) ;
#59468 = ORIENTED_EDGE ( 'NONE', *, *, #61221, .T. ) ;
#59469 = COLOUR_RGB ( '', 0.09019608, 0.27058824, 0.51372549) ;
#59470 = AXIS2_PLACEMENT_3D ( 'NONE', #770, #11751, #65214 ) ;
#59471 = EDGE_CURVE ( 'NONE', #51828, #4422, #59003, .T. ) ;
#59472 = DIRECTION ( 'NONE',  ( 0.000000000000000000, -1.000000000000000000, 0.000000000000000000 ) ) ;
#59473 = VECTOR ( 'NONE', #51880, 1000.000000000000000 ) ;
#59474 = CARTESIAN_POINT ( 'NONE',  ( 9.058813317711337021, 132.5449999999999875, 2.943386871421375783 ) ) ;
#59475 = CARTESIAN_POINT ( 'NONE',  ( 15.98999599679679839, 118.4999999999999716, 7.000000000000000000 ) ) ;
#59476 = CIRCLE ( 'NONE', #60571, 5.999999999999998224 ) ;
#59477 = COLOUR_RGB ( '', 0.08235294, 0.09019608, 0.10196078) ;
#59478 = EDGE_LOOP ( 'NONE', ( #8939, #8002, #36529, #61217 ) ) ;
#59479 = DIRECTION ( 'NONE',  ( 0.000000000000000000, -1.000000000000000000, 0.000000000000000000 ) ) ;
#59481 = EDGE_CURVE ( 'NONE', #39204, #28720, #31492, .T. ) ;
#59480 = CARTESIAN_POINT ( 'NONE',  ( 8.102448949553181734, 128.1049999999999898, -5.886773742842746238 ) ) ;
#59482 = CARTESIAN_POINT ( 'NONE',  ( -61.25499999999998835, -4.716976649647092401, 6.492361379858946790 ) ) ;
#59483 = CARTESIAN_POINT ( 'NONE',  ( -121.6449999999999960, 4.716976649647091513, -6.492361379858946790 ) ) ;
#59484 = AXIS2_PLACEMENT_3D ( 'NONE', #39218, #60617, #28611 ) ;
#59485 = CARTESIAN_POINT ( 'NONE',  ( -41.61212508608682725, 107.5086115709060834, -4.000000005149773052 ) ) ;
#59486 = ORIENTED_EDGE ( 'NONE', *, *, #27051, .F. ) ;
#59487 = CARTESIAN_POINT ( 'NONE',  ( -8.102448949553181734, 147.6049999999999329, 5.886773742842747126 ) ) ;
#59488 = PRESENTATION_STYLE_ASSIGNMENT (( #61714 ) ) ;
#59489 = UNCERTAINTY_MEASURE_WITH_UNIT (LENGTH_MEASURE( 1.000000000000000082E-05 ), #5556, 'distance_accuracy_value', 'NONE');
#59490 = VECTOR ( 'NONE', #59040, 1000.000000000000114 ) ;
#59491 =( NAMED_UNIT ( * ) SI_UNIT ( $, .STERADIAN. ) SOLID_ANGLE_UNIT ( ) );
#59492 = ADVANCED_FACE ( 'NONE', ( #26951 ), #61798, .T. ) ;
#59493 = PRESENTATION_STYLE_ASSIGNMENT (( #38093 ) ) ;
#59494 = ORIENTED_EDGE ( 'NONE', *, *, #12332, .T. ) ;
#59495 = AXIS2_PLACEMENT_3D ( 'NONE', #65860, #60234, #66551 ) ;
#59496 = CARTESIAN_POINT ( 'NONE',  ( 40.78947368421051323, 108.1536491499103363, 3.000000000000000000 ) ) ;
#59497 = CARTESIAN_POINT ( 'NONE',  ( -175.2549999999999955, -4.716976649647092401, 6.492361379858946790 ) ) ;
#59498 = ORIENTED_EDGE ( 'NONE', *, *, #50438, .F. ) ;
#59499 = PRESENTATION_STYLE_ASSIGNMENT (( #38103 ) ) ;
#59500 = UNCERTAINTY_MEASURE_WITH_UNIT (LENGTH_MEASURE( 1.000000000000000082E-05 ), #18231, 'distance_accuracy_value', 'NONE');
#59501 = VECTOR ( 'NONE', #21205, 1000.000000000000000 ) ;
#59502 = FACE_OUTER_BOUND ( 'NONE', #58737, .T. ) ;
#59503 = CYLINDRICAL_SURFACE ( 'NONE', #20665, 9.524999999999991473 ) ;
#59504 =( NAMED_UNIT ( * ) SI_UNIT ( $, .STERADIAN. ) SOLID_ANGLE_UNIT ( ) );
#59505 = DIRECTION ( 'NONE',  ( 0.000000000000000000, 1.000000000000000000, 0.000000000000000000 ) ) ;
#59506 = ORIENTED_EDGE ( 'NONE', *, *, #59797, .T. ) ;
#59507 = CARTESIAN_POINT ( 'NONE',  ( -45.89905495991339990, 9.405628579550478818, -3.102097799525639132 ) ) ;
#59508 = CARTESIAN_POINT ( 'NONE',  ( -89.15499999999998693, 7.632228543268600340, 2.479861379858949277 ) ) ;
#59509 = VERTEX_POINT ( 'NONE', #538 ) ;
#59510 = DIRECTION ( 'NONE',  ( 0.000000000000000000, -0.000000000000000000, 1.000000000000000000 ) ) ;
#59511 = CARTESIAN_POINT ( 'NONE',  ( -7.731910350068054619E-16, -6.500000000000000888, 21.00000000000000000 ) ) ;
#59512 = TOROIDAL_SURFACE ( 'NONE', #13465, 8.499999999999994671, 0.5000000000000000000 ) ;
#59513 = AXIS2_PLACEMENT_3D ( 'NONE', #20779, #47563, #41221 ) ;
#59514 = CARTESIAN_POINT ( 'NONE',  ( 2.607480562269160362, 144.9070736234662036, -8.024999999999939959 ) ) ;
#59515 = CARTESIAN_POINT ( 'NONE',  ( -15.75000000000000000, 4.336808689942018722E-16, 24.00000000000000000 ) ) ;
#59516 = CARTESIAN_POINT ( 'NONE',  ( -65.00707362346616947, -8.102448949553172852, -5.886773742842741797 ) ) ;
#59517 = AXIS2_PLACEMENT_3D ( 'NONE', #38406, #69666, #16243 ) ;
#59518 = PRESENTATION_STYLE_ASSIGNMENT (( #10325 ) ) ;
#59519 = ORIENTED_EDGE ( 'NONE', *, *, #15685, .T. ) ;
#59520 = DIRECTION ( 'NONE',  ( -0.000000000000000000, -0.000000000000000000, -1.000000000000000000 ) ) ;
#59522 = DIRECTION ( 'NONE',  ( -1.000000000000000000, 0.000000000000000000, 0.000000000000000000 ) ) ;
#59521 = DIRECTION ( 'NONE',  ( -0.000000000000000000, -0.000000000000000000, -1.000000000000000000 ) ) ;
#59523 = CARTESIAN_POINT ( 'NONE',  ( -102.9549999999999841, -7.632228543268599452, 2.479861379858951054 ) ) ;
#59524 = CARTESIAN_POINT ( 'NONE',  ( -5.598654528085806881, 130.7450000000000045, -7.705886871421374629 ) ) ;
#59525 = CARTESIAN_POINT ( 'NONE',  ( -121.1949999999999790, 8.437984349512085203, -1.550032578732815448E-15 ) ) ;
#59526 = VECTOR ( 'NONE', #64311, 1000.000000000000000 ) ;
#59527 = VECTOR ( 'NONE', #33068, 1000.000000000000000 ) ;
#59528 = FILL_AREA_STYLE ('',( #396 ) ) ;
#59529 = AXIS2_PLACEMENT_3D ( 'NONE', #55672, #65535, #45158 ) ;
#59531 = SURFACE_STYLE_FILL_AREA ( #37463 ) ;
#59530 = CARTESIAN_POINT ( 'NONE',  ( 6.000000000000017764, 13.99999999999997691, 35.50000000000000000 ) ) ;
#59532 = CIRCLE ( 'NONE', #20221, 3.599999999999992095 ) ;
#59533 = CARTESIAN_POINT ( 'NONE',  ( -156.2929263765338135, 3.094860106618428031, -9.524999999999993250 ) ) ;
#59534 = CARTESIAN_POINT ( 'NONE',  ( -178.7949999999999875, 2.607480562269068880, -8.024999999999993250 ) ) ;
#59535 = CIRCLE ( 'NONE', #11244, 0.5000000000000004441 ) ;
#59536 =( LENGTH_UNIT ( ) NAMED_UNIT ( * ) SI_UNIT ( .MILLI., .METRE. ) );
#59537 = VECTOR ( 'NONE', #64676, 1000.000000000000000 ) ;
#59538 = EDGE_CURVE ( 'NONE', #17716, #20740, #6787, .T. ) ;
#59539 = LINE ( 'NONE', #22266, #56248 ) ;
#59540 = ORIENTED_EDGE ( 'NONE', *, *, #51619, .F. ) ;
#59541 = CARTESIAN_POINT ( 'NONE',  ( 15.98999599679679839, 146.4999999999999716, -9.500000000000000000 ) ) ;
#59542 = DIRECTION ( 'NONE',  ( 0.000000000000000000, 0.000000000000000000, -1.000000000000000000 ) ) ;
#59543 = ORIENTED_EDGE ( 'NONE', *, *, #37804, .F. ) ;
#59544 = CARTESIAN_POINT ( 'NONE',  ( -79.49292637653380211, -8.102448949553172852, 5.886773742842742685 ) ) ;
#59545 = VECTOR ( 'NONE', #1353, 1000.000000000000000 ) ;
#59547 = EDGE_CURVE ( 'NONE', #16561, #40163, #64632, .T. ) ;
#59546 = CARTESIAN_POINT ( 'NONE',  ( -48.00000000000000000, 99.99999999999992895, -7.500000000000000000 ) ) ;
#59548 = CARTESIAN_POINT ( 'NONE',  ( 10.99999999999999645, 11.99999999999999289, -4.000000000000000000 ) ) ;
#59549 = EDGE_CURVE ( 'NONE', #68323, #3926, #53045, .T. ) ;
#59550 = CARTESIAN_POINT ( 'NONE',  ( 62.59999999999998721, 11.99999999999999822, -4.000000000000000000 ) ) ;
#59551 = EDGE_CURVE ( 'NONE', #25953, #66309, #58310, .T. ) ;
#59552 = ORIENTED_EDGE ( 'NONE', *, *, #63387, .T. ) ;
#59553 = CARTESIAN_POINT ( 'NONE',  ( -167.1550000000000011, 7.632228543268600340, 2.479861379858949277 ) ) ;
#59554 = EDGE_CURVE ( 'NONE', #51351, #60581, #16480, .T. ) ;
#59555 = ORIENTED_EDGE ( 'NONE', *, *, #13164, .T. ) ;
#59556 = CARTESIAN_POINT ( 'NONE',  ( 35.99999999999999289, 5.000000000000000000, 37.00402776293825724 ) ) ;
#59557 = DIRECTION ( 'NONE',  ( -1.189524669241239115E-16, -1.000000000000000000, -0.000000000000000000 ) ) ;
#59558 = EDGE_CURVE ( 'NONE', #12616, #38944, #27308, .T. ) ;
#59559 = SURFACE_SIDE_STYLE ('',( #38155 ) ) ;
#59560 = AXIS2_PLACEMENT_3D ( 'NONE', #62230, #14054, #52050 ) ;
#59561 = DIRECTION ( 'NONE',  ( -0.000000000000000000, -0.000000000000000000, 1.000000000000000000 ) ) ;
#59562 = CARTESIAN_POINT ( 'NONE',  ( -9.827790563157511022E-16, 152.5570736234661524, 8.025000000000000355 ) ) ;
#59563 = EDGE_LOOP ( 'NONE', ( #26694, #8008, #44418, #33090 ) ) ;
#59564 = AXIS2_PLACEMENT_3D ( 'NONE', #3556, #62346, #29647 ) ;
#59566 = EDGE_CURVE ( 'NONE', #26634, #49493, #35991, .T. ) ;
#59565 = CARTESIAN_POINT ( 'NONE',  ( 6.826472737025119919, 136.8929263765338362, 4.959722759717908325 ) ) ;
#59567 = CARTESIAN_POINT ( 'NONE',  ( -88.70499999999998408, 2.607480562269072433, 8.024999999999991473 ) ) ;
#59568 = UNCERTAINTY_MEASURE_WITH_UNIT (LENGTH_MEASURE( 1.000000000000000082E-05 ), #52366, 'distance_accuracy_value', 'NONE');
#59569 = CARTESIAN_POINT ( 'NONE',  ( 22.00000000000002132, 42.00000000000000000, 29.68999999999999417 ) ) ;
#59570 = ORIENTED_EDGE ( 'NONE', *, *, #37388, .F. ) ;
#59571 = CARTESIAN_POINT ( 'NONE',  ( -92.90707362346728360, -3.094860106600009875, 9.525000000013374546 ) ) ;
#59572 =( LENGTH_UNIT ( ) NAMED_UNIT ( * ) SI_UNIT ( .MILLI., .METRE. ) );
#59573 =( NAMED_UNIT ( * ) SI_UNIT ( $, .STERADIAN. ) SOLID_ANGLE_UNIT ( ) );
#59574 = AXIS2_PLACEMENT_3D ( 'NONE', #2930, #41001, #4332 ) ;
#59576 = PRESENTATION_LAYER_ASSIGNMENT (  '', '', ( #25885 ) ) ;
#59575 = CARTESIAN_POINT ( 'NONE',  ( 4.793834890952475725, -1.308853920463818987, 9.000000000000005329 ) ) ;
#59577 = ORIENTED_EDGE ( 'NONE', *, *, #61369, .F. ) ;
#59578 = CARTESIAN_POINT ( 'NONE',  ( -63.89499999999998181, 6.826472737025116366, 4.959722759717898555 ) ) ;
#59580 = ORIENTED_EDGE ( 'NONE', *, *, #23485, .F. ) ;
#59579 = PRESENTATION_LAYER_ASSIGNMENT (  '', '', ( #1119 ) ) ;
#59581 = CARTESIAN_POINT ( 'NONE',  ( -7.249999999999999112, 0.000000000000000000, 1.000000000000000000 ) ) ;
#59582 = CARTESIAN_POINT ( 'NONE',  ( 9.827790563157511022E-16, 152.9999999999999716, -8.025000000000000355 ) ) ;
#59583 = CARTESIAN_POINT ( 'NONE',  ( -45.00000000000000000, 8.062885929673873520, -5.900610682604093604 ) ) ;
#59584 = ORIENTED_EDGE ( 'NONE', *, *, #62251, .T. ) ;
#59585 = FILL_AREA_STYLE ('',( #32497 ) ) ;
#59586 =( NAMED_UNIT ( * ) PLANE_ANGLE_UNIT ( ) SI_UNIT ( $, .RADIAN. ) );
#59587 = EDGE_LOOP ( 'NONE', ( #27714, #8101, #49308, #38869 ) ) ;
#59588 = CARTESIAN_POINT ( 'NONE',  ( 3.000000000000002665, 38.70020753820971748, -90.00000000000000000 ) ) ;
#59589 = CARTESIAN_POINT ( 'NONE',  ( -112.5549999999999926, 0.000000000000000000, 8.024999999999991473 ) ) ;
#59590 = ORIENTED_EDGE ( 'NONE', *, *, #30238, .F. ) ;
#59591 = DIRECTION ( 'NONE',  ( 1.300977106640435137E-16, 0.000000000000000000, 1.000000000000000000 ) ) ;
#59592 = DIRECTION ( 'NONE',  ( 0.000000000000000000, 0.000000000000000000, 1.000000000000000000 ) ) ;
#59593 = DIRECTION ( 'NONE',  ( -7.080503983578803083E-17, 1.000000000000000000, 0.000000000000000000 ) ) ;
#59594 = LINE ( 'NONE', #48403, #18472 ) ;
#59595 = CYLINDRICAL_SURFACE ( 'NONE', #7536, 7.499999999999985789 ) ;
#59596 = CARTESIAN_POINT ( 'NONE',  ( -153.5070736234661979, 8.102448949553176405, 5.886773742842740909 ) ) ;
#59597 = AXIS2_PLACEMENT_3D ( 'NONE', #54089, #69584, #5898 ) ;
#59598 = CARTESIAN_POINT ( 'NONE',  ( 8.102448949553181734, 132.9949999999999477, -5.886773742842746238 ) ) ;
#59599 = CARTESIAN_POINT ( 'NONE',  ( -91.85707362346617799, -5.598654528085803328, -7.705886871421366635 ) ) ;
#59600 = ADVANCED_FACE ( 'NONE', ( #4151 ), #57658, .F. ) ;
#59601 =( GEOMETRIC_REPRESENTATION_CONTEXT ( 3 ) GLOBAL_UNCERTAINTY_ASSIGNED_CONTEXT ( ( #65611 ) ) GLOBAL_UNIT_ASSIGNED_CONTEXT ( ( #57208, #41774, #45065 ) ) REPRESENTATION_CONTEXT ( 'NONE', 'WORKASPACE' ) );
#59602 = DIRECTION ( 'NONE',  ( 0.000000000000000000, 1.000000000000000000, 0.000000000000000000 ) ) ;
#59603 = ORIENTED_EDGE ( 'NONE', *, *, #15448, .F. ) ;
#59604 = PRESENTATION_LAYER_ASSIGNMENT (  '', '', ( #5671 ) ) ;
#59605 = CARTESIAN_POINT ( 'NONE',  ( 60.00000000000000000, 1.797044900979284448E-15, 6.999999999999988454 ) ) ;
#59607 =( LENGTH_UNIT ( ) NAMED_UNIT ( * ) SI_UNIT ( .MILLI., .METRE. ) );
#59606 = FACE_BOUND ( 'NONE', #52275, .T. ) ;
#59608 = CARTESIAN_POINT ( 'NONE',  ( -2.607480562269032909, 131.4070736234661467, 8.025000000000032330 ) ) ;
#59609 = CARTESIAN_POINT ( 'NONE',  ( -129.9549999999999841, -7.632228543268599452, 2.479861379858951054 ) ) ;
#59610 = CARTESIAN_POINT ( 'NONE',  ( -86.60707362346619220, -8.102448949553174629, 5.886773742842742685 ) ) ;
#59611 = CARTESIAN_POINT ( 'NONE',  ( -142.6449999999999818, 4.716976649647091513, -6.492361379858946790 ) ) ;
#59612 = CARTESIAN_POINT ( 'NONE',  ( -134.6950000000000500, -8.437984349512086979, 5.166775262442717831E-16 ) ) ;
#59613 = VECTOR ( 'NONE', #33342, 1000.000000000000000 ) ;
#59614 = ORIENTED_EDGE ( 'NONE', *, *, #56396, .F. ) ;
#59615 =( NAMED_UNIT ( * ) PLANE_ANGLE_UNIT ( ) SI_UNIT ( $, .RADIAN. ) );
#59616 =( NAMED_UNIT ( * ) SI_UNIT ( $, .STERADIAN. ) SOLID_ANGLE_UNIT ( ) );
#59617 =( GEOMETRIC_REPRESENTATION_CONTEXT ( 3 ) GLOBAL_UNCERTAINTY_ASSIGNED_CONTEXT ( ( #47395 ) ) GLOBAL_UNIT_ASSIGNED_CONTEXT ( ( #51445, #46916, #19778 ) ) REPRESENTATION_CONTEXT ( 'NONE', 'WORKASPACE' ) );
#59618 = SURFACE_SIDE_STYLE ('',( #49117 ) ) ;
#59619 = CARTESIAN_POINT ( 'NONE',  ( -56.90499999999998693, 2.607480562269068880, -8.024999999999993250 ) ) ;
#59620 =( BOUNDED_CURVE ( )  B_SPLINE_CURVE ( 2, ( #60645, #12461, #35333, #28275, #7889, #23048, #18464, #28978, #50468, #23375, #39947 ),
 .UNSPECIFIED., .F., .F. ) 
 B_SPLINE_CURVE_WITH_KNOTS ( ( 3, 2, 2, 2, 2, 3 ),
 ( 0.2608695652173851909, 0.2630434782608633837, 0.2652173913043416320, 0.2673913043478198803, 0.2695652173912980731, 0.2717391304347762659 ),
 .UNSPECIFIED. ) 
 CURVE ( )  GEOMETRIC_REPRESENTATION_ITEM ( )  RATIONAL_B_SPLINE_CURVE ( ( 1.000000000000137446, 0.9510565162950160856, 1.000000000000000000, 0.9510565162951535312, 1.000000000000000000, 0.9510565162951535312, 1.000000000000000000, 0.9510565162951535312, 1.000000000000000000, 0.9510565162952959728, 0.9999999999998575584 ) ) 
 REPRESENTATION_ITEM ( '' )  );
#59621 = LINE ( 'NONE', #59260, #39418 ) ;
#59622 = CARTESIAN_POINT ( 'NONE',  ( -60.74499999999997613, 4.716976649647094177, 6.492361379858945902 ) ) ;
#59623 = EDGE_CURVE ( 'NONE', #1575, #64348, #60752, .T. ) ;
#59624 = CARTESIAN_POINT ( 'NONE',  ( -139.6429263765338078, -5.598654528085801552, 7.705886871421367523 ) ) ;
#59625 = FACE_OUTER_BOUND ( 'NONE', #43621, .T. ) ;
#59626 = AXIS2_PLACEMENT_3D ( 'NONE', #69100, #20901, #37822 ) ;
#59627 = FILL_AREA_STYLE ('',( #1170 ) ) ;
#59628 = STYLED_ITEM ( 'NONE', ( #53008 ), #34790 ) ;
#59629 = CARTESIAN_POINT ( 'NONE',  ( -101.9929263765338021, 8.102448949553171076, -5.886773742842744461 ) ) ;
#59630 = CARTESIAN_POINT ( 'NONE',  ( -6.799999999999979394, 26.00000000000000711, 23.99999999999999289 ) ) ;
#59631 = EDGE_CURVE ( 'NONE', #54902, #43549, #61872, .T. ) ;
#59632 = DIRECTION ( 'NONE',  ( 1.000000000000000000, 0.000000000000000000, 0.000000000000000000 ) ) ;
#59633 = CIRCLE ( 'NONE', #43969, 0.4999999999999991118 ) ;
#59634 = CARTESIAN_POINT ( 'NONE',  ( -44.99999999999998579, 119.9999999999999716, 7.000000000000000000 ) ) ;
#59635 = DIRECTION ( 'NONE',  ( 0.000000000000000000, 0.000000000000000000, 1.000000000000000000 ) ) ;
#59636 = AXIS2_PLACEMENT_3D ( 'NONE', #47064, #15049, #30474 ) ;
#59637 = ORIENTED_EDGE ( 'NONE', *, *, #64894, .T. ) ;
#59638 = VECTOR ( 'NONE', #11840, 1000.000000000000000 ) ;
#59639 = CARTESIAN_POINT ( 'NONE',  ( -69.74999999999998579, -3.000000000000000000, 0.000000000000000000 ) ) ;
#59640 = ADVANCED_FACE ( 'NONE', ( #9829 ), #30369, .F. ) ;
#59641 = DIRECTION ( 'NONE',  ( -0.000000000000000000, -0.000000000000000000, -1.000000000000000000 ) ) ;
#59642 = EDGE_LOOP ( 'NONE', ( #29586, #18504, #48493 ) ) ;
#59643 = LINE ( 'NONE', #27953, #47746 ) ;
#59644 =( BOUNDED_CURVE ( )  B_SPLINE_CURVE ( 3, ( #36537, #4441, #26265, #20294 ),
 .UNSPECIFIED., .F., .F. ) 
 B_SPLINE_CURVE_WITH_KNOTS ( ( 4, 4 ),
 ( 4.712388980384691450, 6.283185307179586232 ),
 .UNSPECIFIED. ) 
 CURVE ( )  GEOMETRIC_REPRESENTATION_ITEM ( )  RATIONAL_B_SPLINE_CURVE ( ( 1.000000000000000000, 0.8047378541243654926, 0.8047378541243654926, 1.000000000000000000 ) ) 
 REPRESENTATION_ITEM ( '' )  );
#59645 = CARTESIAN_POINT ( 'NONE',  ( -2.607480562269075097, 110.4070736234661467, 8.025000000000000355 ) ) ;
#59646 = DIRECTION ( 'NONE',  ( 0.7071067811865352493, 8.659560562354782482E-17, -0.7071067811865597852 ) ) ;
#59648 = EDGE_CURVE ( 'NONE', #33374, #29900, #60709, .T. ) ;
#59647 = DIRECTION ( 'NONE',  ( 0.000000000000000000, 1.000000000000000000, -0.000000000000000000 ) ) ;
#59649 = CARTESIAN_POINT ( 'NONE',  ( 75.00000000000000000, 19.99999999999998224, -5.999999999999998224 ) ) ;
#59650 = MECHANICAL_DESIGN_GEOMETRIC_PRESENTATION_REPRESENTATION (  '', ( #52952 ), #31586 ) ;
#59651 = EDGE_LOOP ( 'NONE', ( #14845, #61887, #2708, #57349 ) ) ;
#59652 = ORIENTED_EDGE ( 'NONE', *, *, #44823, .T. ) ;
#59653 = CYLINDRICAL_SURFACE ( 'NONE', #23128, 1.000000000000000888 ) ;
#59654 = DIRECTION ( 'NONE',  ( -1.000000000000000000, 0.000000000000000000, 0.000000000000000000 ) ) ;
#59655 = ORIENTED_EDGE ( 'NONE', *, *, #68767, .F. ) ;
#59656 =( NAMED_UNIT ( * ) PLANE_ANGLE_UNIT ( ) SI_UNIT ( $, .RADIAN. ) );
#59657 = AXIS2_PLACEMENT_3D ( 'NONE', #34897, #34544, #67254 ) ;
#59658 = CARTESIAN_POINT ( 'NONE',  ( 6.826472737025119919, 133.8929263765338078, 4.959722759717908325 ) ) ;
#59659 = CARTESIAN_POINT ( 'NONE',  ( -88.79499999999998749, 2.607480562269068880, -8.024999999999993250 ) ) ;
#59660 = EDGE_LOOP ( 'NONE', ( #25227, #52747, #34832, #66839 ) ) ;
#59661 = VECTOR ( 'NONE', #66683, 1000.000000000000000 ) ;
#59662 = CARTESIAN_POINT ( 'NONE',  ( 74.50000000000000000, -2.220952357103124925E-14, -6.500000000000000000 ) ) ;
#59663 = FILL_AREA_STYLE ('',( #61047 ) ) ;
#59664 = ORIENTED_EDGE ( 'NONE', *, *, #17209, .T. ) ;
#59665 = DIRECTION ( 'NONE',  ( 1.156482317317870344E-15, -1.000000000000000000, 0.000000000000000000 ) ) ;
#59666 = STYLED_ITEM ( 'NONE', ( #51687 ), #13575 ) ;
#59667 = DIRECTION ( 'NONE',  ( -6.591949208711860648E-14, 0.000000000000000000, 1.000000000000000000 ) ) ;
#59668 = CARTESIAN_POINT ( 'NONE',  ( 0.000000000000000000, 0.000000000000000000, 52.50000000000000000 ) ) ;
#59669 = ORIENTED_EDGE ( 'NONE', *, *, #60201, .T. ) ;
#59670 = AXIS2_PLACEMENT_3D ( 'NONE', #32059, #43011, #5644 ) ;
#59671 = FACE_OUTER_BOUND ( 'NONE', #2117, .T. ) ;
#59672 = EDGE_LOOP ( 'NONE', ( #68969, #38184, #35626, #11725, #67653 ) ) ;
#59673 = CARTESIAN_POINT ( 'NONE',  ( -166.5570736234661808, -1.166476076187852838E-15, -9.524999999999991473 ) ) ;
#59674 = CARTESIAN_POINT ( 'NONE',  ( -195.0000000000000000, 0.000000000000000000, 0.000000000000000000 ) ) ;
#59675 =( NAMED_UNIT ( * ) SI_UNIT ( $, .STERADIAN. ) SOLID_ANGLE_UNIT ( ) );
#59676 = DIRECTION ( 'NONE',  ( 0.000000000000000000, 0.000000000000000000, -1.000000000000000000 ) ) ;
#59677 = DIRECTION ( 'NONE',  ( 0.000000000000000000, 0.000000000000000000, 1.000000000000000000 ) ) ;
#59678 = ADVANCED_FACE ( 'NONE', ( #58020 ), #31241, .F. ) ;
#59679 = AXIS2_PLACEMENT_3D ( 'NONE', #21665, #16077, #58607 ) ;
#59680 = CARTESIAN_POINT ( 'NONE',  ( 11.00000000000001776, 15.00000000000000000, -29.68999999999999417 ) ) ;
#59681 = CARTESIAN_POINT ( 'NONE',  ( -8.234833373661349043, 153.6756281844815248, 2.821501943811211888 ) ) ;
#59682 = ORIENTED_EDGE ( 'NONE', *, *, #10660, .T. ) ;
#59683 = VECTOR ( 'NONE', #20893, 1000.000000000000000 ) ;
#59684 = CARTESIAN_POINT ( 'NONE',  ( -161.2429263765338021, 5.598654528085804216, 7.705886871421366635 ) ) ;
#59685 = DIRECTION ( 'NONE',  ( 0.000000000000000000, 0.000000000000000000, 1.000000000000000000 ) ) ;
#59686 = CARTESIAN_POINT ( 'NONE',  ( -149.1570736234661751, -9.058813317711329915, -2.943386871421370898 ) ) ;
#59687 = CARTESIAN_POINT ( 'NONE',  ( 48.50000000000000000, 14.49137674618942562, -7.000000000000000000 ) ) ;
#59688 = VERTEX_POINT ( 'NONE', #32632 ) ;
#59689 = PRESENTATION_STYLE_ASSIGNMENT (( #32978 ) ) ;
#59690 = CARTESIAN_POINT ( 'NONE',  ( -168.6550000000000011, -7.632228543268600340, -2.479861379858950166 ) ) ;
#59691 = CARTESIAN_POINT ( 'NONE',  ( -58.75000000000000000, -8.499999999999992895, 15.00000000000000178 ) ) ;
#59692 = DIRECTION ( 'NONE',  ( -0.7071067811865474617, 8.659560562354932858E-17, 0.7071067811865474617 ) ) ;
#59693 = COLOUR_RGB ( '', 0.31764706, 0.68627451, 0.89019608) ;
#59694 = CARTESIAN_POINT ( 'NONE',  ( -177.1450000000000102, -4.716976649647092401, 6.492361379858946790 ) ) ;
#59695 = CARTESIAN_POINT ( 'NONE',  ( -169.6449999999999818, 4.716976649647091513, -6.492361379858946790 ) ) ;
#59696 = VECTOR ( 'NONE', #59191, 1000.000000000000000 ) ;
#59697 = EDGE_LOOP ( 'NONE', ( #4008, #757, #47732, #62372 ) ) ;
#59698 = PRODUCT_DEFINITION ( 'UNKNOWN', '', #41676, #7902 ) ;
#59699 = CARTESIAN_POINT ( 'NONE',  ( -45.50000000000000000, -2.024042244987997205E-14, 9.500000000000000000 ) ) ;
#59700 = VECTOR ( 'NONE', #56922, 1000.000000000000000 ) ;
#59701 = ADVANCED_FACE ( 'NONE', ( #49189 ), #64668, .T. ) ;
#59702 = DIRECTION ( 'NONE',  ( 5.782411586589351722E-16, 1.000000000000000000, 0.000000000000000000 ) ) ;
#59703 =( NAMED_UNIT ( * ) SI_UNIT ( $, .STERADIAN. ) SOLID_ANGLE_UNIT ( ) );
#59704 = CARTESIAN_POINT ( 'NONE',  ( -83.90500000000000114, 2.607480562269068880, -8.024999999999993250 ) ) ;
#59705 = LINE ( 'NONE', #42901, #39357 ) ;
#59706 = VECTOR ( 'NONE', #39839, 1000.000000000000000 ) ;
#59707 = DIRECTION ( 'NONE',  ( 0.000000000000000000, 1.350863103983176297E-16, -1.000000000000000000 ) ) ;
#59708 = ADVANCED_FACE ( 'NONE', ( #15465 ), #31540, .T. ) ;
#59709 = CARTESIAN_POINT ( 'NONE',  ( -78.14499999999999602, -4.716976649647092401, 6.492361379858946790 ) ) ;
#59710 = EDGE_CURVE ( 'NONE', #30297, #52608, #61870, .T. ) ;
#59711 = CARTESIAN_POINT ( 'NONE',  ( -3.094860106618434248, 132.9050000000000011, 9.525000000000000355 ) ) ;
#59712 = CARTESIAN_POINT ( 'NONE',  ( 6.938426666069066329, -1.982292489777644828, 0.2088670156639322040 ) ) ;
#59713 = PRESENTATION_LAYER_ASSIGNMENT (  '', '', ( #53004 ) ) ;
#59714 =( LENGTH_UNIT ( ) NAMED_UNIT ( * ) SI_UNIT ( .MILLI., .METRE. ) );
#59715 = LINE ( 'NONE', #7990, #60750 ) ;
#59717 = EDGE_LOOP ( 'NONE', ( #55763, #17679, #20136 ) ) ;
#59716 = PRESENTATION_LAYER_ASSIGNMENT (  '', '', ( #12505 ) ) ;
#59718 = ADVANCED_FACE ( 'NONE', ( #16844 ), #40569, .F. ) ;
#59719 = PRESENTATION_LAYER_ASSIGNMENT (  '', '', ( #41789 ) ) ;
#59720 =( NAMED_UNIT ( * ) SI_UNIT ( $, .STERADIAN. ) SOLID_ANGLE_UNIT ( ) );
#59721 = CIRCLE ( 'NONE', #8065, 0.5000000000000004441 ) ;
#59722 = EDGE_CURVE ( 'NONE', #19333, #43779, #59715, .T. ) ;
#59723 = AXIS2_PLACEMENT_3D ( 'NONE', #24392, #9644, #68367 ) ;
#59724 = SURFACE_SIDE_STYLE ('',( #63014 ) ) ;
#59725 = DIRECTION ( 'NONE',  ( 1.000000000000000000, 0.000000000000000000, 0.000000000000000000 ) ) ;
#59726 = EDGE_CURVE ( 'NONE', #15864, #34648, #50222, .T. ) ;
#59727 = CARTESIAN_POINT ( 'NONE',  ( -74.99999999999998579, 50.00000000000000000, -6.500000000000000000 ) ) ;
#59728 = ORIENTED_EDGE ( 'NONE', *, *, #49967, .F. ) ;
#59729 = ORIENTED_EDGE ( 'NONE', *, *, #21047, .T. ) ;
#59730 = SURFACE_STYLE_FILL_AREA ( #12217 ) ;
#59731 = COLOUR_RGB ( '', 0.72549020, 0.75294118, 0.79215686) ;
#59732 = FACE_OUTER_BOUND ( 'NONE', #4819, .T. ) ;
#59733 = AXIS2_PLACEMENT_3D ( 'NONE', #51185, #34995, #2933 ) ;
#59734 = EDGE_CURVE ( 'NONE', #57680, #47261, #44293, .T. ) ;
#59735 = DIRECTION ( 'NONE',  ( 0.000000000000000000, 0.000000000000000000, 1.000000000000000000 ) ) ;
#59736 = FACE_OUTER_BOUND ( 'NONE', #53878, .T. ) ;
#59737 = CARTESIAN_POINT ( 'NONE',  ( 13.25000000000000355, 27.99999999999998934, 3.750000000000000000 ) ) ;
#59738 = ORIENTED_EDGE ( 'NONE', *, *, #54761, .F. ) ;
#59739 = CARTESIAN_POINT ( 'NONE',  ( -113.1549999999999869, 7.632228543268600340, 2.479861379858949277 ) ) ;
#59740 = EDGE_LOOP ( 'NONE', ( #33639, #28501, #30268, #31045 ) ) ;
#59741 =( NAMED_UNIT ( * ) SI_UNIT ( $, .STERADIAN. ) SOLID_ANGLE_UNIT ( ) );
#59742 = FACE_OUTER_BOUND ( 'NONE', #44393, .T. ) ;
#59743 = VECTOR ( 'NONE', #31207, 1000.000000000000000 ) ;
#59744 = ORIENTED_EDGE ( 'NONE', *, *, #42387, .T. ) ;
#59745 = FACE_OUTER_BOUND ( 'NONE', #3102, .T. ) ;
#59746 = EDGE_LOOP ( 'NONE', ( #37021, #44167 ) ) ;
#59747 = VECTOR ( 'NONE', #1325, 1000.000000000000000 ) ;
#59748 = CARTESIAN_POINT ( 'NONE',  ( 0.000000000000000000, 157.4449999999999932, -9.525000000000000355 ) ) ;
#59749 =( NAMED_UNIT ( * ) SI_UNIT ( $, .STERADIAN. ) SOLID_ANGLE_UNIT ( ) );
#59750 = ORIENTED_EDGE ( 'NONE', *, *, #33826, .T. ) ;
#59751 =( BOUNDED_CURVE ( )  B_SPLINE_CURVE ( 2, ( #49895, #7320, #12566, #32644, #43606, #64996, #16519, #229, #39014, #43945, #27695 ),
 .UNSPECIFIED., .F., .F. ) 
 B_SPLINE_CURVE_WITH_KNOTS ( ( 3, 2, 2, 2, 2, 3 ),
 ( 0.4705882352941177516, 0.4764705882352942012, 0.4823529411764707620, 0.4882352941176472116, 0.4941176470588237724, 0.5000000000000002220 ),
 .UNSPECIFIED. ) 
 CURVE ( )  GEOMETRIC_REPRESENTATION_ITEM ( )  RATIONAL_B_SPLINE_CURVE ( ( 0.9999999999999991118, 0.9510565162951544194, 1.000000000000000000, 0.9510565162951535312, 1.000000000000000000, 0.9510565162951535312, 1.000000000000000000, 0.9510565162951535312, 1.000000000000000000, 0.9510565162951516438, 1.000000000000001776 ) ) 
 REPRESENTATION_ITEM ( '' )  );
#59752 = ORIENTED_EDGE ( 'NONE', *, *, #334, .T. ) ;
#59753 = CIRCLE ( 'NONE', #19325, 23.00000000000000355 ) ;
#59754 = CARTESIAN_POINT ( 'NONE',  ( -117.6570736234661894, 9.058813317711329915, 2.943386871421369566 ) ) ;
#59755 =( NAMED_UNIT ( * ) SI_UNIT ( $, .STERADIAN. ) SOLID_ANGLE_UNIT ( ) );
#59756 = CARTESIAN_POINT ( 'NONE',  ( 57.00000000000000000, 14.00000000000000000, -60.00402776293825724 ) ) ;
#59757 = ORIENTED_EDGE ( 'NONE', *, *, #69200, .T. ) ;
#59758 = CARTESIAN_POINT ( 'NONE',  ( 6.826472737025121695, 134.4929263765338305, -4.959722759717905660 ) ) ;
#59759 = DIRECTION ( 'NONE',  ( -1.000000000000000000, 0.000000000000000000, 0.000000000000000000 ) ) ;
#59760 = CYLINDRICAL_SURFACE ( 'NONE', #60225, 9.524999999999991473 ) ;
#59761 = VECTOR ( 'NONE', #15257, 1000.000000000000000 ) ;
#59762 = CYLINDRICAL_SURFACE ( 'NONE', #41893, 3.499999999999999556 ) ;
#59763 = DIRECTION ( 'NONE',  ( 1.000000000000000000, 0.000000000000000000, 0.000000000000000000 ) ) ;
#59764 = ORIENTED_EDGE ( 'NONE', *, *, #11354, .T. ) ;
#59765 = LINE ( 'NONE', #12957, #3716 ) ;
#59766 = ORIENTED_EDGE ( 'NONE', *, *, #9987, .F. ) ;
#59767 = CARTESIAN_POINT ( 'NONE',  ( -48.89292637653380780, -8.102448949553172852, -5.886773742842741797 ) ) ;
#59768 =( NAMED_UNIT ( * ) SI_UNIT ( $, .STERADIAN. ) SOLID_ANGLE_UNIT ( ) );
#59769 = CYLINDRICAL_SURFACE ( 'NONE', #46478, 0.2500000000000002220 ) ;
#59770 = DIRECTION ( 'NONE',  ( 0.000000000000000000, 0.000000000000000000, -1.000000000000000000 ) ) ;
#59772 = CARTESIAN_POINT ( 'NONE',  ( -139.1049999999999898, -6.826472737025115478, 4.959722759717900331 ) ) ;
#59771 = STYLED_ITEM ( 'NONE', ( #7995 ), #60722 ) ;
#59773 = CARTESIAN_POINT ( 'NONE',  ( -44.50000000000000000, 9.499999999999980460, -3.000000000000000444 ) ) ;
#59774 = DIRECTION ( 'NONE',  ( 0.000000000000000000, 0.000000000000000000, 1.000000000000000000 ) ) ;
#59775 = ORIENTED_EDGE ( 'NONE', *, *, #36687, .T. ) ;
#59776 = MECHANICAL_DESIGN_GEOMETRIC_PRESENTATION_REPRESENTATION (  '', ( #63143 ), #68784 ) ;
#59777 = AXIS2_PLACEMENT_3D ( 'NONE', #16923, #1350, #44028 ) ;
#59778 = CARTESIAN_POINT ( 'NONE',  ( -7.632228543268608334, 115.9570736234661581, 2.479861379858952830 ) ) ;
#59779 = DIRECTION ( 'NONE',  ( -0.000000000000000000, -1.000000000000000000, -0.000000000000000000 ) ) ;
#59780 = FACE_OUTER_BOUND ( 'NONE', #68687, .T. ) ;
#59781 = ORIENTED_EDGE ( 'NONE', *, *, #37200, .T. ) ;
#59782 = AXIS2_PLACEMENT_3D ( 'NONE', #23407, #7585, #8986 ) ;
#59783 = ORIENTED_EDGE ( 'NONE', *, *, #36348, .F. ) ;
#59784 = CARTESIAN_POINT ( 'NONE',  ( -195.0000000000000000, 0.000000000000000000, 0.000000000000000000 ) ) ;
#59785 = CARTESIAN_POINT ( 'NONE',  ( -108.8929263765338078, -8.102448949553174629, -5.886773742842741797 ) ) ;
#59786 = CARTESIAN_POINT ( 'NONE',  ( -57.35499999999998977, -4.716976649647093289, -6.492361379858945902 ) ) ;
#59787 = ORIENTED_EDGE ( 'NONE', *, *, #47883, .F. ) ;
#59788 =( NAMED_UNIT ( * ) SI_UNIT ( $, .STERADIAN. ) SOLID_ANGLE_UNIT ( ) );
#59789 = SURFACE_STYLE_USAGE ( .BOTH. , #64022 ) ;
#59790 = AXIS2_PLACEMENT_3D ( 'NONE', #12927, #13978, #34392 ) ;
#59791 = CYLINDRICAL_SURFACE ( 'NONE', #26749, 0.5000000000000004441 ) ;
#59792 = AXIS2_PLACEMENT_3D ( 'NONE', #50591, #2698, #13636 ) ;
#59793 = CARTESIAN_POINT ( 'NONE',  ( 60.00000000000000000, 115.4999999999999574, -10.50000000000000000 ) ) ;
#59794 = CYLINDRICAL_SURFACE ( 'NONE', #5033, 8.025000000000000355 ) ;
#59795 = ORIENTED_EDGE ( 'NONE', *, *, #59269, .T. ) ;
#59796 = COLOUR_RGB ( '', 0.09019608, 0.27058824, 0.51372549) ;
#59797 = EDGE_CURVE ( 'NONE', #68610, #2459, #65345, .T. ) ;
#59798 = PLANE ( 'NONE',  #51544 ) ;
#59799 = CARTESIAN_POINT ( 'NONE',  ( 52.99999999999999289, 27.74999999999998579, -3.750000000000000000 ) ) ;
#59800 = SURFACE_STYLE_FILL_AREA ( #38398 ) ;
#59801 = EDGE_CURVE ( 'NONE', #62258, #58402, #28374, .T. ) ;
#59802 = EDGE_CURVE ( 'NONE', #13725, #49467, #32645, .T. ) ;
#59803 = CARTESIAN_POINT ( 'NONE',  ( -108.7449999999999903, 4.716976649647094177, 6.492361379858945902 ) ) ;
#59804 = CARTESIAN_POINT ( 'NONE',  ( -10.01517768586949231, 155.1949999999999648, -6.132527647946036459E-16 ) ) ;
#59805 = CARTESIAN_POINT ( 'NONE',  ( -88.19499999999996476, 8.437984349512085203, -1.550032578732815448E-15 ) ) ;
#59806 = COLOUR_RGB ( '', 0.66274510, 0.83137255, 0.94901961) ;
#59807 = DIRECTION ( 'NONE',  ( -1.000000000000000000, 0.000000000000000000, 0.000000000000000000 ) ) ;
#59808 = FACE_BOUND ( 'NONE', #24670, .T. ) ;
#59809 = CARTESIAN_POINT ( 'NONE',  ( 52.49999999999998579, 2.715530000339800426E-15, -11.50000000000000000 ) ) ;
#59810 = CIRCLE ( 'NONE', #27242, 2.499999999999999556 ) ;
#59811 = ORIENTED_EDGE ( 'NONE', *, *, #22161, .T. ) ;
#59812 = CARTESIAN_POINT ( 'NONE',  ( -126.4429263765338192, -1.166476076187852838E-15, -9.524999999999991473 ) ) ;
#59813 = SURFACE_STYLE_USAGE ( .BOTH. , #7398 ) ;
#59814 = CARTESIAN_POINT ( 'NONE',  ( -146.2449999999999761, -4.716976649647093289, -6.492361379858945902 ) ) ;
#59815 = SURFACE_SIDE_STYLE ('',( #58434 ) ) ;
#59816 = PRESENTATION_LAYER_ASSIGNMENT (  '', '', ( #47516 ) ) ;
#59817 = EDGE_CURVE ( 'NONE', #12327, #48755, #58520, .T. ) ;
#59818 = ORIENTED_EDGE ( 'NONE', *, *, #47772, .T. ) ;
#59820 = ORIENTED_EDGE ( 'NONE', *, *, #8594, .T. ) ;
#59819 = CIRCLE ( 'NONE', #11556, 9.499999999999994671 ) ;
#59821 = AXIS2_PLACEMENT_3D ( 'NONE', #55766, #55409, #6876 ) ;
#59822 = DIRECTION ( 'NONE',  ( -1.000000000000000000, 0.000000000000000000, 0.000000000000000000 ) ) ;
#59823 = FILL_AREA_STYLE ('',( #43692 ) ) ;
#59824 = AXIS2_PLACEMENT_3D ( 'NONE', #14423, #63997, #36637 ) ;
#59825 = CARTESIAN_POINT ( 'NONE',  ( -22.75000000000000711, 37.00000000000000000, 4.000000000000000000 ) ) ;
#59826 = CARTESIAN_POINT ( 'NONE',  ( 0.000000000000000000, 42.00000000000000000, 35.50000000000000000 ) ) ;
#59827 = CARTESIAN_POINT ( 'NONE',  ( -151.4929263765338021, -8.102448949553174629, 5.886773742842742685 ) ) ;
#59828 = VERTEX_POINT ( 'NONE', #43936 ) ;
#59829 = CARTESIAN_POINT ( 'NONE',  ( -141.6550000000000011, -7.632228543268600340, -2.479861379858950166 ) ) ;
#59830 = ORIENTED_EDGE ( 'NONE', *, *, #29954, .T. ) ;
#59831 = CIRCLE ( 'NONE', #29504, 0.5000000000000004441 ) ;
#59832 = ADVANCED_FACE ( 'NONE', ( #17198 ), #21465, .T. ) ;
#59833 = ORIENTED_EDGE ( 'NONE', *, *, #39023, .F. ) ;
#59834 = DIRECTION ( 'NONE',  ( 0.000000000000000000, 0.000000000000000000, -1.000000000000000000 ) ) ;
#59835 = PLANE ( 'NONE',  #37799 ) ;
#59836 = AXIS2_PLACEMENT_3D ( 'NONE', #51793, #37405, #69369 ) ;
#59837 = ORIENTED_EDGE ( 'NONE', *, *, #51088, .F. ) ;
#59838 = CARTESIAN_POINT ( 'NONE',  ( -0.9109038252169214811, 2.456844516558468694, -9.000000000000003553 ) ) ;
#59839 = VECTOR ( 'NONE', #2150, 1000.000000000000000 ) ;
#59840 = ADVANCED_FACE ( 'NONE', ( #17858 ), #52912, .T. ) ;
#59841 = CARTESIAN_POINT ( 'NONE',  ( 1.227708416145222385E-15, 109.9999999999999858, 10.02500000000000568 ) ) ;
#59842 = CARTESIAN_POINT ( 'NONE',  ( 8.102448949553181734, 126.3949999999999818, 5.886773742842750679 ) ) ;
#59843 = DIRECTION ( 'NONE',  ( 0.000000000000000000, -1.000000000000000000, 0.000000000000000000 ) ) ;
#59844 = ORIENTED_EDGE ( 'NONE', *, *, #56688, .F. ) ;
#59845 = FACE_BOUND ( 'NONE', #17317, .T. ) ;
#59846 = CARTESIAN_POINT ( 'NONE',  ( 5.598654528085809545, 131.2549999999999955, -7.705886871421373741 ) ) ;
#59847 = CARTESIAN_POINT ( 'NONE',  ( -57.50499999999997414, -6.826472737025113702, -4.959722759717900331 ) ) ;
#59848 = CARTESIAN_POINT ( 'NONE',  ( -117.2949999999999875, -2.607480562269069768, 8.024999999999991473 ) ) ;
#59849 = CARTESIAN_POINT ( 'NONE',  ( -41.84210526315788314, 107.2928455055531600, -3.499999999999996891 ) ) ;
#59850 = EDGE_LOOP ( 'NONE', ( #59795, #5750, #3598, #69394 ) ) ;
#59851 = CARTESIAN_POINT ( 'NONE',  ( -5.598654528085808657, 159.7549999999999670, 7.705886871421373741 ) ) ;
#59852 = CARTESIAN_POINT ( 'NONE',  ( -12.48999599679679662, 115.4999999999999574, 10.00000000000000000 ) ) ;
#59853 = SURFACE_STYLE_USAGE ( .BOTH. , #5329 ) ;
#59854 = DIRECTION ( 'NONE',  ( -1.000000000000000000, 0.000000000000000000, 0.000000000000000000 ) ) ;
#59855 = CARTESIAN_POINT ( 'NONE',  ( -21.02379604162863913, 110.4999999999999858, 10.00000000000000000 ) ) ;
#59856 = AXIS2_PLACEMENT_3D ( 'NONE', #42200, #10484, #24905 ) ;
#59857 = CARTESIAN_POINT ( 'NONE',  ( 62.24999999999998579, 0.000000000000000000, 4.000000000000000000 ) ) ;
#59858 = ORIENTED_EDGE ( 'NONE', *, *, #11928, .T. ) ;
#59859 = CARTESIAN_POINT ( 'NONE',  ( -33.89861119020018521, -9.947368421756124235, -2.262137787255368515 ) ) ;
#59860 = DIRECTION ( 'NONE',  ( -1.000000000000000000, 0.000000000000000000, 0.000000000000000000 ) ) ;
#59861 = CARTESIAN_POINT ( 'NONE',  ( -172.4050000000000296, -2.607480562269069768, 8.024999999999991473 ) ) ;
#59862 = ORIENTED_EDGE ( 'NONE', *, *, #66654, .F. ) ;
#59863 = LINE ( 'NONE', #32785, #30566 ) ;
#59864 = MECHANICAL_DESIGN_GEOMETRIC_PRESENTATION_REPRESENTATION (  '', ( #8202 ), #41985 ) ;
#59865 = DIRECTION ( 'NONE',  ( -0.000000000000000000, -0.000000000000000000, -1.000000000000000000 ) ) ;
#59866 = ORIENTED_EDGE ( 'NONE', *, *, #9722, .F. ) ;
#59867 = AXIS2_PLACEMENT_3D ( 'NONE', #58068, #14112, #51389 ) ;
#59868 = CARTESIAN_POINT ( 'NONE',  ( -18.25000000000000711, 33.74999999999999289, -3.750000000000000000 ) ) ;
#59869 = CARTESIAN_POINT ( 'NONE',  ( -89.30499999999999261, 8.437984349512085203, -1.550032578732815448E-15 ) ) ;
#59870 = EDGE_LOOP ( 'NONE', ( #50880, #56262, #1571, #65376, #22138 ) ) ;
#59871 = ADVANCED_FACE ( 'NONE', ( #12202 ), #61193, .F. ) ;
#59872 = AXIS2_PLACEMENT_3D ( 'NONE', #51651, #24540, #18612 ) ;
#59873 = SURFACE_STYLE_FILL_AREA ( #16988 ) ;
#59874 = CARTESIAN_POINT ( 'NONE',  ( -63.20707362346617231, 3.094860106618433360, 9.524999999999991473 ) ) ;
#59875 = ORIENTED_EDGE ( 'NONE', *, *, #17189, .T. ) ;
#59876 = FACE_OUTER_BOUND ( 'NONE', #65481, .T. ) ;
#59878 = LINE ( 'NONE', #22955, #38209 ) ;
#59877 = CARTESIAN_POINT ( 'NONE',  ( -71.50000000000000000, 36.32520566882265456, -7.000000000000000000 ) ) ;
#59879 = CARTESIAN_POINT ( 'NONE',  ( -106.8549999999999898, 4.716976649647094177, 6.492361379858945902 ) ) ;
#59880 = ADVANCED_FACE ( 'NONE', ( #36425 ), #31079, .F. ) ;
#59881 = CARTESIAN_POINT ( 'NONE',  ( -3.094860106618432471, 127.5949999999999847, -9.525000000000000355 ) ) ;
#59882 = AXIS2_PLACEMENT_3D ( 'NONE', #22826, #44324, #65722 ) ;
#59883 = CARTESIAN_POINT ( 'NONE',  ( -119.0949999999999847, -2.607480562269071545, -8.024999999999991473 ) ) ;
#59884 = CIRCLE ( 'NONE', #67777, 0.2500000000000002220 ) ;
#59885 = DIRECTION ( 'NONE',  ( -0.000000000000000000, 1.000000000000000000, -0.000000000000000000 ) ) ;
#59886 = VECTOR ( 'NONE', #20768, 1000.000000000000000 ) ;
#59888 = CARTESIAN_POINT ( 'NONE',  ( 1.000000000000000888, 0.9999999999999991118, 80.00402776293826435 ) ) ;
#59887 = CARTESIAN_POINT ( 'NONE',  ( -14.98999599679678951, 1.797044900979284448E-15, -9.500000000000000000 ) ) ;
#59889 = CARTESIAN_POINT ( 'NONE',  ( -155.8429263765337964, 9.058813317711329915, -2.943386871421373119 ) ) ;
#59890 = AXIS2_PLACEMENT_3D ( 'NONE', #63295, #41182, #14774 ) ;
#59891 = FILL_AREA_STYLE_COLOUR ( '', #1039 ) ;
#59892 = CARTESIAN_POINT ( 'NONE',  ( -177.2950000000000159, -2.607480562269069768, 8.024999999999991473 ) ) ;
#59893 = ADVANCED_FACE ( 'NONE', ( #26495 ), #20538, .T. ) ;
#59894 =( GEOMETRIC_REPRESENTATION_CONTEXT ( 3 ) GLOBAL_UNCERTAINTY_ASSIGNED_CONTEXT ( ( #36368 ) ) GLOBAL_UNIT_ASSIGNED_CONTEXT ( ( #45424, #47505, #14389 ) ) REPRESENTATION_CONTEXT ( 'NONE', 'WORKASPACE' ) );
#59895 = CARTESIAN_POINT ( 'NONE',  ( -47.00571487472603849, -11.85301361210301430, 3.279042910798484645 ) ) ;
#59896 = VERTEX_POINT ( 'NONE', #47320 ) ;
#59897 =( NAMED_UNIT ( * ) SI_UNIT ( $, .STERADIAN. ) SOLID_ANGLE_UNIT ( ) );
#59898 = EDGE_LOOP ( 'NONE', ( #53467, #47869, #46919, #44542 ) ) ;
#59899 = CARTESIAN_POINT ( 'NONE',  ( -65.09292637653379643, 3.094860106618433360, 9.524999999999991473 ) ) ;
#59900 = CARTESIAN_POINT ( 'NONE',  ( -45.85105888842022637, 9.184645374706622789, 6.276135203588958156 ) ) ;
#59901 =( NAMED_UNIT ( * ) SI_UNIT ( $, .STERADIAN. ) SOLID_ANGLE_UNIT ( ) );
#59902 = CIRCLE ( 'NONE', #19431, 1.000000000000000888 ) ;
#59903 = CARTESIAN_POINT ( 'NONE',  ( -1.224646799147353207E-16, 1.000000000000000000, 4.000000000000000000 ) ) ;
#59904 = CARTESIAN_POINT ( 'NONE',  ( -12.72792206135785698, 115.4999999999999574, -10.50000000000000000 ) ) ;
#59905 = DIRECTION ( 'NONE',  ( 1.000000000000000000, 0.000000000000000000, 0.000000000000000000 ) ) ;
#59906 = DIRECTION ( 'NONE',  ( -0.3162277660168358873, 0.9486832980505145452, 0.000000000000000000 ) ) ;
#59907 = ORIENTED_EDGE ( 'NONE', *, *, #6104, .F. ) ;
#59908 = CARTESIAN_POINT ( 'NONE',  ( -165.3549999999999898, -4.716976649647093289, -6.492361379858945902 ) ) ;
#59909 = B_SPLINE_CURVE_WITH_KNOTS ( 'NONE', 3,
 ( #66438, #29495, #39396, #18255, #39742, #55883, #28429, #45379, #65753 ),
 .UNSPECIFIED., .F., .F.,
 ( 4, 2, 1, 2, 4 ),
 ( 0.007659788818331632332, 0.009746199297478889273, 0.01078940453705251774, 0.01131100715683933111, 0.01183260977662614621 ),
 .UNSPECIFIED. ) ;
#59910 = ORIENTED_EDGE ( 'NONE', *, *, #60560, .T. ) ;
#59911 =( NAMED_UNIT ( * ) PLANE_ANGLE_UNIT ( ) SI_UNIT ( $, .RADIAN. ) );
#59912 = LINE ( 'NONE', #54635, #45509 ) ;
#59913 = MECHANICAL_DESIGN_GEOMETRIC_PRESENTATION_REPRESENTATION (  '', ( #27303 ), #8264 ) ;
#59914 = AXIS2_PLACEMENT_3D ( 'NONE', #24265, #66855, #18316 ) ;
#59915 = FACE_OUTER_BOUND ( 'NONE', #69558, .T. ) ;
#59916 = CARTESIAN_POINT ( 'NONE',  ( -6.826472737025120807, 155.1070736234661069, 4.959722759717906548 ) ) ;
#59917 =( REPRESENTATION_RELATIONSHIP ('NONE','NONE', #5102, #60355 ) REPRESENTATION_RELATIONSHIP_WITH_TRANSFORMATION ( #11365 )SHAPE_REPRESENTATION_RELATIONSHIP( ) );
#59918 = AXIS2_PLACEMENT_3D ( 'NONE', #67302, #25426, #66968 ) ;
#59919 = VERTEX_POINT ( 'NONE', #9997 ) ;
#59920 = CARTESIAN_POINT ( 'NONE',  ( -80.00499999999999545, 6.826472737025115478, 4.959722759717899443 ) ) ;
#59921 =( LENGTH_UNIT ( ) NAMED_UNIT ( * ) SI_UNIT ( .MILLI., .METRE. ) );
#59922 = CARTESIAN_POINT ( 'NONE',  ( 16.75000000000000711, 27.74999999999998224, 4.000000000000000000 ) ) ;
#59923 = CARTESIAN_POINT ( 'NONE',  ( 44.50000000000000000, 99.99999999999998579, 4.000000000000000000 ) ) ;
#59924 = CARTESIAN_POINT ( 'NONE',  ( 7.999999999999989342, 5.000000000000000000, 37.00402776293825724 ) ) ;
#59925 = ORIENTED_EDGE ( 'NONE', *, *, #29632, .F. ) ;
#59927 = CARTESIAN_POINT ( 'NONE',  ( 48.00000000000000000, 14.49137674618942562, -10.00000000000000000 ) ) ;
#59926 = CIRCLE ( 'NONE', #3712, 0.2500000000000002220 ) ;
#59928 = CARTESIAN_POINT ( 'NONE',  ( -72.50000000000001421, 14.49137674618942562, -9.500000000000000000 ) ) ;
#59929 = CARTESIAN_POINT ( 'NONE',  ( -60.14499999999998892, -4.716976649647092401, 6.492361379858946790 ) ) ;
#59930 = EDGE_LOOP ( 'NONE', ( #7935, #36947, #1810, #61469 ) ) ;
#59931 = DIRECTION ( 'NONE',  ( 0.000000000000000000, -1.000000000000000000, 0.000000000000000000 ) ) ;
#59932 = DIRECTION ( 'NONE',  ( -0.000000000000000000, -0.000000000000000000, 1.000000000000000000 ) ) ;
#59933 = CARTESIAN_POINT ( 'NONE',  ( -45.00000000000000000, 9.025366258634486272, -6.779481487458365763 ) ) ;
#59934 = AXIS2_PLACEMENT_3D ( 'NONE', #10865, #32307, #53762 ) ;
#59935 = VERTEX_POINT ( 'NONE', #4699 ) ;
#59936 = VERTEX_POINT ( 'NONE', #36766 ) ;
#59937 = CIRCLE ( 'NONE', #68956, 0.5000000000000004441 ) ;
#59938 = CARTESIAN_POINT ( 'NONE',  ( 19.89974874213239886, 114.9999999999999574, -10.49999999999999645 ) ) ;
#59939 = CARTESIAN_POINT ( 'NONE',  ( -75.00000000000000000, 9.656580361551663216, 6.242521039668915250 ) ) ;
#59940 = CARTESIAN_POINT ( 'NONE',  ( -113.4549999999999841, 7.632228543268599452, -2.479861379858951942 ) ) ;
#59941 = ORIENTED_EDGE ( 'NONE', *, *, #2902, .T. ) ;
#59942 = FILL_AREA_STYLE ('',( #36888 ) ) ;
#59943 = CARTESIAN_POINT ( 'NONE',  ( 31.00000000000000355, 43.00000000000000000, -45.61250543006184444 ) ) ;
#59944 = EDGE_CURVE ( 'NONE', #27464, #16826, #39479, .T. ) ;
#59945 = DIRECTION ( 'NONE',  ( 1.000000000000000000, -0.000000000000000000, -0.000000000000000000 ) ) ;
#59946 = SURFACE_STYLE_FILL_AREA ( #4376 ) ;
#59947 = FACE_OUTER_BOUND ( 'NONE', #6124, .T. ) ;
#59948 = CARTESIAN_POINT ( 'NONE',  ( -147.0570736234661808, 0.000000000000000000, 9.524999999999991473 ) ) ;
#59949 = VECTOR ( 'NONE', #29560, 1000.000000000000000 ) ;
#59950 = CARTESIAN_POINT ( 'NONE',  ( 3.094860106618435136, 136.2949999999999875, -9.525000000000000355 ) ) ;
#59951 = EDGE_CURVE ( 'NONE', #31359, #13744, #20295, .T. ) ;
#59952 =( BOUNDED_CURVE ( )  B_SPLINE_CURVE ( 2, ( #69115, #63809, #37135, #10378, #54970, #50418, #22646, #39900, #38530, #66951, #27879 ),
 .UNSPECIFIED., .F., .F. ) 
 B_SPLINE_CURVE_WITH_KNOTS ( ( 3, 2, 2, 2, 2, 3 ),
 ( 0.4411764705882353921, 0.4470588235294118973, 0.4529411764705883470, 0.4588235294117647967, 0.4647058823529413019, 0.4705882352941177516 ),
 .UNSPECIFIED. ) 
 CURVE ( )  GEOMETRIC_REPRESENTATION_ITEM ( )  RATIONAL_B_SPLINE_CURVE ( ( 0.9999999999999991118, 0.9510565162951544194, 1.000000000000000000, 0.9510565162951535312, 1.000000000000000000, 0.9510565162951535312, 1.000000000000000000, 0.9510565162951535312, 1.000000000000000000, 0.9510565162951526430, 1.000000000000000888 ) ) 
 REPRESENTATION_ITEM ( '' )  );
#59953 = CARTESIAN_POINT ( 'NONE',  ( -90.95707362346617231, 9.058813317711329915, -2.943386871421373119 ) ) ;
#59954 = CIRCLE ( 'NONE', #68970, 7.249999999999999112 ) ;
#59955 = EDGE_CURVE ( 'NONE', #33110, #35954, #66387, .T. ) ;
#59956 = AXIS2_PLACEMENT_3D ( 'NONE', #12843, #19854, #13529 ) ;
#59957 = DIRECTION ( 'NONE',  ( -0.000000000000000000, -0.000000000000000000, -1.000000000000000000 ) ) ;
#59958 = ORIENTED_EDGE ( 'NONE', *, *, #26733, .T. ) ;
#59959 = EDGE_CURVE ( 'NONE', #1454, #23924, #26149, .T. ) ;
#59961 = LINE ( 'NONE', #69150, #68403 ) ;
#59960 =( NAMED_UNIT ( * ) PLANE_ANGLE_UNIT ( ) SI_UNIT ( $, .RADIAN. ) );
#59962 = PLANE ( 'NONE',  #47927 ) ;
#59963 = CARTESIAN_POINT ( 'NONE',  ( -129.0549999999999784, -9.827790563157499189E-16, -8.024999999999991473 ) ) ;
#59964 = EDGE_CURVE ( 'NONE', #4472, #57125, #20891, .T. ) ;
#59965 = FILL_AREA_STYLE ('',( #23040 ) ) ;
#59966 = CARTESIAN_POINT ( 'NONE',  ( -54.44292637653380496, -1.166476076187852838E-15, -9.524999999999991473 ) ) ;
#59967 = CARTESIAN_POINT ( 'NONE',  ( -148.4950000000000045, 6.826472737025113702, -4.959722759717902107 ) ) ;
#59968 = ADVANCED_FACE ( 'NONE', ( #48021 ), #67083, .T. ) ;
#59969 =( GEOMETRIC_REPRESENTATION_CONTEXT ( 3 ) GLOBAL_UNCERTAINTY_ASSIGNED_CONTEXT ( ( #44632 ) ) GLOBAL_UNIT_ASSIGNED_CONTEXT ( ( #60415, #3014, #12930 ) ) REPRESENTATION_CONTEXT ( 'NONE', 'WORKASPACE' ) );
#59970 = CARTESIAN_POINT ( 'NONE',  ( -127.6450000000000102, 4.716976649647091513, -6.492361379858946790 ) ) ;
#59971 = ADVANCED_FACE ( 'NONE', ( #37473 ), #7954, .T. ) ;
#59972 = ORIENTED_EDGE ( 'NONE', *, *, #17203, .T. ) ;
#59973 = FACE_OUTER_BOUND ( 'NONE', #53920, .T. ) ;
#59974 = EDGE_CURVE ( 'NONE', #66051, #2274, #8665, .T. ) ;
#59975 = UNCERTAINTY_MEASURE_WITH_UNIT (LENGTH_MEASURE( 1.000000000000000082E-05 ), #5040, 'distance_accuracy_value', 'NONE');
#59976 = CARTESIAN_POINT ( 'NONE',  ( -184.6429263765338078, -5.598654528085801552, 7.705886871421367523 ) ) ;
#59977 = CARTESIAN_POINT ( 'NONE',  ( 0.000000000000000000, 0.000000000000000000, 0.000000000000000000 ) ) ;
#59978 = CARTESIAN_POINT ( 'NONE',  ( -54.59499999999997044, 2.607480562269073321, 8.024999999999991473 ) ) ;
#59979 = CARTESIAN_POINT ( 'NONE',  ( -43.99999999999998579, 0.000000000000000000, 11.99999999999999467 ) ) ;
#59980 = CARTESIAN_POINT ( 'NONE',  ( -15.75000000000000000, -0.9999999999999995559, 20.00000000000000000 ) ) ;
#59981 = CARTESIAN_POINT ( 'NONE',  ( -75.65707362346617515, 9.058813317711329915, 2.943386871421369566 ) ) ;
#59982 = CARTESIAN_POINT ( 'NONE',  ( -93.74292637653380211, -5.598654528085803328, -7.705886871421366635 ) ) ;
#59983 = CARTESIAN_POINT ( 'NONE',  ( 1.700000000000152722, 100.0000000000000142, 75.00000000000000000 ) ) ;
#59984 = AXIS2_PLACEMENT_3D ( 'NONE', #31822, #48063, #63157 ) ;
#59985 =( NAMED_UNIT ( * ) SI_UNIT ( $, .STERADIAN. ) SOLID_ANGLE_UNIT ( ) );
#59986 = CARTESIAN_POINT ( 'NONE',  ( -163.2570736234661695, 5.598654528085800663, -7.705886871421367523 ) ) ;
#59987 = MECHANICAL_DESIGN_GEOMETRIC_PRESENTATION_REPRESENTATION (  '', ( #1540 ), #61092 ) ;
#59988 = DIRECTION ( 'NONE',  ( -0.000000000000000000, 1.000000000000000000, -0.000000000000000000 ) ) ;
#59989 = CYLINDRICAL_SURFACE ( 'NONE', #20108, 0.2500000000000002220 ) ;
#59990 = AXIS2_PLACEMENT_3D ( 'NONE', #24341, #35618, #12749 ) ;
#59991 = CARTESIAN_POINT ( 'NONE',  ( -87.50000000000000000, -3.500000000000000000, 0.000000000000000000 ) ) ;
#59992 = EDGE_LOOP ( 'NONE', ( #14993, #47993, #55940, #28662 ) ) ;
#59993 = DIRECTION ( 'NONE',  ( -0.000000000000000000, 0.000000000000000000, 1.000000000000000000 ) ) ;
#59994 = ORIENTED_EDGE ( 'NONE', *, *, #19817, .F. ) ;
#59995 = DIRECTION ( 'NONE',  ( 0.000000000000000000, 0.000000000000000000, -1.000000000000000000 ) ) ;
#59996 = AXIS2_PLACEMENT_3D ( 'NONE', #46573, #58128, #25064 ) ;
#59997 = CARTESIAN_POINT ( 'NONE',  ( -4.716976649647097730, 124.3570736234661496, -6.492361379858953896 ) ) ;
#59998 = AXIS2_PLACEMENT_3D ( 'NONE', #2645, #33325, #1240 ) ;
#59999 = VECTOR ( 'NONE', #56117, 1000.000000000000000 ) ;
#60000 = CARTESIAN_POINT ( 'NONE',  ( 20.94636006565341191, 149.9999999999999716, 9.500000000000000000 ) ) ;
#60001 = CARTESIAN_POINT ( 'NONE',  ( 7.632228543268607446, 138.1570736234661467, 2.479861379858954606 ) ) ;
#60002 = ORIENTED_EDGE ( 'NONE', *, *, #43719, .F. ) ;
#60003 = ORIENTED_EDGE ( 'NONE', *, *, #12836, .F. ) ;
#60004 = CARTESIAN_POINT ( 'NONE',  ( 1.000000000000000000, 36.99999999999999289, -3.000000000000000000 ) ) ;
#60005 = VECTOR ( 'NONE', #35228, 1000.000000000000000 ) ;
#60006 = CARTESIAN_POINT ( 'NONE',  ( -11.74999999999999645, -4.000000000000000000, 6.000000000000001776 ) ) ;
#60007 = VERTEX_POINT ( 'NONE', #16674 ) ;
#60008 = FILL_AREA_STYLE ('',( #6198 ) ) ;
#60009 = CARTESIAN_POINT ( 'NONE',  ( -4.000000000000000000, -2.499999999999999556, 0.000000000000000000 ) ) ;
#60010 = PRESENTATION_LAYER_ASSIGNMENT (  '', '', ( #28521 ) ) ;
#60011 = DIRECTION ( 'NONE',  ( 0.000000000000000000, 1.000000000000000000, -0.000000000000000000 ) ) ;
#60012 = CARTESIAN_POINT ( 'NONE',  ( -90.89499999999999602, 6.826472737025116366, 4.959722759717898555 ) ) ;
#60013 = ORIENTED_EDGE ( 'NONE', *, *, #52149, .F. ) ;
#60014 = SURFACE_SIDE_STYLE ('',( #2617 ) ) ;
#60015 = PRESENTATION_STYLE_ASSIGNMENT (( #7258 ) ) ;
#60016 = FACE_OUTER_BOUND ( 'NONE', #5781, .T. ) ;
#60017 = UNCERTAINTY_MEASURE_WITH_UNIT (LENGTH_MEASURE( 1.000000000000000082E-05 ), #69621, 'distance_accuracy_value', 'NONE');
#60018 = ORIENTED_EDGE ( 'NONE', *, *, #58106, .T. ) ;
#60019 = CARTESIAN_POINT ( 'NONE',  ( -175.3429263765338249, -9.058813317711329915, 2.943386871421371787 ) ) ;
#60020 = DIRECTION ( 'NONE',  ( 0.000000000000000000, -1.099520432716498821E-15, 1.000000000000000000 ) ) ;
#60021 = CARTESIAN_POINT ( 'NONE',  ( 7.342319042881613633, 2.499999999999998224, -5.282730372348551029 ) ) ;
#60022 = ADVANCED_FACE ( 'NONE', ( #38836 ), #29276, .T. ) ;
#60023 = VERTEX_POINT ( 'NONE', #43087 ) ;
#60024 =( LENGTH_UNIT ( ) NAMED_UNIT ( * ) SI_UNIT ( .MILLI., .METRE. ) );
#60026 = EDGE_LOOP ( 'NONE', ( #30646, #1077, #29108, #30001 ) ) ;
#60025 = EDGE_CURVE ( 'NONE', #4230, #4136, #59539, .T. ) ;
#60027 = CARTESIAN_POINT ( 'NONE',  ( 22.50000000000000711, 33.74999999999999289, -3.750000000000000000 ) ) ;
#60028 = DIRECTION ( 'NONE',  ( -0.000000000000000000, 0.000000000000000000, 1.000000000000000000 ) ) ;
#60029 = DIRECTION ( 'NONE',  ( 1.000000000000000000, 0.000000000000000000, 0.000000000000000000 ) ) ;
#60030 = CARTESIAN_POINT ( 'NONE',  ( -31.35611772383057527, -8.500000000000001776, 7.349426879360468234 ) ) ;
#60031 = CIRCLE ( 'NONE', #9500, 0.5000000000000004441 ) ;
#60032 = CARTESIAN_POINT ( 'NONE',  ( -182.7570736234661979, -5.598654528085801552, 7.705886871421367523 ) ) ;
#60033 = SURFACE_STYLE_FILL_AREA ( #38978 ) ;
#60034 =( GEOMETRIC_REPRESENTATION_CONTEXT ( 3 ) GLOBAL_UNCERTAINTY_ASSIGNED_CONTEXT ( ( #17939 ) ) GLOBAL_UNIT_ASSIGNED_CONTEXT ( ( #33564, #46512, #29934 ) ) REPRESENTATION_CONTEXT ( 'NONE', 'WORKASPACE' ) );
#60035 = ADVANCED_FACE ( 'NONE', ( #22616 ), #25235, .T. ) ;
#60036 = DIRECTION ( 'NONE',  ( -1.000000000000000000, 0.000000000000000000, 0.000000000000000000 ) ) ;
#60037 = CIRCLE ( 'NONE', #29718, 0.5000000000000004441 ) ;
#60038 = CARTESIAN_POINT ( 'NONE',  ( -5.015307210679823768, 153.2028691003589245, -6.528277465523972367 ) ) ;
#60039 = ORIENTED_EDGE ( 'NONE', *, *, #53917, .T. ) ;
#60040 = CARTESIAN_POINT ( 'NONE',  ( -161.0929263765340806, 3.094860106623507967, 9.524999999996303757 ) ) ;
#60041 = DIRECTION ( 'NONE',  ( -1.000000000000000000, 0.000000000000000000, 0.000000000000000000 ) ) ;
#60042 = LINE ( 'NONE', #18172, #1891 ) ;
#60043 = CARTESIAN_POINT ( 'NONE',  ( -60.00000000000000000, -2.024042244987997205E-14, -10.00000000000000000 ) ) ;
#60044 = EDGE_LOOP ( 'NONE', ( #22116, #6360, #26686, #63738 ) ) ;
#60045 = CARTESIAN_POINT ( 'NONE',  ( -156.9549999999999841, -7.632228543268599452, 2.479861379858951054 ) ) ;
#60046 = CARTESIAN_POINT ( 'NONE',  ( 28.00000000000000000, 38.70020753820971748, -90.00000000000000000 ) ) ;
#60047 = DIRECTION ( 'NONE',  ( -0.000000000000000000, -0.000000000000000000, -1.000000000000000000 ) ) ;
#60048 = CARTESIAN_POINT ( 'NONE',  ( -177.4449999999999932, 0.000000000000000000, 8.024999999999991473 ) ) ;
#60049 = EDGE_CURVE ( 'NONE', #35530, #22804, #33511, .T. ) ;
#60050 = CARTESIAN_POINT ( 'NONE',  ( -157.9449999999999932, -9.827790563157499189E-16, -8.024999999999991473 ) ) ;
#60051 = ORIENTED_EDGE ( 'NONE', *, *, #4428, .F. ) ;
#60052 = DIRECTION ( 'NONE',  ( -1.000000000000000000, 0.000000000000000000, 0.000000000000000000 ) ) ;
#60053 = AXIS2_PLACEMENT_3D ( 'NONE', #37336, #21806, #26702 ) ;
#60054 = EDGE_CURVE ( 'NONE', #53146, #33110, #54612, .T. ) ;
#60055 = CARTESIAN_POINT ( 'NONE',  ( -195.0000000000000000, 0.000000000000000000, 9.524999999999991473 ) ) ;
#60056 = CARTESIAN_POINT ( 'NONE',  ( -75.20499999999995566, -2.607480562269071545, -8.024999999999991473 ) ) ;
#60057 = CARTESIAN_POINT ( 'NONE',  ( 24.08751298501318772, 24.72230729296544993, 27.25873204504173231 ) ) ;
#60058 = CARTESIAN_POINT ( 'NONE',  ( 71.74137931034479720, 63.10081643261027295, 10.00000000000000000 ) ) ;
#60059 = CARTESIAN_POINT ( 'NONE',  ( -81.89499999999998181, 6.826472737025115478, 4.959722759717899443 ) ) ;
#60060 = CARTESIAN_POINT ( 'NONE',  ( -8.102448949553181734, 141.0049999999999386, -5.886773742842749790 ) ) ;
#60061 = CARTESIAN_POINT ( 'NONE',  ( -134.3070736234661524, -10.01517768586948698, 6.132527647946031529E-16 ) ) ;
#60062 = CIRCLE ( 'NONE', #459, 0.2500000000000002220 ) ;
#60063 = STYLED_ITEM ( 'NONE', ( #47344 ), #62279 ) ;
#60064 = VECTOR ( 'NONE', #3374, 1000.000000000000000 ) ;
#60065 = DIRECTION ( 'NONE',  ( 0.000000000000000000, 0.000000000000000000, 1.000000000000000000 ) ) ;
#60066 = UNCERTAINTY_MEASURE_WITH_UNIT (LENGTH_MEASURE( 1.000000000000000082E-05 ), #42293, 'distance_accuracy_value', 'NONE');
#60067 = DIRECTION ( 'NONE',  ( -1.000000000000000000, -0.000000000000000000, -0.000000000000000000 ) ) ;
#60068 = ORIENTED_EDGE ( 'NONE', *, *, #50271, .T. ) ;
#60069 = CARTESIAN_POINT ( 'NONE',  ( -74.99999999999998579, 50.00000000000000000, 12.00000000000000000 ) ) ;
#60070 = CARTESIAN_POINT ( 'NONE',  ( 4.750000000000002665, 22.24999999999998579, 4.000000000000000000 ) ) ;
#60071 =( GEOMETRIC_REPRESENTATION_CONTEXT ( 3 ) GLOBAL_UNCERTAINTY_ASSIGNED_CONTEXT ( ( #57159 ) ) GLOBAL_UNIT_ASSIGNED_CONTEXT ( ( #57173, #40329, #30421 ) ) REPRESENTATION_CONTEXT ( 'NONE', 'WORKASPACE' ) );
#60072 = VECTOR ( 'NONE', #59557, 1000.000000000000000 ) ;
#60073 = FACE_OUTER_BOUND ( 'NONE', #12658, .T. ) ;
#60074 = COLOUR_RGB ( '', 0.66274510, 0.83137255, 0.94901961) ;
#60075 = CYLINDRICAL_SURFACE ( 'NONE', #29620, 9.524999999999991473 ) ;
#60076 = CARTESIAN_POINT ( 'NONE',  ( 17.75000000000000711, 31.24999999999999289, -4.000000000000000000 ) ) ;
#60077 = VERTEX_POINT ( 'NONE', #44471 ) ;
#60078 = ORIENTED_EDGE ( 'NONE', *, *, #29621, .T. ) ;
#60079 = CARTESIAN_POINT ( 'NONE',  ( 75.00000000000000000, 19.30628705663858113, -6.999999999999999112 ) ) ;
#60080 = EDGE_CURVE ( 'NONE', #20480, #69284, #29333, .T. ) ;
#60081 =( NAMED_UNIT ( * ) SI_UNIT ( $, .STERADIAN. ) SOLID_ANGLE_UNIT ( ) );
#60082 = SURFACE_STYLE_USAGE ( .BOTH. , #44310 ) ;
#60083 = FILL_AREA_STYLE_COLOUR ( '', #6007 ) ;
#60084 = CARTESIAN_POINT ( 'NONE',  ( 6.826472737025119919, 139.8929263765338362, 4.959722759717908325 ) ) ;
#60085 = ORIENTED_EDGE ( 'NONE', *, *, #34391, .F. ) ;
#60086 = CARTESIAN_POINT ( 'NONE',  ( -110.7549999999999955, 4.716976649647091513, -6.492361379858946790 ) ) ;
#60087 = VERTEX_POINT ( 'NONE', #49704 ) ;
#60088 =( NAMED_UNIT ( * ) PLANE_ANGLE_UNIT ( ) SI_UNIT ( $, .RADIAN. ) );
#60089 = CARTESIAN_POINT ( 'NONE',  ( 5.196152422706636465, -9.000000000000005329, 1.392304845413258274 ) ) ;
#60090 = ORIENTED_EDGE ( 'NONE', *, *, #34394, .F. ) ;
#60091 =( NAMED_UNIT ( * ) PLANE_ANGLE_UNIT ( ) SI_UNIT ( $, .RADIAN. ) );
#60092 = ORIENTED_EDGE ( 'NONE', *, *, #20545, .T. ) ;
#60093 = FACE_OUTER_BOUND ( 'NONE', #68582, .T. ) ;
#60094 = CARTESIAN_POINT ( 'NONE',  ( 5.598654528085805993, 159.2450000000000045, 7.705886871421374629 ) ) ;
#60095 = ORIENTED_EDGE ( 'NONE', *, *, #23142, .F. ) ;
#60096 = CIRCLE ( 'NONE', #63477, 4.000000000000000000 ) ;
#60097 = ORIENTED_EDGE ( 'NONE', *, *, #25169, .T. ) ;
#60098 = COLOUR_RGB ( '', 0.08235294, 0.09019608, 0.10196078) ;
#60099 = CARTESIAN_POINT ( 'NONE',  ( -117.0570736234661808, 0.000000000000000000, 9.524999999999991473 ) ) ;
#60100 = CARTESIAN_POINT ( 'NONE',  ( -23.71231517720798010, 117.9999999999999716, -7.000000000000000000 ) ) ;
#60101 = CARTESIAN_POINT ( 'NONE',  ( -9.985360875542991010, -1.514639124457108244, -0.7048476316491002480 ) ) ;
#60102 = ORIENTED_EDGE ( 'NONE', *, *, #58339, .F. ) ;
#60103 = CARTESIAN_POINT ( 'NONE',  ( 7.632228543268607446, 131.0429263765338135, 2.479861379858954606 ) ) ;
#60104 = LINE ( 'NONE', #48914, #37982 ) ;
#60105 = LINE ( 'NONE', #33042, #25369 ) ;
#60106 = EDGE_CURVE ( 'NONE', #42295, #11259, #52962, .T. ) ;
#60107 = CIRCLE ( 'NONE', #54533, 0.5000000000000004441 ) ;
#60108 = CARTESIAN_POINT ( 'NONE',  ( 6.826472737025119919, 124.8929263765338220, 4.959722759717908325 ) ) ;
#60109 = CARTESIAN_POINT ( 'NONE',  ( -75.75000000000000000, -4.000000000000000000, 6.000000000000001776 ) ) ;
#60110 = EDGE_CURVE ( 'NONE', #36029, #57008, #4629, .T. ) ;
#60111 = ORIENTED_EDGE ( 'NONE', *, *, #64247, .F. ) ;
#60112 =( NAMED_UNIT ( * ) PLANE_ANGLE_UNIT ( ) SI_UNIT ( $, .RADIAN. ) );
#60113 = ORIENTED_EDGE ( 'NONE', *, *, #9323, .T. ) ;
#60114 = DIRECTION ( 'NONE',  ( 0.000000000000000000, -0.000000000000000000, 1.000000000000000000 ) ) ;
#60115 = MECHANICAL_DESIGN_GEOMETRIC_PRESENTATION_REPRESENTATION (  '', ( #57877 ), #9585 ) ;
#60116 = CARTESIAN_POINT ( 'NONE',  ( 24.00000000000000000, 1.000000000000000000, 3.000000000000000000 ) ) ;
#60117 = CARTESIAN_POINT ( 'NONE',  ( 1.000000000000000222, 1.224646799147373175E-16, 3.000000000000000000 ) ) ;
#60118 = CARTESIAN_POINT ( 'NONE',  ( -44.99999999999998579, 119.9999999999999716, -7.000000000000000000 ) ) ;
#60119 = STYLED_ITEM ( 'NONE', ( #31214 ), #5139 ) ;
#60120 = CARTESIAN_POINT ( 'NONE',  ( -138.3550000000000182, -4.716976649647093289, -6.492361379858945902 ) ) ;
#60121 = FACE_OUTER_BOUND ( 'NONE', #64669, .T. ) ;
#60122 = DIRECTION ( 'NONE',  ( 0.000000000000000000, 0.000000000000000000, -1.000000000000000000 ) ) ;
#60123 = UNCERTAINTY_MEASURE_WITH_UNIT (LENGTH_MEASURE( 1.000000000000000082E-05 ), #50216, 'distance_accuracy_value', 'NONE');
#60124 = VERTEX_POINT ( 'NONE', #18721 ) ;
#60125 = EDGE_CURVE ( 'NONE', #17419, #10952, #38390, .T. ) ;
#60126 = CARTESIAN_POINT ( 'NONE',  ( -105.5929263765348054, -3.094860106635102692, -9.524999999987880273 ) ) ;
#60127 = CARTESIAN_POINT ( 'NONE',  ( -157.4929263765337737, -8.102448949553174629, 5.886773742842742685 ) ) ;
#60128 = ORIENTED_EDGE ( 'NONE', *, *, #7013, .F. ) ;
#60130 = ADVANCED_FACE ( 'NONE', ( #40199 ), #23997, .T. ) ;
#60129 = EDGE_LOOP ( 'NONE', ( #14117, #41759, #53715, #7365 ) ) ;
#60131 = CARTESIAN_POINT ( 'NONE',  ( -45.15333726543703818, 8.290013047818442615, 3.464655003380054943 ) ) ;
#60132 = CARTESIAN_POINT ( 'NONE',  ( -52.55707362346618083, -1.166476076187852838E-15, -9.524999999999991473 ) ) ;
#60133 = CARTESIAN_POINT ( 'NONE',  ( -55.10499999999998266, -6.826472737025115478, 4.959722759717900331 ) ) ;
#60135 = ORIENTED_EDGE ( 'NONE', *, *, #21022, .F. ) ;
#60134 = CIRCLE ( 'NONE', #26427, 23.00000000000000000 ) ;
#60136 = SURFACE_STYLE_USAGE ( .BOTH. , #17601 ) ;
#60137 = CARTESIAN_POINT ( 'NONE',  ( 25.00000000000001421, 42.00000000000000000, -29.68999999999999417 ) ) ;
#60138 = CARTESIAN_POINT ( 'NONE',  ( -195.0000000000000000, 0.000000000000000000, 0.000000000000000000 ) ) ;
#60139 = AXIS2_PLACEMENT_3D ( 'NONE', #48657, #6041, #47981 ) ;
#60140 = ADVANCED_FACE ( 'NONE', ( #55306 ), #61924, .F. ) ;
#60141 = CARTESIAN_POINT ( 'NONE',  ( 179.4361977533476136, 5.000000000000000000, 103.7004518695250823 ) ) ;
#60142 = CARTESIAN_POINT ( 'NONE',  ( -97.94292637653380496, 0.000000000000000000, 9.524999999999991473 ) ) ;
#60143 = MECHANICAL_DESIGN_GEOMETRIC_PRESENTATION_REPRESENTATION (  '', ( #27526 ), #61284 ) ;
#60144 = VERTEX_POINT ( 'NONE', #29623 ) ;
#60145 = FACE_OUTER_BOUND ( 'NONE', #68081, .T. ) ;
#60146 = COLOUR_RGB ( '', 0.72549020, 0.75294118, 0.79215686) ;
#60147 = ADVANCED_FACE ( 'NONE', ( #19043 ), #7810, .T. ) ;
#60148 = CARTESIAN_POINT ( 'NONE',  ( -48.81081081081080697, 14.09971791521133255, -7.000000000000000000 ) ) ;
#60149 = CARTESIAN_POINT ( 'NONE',  ( 25.00000000000000355, 37.00000000000000000, 4.000000000000000000 ) ) ;
#60150 = CARTESIAN_POINT ( 'NONE',  ( -113.5449999999999875, -7.632228543268600340, -2.479861379858950166 ) ) ;
#60151 = CARTESIAN_POINT ( 'NONE',  ( 9.058813317711337021, 156.5449999999999875, 2.943386871421375783 ) ) ;
#60152 = CARTESIAN_POINT ( 'NONE',  ( -74.69499999999997897, -8.437984349512085203, 5.166775262442717831E-16 ) ) ;
#60153 = DIRECTION ( 'NONE',  ( -1.000000000000000000, 0.000000000000000000, 0.000000000000000000 ) ) ;
#60154 = CARTESIAN_POINT ( 'NONE',  ( -4.716976649647097730, 141.2429263765338305, -6.492361379858953896 ) ) ;
#60155 = DIRECTION ( 'NONE',  ( 0.000000000000000000, 0.000000000000000000, -1.000000000000000000 ) ) ;
#60156 = CARTESIAN_POINT ( 'NONE',  ( 0.000000000000000000, -2.500000000000000000, 0.000000000000000000 ) ) ;
#60157 = UNCERTAINTY_MEASURE_WITH_UNIT (LENGTH_MEASURE( 1.000000000000000082E-05 ), #39117, 'distance_accuracy_value', 'NONE');
#60158 = DIRECTION ( 'NONE',  ( -1.000000000000000000, 0.000000000000000000, 0.000000000000000000 ) ) ;
#60159 = PRESENTATION_LAYER_ASSIGNMENT (  '', '', ( #2825 ) ) ;
#60160 = ORIENTED_EDGE ( 'NONE', *, *, #59551, .T. ) ;
#60161 = CARTESIAN_POINT ( 'NONE',  ( -121.9429263765338050, 0.000000000000000000, 9.524999999999991473 ) ) ;
#60162 = CARTESIAN_POINT ( 'NONE',  ( -151.7949999999999591, 2.607480562269068880, -8.024999999999993250 ) ) ;
#60163 = AXIS2_PLACEMENT_3D ( 'NONE', #1312, #6627, #55533 ) ;
#60164 = CARTESIAN_POINT ( 'NONE',  ( -47.54499999999997328, -7.632228543268600340, -2.479861379858950166 ) ) ;
#60165 = CIRCLE ( 'NONE', #19746, 0.5000000000000004441 ) ;
#60166 = VERTEX_POINT ( 'NONE', #66568 ) ;
#60167 = ORIENTED_EDGE ( 'NONE', *, *, #5019, .F. ) ;
#60168 = COLOUR_RGB ( '', 0.31764706, 0.68627451, 0.89019608) ;
#60169 = CARTESIAN_POINT ( 'NONE',  ( 66.74999999999998579, 0.000000000000000000, 4.000000000000000000 ) ) ;
#60170 = EDGE_CURVE ( 'NONE', #66608, #43138, #51428, .T. ) ;
#60171 = CARTESIAN_POINT ( 'NONE',  ( 4.041451884327379673, -7.000000000000002665, 7.500000000000000000 ) ) ;
#60172 = CARTESIAN_POINT ( 'NONE',  ( -130.8570736234661922, -5.598654528085803328, -7.705886871421366635 ) ) ;
#60173 = CARTESIAN_POINT ( 'NONE',  ( -71.99999999999998579, 119.9999999999997868, 7.500000000000000000 ) ) ;
#60174 = CARTESIAN_POINT ( 'NONE',  ( 44.25000000000000000, 21.99999999999998579, -3.750000000000000000 ) ) ;
#60175 = ORIENTED_EDGE ( 'NONE', *, *, #19717, .F. ) ;
#60176 = CARTESIAN_POINT ( 'NONE',  ( -145.8549999999999898, 4.716976649647094177, 6.492361379858945902 ) ) ;
#60177 = EDGE_LOOP ( 'NONE', ( #50656, #56367, #54779, #61790 ) ) ;
#60178 = AXIS2_PLACEMENT_3D ( 'NONE', #14082, #62257, #13724 ) ;
#60179 = EDGE_LOOP ( 'NONE', ( #22930, #55541, #56551, #44921, #17374, #43875, #5589, #48265, #38525, #8795, #69207, #57234, #50240, #3697, #50326, #10652 ) ) ;
#60180 = DIRECTION ( 'NONE',  ( 0.000000000000000000, 0.000000000000000000, 1.000000000000000000 ) ) ;
#60181 = DIRECTION ( 'NONE',  ( 0.000000000000000000, 1.000000000000000000, -0.000000000000000000 ) ) ;
#60182 = VERTEX_POINT ( 'NONE', #40908 ) ;
#60183 =( GEOMETRIC_REPRESENTATION_CONTEXT ( 3 ) GLOBAL_UNCERTAINTY_ASSIGNED_CONTEXT ( ( #8773 ) ) GLOBAL_UNIT_ASSIGNED_CONTEXT ( ( #41209, #19354, #51738 ) ) REPRESENTATION_CONTEXT ( 'NONE', 'WORKASPACE' ) );
#60184 = COLOUR_RGB ( '', 0.66274510, 0.83137255, 0.94901961) ;
#60185 = CARTESIAN_POINT ( 'NONE',  ( -3.542344102440325049, 1.863645424029197750, -9.000000000000007105 ) ) ;
#60186 = DIRECTION ( 'NONE',  ( 1.000000000000000000, 0.000000000000000000, 0.000000000000000000 ) ) ;
#60187 = CARTESIAN_POINT ( 'NONE',  ( -10.01517768586949231, 131.1949999999999363, -6.132527647946036459E-16 ) ) ;
#60188 = MECHANICAL_DESIGN_GEOMETRIC_PRESENTATION_REPRESENTATION (  '', ( #63549 ), #27621 ) ;
#60189 = ORIENTED_EDGE ( 'NONE', *, *, #30594, .F. ) ;
#60190 = ADVANCED_FACE ( 'NONE', ( #33843 ), #13613, .T. ) ;
#60191 = FILL_AREA_STYLE_COLOUR ( '', #69009 ) ;
#60192 = CARTESIAN_POINT ( 'NONE',  ( -1.166476076187854022E-15, 133.0549999999999784, 9.525000000000000355 ) ) ;
#60193 = CARTESIAN_POINT ( 'NONE',  ( -51.80499999999997840, -8.437984349512086979, 5.166775262442717831E-16 ) ) ;
#60194 = AXIS2_PLACEMENT_3D ( 'NONE', #48700, #22615, #55998 ) ;
#60195 = CYLINDRICAL_SURFACE ( 'NONE', #41971, 0.2500000000000002220 ) ;
#60196 = VERTEX_POINT ( 'NONE', #3174 ) ;
#60197 = CARTESIAN_POINT ( 'NONE',  ( 3.094860106618431583, 154.2049999999999272, 9.525000000000000355 ) ) ;
#60198 = DIRECTION ( 'NONE',  ( 1.000000000000000000, -1.776356839400250465E-15, 0.000000000000000000 ) ) ;
#60199 = UNCERTAINTY_MEASURE_WITH_UNIT (LENGTH_MEASURE( 1.000000000000000082E-05 ), #57140, 'distance_accuracy_value', 'NONE');
#60200 = CARTESIAN_POINT ( 'NONE',  ( -74.99999999999998579, 50.00000000000000000, -10.49999999999999822 ) ) ;
#60201 = EDGE_CURVE ( 'NONE', #45776, #32941, #15224, .T. ) ;
#60202 = DIRECTION ( 'NONE',  ( 0.000000000000000000, 0.000000000000000000, -1.000000000000000000 ) ) ;
#60203 =( NAMED_UNIT ( * ) PLANE_ANGLE_UNIT ( ) SI_UNIT ( $, .RADIAN. ) );
#60204 = EDGE_CURVE ( 'NONE', #7911, #30495, #39516, .T. ) ;
#60205 = ORIENTED_EDGE ( 'NONE', *, *, #61057, .T. ) ;
#60206 = CARTESIAN_POINT ( 'NONE',  ( -71.50000000000000000, 14.49137674618942562, -9.500000000000000000 ) ) ;
#60207 = ORIENTED_EDGE ( 'NONE', *, *, #49975, .F. ) ;
#60208 = DIRECTION ( 'NONE',  ( -1.000000000000000000, -0.000000000000000000, -0.000000000000000000 ) ) ;
#60209 = CARTESIAN_POINT ( 'NONE',  ( -168.2050000000000125, -2.607480562269071545, -8.024999999999991473 ) ) ;
#60210 = ORIENTED_EDGE ( 'NONE', *, *, #19773, .T. ) ;
#60211 = DIRECTION ( 'NONE',  ( -0.000000000000000000, -1.000000000000000000, -0.000000000000000000 ) ) ;
#60212 = UNCERTAINTY_MEASURE_WITH_UNIT (LENGTH_MEASURE( 1.000000000000000082E-05 ), #63756, 'distance_accuracy_value', 'NONE');
#60213 = STYLED_ITEM ( 'NONE', ( #49771 ), #8754 ) ;
#60214 = SURFACE_STYLE_USAGE ( .BOTH. , #21539 ) ;
#60215 = EDGE_CURVE ( 'NONE', #28936, #36029, #19225, .T. ) ;
#60216 =( LENGTH_UNIT ( ) NAMED_UNIT ( * ) SI_UNIT ( .MILLI., .METRE. ) );
#60217 = CARTESIAN_POINT ( 'NONE',  ( -77.69292637653380496, 10.01517768586948698, -1.839758294383808966E-15 ) ) ;
#60218 = ORIENTED_EDGE ( 'NONE', *, *, #44010, .F. ) ;
#60219 = EDGE_CURVE ( 'NONE', #52535, #50964, #58108, .T. ) ;
#60220 = AXIS2_PLACEMENT_3D ( 'NONE', #30506, #2714, #66791 ) ;
#60221 = CARTESIAN_POINT ( 'NONE',  ( 33.00000000000002132, 15.00000000000000000, 79.00402776293826435 ) ) ;
#60222 = CARTESIAN_POINT ( 'NONE',  ( -81.35499999999998977, -4.716976649647093289, -6.492361379858945902 ) ) ;
#60223 = ORIENTED_EDGE ( 'NONE', *, *, #54189, .T. ) ;
#60224 = VECTOR ( 'NONE', #14886, 1000.000000000000000 ) ;
#60225 = AXIS2_PLACEMENT_3D ( 'NONE', #49221, #43977, #22479 ) ;
#60226 = COLOUR_RGB ( '', 0.40784314, 0.44705882, 0.49803922) ;
#60227 = DIRECTION ( 'NONE',  ( -1.000000000000000000, 0.000000000000000000, 0.000000000000000000 ) ) ;
#60228 = DIRECTION ( 'NONE',  ( 0.000000000000000000, 0.000000000000000000, 1.000000000000000000 ) ) ;
#60229 = CARTESIAN_POINT ( 'NONE',  ( -55.55707362346618083, -1.166476076187852838E-15, -9.524999999999991473 ) ) ;
#60230 = DIRECTION ( 'NONE',  ( 0.000000000000000000, 0.000000000000000000, 1.000000000000000000 ) ) ;
#60231 = ORIENTED_EDGE ( 'NONE', *, *, #3521, .F. ) ;
#60232 = FACE_OUTER_BOUND ( 'NONE', #48809, .T. ) ;
#60234 = DIRECTION ( 'NONE',  ( 0.000000000000000000, 1.000000000000000000, -0.000000000000000000 ) ) ;
#60233 = FILL_AREA_STYLE_COLOUR ( '', #57130 ) ;
#60235 = CIRCLE ( 'NONE', #44564, 1.000000000000000888 ) ;
#60236 = EDGE_CURVE ( 'NONE', #17125, #42263, #67564, .T. ) ;
#60237 = CARTESIAN_POINT ( 'NONE',  ( 3.094860106618435136, 133.2950000000000159, -9.525000000000000355 ) ) ;
#60238 = CARTESIAN_POINT ( 'NONE',  ( -110.5449999999999875, -7.632228543268600340, -2.479861379858950166 ) ) ;
#60239 = STYLED_ITEM ( 'NONE', ( #20135 ), #1547 ) ;
#60240 = FILL_AREA_STYLE ('',( #12730 ) ) ;
#60241 = EDGE_CURVE ( 'NONE', #37066, #44394, #67995, .T. ) ;
#60242 = PRESENTATION_LAYER_ASSIGNMENT (  '', '', ( #47952 ) ) ;
#60244 = CARTESIAN_POINT ( 'NONE',  ( -16.31125505495063166, 10.98243589408808951, -4.836450918052216608 ) ) ;
#60243 = CARTESIAN_POINT ( 'NONE',  ( -32.56443198605083467, -8.762778093182605588, -2.500000000007038370 ) ) ;
#60245 = CARTESIAN_POINT ( 'NONE',  ( -153.8929263765338362, -8.102448949553172852, -5.886773742842741797 ) ) ;
#60246 =( LENGTH_UNIT ( ) NAMED_UNIT ( * ) SI_UNIT ( .MILLI., .METRE. ) );
#60247 = CARTESIAN_POINT ( 'NONE',  ( -178.1949999999999648, 8.437984349512085203, -1.550032578732815448E-15 ) ) ;
#60248 = CARTESIAN_POINT ( 'NONE',  ( 30.50000000000001066, 15.99999999999997691, 3.750000000000000000 ) ) ;
#60249 = CARTESIAN_POINT ( 'NONE',  ( -45.19495320693604157, -13.94006660658549634, 0.7849218814955336576 ) ) ;
#60250 = DIRECTION ( 'NONE',  ( -0.000000000000000000, -0.000000000000000000, 1.000000000000000000 ) ) ;
#60251 = ORIENTED_EDGE ( 'NONE', *, *, #49300, .T. ) ;
#60252 = CARTESIAN_POINT ( 'NONE',  ( -67.49292637653380211, -8.102448949553172852, 5.886773742842742685 ) ) ;
#60253 = CARTESIAN_POINT ( 'NONE',  ( 1.000000000000000888, 14.00000000000000000, -60.00402776293827145 ) ) ;
#60254 = DIRECTION ( 'NONE',  ( -0.000000000000000000, -0.000000000000000000, -1.000000000000000000 ) ) ;
#60255 = CARTESIAN_POINT ( 'NONE',  ( 21.75000000000001066, 21.99999999999998224, 3.750000000000000000 ) ) ;
#60256 = CARTESIAN_POINT ( 'NONE',  ( -79.79292637653379927, -3.094860106618429807, 9.524999999999991473 ) ) ;
#60257 = AXIS2_PLACEMENT_3D ( 'NONE', #46324, #35737, #35033 ) ;
#60258 = EDGE_LOOP ( 'NONE', ( #56189, #46110, #60515, #26339 ) ) ;
#60259 = CARTESIAN_POINT ( 'NONE',  ( -173.6049999999999898, 6.826472737025113702, -4.959722759717902107 ) ) ;
#60260 = AXIS2_PLACEMENT_3D ( 'NONE', #43550, #54385, #37588 ) ;
#60261 = EDGE_LOOP ( 'NONE', ( #10801, #24035, #10449, #11433 ) ) ;
#60262 = CARTESIAN_POINT ( 'NONE',  ( -112.3429263765337964, -9.058813317711329915, 2.943386871421371787 ) ) ;
#60264 = EDGE_CURVE ( 'NONE', #21109, #58564, #6891, .T. ) ;
#60263 = SURFACE_STYLE_USAGE ( .BOTH. , #66586 ) ;
#60265 = DIRECTION ( 'NONE',  ( -1.000000000000000000, 0.000000000000000000, 6.938893903907222067E-15 ) ) ;
#60266 = DIRECTION ( 'NONE',  ( 1.000000000000000000, 0.000000000000000000, 0.000000000000000000 ) ) ;
#60267 = FILL_AREA_STYLE_COLOUR ( '', #19667 ) ;
#60268 = CARTESIAN_POINT ( 'NONE',  ( 7.632228543268608334, 150.4570736234661581, -2.479861379858951942 ) ) ;
#60269 = ORIENTED_EDGE ( 'NONE', *, *, #31007, .F. ) ;
#60270 = ADVANCED_FACE ( 'NONE', ( #30645 ), #50698, .T. ) ;
#60271 = PLANE ( 'NONE',  #48484 ) ;
#60272 = CARTESIAN_POINT ( 'NONE',  ( -86.75499999999998124, 4.716976649647091513, -6.492361379858946790 ) ) ;
#60273 = UNCERTAINTY_MEASURE_WITH_UNIT (LENGTH_MEASURE( 1.000000000000000082E-05 ), #2943, 'distance_accuracy_value', 'NONE');
#60274 = DIRECTION ( 'NONE',  ( 4.625929269271505635E-16, 0.000000000000000000, -1.000000000000000000 ) ) ;
#60275 =( GEOMETRIC_REPRESENTATION_CONTEXT ( 3 ) GLOBAL_UNCERTAINTY_ASSIGNED_CONTEXT ( ( #57339 ) ) GLOBAL_UNIT_ASSIGNED_CONTEXT ( ( #21327, #4812, #16101 ) ) REPRESENTATION_CONTEXT ( 'NONE', 'WORKASPACE' ) );
#60276 = EDGE_CURVE ( 'NONE', #61571, #41886, #64187, .T. ) ;
#60277 = FILL_AREA_STYLE ('',( #65552 ) ) ;
#60278 = CARTESIAN_POINT ( 'NONE',  ( -28.74999999999999645, -4.000000000000000000, 18.10000000000000497 ) ) ;
#60279 = DIRECTION ( 'NONE',  ( -1.000000000000000000, 0.000000000000000000, 0.000000000000000000 ) ) ;
#60280 = ORIENTED_EDGE ( 'NONE', *, *, #64385, .T. ) ;
#60281 = CARTESIAN_POINT ( 'NONE',  ( -141.0570736234661808, 0.000000000000000000, 9.524999999999991473 ) ) ;
#60282 = CARTESIAN_POINT ( 'NONE',  ( -66.29500000000000171, -2.607480562269069768, 8.024999999999991473 ) ) ;
#60283 = ORIENTED_EDGE ( 'NONE', *, *, #2090, .F. ) ;
#60284 = DIRECTION ( 'NONE',  ( 0.000000000000000000, 0.000000000000000000, -1.000000000000000000 ) ) ;
#60285 =( GEOMETRIC_REPRESENTATION_CONTEXT ( 3 ) GLOBAL_UNCERTAINTY_ASSIGNED_CONTEXT ( ( #44585 ) ) GLOBAL_UNIT_ASSIGNED_CONTEXT ( ( #41801, #10456, #42497 ) ) REPRESENTATION_CONTEXT ( 'NONE', 'WORKASPACE' ) );
#60286 = CARTESIAN_POINT ( 'NONE',  ( -49.19292637653380496, -10.01517768586948698, 6.132527647946031529E-16 ) ) ;
#60287 = CARTESIAN_POINT ( 'NONE',  ( -45.78667142738931517, 8.935426707107499311, -6.369485321263473665 ) ) ;
#60288 = ORIENTED_EDGE ( 'NONE', *, *, #26385, .T. ) ;
#60289 =( LENGTH_UNIT ( ) NAMED_UNIT ( * ) SI_UNIT ( .MILLI., .METRE. ) );
#60290 = DIRECTION ( 'NONE',  ( -0.7071067811865352493, 8.659560562354781249E-17, 0.7071067811865597852 ) ) ;
#60291 = VERTEX_POINT ( 'NONE', #35608 ) ;
#60292 = ADVANCED_FACE ( 'NONE', ( #41255 ), #51787, .F. ) ;
#60293 = CARTESIAN_POINT ( 'NONE',  ( -74.12609030924235753, 9.272074904602392920, 6.224541297626261738 ) ) ;
#60294 = CARTESIAN_POINT ( 'NONE',  ( -110.7549999999999955, 4.716976649647091513, -6.492361379858946790 ) ) ;
#60295 = EDGE_LOOP ( 'NONE', ( #6702, #59775, #68366 ) ) ;
#60296 = CARTESIAN_POINT ( 'NONE',  ( 54.99999999999999289, 2.409368300552961372E-15, -7.000000000000017764 ) ) ;
#60297 = DIRECTION ( 'NONE',  ( 0.000000000000000000, 0.000000000000000000, -1.000000000000000000 ) ) ;
#60298 = DIRECTION ( 'NONE',  ( 1.000000000000000000, 0.000000000000000000, 0.000000000000000000 ) ) ;
#60299 = CARTESIAN_POINT ( 'NONE',  ( -148.4070736234661751, 3.094860106618428031, -9.524999999999993250 ) ) ;
#60300 = CARTESIAN_POINT ( 'NONE',  ( -8.102448949553179958, 133.8949999999999818, -5.886773742842749790 ) ) ;
#60301 = CARTESIAN_POINT ( 'NONE',  ( -83.00707362346614104, -8.102448949553172852, -5.886773742842741797 ) ) ;
#60302 = CARTESIAN_POINT ( 'NONE',  ( -53.80170265663038265, -9.571662231010620303, -3.215428675398786407 ) ) ;
#60303 = VERTEX_POINT ( 'NONE', #35953 ) ;
#60304 = LINE ( 'NONE', #55378, #4343 ) ;
#60306 = FILL_AREA_STYLE_COLOUR ( '', #34390 ) ;
#60305 = CIRCLE ( 'NONE', #21046, 1.000000000000000000 ) ;
#60307 = CARTESIAN_POINT ( 'NONE',  ( -127.8549999999999898, 4.716976649647094177, 6.492361379858945902 ) ) ;
#60308 = DIRECTION ( 'NONE',  ( 1.000000000000000000, 0.000000000000000000, 0.000000000000000000 ) ) ;
#60309 = VECTOR ( 'NONE', #17668, 1000.000000000000000 ) ;
#60310 = CARTESIAN_POINT ( 'NONE',  ( 16.75000000000000711, 27.99999999999998224, 3.750000000000000000 ) ) ;
#60311 = CARTESIAN_POINT ( 'NONE',  ( 35.99999999999999289, 5.000000000000000000, -29.00402776293825724 ) ) ;
#60312 = CARTESIAN_POINT ( 'NONE',  ( -142.0449999999999875, 7.632228543268600340, 2.479861379858949277 ) ) ;
#60313 = PRESENTATION_LAYER_ASSIGNMENT (  '', '', ( #56956 ) ) ;
#60314 = CARTESIAN_POINT ( 'NONE',  ( -130.7949999999999875, 2.607480562269069324, -8.024999999999993250 ) ) ;
#60315 = ORIENTED_EDGE ( 'NONE', *, *, #46929, .T. ) ;
#60316 = FACE_OUTER_BOUND ( 'NONE', #22989, .T. ) ;
#60317 = CYLINDRICAL_SURFACE ( 'NONE', #53857, 0.2500000000000002220 ) ;
#60318 = DIRECTION ( 'NONE',  ( 0.000000000000000000, 1.000000000000000000, 0.000000000000000000 ) ) ;
#60319 = CARTESIAN_POINT ( 'NONE',  ( -181.7929263765337566, -3.094860106618429807, 9.524999999999991473 ) ) ;
#60320 = CARTESIAN_POINT ( 'NONE',  ( -54.14499999999999602, -4.716976649647092401, 6.492361379858946790 ) ) ;
#60321 = CIRCLE ( 'NONE', #23281, 17.00000000000000000 ) ;
#60322 = CARTESIAN_POINT ( 'NONE',  ( -22.75000000000000711, 36.75000000000000000, 3.750000000000000000 ) ) ;
#60323 =( NAMED_UNIT ( * ) SI_UNIT ( $, .STERADIAN. ) SOLID_ANGLE_UNIT ( ) );
#60324 = SURFACE_STYLE_FILL_AREA ( #33935 ) ;
#60325 = CARTESIAN_POINT ( 'NONE',  ( -75.05707362346616662, 0.000000000000000000, 9.524999999999991473 ) ) ;
#60326 = CARTESIAN_POINT ( 'NONE',  ( -92.39292637653379359, 8.102448949553176405, 5.886773742842740909 ) ) ;
#60327 =( NAMED_UNIT ( * ) SI_UNIT ( $, .STERADIAN. ) SOLID_ANGLE_UNIT ( ) );
#60328 = FACE_OUTER_BOUND ( 'NONE', #68982, .T. ) ;
#60329 = CARTESIAN_POINT ( 'NONE',  ( -195.0000000000000000, 0.000000000000000000, 0.000000000000000000 ) ) ;
#60330 = FILL_AREA_STYLE_COLOUR ( '', #55049 ) ;
#60331 = CARTESIAN_POINT ( 'NONE',  ( -41.47640344042682869, 107.6239624391513559, 3.580003982102259119 ) ) ;
#60332 =( NAMED_UNIT ( * ) PLANE_ANGLE_UNIT ( ) SI_UNIT ( $, .RADIAN. ) );
#60333 = ORIENTED_EDGE ( 'NONE', *, *, #1631, .F. ) ;
#60334 = CARTESIAN_POINT ( 'NONE',  ( 20.00000000000001776, 15.00000000000000000, -29.68999999999999417 ) ) ;
#60335 = EDGE_CURVE ( 'NONE', #16364, #17287, #10604, .T. ) ;
#60336 = DIRECTION ( 'NONE',  ( -1.000000000000000000, 0.000000000000000000, 0.000000000000000000 ) ) ;
#60337 = ORIENTED_EDGE ( 'NONE', *, *, #66986, .T. ) ;
#60338 = CARTESIAN_POINT ( 'NONE',  ( 0.000000000000000000, 87.30187232391182306, 8.025000000000000355 ) ) ;
#60339 = CARTESIAN_POINT ( 'NONE',  ( -6.826472737025120807, 124.5070736234661553, -4.959722759717907437 ) ) ;
#60340 = LINE ( 'NONE', #37911, #47492 ) ;
#60341 = LINE ( 'NONE', #33615, #46568 ) ;
#60342 = ORIENTED_EDGE ( 'NONE', *, *, #5911, .F. ) ;
#60343 = CIRCLE ( 'NONE', #44693, 14.49999999999999822 ) ;
#60344 = CARTESIAN_POINT ( 'NONE',  ( 57.00000000000000000, 14.00000000000000000, 72.50402776293826435 ) ) ;
#60345 = ADVANCED_FACE ( 'NONE', ( #28118 ), #32052, .T. ) ;
#60346 = VERTEX_POINT ( 'NONE', #54535 ) ;
#60347 = FACE_OUTER_BOUND ( 'NONE', #27661, .T. ) ;
#60348 = COLOUR_RGB ( '', 0.66274510, 0.83137255, 0.94901961) ;
#60349 = CARTESIAN_POINT ( 'NONE',  ( -93.80707362346615241, 10.01517768586948698, -1.839758294383808966E-15 ) ) ;
#60350 = EDGE_CURVE ( 'NONE', #50251, #58449, #69680, .T. ) ;
#60351 = ADVANCED_FACE ( 'NONE', ( #49626 ), #33097, .T. ) ;
#60352 = CARTESIAN_POINT ( 'NONE',  ( 8.437984349512095861, 149.1929263765337907, 1.550032578732816828E-15 ) ) ;
#60353 = CARTESIAN_POINT ( 'NONE',  ( -92.54499999999998749, -7.632228543268600340, -2.479861379858950166 ) ) ;
#60354 = EDGE_LOOP ( 'NONE', ( #63992, #9155, #22465, #35576 ) ) ;
#60355 = SHAPE_REPRESENTATION ( '14. Nut M6', ( #42840 ), #1086 ) ;
#60356 = DIRECTION ( 'NONE',  ( -0.000000000000000000, -1.000000000000000000, -0.000000000000000000 ) ) ;
#60357 = EDGE_CURVE ( 'NONE', #42918, #23561, #5999, .T. ) ;
#60358 = PRESENTATION_STYLE_ASSIGNMENT (( #38957 ) ) ;
#60359 = ORIENTED_EDGE ( 'NONE', *, *, #45789, .F. ) ;
#60360 = CARTESIAN_POINT ( 'NONE',  ( 0.000000000000000000, 2.500000000000000000, 0.000000000000000000 ) ) ;
#60361 = DIRECTION ( 'NONE',  ( -0.000000000000000000, -0.000000000000000000, -1.000000000000000000 ) ) ;
#60362 = AXIS2_PLACEMENT_3D ( 'NONE', #16417, #63858, #68458 ) ;
#60364 = EDGE_CURVE ( 'NONE', #38885, #37037, #49279, .T. ) ;
#60363 = CIRCLE ( 'NONE', #32297, 0.2500000000000002220 ) ;
#60365 =( NAMED_UNIT ( * ) SI_UNIT ( $, .STERADIAN. ) SOLID_ANGLE_UNIT ( ) );
#60366 = VERTEX_POINT ( 'NONE', #27089 ) ;
#60367 = ORIENTED_EDGE ( 'NONE', *, *, #46021, .F. ) ;
#60368 = CARTESIAN_POINT ( 'NONE',  ( -4.250000000000001776, 21.74999999999998579, 3.750000000000000000 ) ) ;
#60369 = FILL_AREA_STYLE_COLOUR ( '', #51508 ) ;
#60370 = CARTESIAN_POINT ( 'NONE',  ( -72.00000000000000000, 36.32520566882265456, 7.000000000000000000 ) ) ;
#60371 = SPHERICAL_SURFACE ( 'NONE', #14182, 0.2500000000000000000 ) ;
#60372 = CARTESIAN_POINT ( 'NONE',  ( -179.0070736234661410, -8.102448949553172852, -5.886773742842741797 ) ) ;
#60373 = CARTESIAN_POINT ( 'NONE',  ( 16.00000000000001776, 15.00000000000000000, -34.68999999999999773 ) ) ;
#60374 = CARTESIAN_POINT ( 'NONE',  ( -84.35707362346617799, 5.598654528085804216, 7.705886871421366635 ) ) ;
#60375 = ORIENTED_EDGE ( 'NONE', *, *, #21871, .T. ) ;
#60376 = CARTESIAN_POINT ( 'NONE',  ( -48.20707362346615099, 3.094860106618433360, 9.524999999999991473 ) ) ;
#60377 =( LENGTH_UNIT ( ) NAMED_UNIT ( * ) SI_UNIT ( .MILLI., .METRE. ) );
#60378 = CARTESIAN_POINT ( 'NONE',  ( 0.9999999999999991118, 50.00000000000000000, -60.00000000000000000 ) ) ;
#60379 = VERTEX_POINT ( 'NONE', #48967 ) ;
#60380 = CARTESIAN_POINT ( 'NONE',  ( -158.9050000000000011, 2.607480562269068880, -8.024999999999993250 ) ) ;
#60381 = FACE_OUTER_BOUND ( 'NONE', #11989, .T. ) ;
#60382 = CARTESIAN_POINT ( 'NONE',  ( -183.8192599248787076, -8.214053869287363696, -2.901243250066394719 ) ) ;
#60383 = CARTESIAN_POINT ( 'NONE',  ( -171.4449999999999932, 0.000000000000000000, 8.024999999999991473 ) ) ;
#60384 = CARTESIAN_POINT ( 'NONE',  ( -156.2949999999999591, -2.607480562269069768, 8.024999999999991473 ) ) ;
#60385 = ORIENTED_EDGE ( 'NONE', *, *, #56882, .T. ) ;
#60386 = CYLINDRICAL_SURFACE ( 'NONE', #58283, 9.524999999999991473 ) ;
#60387 = SURFACE_SIDE_STYLE ('',( #38654 ) ) ;
#60388 = CIRCLE ( 'NONE', #69404, 0.5000000000000004441 ) ;
#60389 = DIRECTION ( 'NONE',  ( -0.000000000000000000, 0.000000000000000000, -1.000000000000000000 ) ) ;
#60390 = CARTESIAN_POINT ( 'NONE',  ( -76.70499999999999829, 2.607480562269073321, 8.024999999999991473 ) ) ;
#60391 = CARTESIAN_POINT ( 'NONE',  ( -37.45648088167604328, -10.91878729800595238, 3.716390883267106648 ) ) ;
#60392 =( GEOMETRIC_REPRESENTATION_CONTEXT ( 3 ) GLOBAL_UNCERTAINTY_ASSIGNED_CONTEXT ( ( #40544 ) ) GLOBAL_UNIT_ASSIGNED_CONTEXT ( ( #55353, #21977, #38179 ) ) REPRESENTATION_CONTEXT ( 'NONE', 'WORKASPACE' ) );
#60393 = VECTOR ( 'NONE', #35824, 1000.000000000000000 ) ;
#60394 = CARTESIAN_POINT ( 'NONE',  ( -71.54499999999998749, -7.632228543268600340, -2.479861379858950166 ) ) ;
#60395 = CARTESIAN_POINT ( 'NONE',  ( -3.094860106618432471, 143.7050000000000125, -9.525000000000000355 ) ) ;
#60396 = DIRECTION ( 'NONE',  ( -1.000000000000000000, 0.000000000000000000, 0.000000000000000000 ) ) ;
#60397 = VECTOR ( 'NONE', #49450, 1000.000000000000000 ) ;
#60398 = PRESENTATION_STYLE_ASSIGNMENT (( #1942 ) ) ;
#60399 = CARTESIAN_POINT ( 'NONE',  ( 0.9999999999999991118, 50.00000000000000000, 60.00000000000000000 ) ) ;
#60400 = DIRECTION ( 'NONE',  ( 0.000000000000000000, 0.000000000000000000, 1.000000000000000000 ) ) ;
#60401 = ORIENTED_EDGE ( 'NONE', *, *, #65266, .T. ) ;
#60402 = DIRECTION ( 'NONE',  ( 0.000000000000000000, -0.000000000000000000, -1.000000000000000000 ) ) ;
#60403 = AXIS2_PLACEMENT_3D ( 'NONE', #41677, #69417, #42388 ) ;
#60404 =( GEOMETRIC_REPRESENTATION_CONTEXT ( 3 ) GLOBAL_UNCERTAINTY_ASSIGNED_CONTEXT ( ( #62952 ) ) GLOBAL_UNIT_ASSIGNED_CONTEXT ( ( #31119, #14621, #9353 ) ) REPRESENTATION_CONTEXT ( 'NONE', 'WORKASPACE' ) );
#60405 = CARTESIAN_POINT ( 'NONE',  ( -87.50000000000000000, -8.499999999999989342, 3.000000000000000000 ) ) ;
#60406 = EDGE_CURVE ( 'NONE', #65961, #58823, #22189, .T. ) ;
#60407 = CARTESIAN_POINT ( 'NONE',  ( -8.082903768654762899, 3.463586619550771876E-15, 1.082903768654759125 ) ) ;
#60408 = VERTEX_POINT ( 'NONE', #48623 ) ;
#60409 = ORIENTED_EDGE ( 'NONE', *, *, #15964, .F. ) ;
#60410 = ADVANCED_FACE ( 'NONE', ( #32373 ), #16595, .F. ) ;
#60411 = CARTESIAN_POINT ( 'NONE',  ( 17.15973193263811680, -3.000000000000000000, 12.50000000000000000 ) ) ;
#60412 =( LENGTH_UNIT ( ) NAMED_UNIT ( * ) SI_UNIT ( .MILLI., .METRE. ) );
#60413 = FACE_OUTER_BOUND ( 'NONE', #33572, .T. ) ;
#60414 = ADVANCED_FACE ( 'NONE', ( #13011 ), #35165, .F. ) ;
#60415 =( LENGTH_UNIT ( ) NAMED_UNIT ( * ) SI_UNIT ( .MILLI., .METRE. ) );
#60416 = VERTEX_POINT ( 'NONE', #17630 ) ;
#60417 = CARTESIAN_POINT ( 'NONE',  ( -114.5049999999999955, -6.826472737025113702, -4.959722759717900331 ) ) ;
#60418 = VERTEX_POINT ( 'NONE', #66487 ) ;
#60419 = DIRECTION ( 'NONE',  ( 1.000000000000000000, -0.000000000000000000, 0.000000000000000000 ) ) ;
#60420 = CARTESIAN_POINT ( 'NONE',  ( 5.603096392576913054, -8.295152368350905192, 0.9853608755428857613 ) ) ;
#60421 = EDGE_LOOP ( 'NONE', ( #45160, #23746, #26710, #3304 ) ) ;
#60422 = CARTESIAN_POINT ( 'NONE',  ( -56.84292637653378932, 9.058813317711329915, -2.943386871421373119 ) ) ;
#60423 = CARTESIAN_POINT ( 'NONE',  ( 31.00000000000001421, 14.00000000000000000, 34.49999999999998579 ) ) ;
#60424 = ORIENTED_EDGE ( 'NONE', *, *, #3028, .T. ) ;
#60425 = EDGE_CURVE ( 'NONE', #57659, #49213, #18051, .T. ) ;
#60426 = DIRECTION ( 'NONE',  ( -0.000000000000000000, -0.000000000000000000, -1.000000000000000000 ) ) ;
#60427 = SURFACE_SIDE_STYLE ('',( #64697 ) ) ;
#60428 = DIRECTION ( 'NONE',  ( 0.8660254037844388186, 0.4999999999999998335, -0.000000000000000000 ) ) ;
#60429 = ORIENTED_EDGE ( 'NONE', *, *, #42548, .F. ) ;
#60430 = VERTEX_POINT ( 'NONE', #61202 ) ;
#60431 =( NAMED_UNIT ( * ) PLANE_ANGLE_UNIT ( ) SI_UNIT ( $, .RADIAN. ) );
#60432 = CARTESIAN_POINT ( 'NONE',  ( -152.0070736234661695, -8.102448949553174629, -5.886773742842741797 ) ) ;
#60433 = ADVANCED_FACE ( 'NONE', ( #66122 ), #11415, .T. ) ;
#60434 = SURFACE_SIDE_STYLE ('',( #18591 ) ) ;
#60435 = VERTEX_POINT ( 'NONE', #34122 ) ;
#60436 = CARTESIAN_POINT ( 'NONE',  ( -6.826472737025120807, 138.9929263765338305, 4.959722759717906548 ) ) ;
#60437 = CARTESIAN_POINT ( 'NONE',  ( -195.0000000000000000, 0.000000000000000000, 0.000000000000000000 ) ) ;
#60438 = PRESENTATION_LAYER_ASSIGNMENT (  '', '', ( #28996 ) ) ;
#60439 = AXIS2_PLACEMENT_3D ( 'NONE', #52633, #15364, #26876 ) ;
#60440 = B_SPLINE_CURVE_WITH_KNOTS ( 'NONE', 3,
 ( #34527, #65149, #7113, #22602, #28180, #28889, #65504, #55983 ),
 .UNSPECIFIED., .F., .F.,
 ( 4, 2, 2, 4 ),
 ( 0.01132179082380021552, 0.01341090848792873130, 0.01445546731999298833, 0.01550002615205724535 ),
 .UNSPECIFIED. ) ;
#60441 = CARTESIAN_POINT ( 'NONE',  ( -104.3929263765338078, 8.102448949553176405, 5.886773742842740909 ) ) ;
#60442 = CARTESIAN_POINT ( 'NONE',  ( 48.74999999999999289, 24.74999999999998579, 3.750000000000000000 ) ) ;
#60443 = ORIENTED_EDGE ( 'NONE', *, *, #2493, .T. ) ;
#60444 = EDGE_LOOP ( 'NONE', ( #29565, #33409, #42364, #67048, #41662, #64080, #22365, #4080 ) ) ;
#60445 = CARTESIAN_POINT ( 'NONE',  ( -48.29292637653378506, 3.094860106618428031, -9.524999999999993250 ) ) ;
#60447 = VECTOR ( 'NONE', #20539, 1000.000000000000000 ) ;
#60446 = CARTESIAN_POINT ( 'NONE',  ( -10.50000000000002309, 8.000000000000000000, -4.000000000000000000 ) ) ;
#60448 = CARTESIAN_POINT ( 'NONE',  ( -130.7049999999999841, 2.607480562269073321, 8.024999999999991473 ) ) ;
#60449 = DIRECTION ( 'NONE',  ( 1.000000000000000000, 0.000000000000000000, 0.000000000000000000 ) ) ;
#60450 = CARTESIAN_POINT ( 'NONE',  ( 10.00000000000001954, 42.00000000000000000, -28.38386403503541899 ) ) ;
#60451 = VERTEX_POINT ( 'NONE', #61521 ) ;
#60452 = CARTESIAN_POINT ( 'NONE',  ( 21.75000000000001066, 21.99999999999998224, -3.750000000000000000 ) ) ;
#60453 = CARTESIAN_POINT ( 'NONE',  ( 1.800649583398759468, 9.000000000000008882, 0.1402270904467449175 ) ) ;
#60454 = SURFACE_STYLE_FILL_AREA ( #24213 ) ;
#60455 = ORIENTED_EDGE ( 'NONE', *, *, #50924, .T. ) ;
#60456 = COLOUR_RGB ( '', 0.72549020, 0.75294118, 0.79215686) ;
#60457 = EDGE_LOOP ( 'NONE', ( #48062, #54448, #7419, #7779 ) ) ;
#60458 = CARTESIAN_POINT ( 'NONE',  ( -75.00000000000000000, 33.00000000000000000, -6.500000000000000000 ) ) ;
#60459 = CARTESIAN_POINT ( 'NONE',  ( -109.0429263765337993, -9.058813317711329915, -2.943386871421370898 ) ) ;
#60460 = CARTESIAN_POINT ( 'NONE',  ( -57.05499999999999261, -9.827790563157499189E-16, -8.024999999999991473 ) ) ;
#60461 = ORIENTED_EDGE ( 'NONE', *, *, #57769, .F. ) ;
#60462 = PLANE ( 'NONE',  #41422 ) ;
#60463 = CARTESIAN_POINT ( 'NONE',  ( -183.2949999999999591, -2.607480562269069768, 8.024999999999991473 ) ) ;
#60464 = LINE ( 'NONE', #61495, #51091 ) ;
#60465 = ORIENTED_EDGE ( 'NONE', *, *, #26453, .F. ) ;
#60466 = EDGE_CURVE ( 'NONE', #63831, #57600, #37334, .T. ) ;
#60467 =( LENGTH_UNIT ( ) NAMED_UNIT ( * ) SI_UNIT ( .MILLI., .METRE. ) );
#60469 = AXIS2_PLACEMENT_3D ( 'NONE', #31676, #26045, #16913 ) ;
#60468 =( NAMED_UNIT ( * ) SI_UNIT ( $, .STERADIAN. ) SOLID_ANGLE_UNIT ( ) );
#60470 = CARTESIAN_POINT ( 'NONE',  ( 44.25000000000000000, 19.24999999999998224, 4.000000000000000000 ) ) ;
#60471 = CARTESIAN_POINT ( 'NONE',  ( -27.33622931176552839, -7.538750321409861677, -3.015364001751804897E-16 ) ) ;
#60472 = CARTESIAN_POINT ( 'NONE',  ( 22.99999999999995026, 0.000000000000000000, 77.00402776293825013 ) ) ;
#60473 = VECTOR ( 'NONE', #23965, 1000.000000000000000 ) ;
#60474 = CARTESIAN_POINT ( 'NONE',  ( -97.94499999999999318, -9.827790563157499189E-16, -8.024999999999991473 ) ) ;
#60475 = CARTESIAN_POINT ( 'NONE',  ( -5.598654528085808657, 158.6449999999999818, 7.705886871421373741 ) ) ;
#60476 = CARTESIAN_POINT ( 'NONE',  ( -76.94499999999997897, -9.827790563157499189E-16, -8.024999999999991473 ) ) ;
#60477 = DIRECTION ( 'NONE',  ( -1.189524669241239115E-16, -1.000000000000000000, -0.000000000000000000 ) ) ;
#60478 = CYLINDRICAL_SURFACE ( 'NONE', #1102, 0.5000000000000004441 ) ;
#60479 = DIRECTION ( 'NONE',  ( -0.000000000000000000, 0.000000000000000000, -1.000000000000000000 ) ) ;
#60480 = FACE_OUTER_BOUND ( 'NONE', #24258, .T. ) ;
#60481 = ORIENTED_EDGE ( 'NONE', *, *, #33836, .T. ) ;
#60482 = CARTESIAN_POINT ( 'NONE',  ( -122.9929263765338163, 8.102448949553171076, -5.886773742842744461 ) ) ;
#60483 = CARTESIAN_POINT ( 'NONE',  ( -140.6949999999999363, -8.437984349512085203, 5.166775262442717831E-16 ) ) ;
#60484 = FACE_OUTER_BOUND ( 'NONE', #25706, .T. ) ;
#60485 = AXIS2_PLACEMENT_3D ( 'NONE', #22353, #68302, #26066 ) ;
#60486 = PRESENTATION_LAYER_ASSIGNMENT (  '', '', ( #51515 ) ) ;
#60487 = EDGE_CURVE ( 'NONE', #59067, #5967, #27159, .T. ) ;
#60488 = EDGE_CURVE ( 'NONE', #19597, #4894, #50742, .T. ) ;
#60489 = CARTESIAN_POINT ( 'NONE',  ( -174.4429263765337907, -1.166476076187852838E-15, -9.524999999999991473 ) ) ;
#60490 = ORIENTED_EDGE ( 'NONE', *, *, #66388, .F. ) ;
#60491 = COLOUR_RGB ( '', 0.72549020, 0.75294118, 0.79215686) ;
#60492 = ORIENTED_EDGE ( 'NONE', *, *, #8007, .T. ) ;
#60493 = DIRECTION ( 'NONE',  ( -0.000000000000000000, -1.000000000000000000, -0.000000000000000000 ) ) ;
#60494 = EDGE_CURVE ( 'NONE', #60346, #4855, #67173, .T. ) ;
#60495 = CARTESIAN_POINT ( 'NONE',  ( -99.05707362346618083, 0.000000000000000000, 9.524999999999991473 ) ) ;
#60496 = AXIS2_PLACEMENT_3D ( 'NONE', #11511, #11160, #5514 ) ;
#60497 = CARTESIAN_POINT ( 'NONE',  ( -71.50000000000000000, 14.49137674618942562, -7.500000000000000000 ) ) ;
#60498 = ORIENTED_EDGE ( 'NONE', *, *, #68319, .F. ) ;
#60499 = CARTESIAN_POINT ( 'NONE',  ( -145.4050000000000011, -2.607480562269069768, 8.024999999999991473 ) ) ;
#60500 = ORIENTED_EDGE ( 'NONE', *, *, #27909, .T. ) ;
#60501 = ORIENTED_EDGE ( 'NONE', *, *, #24686, .T. ) ;
#60502 = CARTESIAN_POINT ( 'NONE',  ( 0.000000000000000000, 0.000000000000000000, 1.000000000000000000 ) ) ;
#60503 = DIRECTION ( 'NONE',  ( 0.000000000000000000, 0.000000000000000000, 1.000000000000000000 ) ) ;
#60504 = VERTEX_POINT ( 'NONE', #40466 ) ;
#60505 = ADVANCED_FACE ( 'NONE', ( #57666 ), #66504, .F. ) ;
#60506 = CARTESIAN_POINT ( 'NONE',  ( -55.15277687475337842, -8.620516334094102007, -2.355797634318733458 ) ) ;
#60507 = CARTESIAN_POINT ( 'NONE',  ( -5.598654528085808657, 131.6449999999999818, 7.705886871421373741 ) ) ;
#60508 =( NAMED_UNIT ( * ) SI_UNIT ( $, .STERADIAN. ) SOLID_ANGLE_UNIT ( ) );
#60509 = VERTEX_POINT ( 'NONE', #40821 ) ;
#60510 = CARTESIAN_POINT ( 'NONE',  ( -9.058813317711337021, 129.1550000000000011, -2.943386871421374895 ) ) ;
#60511 = CARTESIAN_POINT ( 'NONE',  ( -54.65499999999997982, -7.632228543268600340, -2.479861379858950166 ) ) ;
#60512 = CIRCLE ( 'NONE', #8869, 7.500000000000000000 ) ;
#60513 = EDGE_CURVE ( 'NONE', #36309, #26603, #65342, .T. ) ;
#60514 = CARTESIAN_POINT ( 'NONE',  ( 40.78947368421051323, 108.1536491499103363, -3.000000000000000444 ) ) ;
#60515 = ORIENTED_EDGE ( 'NONE', *, *, #9902, .F. ) ;
#60516 = CARTESIAN_POINT ( 'NONE',  ( -3.094860106618432471, 158.7049999999999557, -9.525000000000000355 ) ) ;
#60517 = DIRECTION ( 'NONE',  ( 0.000000000000000000, 0.000000000000000000, -1.000000000000000000 ) ) ;
#60518 = CYLINDRICAL_SURFACE ( 'NONE', #652, 9.524999999999991473 ) ;
#60519 = CIRCLE ( 'NONE', #58331, 0.5000000000000004441 ) ;
#60520 = CARTESIAN_POINT ( 'NONE',  ( -74.99999999999998579, 50.00000000000000000, 9.500000000000001776 ) ) ;
#60521 = CYLINDRICAL_SURFACE ( 'NONE', #43336, 0.2500000000000002220 ) ;
#60522 = VERTEX_POINT ( 'NONE', #68228 ) ;
#60523 = CIRCLE ( 'NONE', #20066, 5.499999999999976907 ) ;
#60524 = SURFACE_STYLE_USAGE ( .BOTH. , #33473 ) ;
#60525 = ORIENTED_EDGE ( 'NONE', *, *, #26, .F. ) ;
#60526 = COLOUR_RGB ( '', 0.72549020, 0.75294118, 0.79215686) ;
#60527 = FILL_AREA_STYLE ('',( #33141 ) ) ;
#60528 = FILL_AREA_STYLE ('',( #6385 ) ) ;
#60529 = CARTESIAN_POINT ( 'NONE',  ( -160.7049999999999841, 2.607480562269073321, 8.024999999999991473 ) ) ;
#60530 = ORIENTED_EDGE ( 'NONE', *, *, #66817, .F. ) ;
#60531 =( LENGTH_UNIT ( ) NAMED_UNIT ( * ) SI_UNIT ( .MILLI., .METRE. ) );
#60532 = COLOUR_RGB ( '', 0.40784314, 0.44705882, 0.49803922) ;
#60533 = DIRECTION ( 'NONE',  ( 1.000000000000000000, 0.000000000000000000, 0.000000000000000000 ) ) ;
#60534 = LINE ( 'NONE', #34514, #52953 ) ;
#60535 = CARTESIAN_POINT ( 'NONE',  ( -83.49999999999998579, 4.336808689942018722E-16, -5.100000000000000533 ) ) ;
#60536 = VERTEX_POINT ( 'NONE', #62239 ) ;
#60537 = AXIS2_PLACEMENT_3D ( 'NONE', #36608, #19673, #14388 ) ;
#60538 = VECTOR ( 'NONE', #24651, 1000.000000000000000 ) ;
#60539 = VERTEX_POINT ( 'NONE', #36241 ) ;
#60540 = CARTESIAN_POINT ( 'NONE',  ( 0.000000000000000000, 115.4999999999999574, 0.000000000000000000 ) ) ;
#60541 = CARTESIAN_POINT ( 'NONE',  ( 24.00000000000000000, 0.000000000000000000, -3.000000000000000000 ) ) ;
#60542 = CARTESIAN_POINT ( 'NONE',  ( -87.95499999999999829, -7.632228543268599452, 2.479861379858951054 ) ) ;
#60543 = VERTEX_POINT ( 'NONE', #25980 ) ;
#60544 = DIRECTION ( 'NONE',  ( 0.000000000000000000, 0.000000000000000000, -1.000000000000000000 ) ) ;
#60545 = PRESENTATION_STYLE_ASSIGNMENT (( #17687 ) ) ;
#60546 = PRESENTATION_LAYER_ASSIGNMENT (  '', '', ( #21232 ) ) ;
#60547 = EDGE_CURVE ( 'NONE', #56195, #52813, #40666, .T. ) ;
#60548 = SURFACE_STYLE_FILL_AREA ( #28887 ) ;
#60549 = ORIENTED_EDGE ( 'NONE', *, *, #34142, .T. ) ;
#60551 = PLANE ( 'NONE',  #24642 ) ;
#60550 = CARTESIAN_POINT ( 'NONE',  ( 45.00000000000000000, 9.639620389971920389, 6.999999999999999112 ) ) ;
#60552 = CARTESIAN_POINT ( 'NONE',  ( -5.598654528085806881, 127.7450000000000045, -7.705886871421374629 ) ) ;
#60553 = CARTESIAN_POINT ( 'NONE',  ( -102.1449999999999818, -4.716976649647092401, 6.492361379858946790 ) ) ;
#60554 = PRODUCT_RELATED_PRODUCT_CATEGORY ( 'part', '', ( #32191 ) ) ;
#60556 = CARTESIAN_POINT ( 'NONE',  ( -16.30670699309780503, 10.98201309903883072, 4.837397118674712893 ) ) ;
#60555 = CARTESIAN_POINT ( 'NONE',  ( -21.02379604162863913, 110.4999999999999858, -10.00000000000000000 ) ) ;
#60557 = EDGE_CURVE ( 'NONE', #8139, #2682, #23815, .T. ) ;
#60558 = AXIS2_PLACEMENT_3D ( 'NONE', #43435, #33172, #48691 ) ;
#60559 = CARTESIAN_POINT ( 'NONE',  ( -155.5429263765338135, 9.058813317711329915, 2.943386871421369566 ) ) ;
#60560 = EDGE_CURVE ( 'NONE', #52516, #17554, #8056, .T. ) ;
#60561 = CARTESIAN_POINT ( 'NONE',  ( -163.4949999999999761, 6.826472737025113702, -4.959722759717902107 ) ) ;
#60562 = VECTOR ( 'NONE', #65147, 1000.000000000000000 ) ;
#60563 = ADVANCED_FACE ( 'NONE', ( #52746 ), #47507, .T. ) ;
#60564 = EDGE_CURVE ( 'NONE', #63887, #56195, #67611, .T. ) ;
#60565 = CARTESIAN_POINT ( 'NONE',  ( 6.667623377008398577, 6.451337545287478825, 0.2685431138779675320 ) ) ;
#60566 = EDGE_LOOP ( 'NONE', ( #527, #44744, #6698, #41282 ) ) ;
#60567 = FACE_OUTER_BOUND ( 'NONE', #41297, .T. ) ;
#60568 = VERTEX_POINT ( 'NONE', #58346 ) ;
#60569 = CARTESIAN_POINT ( 'NONE',  ( -65.84292637653379643, 9.058813317711329915, -2.943386871421373119 ) ) ;
#60570 = COLOUR_RGB ( '', 0.08235294, 0.09019608, 0.10196078) ;
#60571 = AXIS2_PLACEMENT_3D ( 'NONE', #38553, #11762, #51844 ) ;
#60572 = CARTESIAN_POINT ( 'NONE',  ( -45.89268334517834802, 9.343685333619713873, 6.169793031889358126 ) ) ;
#60573 = AXIS2_PLACEMENT_3D ( 'NONE', #19503, #52587, #9322 ) ;
#60574 = ADVANCED_FACE ( 'NONE', ( #10172 ), #16024, .T. ) ;
#60575 = COLOUR_RGB ( '', 0.40784314, 0.44705882, 0.49803922) ;
#60576 = LINE ( 'NONE', #44130, #21431 ) ;
#60577 = FILL_AREA_STYLE_COLOUR ( '', #27016 ) ;
#60578 = PLANE ( 'NONE',  #59529 ) ;
#60579 = ADVANCED_FACE ( 'NONE', ( #8781 ), #30208, .T. ) ;
#60580 = CARTESIAN_POINT ( 'NONE',  ( 3.851859888774471706E-31, -8.500000000000000000, 24.00000000000000000 ) ) ;
#60581 = VERTEX_POINT ( 'NONE', #16850 ) ;
#60582 = CARTESIAN_POINT ( 'NONE',  ( -170.4549999999999841, 7.632228543268599452, -2.479861379858951942 ) ) ;
#60583 = ORIENTED_EDGE ( 'NONE', *, *, #16377, .T. ) ;
#60584 = CARTESIAN_POINT ( 'NONE',  ( -111.8929263765338078, -8.102448949553174629, -5.886773742842741797 ) ) ;
#60585 =( NAMED_UNIT ( * ) SI_UNIT ( $, .STERADIAN. ) SOLID_ANGLE_UNIT ( ) );
#60586 =( GEOMETRIC_REPRESENTATION_CONTEXT ( 3 ) GLOBAL_UNCERTAINTY_ASSIGNED_CONTEXT ( ( #59405 ) ) GLOBAL_UNIT_ASSIGNED_CONTEXT ( ( #15878, #27070, #32035 ) ) REPRESENTATION_CONTEXT ( 'NONE', 'WORKASPACE' ) );
#60587 = SURFACE_STYLE_FILL_AREA ( #18049 ) ;
#60588 = CARTESIAN_POINT ( 'NONE',  ( -4.716976649647097730, 151.3570736234661638, -6.492361379858953896 ) ) ;
#60589 = ORIENTED_EDGE ( 'NONE', *, *, #53745, .T. ) ;
#60590 =( NAMED_UNIT ( * ) PLANE_ANGLE_UNIT ( ) SI_UNIT ( $, .RADIAN. ) );
#60591 = CARTESIAN_POINT ( 'NONE',  ( -82.85499999999998977, 4.716976649647094177, 6.492361379858945902 ) ) ;
#60592 = CARTESIAN_POINT ( 'NONE',  ( 0.000000000000000000, 121.0570736234661524, -8.025000000000000355 ) ) ;
#60593 = CARTESIAN_POINT ( 'NONE',  ( 8.102448949553181734, 124.5049999999999812, 5.886773742842750679 ) ) ;
#60594 =( GEOMETRIC_REPRESENTATION_CONTEXT ( 3 ) GLOBAL_UNCERTAINTY_ASSIGNED_CONTEXT ( ( #55825 ) ) GLOBAL_UNIT_ASSIGNED_CONTEXT ( ( #7206, #33244, #23370 ) ) REPRESENTATION_CONTEXT ( 'NONE', 'WORKASPACE' ) );
#60595 = CARTESIAN_POINT ( 'NONE',  ( -195.0000000000000000, 0.000000000000000000, 0.000000000000000000 ) ) ;
#60596 = SURFACE_STYLE_USAGE ( .BOTH. , #27882 ) ;
#60597 = CARTESIAN_POINT ( 'NONE',  ( -126.5929263765345496, -3.094860106630666241, -9.524999999991102584 ) ) ;
#60598 = CARTESIAN_POINT ( 'NONE',  ( 8.000000000000000000, 33.74999999999998579, -3.750000000000000000 ) ) ;
#60599 = FACE_OUTER_BOUND ( 'NONE', #63747, .T. ) ;
#60600 = CARTESIAN_POINT ( 'NONE',  ( -112.8570736234661638, -5.598654528085803328, -7.705886871421366635 ) ) ;
#60601 = ORIENTED_EDGE ( 'NONE', *, *, #58867, .F. ) ;
#60602 = SURFACE_STYLE_USAGE ( .BOTH. , #1825 ) ;
#60603 = FILL_AREA_STYLE ('',( #46226 ) ) ;
#60605 = EDGE_CURVE ( 'NONE', #53118, #38818, #5482, .T. ) ;
#60604 = AXIS2_PLACEMENT_3D ( 'NONE', #36803, #52951, #46679 ) ;
#60607 = CARTESIAN_POINT ( 'NONE',  ( -59.09499999999997044, -2.607480562269071545, -8.024999999999991473 ) ) ;
#60606 = COLOUR_RGB ( '', 0.31764706, 0.68627451, 0.89019608) ;
#60608 = ORIENTED_EDGE ( 'NONE', *, *, #56629, .T. ) ;
#60609 = DIRECTION ( 'NONE',  ( -0.000000000000000000, -0.000000000000000000, 1.000000000000000000 ) ) ;
#60610 = CARTESIAN_POINT ( 'NONE',  ( -139.4070736234667152, 3.094860106609554684, -9.525000000006441425 ) ) ;
#60611 = AXIS2_PLACEMENT_3D ( 'NONE', #61271, #66916, #50729 ) ;
#60612 = ORIENTED_EDGE ( 'NONE', *, *, #24751, .T. ) ;
#60613 = CARTESIAN_POINT ( 'NONE',  ( -53.24388477452971813, -10.30142299214062085, 2.428806256206293313 ) ) ;
#60614 = CARTESIAN_POINT ( 'NONE',  ( -54.74499999999999034, 4.716976649647094177, 6.492361379858945902 ) ) ;
#60615 = VERTEX_POINT ( 'NONE', #53754 ) ;
#60616 = VECTOR ( 'NONE', #20440, 1000.000000000000000 ) ;
#60617 = DIRECTION ( 'NONE',  ( 0.8660254037844385966, -0.5000000000000001110, 0.000000000000000000 ) ) ;
#60618 = CARTESIAN_POINT ( 'NONE',  ( -109.5549999999999926, 0.000000000000000000, 8.024999999999991473 ) ) ;
#60619 = ORIENTED_EDGE ( 'NONE', *, *, #39255, .F. ) ;
#60620 = PLANE ( 'NONE',  #1293 ) ;
#60621 = CARTESIAN_POINT ( 'NONE',  ( 32.00000000000000711, 42.00000000000000000, -45.00000000000000000 ) ) ;
#60622 = CIRCLE ( 'NONE', #69625, 0.5000000000000004441 ) ;
#60623 = DIRECTION ( 'NONE',  ( 1.000000000000000000, 0.000000000000000000, 0.000000000000000000 ) ) ;
#60624 = LINE ( 'NONE', #6825, #57792 ) ;
#60625 = CARTESIAN_POINT ( 'NONE',  ( 7.899999999999995914, 11.99999999999999289, 3.500000000000004885 ) ) ;
#60626 =( GEOMETRIC_REPRESENTATION_CONTEXT ( 3 ) GLOBAL_UNCERTAINTY_ASSIGNED_CONTEXT ( ( #20777 ) ) GLOBAL_UNIT_ASSIGNED_CONTEXT ( ( #1128, #5414, #43128 ) ) REPRESENTATION_CONTEXT ( 'NONE', 'WORKASPACE' ) );
#60627 = CARTESIAN_POINT ( 'NONE',  ( -149.1570736234661751, -9.058813317711329915, -2.943386871421370898 ) ) ;
#60628 = CARTESIAN_POINT ( 'NONE',  ( 34.99999999999999289, 99.99999999999997158, -4.000000000000000000 ) ) ;
#60629 = CARTESIAN_POINT ( 'NONE',  ( -9.058813317711338797, 131.3449999999999989, 2.943386871421373563 ) ) ;
#60630 = CARTESIAN_POINT ( 'NONE',  ( -84.80707362346616662, 10.01517768586948698, -1.839758294383808571E-15 ) ) ;
#60631 = SURFACE_STYLE_USAGE ( .BOTH. , #50450 ) ;
#60632 = VERTEX_POINT ( 'NONE', #21758 ) ;
#60633 = VECTOR ( 'NONE', #21305, 1000.000000000000227 ) ;
#60634 = DIRECTION ( 'NONE',  ( 0.000000000000000000, 0.9396926207859104263, -0.3420201433256632173 ) ) ;
#60636 = SURFACE_SIDE_STYLE ('',( #33915 ) ) ;
#60635 =( NAMED_UNIT ( * ) SI_UNIT ( $, .STERADIAN. ) SOLID_ANGLE_UNIT ( ) );
#60637 = SURFACE_STYLE_FILL_AREA ( #12112 ) ;
#60638 = CARTESIAN_POINT ( 'NONE',  ( -131.9050000000000011, 2.607480562269068880, -8.024999999999993250 ) ) ;
#60639 = CARTESIAN_POINT ( 'NONE',  ( -164.9929263765338021, 8.102448949553172852, -5.886773742842744461 ) ) ;
#60640 = CARTESIAN_POINT ( 'NONE',  ( -132.8950000000000102, 6.826472737025116366, 4.959722759717898555 ) ) ;
#60641 = PRESENTATION_LAYER_ASSIGNMENT (  '', '', ( #28090 ) ) ;
#60642 = CARTESIAN_POINT ( 'NONE',  ( -132.1449999999999818, -4.716976649647092401, 6.492361379858946790 ) ) ;
#60643 = ORIENTED_EDGE ( 'NONE', *, *, #64407, .F. ) ;
#60644 = AXIS2_PLACEMENT_3D ( 'NONE', #55573, #66112, #50306 ) ;
#60645 = CARTESIAN_POINT ( 'NONE',  ( -147.0570736234661808, 0.000000000000000000, 9.524999999999991473 ) ) ;
#60646 = COLOUR_RGB ( '', 0.08235294, 0.09019608, 0.10196078) ;
#60647 =( NAMED_UNIT ( * ) PLANE_ANGLE_UNIT ( ) SI_UNIT ( $, .RADIAN. ) );
#60648 = EDGE_CURVE ( 'NONE', #25670, #30747, #4730, .T. ) ;
#60649 = CARTESIAN_POINT ( 'NONE',  ( -29.91370621994235890, -7.761720733523295834, -0.7755720678495816589 ) ) ;
#60650 = CARTESIAN_POINT ( 'NONE',  ( -49.10499999999998977, -6.826472737025115478, 4.959722759717900331 ) ) ;
#60651 = CARTESIAN_POINT ( 'NONE',  ( -61.34499999999998465, 7.632228543268599452, -2.479861379858951942 ) ) ;
#60652 = EDGE_CURVE ( 'NONE', #65139, #43795, #60914, .T. ) ;
#60653 = CARTESIAN_POINT ( 'NONE',  ( 39.74999999999999289, 18.99999999999997868, 3.750000000000000000 ) ) ;
#60654 = DIRECTION ( 'NONE',  ( 1.000000000000000000, -7.709882115452468306E-16, -0.000000000000000000 ) ) ;
#60655 = PRESENTATION_STYLE_ASSIGNMENT (( #17782 ) ) ;
#60656 = CARTESIAN_POINT ( 'NONE',  ( 45.50000000000000000, -1.469576158976824618E-14, -6.500000000000000000 ) ) ;
#60657 = DIRECTION ( 'NONE',  ( 0.000000000000000000, 0.000000000000000000, 1.000000000000000000 ) ) ;
#60659 =( BOUNDED_CURVE ( )  B_SPLINE_CURVE ( 3, ( #13667, #24547, #19273, #40782 ),
 .UNSPECIFIED., .F., .F. ) 
 B_SPLINE_CURVE_WITH_KNOTS ( ( 4, 4 ),
 ( 4.712388980384692339, 6.283185307179586232 ),
 .UNSPECIFIED. ) 
 CURVE ( )  GEOMETRIC_REPRESENTATION_ITEM ( )  RATIONAL_B_SPLINE_CURVE ( ( 1.000000000000000000, 0.8047378541243654926, 0.8047378541243654926, 1.000000000000000000 ) ) 
 REPRESENTATION_ITEM ( '' )  );
#60658 = CARTESIAN_POINT ( 'NONE',  ( -97.64292637653380780, -5.598654528085801552, 7.705886871421367523 ) ) ;
#60660 = PRODUCT_CONTEXT ( 'NONE', #57672, 'mechanical' ) ;
#60661 = SURFACE_STYLE_FILL_AREA ( #23062 ) ;
#60662 = CYLINDRICAL_SURFACE ( 'NONE', #42835, 9.524999999999991473 ) ;
#60663 = CIRCLE ( 'NONE', #31496, 9.524999999999991473 ) ;
#60664 = DIRECTION ( 'NONE',  ( 0.000000000000000000, 0.000000000000000000, 1.000000000000000000 ) ) ;
#60665 = LINE ( 'NONE', #24092, #59526 ) ;
#60666 =( NAMED_UNIT ( * ) PLANE_ANGLE_UNIT ( ) SI_UNIT ( $, .RADIAN. ) );
#60667 = EDGE_CURVE ( 'NONE', #36693, #34405, #49696, .T. ) ;
#60668 = FACE_OUTER_BOUND ( 'NONE', #13352, .T. ) ;
#60669 = ORIENTED_EDGE ( 'NONE', *, *, #22174, .F. ) ;
#60670 = DIRECTION ( 'NONE',  ( -1.000000000000000000, -0.000000000000000000, -0.000000000000000000 ) ) ;
#60671 = VECTOR ( 'NONE', #22713, 1000.000000000000000 ) ;
#60672 = CARTESIAN_POINT ( 'NONE',  ( -1.000000000000028644, 1.469576158976823553E-15, -11.99999999999999645 ) ) ;
#60673 = AXIS2_PLACEMENT_3D ( 'NONE', #13671, #35488, #67848 ) ;
#60674 = VERTEX_POINT ( 'NONE', #33007 ) ;
#60675 = PRESENTATION_STYLE_ASSIGNMENT (( #51192 ) ) ;
#60676 = CARTESIAN_POINT ( 'NONE',  ( 2.607480562269071989, 125.7070736234661723, 8.025000000000002132 ) ) ;
#60678 = AXIS2_PLACEMENT_3D ( 'NONE', #43182, #6502, #136 ) ;
#60677 = DIRECTION ( 'NONE',  ( 0.000000000000000000, 1.000000000000000000, 0.000000000000000000 ) ) ;
#60679 = SURFACE_STYLE_FILL_AREA ( #67028 ) ;
#60680 = LINE ( 'NONE', #12148, #8367 ) ;
#60681 = VERTEX_POINT ( 'NONE', #54447 ) ;
#60682 = DIRECTION ( 'NONE',  ( 0.000000000000000000, -1.000000000000000000, 0.000000000000000000 ) ) ;
#60683 = DIRECTION ( 'NONE',  ( 1.000000000000000000, -0.000000000000000000, -0.000000000000000000 ) ) ;
#60684 = VERTEX_POINT ( 'NONE', #5907 ) ;
#60685 = EDGE_CURVE ( 'NONE', #36711, #60416, #20460, .T. ) ;
#60686 = CARTESIAN_POINT ( 'NONE',  ( -119.0070736234661695, -8.102448949553174629, -5.886773742842741797 ) ) ;
#60687 = VECTOR ( 'NONE', #4939, 1000.000000000000000 ) ;
#60688 = FACE_OUTER_BOUND ( 'NONE', #32311, .T. ) ;
#60689 = ADVANCED_FACE ( 'NONE', ( #21398 ), #21606, .F. ) ;
#60690 = CARTESIAN_POINT ( 'NONE',  ( -89.54499999999998749, -7.632228543268600340, -2.479861379858950166 ) ) ;
#60691 = ORIENTED_EDGE ( 'NONE', *, *, #64740, .F. ) ;
#60692 = B_SPLINE_CURVE_WITH_KNOTS ( 'NONE', 3,
 ( #28352, #40342, #67069, #36110, #30800, #19559, #45650, #56497, #8675, #9375, #3692, #41053, #24823, #36486 ),
 .UNSPECIFIED., .F., .F.,
 ( 4, 2, 2, 2, 2, 2, 4 ),
 ( 0.000000000000000000, 0.0005917671672764541774, 0.001183534334552908355, 0.001479417918191135335, 0.001775301501829362532, 0.002071185085467589729, 0.002367068669105816710 ),
 .UNSPECIFIED. ) ;
#60693 = AXIS2_PLACEMENT_3D ( 'NONE', #15035, #4072, #57932 ) ;
#60694 = CARTESIAN_POINT ( 'NONE',  ( -9.827790563157511022E-16, 124.4429263765338192, 8.025000000000000355 ) ) ;
#60695 = SURFACE_STYLE_FILL_AREA ( #11482 ) ;
#60696 = UNCERTAINTY_MEASURE_WITH_UNIT (LENGTH_MEASURE( 1.000000000000000082E-05 ), #67726, 'distance_accuracy_value', 'NONE');
#60697 = ORIENTED_EDGE ( 'NONE', *, *, #61687, .F. ) ;
#60698 = CARTESIAN_POINT ( 'NONE',  ( 6.826472737025121695, 161.4929263765338305, -4.959722759717905660 ) ) ;
#60699 =( LENGTH_UNIT ( ) NAMED_UNIT ( * ) SI_UNIT ( .MILLI., .METRE. ) );
#60700 = COLOUR_RGB ( '', 0.09019608, 0.27058824, 0.51372549) ;
#60701 = FILL_AREA_STYLE ('',( #39295 ) ) ;
#60702 = ORIENTED_EDGE ( 'NONE', *, *, #52333, .T. ) ;
#60703 = CARTESIAN_POINT ( 'NONE',  ( -6.413663052920317575, 2.499999999999997780, -2.891209729714699250 ) ) ;
#60704 = ORIENTED_EDGE ( 'NONE', *, *, #30594, .T. ) ;
#60705 = DIRECTION ( 'NONE',  ( -0.000000000000000000, -1.000000000000000000, 0.000000000000000000 ) ) ;
#60706 = FILL_AREA_STYLE_COLOUR ( '', #18951 ) ;
#60707 = SURFACE_STYLE_FILL_AREA ( #66340 ) ;
#60708 = CARTESIAN_POINT ( 'NONE',  ( -181.7070736234661865, -3.094860106618431139, -9.524999999999991473 ) ) ;
#60709 = CIRCLE ( 'NONE', #56186, 0.9999999999999995559 ) ;
#60710 = DIRECTION ( 'NONE',  ( -0.000000000000000000, -0.000000000000000000, -1.000000000000000000 ) ) ;
#60711 = FACE_BOUND ( 'NONE', #39299, .T. ) ;
#60712 = CARTESIAN_POINT ( 'NONE',  ( -112.5570736234661808, -1.166476076187852838E-15, -9.524999999999991473 ) ) ;
#60713 = SURFACE_STYLE_USAGE ( .BOTH. , #50192 ) ;
#60714 = LINE ( 'NONE', #62108, #4367 ) ;
#60715 = VERTEX_POINT ( 'NONE', #53434 ) ;
#60716 = CARTESIAN_POINT ( 'NONE',  ( 0.000000000000000000, -2.500000000000000000, 3.000000000000000444 ) ) ;
#60717 = DIRECTION ( 'NONE',  ( 0.000000000000000000, 0.000000000000000000, -1.000000000000000000 ) ) ;
#60718 = CARTESIAN_POINT ( 'NONE',  ( -9.250000000000003553, 27.99999999999998934, -3.750000000000000000 ) ) ;
#60719 = ORIENTED_EDGE ( 'NONE', *, *, #6709, .F. ) ;
#60720 = CARTESIAN_POINT ( 'NONE',  ( -157.2549999999999955, -4.716976649647092401, 6.492361379858946790 ) ) ;
#60721 = CARTESIAN_POINT ( 'NONE',  ( -24.00000000000000000, 1.000000000000000000, 4.000000000000000000 ) ) ;
#60722 = ADVANCED_FACE ( 'NONE', ( #61781 ), #13258, .F. ) ;
#60723 = CARTESIAN_POINT ( 'NONE',  ( -163.9449999999999932, -9.827790563157499189E-16, -8.024999999999991473 ) ) ;
#60724 = CARTESIAN_POINT ( 'NONE',  ( -153.5949999999999704, 2.607480562269072433, 8.024999999999991473 ) ) ;
#60725 = ORIENTED_EDGE ( 'NONE', *, *, #354, .F. ) ;
#60726 = CARTESIAN_POINT ( 'NONE',  ( 60.00000000000000000, 1.797044900979284448E-15, -9.500000000000000000 ) ) ;
#60727 = CARTESIAN_POINT ( 'NONE',  ( 44.15219150100326573, 9.717397167001085023, 3.137420992959929489 ) ) ;
#60728 = CARTESIAN_POINT ( 'NONE',  ( -77.30499999999996419, 8.437984349512085203, -1.550032578732815448E-15 ) ) ;
#60729 = CARTESIAN_POINT ( 'NONE',  ( 35.99999999999999289, 0.000000000000000000, -37.00402776293825724 ) ) ;
#60730 = VECTOR ( 'NONE', #34551, 1000.000000000000000 ) ;
#60731 = DIRECTION ( 'NONE',  ( 0.000000000000000000, -0.000000000000000000, 1.000000000000000000 ) ) ;
#60732 = EDGE_CURVE ( 'NONE', #61248, #66756, #23151, .T. ) ;
#60733 = CARTESIAN_POINT ( 'NONE',  ( -71.99499999999999034, -6.826472737025113702, 4.959722759717902107 ) ) ;
#60734 = CARTESIAN_POINT ( 'NONE',  ( -8.102448949553181734, 150.6050000000000182, 5.886773742842747126 ) ) ;
#60735 = DIRECTION ( 'NONE',  ( 0.000000000000000000, -0.000000000000000000, -1.000000000000000000 ) ) ;
#60736 = PRESENTATION_LAYER_ASSIGNMENT (  '', '', ( #43931 ) ) ;
#60737 = EDGE_CURVE ( 'NONE', #50095, #12034, #32815, .T. ) ;
#60738 = UNCERTAINTY_MEASURE_WITH_UNIT (LENGTH_MEASURE( 1.000000000000000082E-05 ), #46100, 'distance_accuracy_value', 'NONE');
#60739 = B_SPLINE_CURVE_WITH_KNOTS ( 'NONE', 3,
 ( #29766, #40013, #61405, #13221, #67060, #56133, #50878, #2636, #24135, #13570, #13932, #35743 ),
 .UNSPECIFIED., .F., .F.,
 ( 4, 2, 2, 2, 2, 4 ),
 ( 2.969228936714856331E-16, 0.002162875435572643792, 0.003244313153358819105, 0.004325750871144991815, 0.006488626306717332030, 0.008651501742289673114 ),
 .UNSPECIFIED. ) ;
#60740 = STYLED_ITEM ( 'NONE', ( #20269 ), #16855 ) ;
#60741 = FILL_AREA_STYLE_COLOUR ( '', #14678 ) ;
#60742 = EDGE_CURVE ( 'NONE', #61621, #52608, #66556, .T. ) ;
#60743 =( LENGTH_UNIT ( ) NAMED_UNIT ( * ) SI_UNIT ( .MILLI., .METRE. ) );
#60744 = DIRECTION ( 'NONE',  ( -1.000000000000000000, 0.000000000000000000, 0.000000000000000000 ) ) ;
#60745 = EDGE_CURVE ( 'NONE', #59067, #197, #2416, .T. ) ;
#60746 = CARTESIAN_POINT ( 'NONE',  ( -22.50000000000000711, 37.00000000000000000, 4.000000000000000000 ) ) ;
#60747 = ORIENTED_EDGE ( 'NONE', *, *, #69200, .F. ) ;
#60748 = ORIENTED_EDGE ( 'NONE', *, *, #6364, .F. ) ;
#60749 = FILL_AREA_STYLE_COLOUR ( '', #35272 ) ;
#60750 = VECTOR ( 'NONE', #55121, 1000.000000000000000 ) ;
#60751 = DIRECTION ( 'NONE',  ( -0.000000000000000000, 1.000000000000000000, -0.000000000000000000 ) ) ;
#60752 =( BOUNDED_CURVE ( )  B_SPLINE_CURVE ( 2, ( #57301, #20719, #47138 ),
 .UNSPECIFIED., .F., .F. ) 
 B_SPLINE_CURVE_WITH_KNOTS ( ( 3, 3 ),
 ( 0.9891304347826086474, 0.9913043478260870067 ),
 .UNSPECIFIED. ) 
 CURVE ( )  GEOMETRIC_REPRESENTATION_ITEM ( )  RATIONAL_B_SPLINE_CURVE ( ( 1.000000000000000000, 0.9510565162951535312, 1.000000000000000000 ) ) 
 REPRESENTATION_ITEM ( '' )  );
#60753 =( GEOMETRIC_REPRESENTATION_CONTEXT ( 3 ) GLOBAL_UNCERTAINTY_ASSIGNED_CONTEXT ( ( #51585 ) ) GLOBAL_UNIT_ASSIGNED_CONTEXT ( ( #22731, #17477, #12859 ) ) REPRESENTATION_CONTEXT ( 'NONE', 'WORKASPACE' ) );
#60754 = VECTOR ( 'NONE', #37007, 1000.000000000000000 ) ;
#60755 = DIRECTION ( 'NONE',  ( -0.000000000000000000, -0.000000000000000000, -1.000000000000000000 ) ) ;
#60756 = SURFACE_STYLE_USAGE ( .BOTH. , #45680 ) ;
#60757 = VERTEX_POINT ( 'NONE', #18565 ) ;
#60758 = PRESENTATION_LAYER_ASSIGNMENT (  '', '', ( #59666 ) ) ;
#60759 = CARTESIAN_POINT ( 'NONE',  ( -105.3549999999999898, -4.716976649647093289, -6.492361379858945902 ) ) ;
#60760 = ORIENTED_EDGE ( 'NONE', *, *, #10508, .F. ) ;
#60761 = DIRECTION ( 'NONE',  ( 0.000000000000000000, 0.000000000000000000, 1.000000000000000000 ) ) ;
#60762 = ORIENTED_EDGE ( 'NONE', *, *, #27537, .F. ) ;
#60763 = CARTESIAN_POINT ( 'NONE',  ( 31.00000000000001066, 42.00000000000000000, -4.033029030585349936E-15 ) ) ;
#60764 = CARTESIAN_POINT ( 'NONE',  ( 52.75000000000000000, 24.99999999999998579, -4.000000000000000000 ) ) ;
#60765 = ORIENTED_EDGE ( 'NONE', *, *, #3838, .F. ) ;
#60766 = VECTOR ( 'NONE', #69353, 1000.000000000000000 ) ;
#60767 = CARTESIAN_POINT ( 'NONE',  ( 75.83633811589984930, 13.00000000000000178, 66.72655454856716517 ) ) ;
#60768 = ORIENTED_EDGE ( 'NONE', *, *, #18581, .F. ) ;
#60769 = ORIENTED_EDGE ( 'NONE', *, *, #41171, .T. ) ;
#60770 = FILL_AREA_STYLE ('',( #50252 ) ) ;
#60771 = CARTESIAN_POINT ( 'NONE',  ( 15.98999599679679839, 117.9999999999999716, 10.00000000000000000 ) ) ;
#60772 = CARTESIAN_POINT ( 'NONE',  ( -51.84221223720477667, -9.947368421052628307, 4.481646853389226415 ) ) ;
#60773 =( NAMED_UNIT ( * ) SI_UNIT ( $, .STERADIAN. ) SOLID_ANGLE_UNIT ( ) );
#60774 = ORIENTED_EDGE ( 'NONE', *, *, #6056, .T. ) ;
#60775 = CARTESIAN_POINT ( 'NONE',  ( 2.607480562269071989, 133.5929263765337680, 8.025000000000002132 ) ) ;
#60776 = CARTESIAN_POINT ( 'NONE',  ( 0.000000000000000000, 87.30187232391182306, 0.000000000000000000 ) ) ;
#60777 = DIRECTION ( 'NONE',  ( 1.000000000000000000, 0.000000000000000000, 0.000000000000000000 ) ) ;
#60778 = COLOUR_RGB ( '', 0.31764706, 0.68627451, 0.89019608) ;
#60779 = CARTESIAN_POINT ( 'NONE',  ( -4.716976649647097730, 114.2429263765338163, -6.492361379858953896 ) ) ;
#60780 = VERTEX_POINT ( 'NONE', #34035 ) ;
#60781 = STYLED_ITEM ( 'NONE', ( #29028 ), #18149 ) ;
#60782 = DIRECTION ( 'NONE',  ( 0.000000000000000000, -0.7431448254773930229, 0.6691306063588596809 ) ) ;
#60783 = ORIENTED_EDGE ( 'NONE', *, *, #21529, .T. ) ;
#60784 = SURFACE_STYLE_FILL_AREA ( #67463 ) ;
#60785 = CARTESIAN_POINT ( 'NONE',  ( -13.50000000000000533, 30.99999999999999289, 4.000000000000000000 ) ) ;
#60786 = CYLINDRICAL_SURFACE ( 'NONE', #1477, 5.000000000000000888 ) ;
#60787 = DIRECTION ( 'NONE',  ( -0.03448275862069643399, 0.9994052928406507164, 0.000000000000000000 ) ) ;
#60788 = CARTESIAN_POINT ( 'NONE',  ( -133.8549999999999898, 4.716976649647094177, 6.492361379858945902 ) ) ;
#60789 = FILL_AREA_STYLE ('',( #39053 ) ) ;
#60790 = VERTEX_POINT ( 'NONE', #33686 ) ;
#60791 = PRESENTATION_LAYER_ASSIGNMENT (  '', '', ( #38422 ) ) ;
#60792 = CARTESIAN_POINT ( 'NONE',  ( 30.99999999999998579, 5.000000000000000000, -72.00402776293822171 ) ) ;
#60793 = CARTESIAN_POINT ( 'NONE',  ( -8.750000000000001776, 24.99999999999998579, 4.000000000000000000 ) ) ;
#60794 =( NAMED_UNIT ( * ) SI_UNIT ( $, .STERADIAN. ) SOLID_ANGLE_UNIT ( ) );
#60795 = ORIENTED_EDGE ( 'NONE', *, *, #46109, .F. ) ;
#60796 =( GEOMETRIC_REPRESENTATION_CONTEXT ( 3 ) GLOBAL_UNCERTAINTY_ASSIGNED_CONTEXT ( ( #15712 ) ) GLOBAL_UNIT_ASSIGNED_CONTEXT ( ( #60246, #22965, #7126 ) ) REPRESENTATION_CONTEXT ( 'NONE', 'WORKASPACE' ) );
#60797 = ORIENTED_EDGE ( 'NONE', *, *, #51397, .F. ) ;
#60798 = CARTESIAN_POINT ( 'NONE',  ( -20.03990113061529144, 115.4999999999999574, 9.999999999999998224 ) ) ;
#60799 = CARTESIAN_POINT ( 'NONE',  ( -109.1929263765337907, -10.01517768586948698, 6.132527647946031529E-16 ) ) ;
#60800 =( NAMED_UNIT ( * ) PLANE_ANGLE_UNIT ( ) SI_UNIT ( $, .RADIAN. ) );
#60801 = ORIENTED_EDGE ( 'NONE', *, *, #45856, .F. ) ;
#60802 = FILL_AREA_STYLE_COLOUR ( '', #31453 ) ;
#60803 = PRESENTATION_STYLE_ASSIGNMENT (( #54834 ) ) ;
#60804 = CARTESIAN_POINT ( 'NONE',  ( 15.00000000000000000, 8.000000000000000000, -4.000000000000000000 ) ) ;
#60805 = ADVANCED_FACE ( 'NONE', ( #40047 ), #44641, .T. ) ;
#60806 = AXIS2_PLACEMENT_3D ( 'NONE', #4238, #26068, #57046 ) ;
#60807 = CARTESIAN_POINT ( 'NONE',  ( -182.5449999999999875, -7.632228543268600340, -2.479861379858950166 ) ) ;
#60809 = EDGE_CURVE ( 'NONE', #20391, #18094, #62833, .T. ) ;
#60808 = VERTEX_POINT ( 'NONE', #17864 ) ;
#60810 = SURFACE_STYLE_USAGE ( .BOTH. , #26481 ) ;
#60811 = EDGE_CURVE ( 'NONE', #48506, #29677, #25214, .T. ) ;
#60812 = AXIS2_PLACEMENT_3D ( 'NONE', #61713, #2947, #9336 ) ;
#60813 = CIRCLE ( 'NONE', #27112, 0.5000000000000004441 ) ;
#60814 = CARTESIAN_POINT ( 'NONE',  ( 1.804495846578303864, 51.08602766979955589, -2.000000000000000000 ) ) ;
#60815 = DIRECTION ( 'NONE',  ( 1.000000000000000000, -0.000000000000000000, 0.000000000000000000 ) ) ;
#60816 = CARTESIAN_POINT ( 'NONE',  ( 3.432329715542617787, 154.5000000000000284, -8.895958039233530457 ) ) ;
#60817 =( NAMED_UNIT ( * ) SI_UNIT ( $, .STERADIAN. ) SOLID_ANGLE_UNIT ( ) );
#60818 = CARTESIAN_POINT ( 'NONE',  ( 9.827790563157511022E-16, 87.30187232391182306, -8.025000000000000355 ) ) ;
#60819 = ADVANCED_FACE ( 'NONE', ( #24494 ), #51966, .T. ) ;
#60820 = AXIS2_PLACEMENT_3D ( 'NONE', #61659, #62391, #14208 ) ;
#60821 = ADVANCED_FACE ( 'NONE', ( #51600 ), #47416, .F. ) ;
#60822 = CARTESIAN_POINT ( 'NONE',  ( -101.9949999999999903, -6.826472737025113702, 4.959722759717902107 ) ) ;
#60823 = CARTESIAN_POINT ( 'NONE',  ( -3.094860106618434248, 120.9049999999999869, 9.525000000000000355 ) ) ;
#60824 = CARTESIAN_POINT ( 'NONE',  ( -80.39499999999998181, -6.826472737025115478, -4.959722759717899443 ) ) ;
#60825 = AXIS2_PLACEMENT_3D ( 'NONE', #38328, #54783, #14320 ) ;
#60826 = EDGE_CURVE ( 'NONE', #58400, #20552, #14315, .T. ) ;
#60827 = FACE_OUTER_BOUND ( 'NONE', #57776, .T. ) ;
#60829 = EDGE_CURVE ( 'NONE', #63169, #23616, #57915, .T. ) ;
#60828 = VECTOR ( 'NONE', #19434, 1000.000000000000000 ) ;
#60830 = DIRECTION ( 'NONE',  ( -1.000000000000000000, 7.709882115452468306E-16, 0.000000000000000000 ) ) ;
#60831 = UNCERTAINTY_MEASURE_WITH_UNIT (LENGTH_MEASURE( 1.000000000000000082E-05 ), #47089, 'distance_accuracy_value', 'NONE');
#60832 = CARTESIAN_POINT ( 'NONE',  ( 30.75000000000001066, 15.74999999999997513, -3.750000000000000000 ) ) ;
#60833 = CARTESIAN_POINT ( 'NONE',  ( 40.78947368421051323, 108.1536491499103363, -3.000000000000000444 ) ) ;
#60834 = VERTEX_POINT ( 'NONE', #68840 ) ;
#60835 = ADVANCED_FACE ( 'NONE', ( #67426 ), #43063, .F. ) ;
#60836 = CARTESIAN_POINT ( 'NONE',  ( -128.0929263765337964, 3.094860106618433360, 9.524999999999991473 ) ) ;
#60837 = DIRECTION ( 'NONE',  ( 0.000000000000000000, 0.000000000000000000, 1.000000000000000000 ) ) ;
#60838 = CARTESIAN_POINT ( 'NONE',  ( -136.9449999999999932, -9.827790563157499189E-16, -8.024999999999991473 ) ) ;
#60839 = VECTOR ( 'NONE', #37475, 1000.000000000000114 ) ;
#60840 = CIRCLE ( 'NONE', #20443, 4.999999999999999112 ) ;
#60841 = VECTOR ( 'NONE', #68355, 1000.000000000000000 ) ;
#60842 = DIRECTION ( 'NONE',  ( 0.000000000000000000, 0.000000000000000000, -1.000000000000000000 ) ) ;
#60843 = SURFACE_STYLE_FILL_AREA ( #7405 ) ;
#60844 = ORIENTED_EDGE ( 'NONE', *, *, #65445, .T. ) ;
#60845 = ORIENTED_EDGE ( 'NONE', *, *, #69490, .F. ) ;
#60846 = DIRECTION ( 'NONE',  ( -0.000000000000000000, -0.000000000000000000, -1.000000000000000000 ) ) ;
#60847 =( NAMED_UNIT ( * ) SI_UNIT ( $, .STERADIAN. ) SOLID_ANGLE_UNIT ( ) );
#60848 = AXIS2_PLACEMENT_3D ( 'NONE', #10563, #50269, #60122 ) ;
#60849 = CARTESIAN_POINT ( 'NONE',  ( 25.75000000000001066, 21.74999999999998224, 4.000000000000000000 ) ) ;
#60850 = CARTESIAN_POINT ( 'NONE',  ( -130.5570736234661808, -1.166476076187852838E-15, -9.524999999999991473 ) ) ;
#60851 = DIRECTION ( 'NONE',  ( -0.000000000000000000, -0.000000000000000000, 1.000000000000000000 ) ) ;
#60852 = CYLINDRICAL_SURFACE ( 'NONE', #6044, 0.5000000000000004441 ) ;
#60853 = SURFACE_STYLE_USAGE ( .BOTH. , #51612 ) ;
#60854 = ORIENTED_EDGE ( 'NONE', *, *, #45528, .F. ) ;
#60855 = CARTESIAN_POINT ( 'NONE',  ( -139.7049999999999841, 2.607480562269072433, 8.024999999999991473 ) ) ;
#60856 = ORIENTED_EDGE ( 'NONE', *, *, #59726, .F. ) ;
#60857 = ORIENTED_EDGE ( 'NONE', *, *, #7483, .T. ) ;
#60858 = SURFACE_STYLE_USAGE ( .BOTH. , #32067 ) ;
#60859 = CARTESIAN_POINT ( 'NONE',  ( 12.25000000000000355, 30.99999999999998579, 4.000000000000000000 ) ) ;
#60860 = ORIENTED_EDGE ( 'NONE', *, *, #69557, .T. ) ;
#60861 = PRESENTATION_LAYER_ASSIGNMENT (  '', '', ( #41786 ) ) ;
#60862 =( LENGTH_UNIT ( ) NAMED_UNIT ( * ) SI_UNIT ( .MILLI., .METRE. ) );
#60863 = CARTESIAN_POINT ( 'NONE',  ( -3.094860106618432471, 130.5949999999999989, -9.525000000000000355 ) ) ;
#60864 =( NAMED_UNIT ( * ) SI_UNIT ( $, .STERADIAN. ) SOLID_ANGLE_UNIT ( ) );
#60865 = EDGE_CURVE ( 'NONE', #7949, #60935, #34006, .T. ) ;
#60866 = VERTEX_POINT ( 'NONE', #57575 ) ;
#60867 = FILL_AREA_STYLE ('',( #44419 ) ) ;
#60868 = CARTESIAN_POINT ( 'NONE',  ( 5.598654528085809545, 140.2549999999999955, -7.705886871421373741 ) ) ;
#60869 = COLOUR_RGB ( '', 0.31764706, 0.68627451, 0.89019608) ;
#60870 = CARTESIAN_POINT ( 'NONE',  ( -59.30499999999999972, 8.437984349512086979, -1.550032578732815448E-15 ) ) ;
#60871 = ORIENTED_EDGE ( 'NONE', *, *, #60025, .F. ) ;
#60872 = CARTESIAN_POINT ( 'NONE',  ( 8.102448949553181734, 154.5049999999999670, 5.886773742842750679 ) ) ;
#60873 = DIRECTION ( 'NONE',  ( 0.000000000000000000, 0.000000000000000000, -1.000000000000000000 ) ) ;
#60874 = UNCERTAINTY_MEASURE_WITH_UNIT (LENGTH_MEASURE( 1.000000000000000082E-05 ), #9791, 'distance_accuracy_value', 'NONE');
#60875 = AXIS2_PLACEMENT_3D ( 'NONE', #36869, #58284, #10113 ) ;
#60876 = DIRECTION ( 'NONE',  ( -0.000000000000000000, 1.000000000000000000, -0.000000000000000000 ) ) ;
#60877 = SURFACE_STYLE_FILL_AREA ( #19711 ) ;
#60878 = SURFACE_SIDE_STYLE ('',( #66520 ) ) ;
#60879 = VERTEX_POINT ( 'NONE', #13968 ) ;
#60880 = AXIS2_PLACEMENT_3D ( 'NONE', #8000, #29450, #50925 ) ;
#60881 = ORIENTED_EDGE ( 'NONE', *, *, #53695, .F. ) ;
#60882 = CARTESIAN_POINT ( 'NONE',  ( -121.5570736234661808, -1.166476076187852838E-15, -9.524999999999991473 ) ) ;
#60883 = SURFACE_STYLE_USAGE ( .BOTH. , #1759 ) ;
#60884 = CARTESIAN_POINT ( 'NONE',  ( -157.7049999999999557, 2.607480562269073321, 8.024999999999991473 ) ) ;
#60886 = EDGE_LOOP ( 'NONE', ( #13043, #4373, #19821, #4660 ) ) ;
#60885 = CIRCLE ( 'NONE', #9245, 0.5000000000000004441 ) ;
#60887 = DIRECTION ( 'NONE',  ( 0.000000000000000000, 1.000000000000000000, -0.000000000000000000 ) ) ;
#60888 = UNCERTAINTY_MEASURE_WITH_UNIT (LENGTH_MEASURE( 1.000000000000000082E-05 ), #23417, 'distance_accuracy_value', 'NONE');
#60889 = VECTOR ( 'NONE', #47272, 1000.000000000000000 ) ;
#60890 = CARTESIAN_POINT ( 'NONE',  ( -184.0000000000000000, -7.358988424933670558, 3.200923985616050071 ) ) ;
#60891 = DIRECTION ( 'NONE',  ( 0.000000000000000000, 0.000000000000000000, -1.000000000000000000 ) ) ;
#60892 = FILL_AREA_STYLE ('',( #2086 ) ) ;
#60893 = ORIENTED_EDGE ( 'NONE', *, *, #46096, .T. ) ;
#60894 = VERTEX_POINT ( 'NONE', #31164 ) ;
#60895 = CARTESIAN_POINT ( 'NONE',  ( -44.99310882439082349, 9.606342690214754398, -3.226428160770427489 ) ) ;
#60896 = DIRECTION ( 'NONE',  ( 0.000000000000000000, 0.000000000000000000, 1.000000000000000000 ) ) ;
#60897 = CARTESIAN_POINT ( 'NONE',  ( -73.70499999999998408, 2.607480562269073321, 8.024999999999991473 ) ) ;
#60898 = EDGE_LOOP ( 'NONE', ( #35693, #58453, #36491 ) ) ;
#60899 = EDGE_CURVE ( 'NONE', #24199, #2488, #58126, .T. ) ;
#60900 =( NAMED_UNIT ( * ) SI_UNIT ( $, .STERADIAN. ) SOLID_ANGLE_UNIT ( ) );
#60901 = CARTESIAN_POINT ( 'NONE',  ( -45.91547277936962246, 9.430195807687219656, -6.500000000000000000 ) ) ;
#60902 = ADVANCED_FACE ( 'NONE', ( #25896 ), #43862, .T. ) ;
#60903 = AXIS2_PLACEMENT_3D ( 'NONE', #40602, #41650, #8916 ) ;
#60904 = CARTESIAN_POINT ( 'NONE',  ( 0.000000000000000000, 18.74999999999997868, 3.750000000000000000 ) ) ;
#60905 = ORIENTED_EDGE ( 'NONE', *, *, #68710, .F. ) ;
#60906 =( LENGTH_UNIT ( ) NAMED_UNIT ( * ) SI_UNIT ( .MILLI., .METRE. ) );
#60907 = VECTOR ( 'NONE', #8220, 1000.000000000000000 ) ;
#60909 = SURFACE_STYLE_USAGE ( .BOTH. , #18011 ) ;
#60908 = CARTESIAN_POINT ( 'NONE',  ( 66.24999999999998579, 33.74999999999999289, -4.000000000000000000 ) ) ;
#60910 = B_SPLINE_CURVE_WITH_KNOTS ( 'NONE', 3,
 ( #59061, #4542, #9852, #53771, #15489, #5572 ),
 .UNSPECIFIED., .F., .F.,
 ( 4, 2, 4 ),
 ( 0.005386537104126975541, 0.008060814333094815098, 0.01073509156206265379 ),
 .UNSPECIFIED. ) ;
#60911 = CARTESIAN_POINT ( 'NONE',  ( 9.058813317711338797, 135.8449999999999989, -2.943386871421372675 ) ) ;
#60912 = CARTESIAN_POINT ( 'NONE',  ( -105.7449999999999903, 4.716976649647094177, 6.492361379858945902 ) ) ;
#60913 = EDGE_CURVE ( 'NONE', #51672, #47453, #38441, .T. ) ;
#60914 = CIRCLE ( 'NONE', #57564, 0.2500000000000002220 ) ;
#60916 = CARTESIAN_POINT ( 'NONE',  ( -18.76341613659756646, 11.53760461768462697, 3.307647553967739018 ) ) ;
#60915 = CARTESIAN_POINT ( 'NONE',  ( -97.55707362346618083, -1.166476076187852838E-15, -9.524999999999991473 ) ) ;
#60917 = ADVANCED_FACE ( 'NONE', ( #10778 ), #53352, .T. ) ;
#60918 = CARTESIAN_POINT ( 'NONE',  ( -151.3429263765337964, -9.058813317711329915, 2.943386871421371787 ) ) ;
#60919 =( LENGTH_UNIT ( ) NAMED_UNIT ( * ) SI_UNIT ( .MILLI., .METRE. ) );
#60920 = CARTESIAN_POINT ( 'NONE',  ( -166.6449999999999818, 4.716976649647091513, -6.492361379858946790 ) ) ;
#60921 = CIRCLE ( 'NONE', #48630, 10.50000000000000178 ) ;
#60922 = SURFACE_STYLE_FILL_AREA ( #7807 ) ;
#60923 = MECHANICAL_DESIGN_GEOMETRIC_PRESENTATION_REPRESENTATION (  '', ( #44119 ), #31712 ) ;
#60924 = SURFACE_STYLE_FILL_AREA ( #13794 ) ;
#60925 = ORIENTED_EDGE ( 'NONE', *, *, #46904, .F. ) ;
#60926 = DIRECTION ( 'NONE',  ( 0.000000000000000000, 0.000000000000000000, 1.000000000000000000 ) ) ;
#60927 = ORIENTED_EDGE ( 'NONE', *, *, #34454, .F. ) ;
#60928 = CARTESIAN_POINT ( 'NONE',  ( -69.59292637653381064, -3.094860106618431139, -9.524999999999991473 ) ) ;
#60929 =( LENGTH_UNIT ( ) NAMED_UNIT ( * ) SI_UNIT ( .MILLI., .METRE. ) );
#60930 = CARTESIAN_POINT ( 'NONE',  ( 0.000000000000000000, 2.500000000000000000, 0.000000000000000000 ) ) ;
#60931 = DIRECTION ( 'NONE',  ( -1.000000000000000000, 0.000000000000000000, -0.000000000000000000 ) ) ;
#60932 = ORIENTED_EDGE ( 'NONE', *, *, #3664, .T. ) ;
#60933 = CARTESIAN_POINT ( 'NONE',  ( -169.1049999999999898, -6.826472737025113702, 4.959722759717902107 ) ) ;
#60934 =( GEOMETRIC_REPRESENTATION_CONTEXT ( 3 ) GLOBAL_UNCERTAINTY_ASSIGNED_CONTEXT ( ( #62358 ) ) GLOBAL_UNIT_ASSIGNED_CONTEXT ( ( #25013, #57375, #16230 ) ) REPRESENTATION_CONTEXT ( 'NONE', 'WORKASPACE' ) );
#60935 = VERTEX_POINT ( 'NONE', #16767 ) ;
#60936 = CIRCLE ( 'NONE', #9306, 5.000000000000000000 ) ;
#60937 = CARTESIAN_POINT ( 'NONE',  ( -20.29401227849671230, 1.590180419696184400, 12.33230205742959740 ) ) ;
#60938 = CARTESIAN_POINT ( 'NONE',  ( 34.99999999999999289, 118.4999999999999716, 7.500000000000000000 ) ) ;
#60939 = CARTESIAN_POINT ( 'NONE',  ( 8.437984349512095861, 156.3070736234661524, 1.550032578732817026E-15 ) ) ;
#60940 = EDGE_CURVE ( 'NONE', #17236, #69376, #4783, .T. ) ;
#60941 = CIRCLE ( 'NONE', #67701, 0.5000000000000004441 ) ;
#60942 = ORIENTED_EDGE ( 'NONE', *, *, #28655, .F. ) ;
#60943 = CARTESIAN_POINT ( 'NONE',  ( 34.99999999999999289, 99.99999999999998579, 7.500000000000000000 ) ) ;
#60944 = LINE ( 'NONE', #45173, #49667 ) ;
#60945 = CARTESIAN_POINT ( 'NONE',  ( -81.50499999999999545, -6.826472737025113702, -4.959722759717900331 ) ) ;
#60946 = CARTESIAN_POINT ( 'NONE',  ( -2.607480562269041791, 121.2070736234661581, -8.025000000000021672 ) ) ;
#60947 = EDGE_CURVE ( 'NONE', #62177, #51568, #20984, .T. ) ;
#60948 = CARTESIAN_POINT ( 'NONE',  ( -8.102448949553181734, 129.0049999999999670, -5.886773742842749790 ) ) ;
#60949 = UNCERTAINTY_MEASURE_WITH_UNIT (LENGTH_MEASURE( 1.000000000000000082E-05 ), #6648, 'distance_accuracy_value', 'NONE');
#60950 = CIRCLE ( 'NONE', #7042, 9.499999999999994671 ) ;
#60951 =( NAMED_UNIT ( * ) PLANE_ANGLE_UNIT ( ) SI_UNIT ( $, .RADIAN. ) );
#60952 = CARTESIAN_POINT ( 'NONE',  ( -127.3429263765337964, -9.058813317711329915, 2.943386871421371787 ) ) ;
#60953 = DIRECTION ( 'NONE',  ( 1.000000000000000000, 0.000000000000000000, 0.000000000000000000 ) ) ;
#60954 = DIRECTION ( 'NONE',  ( -0.000000000000000000, -0.000000000000000000, 1.000000000000000000 ) ) ;
#60955 = SURFACE_STYLE_FILL_AREA ( #17734 ) ;
#60956 = ORIENTED_EDGE ( 'NONE', *, *, #69561, .F. ) ;
#60957 = VECTOR ( 'NONE', #34640, 1000.000000000000000 ) ;
#60958 = FILL_AREA_STYLE ('',( #31895 ) ) ;
#60959 = DIRECTION ( 'NONE',  ( 0.000000000000000000, 0.000000000000000000, 1.000000000000000000 ) ) ;
#60960 = CARTESIAN_POINT ( 'NONE',  ( -50.99499999999999034, -6.826472737025115478, 4.959722759717900331 ) ) ;
#60961 = ORIENTED_EDGE ( 'NONE', *, *, #60054, .T. ) ;
#60962 = DIRECTION ( 'NONE',  ( -1.000000000000000000, -0.000000000000000000, -0.000000000000000000 ) ) ;
#60963 = AXIS2_PLACEMENT_3D ( 'NONE', #28775, #50259, #1981 ) ;
#60964 = CARTESIAN_POINT ( 'NONE',  ( -139.1070736234661638, 8.102448949553172852, -5.886773742842744461 ) ) ;
#60965 = CARTESIAN_POINT ( 'NONE',  ( -8.921435019309294474E-16, -7.500000000000000888, 1.000000000000000000 ) ) ;
#60966 = ORIENTED_EDGE ( 'NONE', *, *, #55402, .F. ) ;
#60967 = CARTESIAN_POINT ( 'NONE',  ( -51.08064578546113665, -11.94071241913273518, 3.088929465764277627 ) ) ;
#60968 = CARTESIAN_POINT ( 'NONE',  ( -54.59499999999997044, 2.607480562269072433, 8.024999999999991473 ) ) ;
#60969 = EDGE_LOOP ( 'NONE', ( #8647, #31881, #55664 ) ) ;
#60970 = MECHANICAL_DESIGN_GEOMETRIC_PRESENTATION_REPRESENTATION (  '', ( #12665 ), #8175 ) ;
#60971 = EDGE_CURVE ( 'NONE', #36334, #8511, #26250, .T. ) ;
#60972 = CARTESIAN_POINT ( 'NONE',  ( -74.13368340934296441, 9.243037840626097790, 6.242508038240137225 ) ) ;
#60973 = CARTESIAN_POINT ( 'NONE',  ( -116.9050000000000011, 2.607480562269068880, -8.024999999999993250 ) ) ;
#60974 = ORIENTED_EDGE ( 'NONE', *, *, #41366, .F. ) ;
#60975 = EDGE_CURVE ( 'NONE', #18052, #57872, #42833, .T. ) ;
#60977 = AXIS2_PLACEMENT_3D ( 'NONE', #16188, #52769, #4544 ) ;
#60976 = FILL_AREA_STYLE_COLOUR ( '', #35055 ) ;
#60978 = CARTESIAN_POINT ( 'NONE',  ( 32.00000000000001421, 15.00000000000000000, -35.50000000000000000 ) ) ;
#60979 = CARTESIAN_POINT ( 'NONE',  ( 4.250000000000001776, 22.24999999999998579, -4.000000000000000000 ) ) ;
#60980 = CARTESIAN_POINT ( 'NONE',  ( -152.0070736234661695, -8.102448949553172852, -5.886773742842741797 ) ) ;
#60981 = CARTESIAN_POINT ( 'NONE',  ( -20.57648123223228254, 154.9999999999999716, 10.27659574468085069 ) ) ;
#60982 = CARTESIAN_POINT ( 'NONE',  ( -9.058813317711338797, 146.3449999999999989, 2.943386871421373563 ) ) ;
#60983 = CARTESIAN_POINT ( 'NONE',  ( -89.00707362346618368, -8.102448949553172852, -5.886773742842741797 ) ) ;
#60984 = AXIS2_PLACEMENT_3D ( 'NONE', #68609, #10211, #69302 ) ;
#60985 = ADVANCED_FACE ( 'NONE', ( #58611 ), #20516, .F. ) ;
#60986 = ORIENTED_EDGE ( 'NONE', *, *, #61166, .T. ) ;
#60987 =( NAMED_UNIT ( * ) PLANE_ANGLE_UNIT ( ) SI_UNIT ( $, .RADIAN. ) );
#60988 = EDGE_CURVE ( 'NONE', #31359, #58413, #47779, .T. ) ;
#60989 = SURFACE_STYLE_FILL_AREA ( #18097 ) ;
#60991 = PRESENTATION_LAYER_ASSIGNMENT (  '', '', ( #21680 ) ) ;
#60990 = SURFACE_STYLE_USAGE ( .BOTH. , #44533 ) ;
#60992 = CARTESIAN_POINT ( 'NONE',  ( -135.5049999999999670, -6.826472737025115478, -4.959722759717899443 ) ) ;
#60993 = DIRECTION ( 'NONE',  ( -1.300977106640434891E-16, 0.000000000000000000, -1.000000000000000000 ) ) ;
#60994 = CARTESIAN_POINT ( 'NONE',  ( -147.1429263765338078, 5.598654528085800663, -7.705886871421367523 ) ) ;
#60995 = MECHANICAL_DESIGN_GEOMETRIC_PRESENTATION_REPRESENTATION (  '', ( #12692 ), #55385 ) ;
#60996 = FILL_AREA_STYLE ('',( #796 ) ) ;
#60997 = CARTESIAN_POINT ( 'NONE',  ( -140.2450000000000045, -4.716976649647093289, -6.492361379858945902 ) ) ;
#60998 = ADVANCED_FACE ( 'NONE', ( #10440 ), #17175, .F. ) ;
#60999 = CARTESIAN_POINT ( 'NONE',  ( -129.4449999999999648, 0.000000000000000000, 8.024999999999991473 ) ) ;
#61000 = DIRECTION ( 'NONE',  ( -0.000000000000000000, -0.000000000000000000, -1.000000000000000000 ) ) ;
#61001 = EDGE_LOOP ( 'NONE', ( #63402, #39666, #55781, #38269 ) ) ;
#61002 = CARTESIAN_POINT ( 'NONE',  ( 13.75000000000000533, 30.74999999999999289, 4.000000000000000000 ) ) ;
#61003 = AXIS2_PLACEMENT_3D ( 'NONE', #46158, #9557, #58409 ) ;
#61004 = SURFACE_STYLE_FILL_AREA ( #33251 ) ;
#61005 = CARTESIAN_POINT ( 'NONE',  ( -120.8929263765338078, -8.102448949553174629, -5.886773742842741797 ) ) ;
#61006 = ADVANCED_FACE ( 'NONE', ( #31870 ), #33274, .T. ) ;
#61007 = CARTESIAN_POINT ( 'NONE',  ( -184.0429263765338135, -9.058813317711329915, -2.943386871421370898 ) ) ;
#61008 =( LENGTH_UNIT ( ) NAMED_UNIT ( * ) SI_UNIT ( .MILLI., .METRE. ) );
#61009 = CARTESIAN_POINT ( 'NONE',  ( -47.54499999999997328, -7.632228543268600340, -2.479861379858950166 ) ) ;
#61010 = DIRECTION ( 'NONE',  ( 0.000000000000000000, 1.000000000000000000, 0.000000000000000000 ) ) ;
#61011 = CARTESIAN_POINT ( 'NONE',  ( 62.24999999999998579, 33.74999999999999289, -3.750000000000000000 ) ) ;
#61012 = PRESENTATION_LAYER_ASSIGNMENT (  '', '', ( #21707 ) ) ;
#61013 = COLOUR_RGB ( '', 0.09019608, 0.27058824, 0.51372549) ;
#61014 = CARTESIAN_POINT ( 'NONE',  ( -24.21231517720798010, 113.4999999999999858, 7.500000000000000000 ) ) ;
#61015 = SPHERICAL_SURFACE ( 'NONE', #14773, 0.5000000000000000000 ) ;
#61016 = CARTESIAN_POINT ( 'NONE',  ( -98.84292637653379643, 9.058813317711329915, -2.943386871421373119 ) ) ;
#61017 = APPLICATION_PROTOCOL_DEFINITION ( 'draft international standard', 'automotive_design', 1998, #58591 ) ;
#61018 = DIRECTION ( 'NONE',  ( -1.000000000000000000, 0.000000000000000000, 0.000000000000000000 ) ) ;
#61019 =( NAMED_UNIT ( * ) SI_UNIT ( $, .STERADIAN. ) SOLID_ANGLE_UNIT ( ) );
#61020 = STYLED_ITEM ( 'NONE', ( #24714 ), #46922 ) ;
#61021 = DIRECTION ( 'NONE',  ( 0.000000000000000000, 0.000000000000000000, 1.000000000000000000 ) ) ;
#61022 = CARTESIAN_POINT ( 'NONE',  ( -41.13907225104363619, 107.8972693614176137, 3.376186789259631560 ) ) ;
#61023 = VERTEX_POINT ( 'NONE', #45246 ) ;
#61024 = DIRECTION ( 'NONE',  ( 1.000000000000000000, 0.000000000000000000, -1.300977106640434891E-16 ) ) ;
#61025 = FILL_AREA_STYLE ('',( #12844 ) ) ;
#61026 = CARTESIAN_POINT ( 'NONE',  ( 0.000000000000000000, 110.5741857357814553, -9.450814264218539762 ) ) ;
#61027 = VERTEX_POINT ( 'NONE', #61026 ) ;
#61028 =( LENGTH_UNIT ( ) NAMED_UNIT ( * ) SI_UNIT ( .MILLI., .METRE. ) );
#61029 = MECHANICAL_DESIGN_GEOMETRIC_PRESENTATION_REPRESENTATION (  '', ( #27322 ), #1530 ) ;
#61030 = CARTESIAN_POINT ( 'NONE',  ( 7.632228543268608334, 126.4570736234661723, -2.479861379858951942 ) ) ;
#61031 = EDGE_CURVE ( 'NONE', #58716, #25360, #10070, .T. ) ;
#61032 = CARTESIAN_POINT ( 'NONE',  ( 21.02379604162863913, 114.9999999999999574, -10.00000000000000000 ) ) ;
#61033 = VECTOR ( 'NONE', #906, 1000.000000000000000 ) ;
#61034 = ORIENTED_EDGE ( 'NONE', *, *, #20827, .F. ) ;
#61035 = CARTESIAN_POINT ( 'NONE',  ( -8.750000000000001776, 25.24999999999998934, 3.750000000000000000 ) ) ;
#61036 = AXIS2_PLACEMENT_3D ( 'NONE', #40046, #61110, #12212 ) ;
#61037 = PRESENTATION_STYLE_ASSIGNMENT (( #32944 ) ) ;
#61038 = CARTESIAN_POINT ( 'NONE',  ( 10.00000000000000711, 50.00000000000000000, -59.99999999999999289 ) ) ;
#61039 = FILL_AREA_STYLE_COLOUR ( '', #52191 ) ;
#61040 = FILL_AREA_STYLE ('',( #39629 ) ) ;
#61041 = CARTESIAN_POINT ( 'NONE',  ( -83.69499999999997897, -8.437984349512085203, 5.166775262442717831E-16 ) ) ;
#61042 = ORIENTED_EDGE ( 'NONE', *, *, #53929, .T. ) ;
#61043 = VECTOR ( 'NONE', #58661, 1000.000000000000000 ) ;
#61044 = CARTESIAN_POINT ( 'NONE',  ( 31.00000000000000355, 42.00000000000000000, -75.00000000000001421 ) ) ;
#61045 = EDGE_CURVE ( 'NONE', #9417, #61535, #65271, .T. ) ;
#61046 = DIRECTION ( 'NONE',  ( -0.000000000000000000, 0.000000000000000000, 1.000000000000000000 ) ) ;
#61047 = FILL_AREA_STYLE_COLOUR ( '', #39638 ) ;
#61048 = ORIENTED_EDGE ( 'NONE', *, *, #67414, .F. ) ;
#61049 = SURFACE_SIDE_STYLE ('',( #29021 ) ) ;
#61050 = FACE_OUTER_BOUND ( 'NONE', #28778, .T. ) ;
#61051 = EDGE_CURVE ( 'NONE', #2459, #26491, #65450, .T. ) ;
#61052 = B_SPLINE_CURVE_WITH_KNOTS ( 'NONE', 3,
 ( #9647, #35671, #20156, #46619, #8929, #25446, #51159, #3602 ),
 .UNSPECIFIED., .F., .F.,
 ( 4, 2, 2, 4 ),
 ( 2.544316211735811779E-07, 0.002094919859796806009, 0.003142252573884622008, 0.004189585287972438440 ),
 .UNSPECIFIED. ) ;
#61053 = ADVANCED_FACE ( 'NONE', ( #1884 ), #35116, .F. ) ;
#61055 = DIRECTION ( 'NONE',  ( -0.000000000000000000, -1.000000000000000000, 0.000000000000000000 ) ) ;
#61054 = VECTOR ( 'NONE', #24249, 1000.000000000000000 ) ;
#61056 = ORIENTED_EDGE ( 'NONE', *, *, #20150, .F. ) ;
#61057 = EDGE_CURVE ( 'NONE', #15830, #39204, #33608, .T. ) ;
#61058 = ORIENTED_EDGE ( 'NONE', *, *, #55603, .T. ) ;
#61059 = DIRECTION ( 'NONE',  ( 0.000000000000000000, 0.000000000000000000, 1.000000000000000000 ) ) ;
#61060 = CARTESIAN_POINT ( 'NONE',  ( 1.000000000000000000, 42.00000000000000000, 79.00402776293826435 ) ) ;
#61061 = DIRECTION ( 'NONE',  ( 1.000000000000000000, 0.000000000000000000, -0.000000000000000000 ) ) ;
#61062 = DIRECTION ( 'NONE',  ( 0.000000000000000000, 1.000000000000000000, 0.000000000000000000 ) ) ;
#61063 = AXIS2_PLACEMENT_3D ( 'NONE', #55128, #22450, #65361 ) ;
#61064 = PRESENTATION_LAYER_ASSIGNMENT (  '', '', ( #13875 ) ) ;
#61065 = CARTESIAN_POINT ( 'NONE',  ( -175.7070736234662149, -3.094860106618431139, -9.524999999999991473 ) ) ;
#61066 = CARTESIAN_POINT ( 'NONE',  ( -3.094860106618434248, 110.7949999999999733, 9.525000000000000355 ) ) ;
#61067 = CARTESIAN_POINT ( 'NONE',  ( -118.1070736234661780, 8.102448949553171076, -5.886773742842744461 ) ) ;
#61068 = CIRCLE ( 'NONE', #66708, 27.49999999999999645 ) ;
#61069 = CIRCLE ( 'NONE', #46527, 23.00000000000000000 ) ;
#61070 = CARTESIAN_POINT ( 'NONE',  ( -0.7087670488515470657, 2.466410156631316131, 7.000000000000000000 ) ) ;
#61071 = DIRECTION ( 'NONE',  ( -0.000000000000000000, -1.000000000000000000, -0.000000000000000000 ) ) ;
#61072 = VERTEX_POINT ( 'NONE', #1548 ) ;
#61073 = LINE ( 'NONE', #60716, #39641 ) ;
#61074 = CYLINDRICAL_SURFACE ( 'NONE', #56817, 0.5000000000000004441 ) ;
#61075 = EDGE_CURVE ( 'NONE', #52813, #8395, #2525, .T. ) ;
#61076 = DIRECTION ( 'NONE',  ( -0.000000000000000000, -0.000000000000000000, -1.000000000000000000 ) ) ;
#61077 = DIRECTION ( 'NONE',  ( 0.000000000000000000, 0.000000000000000000, -1.000000000000000000 ) ) ;
#61078 = ORIENTED_EDGE ( 'NONE', *, *, #2059, .F. ) ;
#61079 = STYLED_ITEM ( 'NONE', ( #61285 ), #37996 ) ;
#61080 = CARTESIAN_POINT ( 'NONE',  ( -155.3050000000000068, 8.437984349512085203, -1.550032578732815448E-15 ) ) ;
#61081 = CARTESIAN_POINT ( 'NONE',  ( 9.000000000000003553, 25.24999999999998934, -3.750000000000000000 ) ) ;
#61082 = DIRECTION ( 'NONE',  ( 0.000000000000000000, 0.000000000000000000, -1.000000000000000000 ) ) ;
#61083 = CARTESIAN_POINT ( 'NONE',  ( -161.2450000000000045, -4.716976649647093289, -6.492361379858945902 ) ) ;
#61084 = VECTOR ( 'NONE', #30086, 1000.000000000000000 ) ;
#61085 = CARTESIAN_POINT ( 'NONE',  ( -161.8449999999999989, -7.632228543268599452, 2.479861379858951054 ) ) ;
#61086 =( BOUNDED_SURFACE ( )  B_SPLINE_SURFACE ( 1, 2, ( 
 ( #68743, #5045, #21210, #26493, #62732, #63449, #42046, #35687, #3990, #20535, #8947, #14566, #57120, #57477, #30725, #52230, #48346, #12041, #22613, #43758, #5369, #21928, #6764, #27163, #38832, #54262, #44117, #33506, #16334, #37811, #17008, #59534, #59181, #11009, #17367, #60247, #6082, #38496, #27848, #65162, #32447, #59892, #53913, #28192, #11353, #5717, #64825, #38, #48698, #65518, #6417, #15984, #49700, #54936, #54610, #21571, #1436, #10678, #42734, #37467, #33177, #401, #27515, #43441, #64491, #64133, #58870, #32130, #16670, #11709, #38135, #32822, #49352, #1072, #49041, #731, #22263, #53583, #26808, #43085, #55303, #23992, #2842, #44800, #29964, #33841, #39872, #23639, #66196, #29254, #18387, #51425, #8174, #22966, #56340, #50386, #24332, #39511, #44466, #28898, #45144, #66563, #17700, #18024, #13084, #55660, #18719, #23301, #13791, #45506, #61276, #65870, #60920, #13425, #19038, #40549, #45826, #12737, #34538, #67250, #8529, #29617, #1790, #66921, #2482, #35247, #34208, #50736, #39168, #50058, #7474, #2112, #61962, #60561, #28553, #56707, #12379, #40193, #7127, #55995, #7805, #61598, #34894, #51090, #52831, #63704, #46545, #67971, #47233, #20086, #19753, #41250, #47599, #69005, #14848, #68654, #58105, #4234, #62646, #20453, #14473, #37025, #41588, #35949, #25378, #30280, #57396, #4608, #36685, #46182, #58433, #20812, #15219, #51781, #15548, #40904, #26065, #67603, #63364, #9220, #36326, #30639, #25036, #3172, #24662, #62323, #46897, #25710, #52146, #3902, #41957, #9915, #68301, #63008, #57751, #19406, #9580, #42318, #35605, #31332, #10259, #30998, #31694, #14144, #52496, #57044, #8860, #3530, #48619, #11971, #38415, #60162, #16929, #10935, #33093, #69674, #53173, #59115, #53835, #27084, #47945, #5290, #43361, #16254, #48961, #53509, #44034, #54182, #4964, #314, #17290, #984, #64403, #43683, #26736, #32370, #32730, #38755, #32047, #26412, #38051, #5995, #69344, #64047, #6340, #42641, #21136, #15895, #59814, #37376, #22187, #48259, #21486, #58783, #64753, #11627, #42998, #16594, #59444, #65442, #37730, #5631, #54531, #659, #10601, #21847, #11276, #27434, #65073, #27771, #49275, #22532, #49979, #67169, #34463, #12296, #23554, #40460, #28471, #6680, #7040, #61879, #18646, #1713, #66479, #60483, #55577, #23230, #18301, #44724, #18957, #2029, #39094, #29162, #23910, #7399, #33428, #40126, #61516, #12654, #39784, #13343, #50650, #39436, #45752, #28828, #2390, #66116, #45422, #45066, #60838, #17945, #54859, #28114, #66843, #34119, #49621, #50998, #34802, #50310, #1358, #61200, #24252, #65791, #13007, #56257, #17626, #55920, #22891, #7726, #29528, #8083, #2763, #44388, #33768, #55217, #8778, #63281, #30913, #62914, #36607, #3810, #46818, #8447, #41504, #3087, #24943, #46455, #25624, #51694, #25295, #47143, #67879, #67513, #41863, #24579, #29881, #35161, #36235, #19672, #46093, #57662, #15129, #41168, #68568, #35857, #68221, #20360, #62570, #19313, #13701, #40816, #62233, #51344, #9490, #14387, #14058, #52409, #56616, #14760, #35519, #4154, #57304, #56965, #30201, #3441, #9134, #19999, #30552, #52055, #37762, #61131, #21516, #347, #39713, #59139, #54216, #64078, #5323, #32402, #5666, #18228, #69374, #53537, #12941, #27800, #48995, #10629, #27114, #34404, #53867, #45001, #59483, #49306, #55857, #43034, #64438, #22217, #64782, #16286, #10964, #22564, #66410, #11310, #43712, #33127, #685, #48648, #65107, #21881, #7658, #16620, #43392, #38086, #26766, #32766, #1016, #11657, #21165, #47975, #42676, #59848, #48292, #15931, #37411, #58814, #32080, #38448, #6032, #27469, #16961, #32688, #54564, #6371, #18582, #3024, #30141, #61801, #45693, #67810, #24875, #24186, #24516, #67109, #23845, #62162, #25233, #61458, #51626, #9071, #50937, #36169, #40069, #46033, #29816, #2694, #35460, #67446, #57599, #14330, #29091, #62514, #56543, #30490, #18894, #50586, #35093, #51281, #19243, #45350, #40393, #40750, #13632, #66768, #2322, #35795, #13995, #13276, #57238, #62853, #56905, #46752, #8715, #8016, #34730, #3381, #46386, #14695, #56188, #51987, #29466, #8382, #19607, #41106, #3740, #68165, #19946, #41443, #63224, #21003, #64248, #47439, #42498, #15742, #21693, #31184, #15411, #10796, #5154, #68505, #31542, #20297, #9426, #58285, #47802, #63893, #160, #25913, #43209, #10460, #57959, #69202, #16458, #4444, #52346, #52678, #37923, #16104, #68861, #37224, #36541, #53023, #20663, #58636, #42174, #64614, #31892, #15069, #26602, #69528, #4815, #30850, #37586, #58983, #10114, #53371, #32244, #48123, #36870, #4096, #26268, #21331, #63565, #42854, #53692, #5479, #26929, #25565, #47078, #48465, #41805, #9775, #7255, #23089, #11822, #59297, #65641, #50174, #22044, #38951, #6893, #43548, #27970, #48822, #1208, #55430, #49824, #44581, #33294, #64934, #1566, #49145, #44919, #39287, #65980, #18150, #60353, #12156, #5842, #28320, #16788, #17140, #38612, #28681, #43885, #33626, #1898, #60012, #38260, #23408, #517, #32574, #17809, #65292, #11125, #66326, #60690, #54719, #54036, #17484, #27281, #59659, #55067, #12502, #11478, #49477, #32949, #22739, #54382, #33969, #6205, #6525, #27634, #841, #22381, #44237, #19523, #30070, #68091, #19165, #62079, #55780, #8642, #2236, #67037, #18828, #35721, #24115, #40668, #57153, #40310, #66687, #51905, #50509, #7586, #61041, #3303, #13547, #23763, #24791, #3661, #35015, #8987, #29744, #18503, #12864, #24441, #13913, #25157, #45268, #62444, #29015, #39630, #39988, #45619, #14258, #46671, #61386, #34653, #13201, #51209, #46306, #7934, #2951, #45945, #34329, #56112, #61719, #41026, #35379, #29376, #56466, #50856, #2614, #8303, #67372, #56834, #30402, #51539, #67728, #20932, #68420, #10032, #26849, #14980, #62770, #63140, #48386, #5083, #57880, #52945, #47008, #42092, #36458, #4732, #9701, #5408, #58210, #25493, #15662, #10387, #63490, #53620, #26534, #48052, #68781, #26183, #69458, #37144, #25842, #32170, #15340, #58552, #31109, #31810, #31456, #47351, #4357, #19870, #52610, #20575, #63819, #36796, #47725, #69125, #64168, #16026, #42428, #53292, #21245, #42776, #37503, #58908, #10716, #41367, #14608, #36074, #57517, #20215, #9343, #30769, #52270, #4027, #41715, #17737, #12080, #48740, #12420, #37847, #23009, #64533, #60282, #54305, #11745, #16711, #21974, #76, #21608, #59219, #43798, #1118, #32865, #38176, #38873, #65558, #64858, #65206, #59578, #16375, #33214, #65909, #32491, #22655, #49741, #43478, #7172, #11045, #17057, #763, #11395, #6455, #38538, #28599, #54980, #43122, #33551, #27559, #1479, #6126, #53951, #49079, #22299, #59929, #5752, #54652, #27890, #49393, #17407, #442, #60607, #44161, #27202, #6806, #33882, #39208, #28232, #44505, #55348, #29298, #29665, #14188, #50777, #57080, #45185, #40589, #46227, #67647, #3219, #50427, #24034, #51463, #35645, #39908, #62366, #23684, #2527, #40946, #61314, #56384, #66244, #7511, #34576, #7846, #19446, #1827, #55704, #8902, #30000, #51132, #12779, #45541, #50098, #56031, #23337, #61639, #24707, #44839, #18069, #2879, #28935, #40235, #39554, #66607, #60960, #18423, #34248, #35295, #13125, #13467, #2152, #66961, #18757, #34937, #8218, #24369, #45863, #67297, #19084, #62004, #13833, #56754, #8568, #15589, #9622, #15258, #37065, #47639, #36378, #42693, #25760, #69046, #20127, #42358 ),
 ( #62687, #63742, #41636, #15945, #10303, #20855, #58826, #9954, #52873, #46589, #58478, #14515, #57795, #31040, #26458, #14897, #31374, #47986, #52534, #57441, #64092, #41291, #68012, #51827, #31732, #4279, #35992, #53217, #37426, #47276, #69386, #20497, #9267, #3575, #36726, #4652, #30326, #30683, #5004, #19800, #25081, #52187, #68698, #21176, #3949, #25422, #46937, #68345, #42006, #63054, #63413, #58142, #26105, #22936, #32417, #16634, #12017, #6386, #6832, #32782, #21534, #10642, #59497, #49004, #65123, #1411, #27129, #699, #43403, #27815, #10980, #44436, #11670, #39139, #6046, #65837, #28154, #21895, #1033, #53881, #11322, #59861, #17670, #54227, #32093, #5679, #22577, #6728, #49666, #33476, #48664, #27482, #54901, #53551, #365, #5337, #64794, #22228, #26779, #38100, #16972, #48306, #37772, #43724, #38461, #43046, #64453, #16300, #59152, #60209, #33142, #54578, #49319, #44081, #65483, #17335, #38796, #40512, #51387, #34174, #55628, #34852, #7768, #7447, #28870, #35210, #56669, #2444, #56303, #45795, #61563, #8137, #1760, #28524, #50353, #23954, #2080, #46142, #29215, #66165, #29579, #51050, #34510, #24626, #67215, #19003, #39833, #45468, #61925, #2809, #66528, #3133, #55962, #24297, #23609, #13750, #66887, #18351, #45113, #60529, #33811, #8494, #61246, #12342, #29927, #67565, #13055, #55264, #18691, #19362, #23271, #40168, #7093, #44767, #50699, #50023, #13391, #17990, #39480, #60884, #12699, #3492, #52792, #30601, #26373, #20774, #31293, #69306, #20410, #63327, #57007, #9877, #24993, #68268, #20047, #36288, #4565, #52108, #26020, #52456, #41547, #25342, #40866, #14110, #47553, #46863, #62286, #58391, #68967, #62963, #35567, #47194, #31653, #46502, #41914, #58066, #67932, #9542, #30244, #4201, #36979, #42283, #63668, #14807, #19722, #15512, #3860, #47908, #10215, #53133, #8819, #15181, #36647, #51747, #4920, #41215, #57710, #30958, #62614, #25673, #14430, #35905, #68613, #57354, #9185, #32002, #58744, #42600, #54489, #64714, #53471, #6300, #54818, #16555, #17250, #11237, #69630, #64007, #5950, #22143, #6628, #5254, #43987, #10561, #21102, #37335, #27040, #65402, #28070, #21441, #16210, #26701, #32684, #27731, #59083, #54137, #27395, #33389, #42959, #48575, #22492, #16892, #48221, #43320, #64361, #15854, #271, #59402, #48926, #11935, #37685, #49581, #43641, #10899, #624, #32340, #53792, #5594, #21805, #38016, #49234, #65031, #38370, #59772, #11578, #33053, #939, #38714, #60120, #39734, #7001, #66792, #61474, #45023, #35117, #56209, #8037, #50267, #55877, #29488, #18608, #7359, #13654, #28421, #40085, #13297, #66430, #56565, #50955, #2715, #1989, #7678, #24207, #34752, #28786, #8399, #18248, #45714, #60788, #67126, #12964, #23509, #55534, #1314, #44343, #18914, #61155, #22846, #40412, #61822, #34422, #65744, #29113, #29834, #33719, #50605, #17586, #55167, #2343, #60448, #23865, #39052, #12254, #49933, #45372, #1671, #23190, #12610, #44681, #66077, #17904, #39389, #34077, #4114, #67467, #20318, #14012, #9091, #30507, #48397, #35815, #30869, #88, #52007, #8733, #64545, #62185, #19263, #3042, #16035, #25252, #35475, #37515, #16386, #46773, #21618, #41461, #30163, #24536, #36191, #52364, #37861, #56920, #5415, #40772, #51302, #51645, #57258, #26858, #59229, #3401, #46407, #24894, #62868, #58921, #19627, #14714, #57618, #11057, #67831, #3761, #53630, #47097, #41126, #68183, #62531, #46050, #19961, #9438, #25580, #43134, #14346, #68520, #41824, #63239, #10729, #32179, #27570, #5765, #6139, #39570, #17750, #65220, #28243, #43487, #453, #49088, #65569, #776, #18082, #1132, #60973, #27900, #66254, #50111, #43810, #23021, #22315, #11758, #12092, #32501, #33225, #53964, #17069, #44517, #28612, #1839, #55361, #32878, #6466, #33896, #27213, #38548, #44853, #59940, #54663, #23350, #49409, #38884, #48754, #59589, #22668, #44171, #21985, #64870, #38186, #16724, #12434, #33561, #11408, #17418, #54316, #60294, #54993, #6818, #7187, #49754, #1493, #65921, #39219, #60618, #56045, #7859, #57092, #8914, #24380, #8579, #67658, #2891, #13478, #34953, #29311, #46606, #29676, #50789, #56398, #39923, #45555, #14197, #46239, #55716, #68024, #30337, #24719, #61326, #25091, #50439, #35655, #7523, #3232, #66975, #45877, #2539, #34590, #12793, #34259, #2166, #8231, #13843, #18770, #24049, #51475, #30011, #40247, #51145, #61651, #28949, #67308, #51840, #45199, #35307, #62377, #19095, #19812, #23698, #40600, #62015, #56765, #19458, #40961, #41300, #3587, #66620, #18438, #13137, #42706, #9632, #13, #68712, #63426, #36738, #57452, #14909, #52884, #25772, #58490, #63067, #53561, #63752, #36390, #42018, #42369, #26788, #15271, #21547, #57808, #53228, #58836, #10651, #15958, #31052, #58155, #64104, #48318, #52545, #5346, #4290, #9968, #62701, #47285, #69060, #9274, #20140, #20509, #31386, #32106, #14528, #68357, #36004, #37439, #15604, #25435, #4665, #30692, #26117, #52199, #47652, #3961, #46947, #20866, #37078, #10315, #31741, #5016, #26470, #41647, #47997, #69396, #21185, #28168, #33156, #43735, #65138, #38115, #7105, #59869, #59508, #16983, #375, #6058, #44444, #6741, #16309, #28534, #60542, #54913, #21904, #55281, #10992, #65851, #37786, #33484, #27496, #54590, #11330, #64802, #43058, #64462, #32428, #38474, #44095, #49015, #32795, #12028, #38809, #54239, #11682, #710, #59161, #6396, #39151, #5690, #65493, #22945, #16645, #50035, #53890, #27827, #49328, #22239, #1048, #22593, #1770, #49684, #27144, #1419, #17347, #17684, #60222, #48675, #12356, #33821, #43416, #18000, #45124, #13404, #55974, #19016, #23619, #14122, #24311, #51762, #18703, #57020, #40882, #34520, #13766, #46156, #30262, #66541, #18362, #7457, #34868, #8506, #61257, #56316, #29591, #35581, #39847, #29231, #24639, #40525, #12711, #45478, #34187, #23283, #2458, #61575, #8154, #8834, #13066, #44779, #45808, #2093, #51064, #66177, #7783, #39490, #50712, #60897, #29938, #23966, #61938, #55640, #28879, #66899, #2818, #40177, #50365, #67227, #35225, #56681, #51402, #3149, #67581, #19380, #62300, #52469, #58081, #58405, #20786, #9554, #15867, #68626, #42294, #62980, #15524, #15193, #30972, #57724, #3505, #46518, #63680, #4213, #25008, #21114, #36993, #25684, #67947, #9892, #64019, #35923, #52805, #10229, #57371, #41930, #62627, #36658, #69319, #31667, #53145, #47207, #9198, #4935, #14823, #58757, #26387, #47919, #32015, #4578, #26034, #19732, #42613, #30616, #20428, #63339, #37348, #31307, #47571, #10574, #68981, #52120, #41226, #14445, #3875, #25355, #46876, #68279, #20062, #41563, #36303, #27408, #49596, #43654, #32348, #5265, #38384, #54500, #17599, #64376, #6640, #42972, #53485, #69645, #59415, #16224, #21458, #26714, #17264, #48935, #37697, #38728, #39065, #634, #1327, #65046, #53804, #48233, #59786, #6311, #60460, #59092, #28082, #10912, #5605, #27052, #11248, #22860, #12263, #48588, #287, #21817, #16903, #60133, #43330, #11595, #33066, #65759, #64723, #32696, #54830, #49246, #16567, #5966, #38028, #54152, #22156, #27742, #950, #44355, #22505, #44003, #65416, #11946, #33401, #40784, #28798, #7014, #7369, #62202, #18928, #66444, #29502, #44695, #1683, #50280, #66809, #2002, #19276, #2358, #39402, #50967, #24219, #7693, #67481, #40428, #61841, #12975, #18620, #13669, #2728, #39750, #46064 ) ),
 .UNSPECIFIED., .F., .F., .T. ) 
 B_SPLINE_SURFACE_WITH_KNOTS ( ( 2, 2 ),
 ( 3, 2, 2, 2, 2, 2, 2, 2, 2, 2, 2, 2, 2, 2, 2, 2, 2, 2, 2, 2, 2, 2, 2, 2, 2, 2, 2, 2, 2, 2, 2, 2, 2, 2, 2, 2, 2, 2, 2, 2, 2, 2, 2, 2, 2, 2, 2, 2, 2, 2, 2, 2, 2, 2, 2, 2, 2, 2, 2, 2, 2, 2, 2, 2, 2, 2, 2, 2, 2, 2, 2, 2, 2, 2, 2, 2, 2, 2, 2, 2, 2, 2, 2, 2, 2, 2, 2, 2, 2, 2, 2, 2, 2, 2, 2, 2, 2, 2, 2, 2, 2, 2, 2, 2, 2, 2, 2, 2, 2, 2, 2, 2, 2, 2, 2, 2, 2, 2, 2, 2, 2, 2, 2, 2, 2, 2, 2, 2, 2, 2, 2, 2, 2, 2, 2, 2, 2, 2, 2, 2, 2, 2, 2, 2, 2, 2, 2, 2, 2, 2, 2, 2, 2, 2, 2, 2, 2, 2, 2, 2, 2, 2, 2, 2, 2, 2, 2, 2, 2, 2, 2, 2, 2, 2, 2, 2, 2, 2, 2, 2, 2, 2, 2, 2, 2, 2, 2, 2, 2, 2, 2, 2, 2, 2, 2, 2, 2, 2, 2, 2, 2, 2, 2, 2, 2, 2, 2, 2, 2, 2, 2, 2, 2, 2, 2, 2, 2, 2, 2, 2, 2, 2, 2, 2, 2, 2, 2, 2, 2, 2, 2, 2, 2, 2, 2, 2, 2, 2, 2, 2, 2, 2, 2, 2, 2, 2, 2, 2, 2, 2, 2, 2, 2, 2, 2, 2, 2, 2, 2, 2, 2, 2, 2, 2, 2, 2, 2, 2, 2, 2, 2, 2, 2, 2, 2, 2, 2, 2, 2, 2, 2, 2, 2, 2, 2, 2, 2, 2, 2, 2, 2, 2, 2, 2, 2, 2, 2, 2, 2, 2, 2, 2, 2, 2, 2, 2, 2, 2, 2, 2, 2, 2, 2, 2, 2, 2, 2, 2, 2, 2, 2, 2, 2, 2, 2, 2, 2, 2, 2, 2, 2, 2, 2, 2, 2, 2, 2, 2, 2, 2, 2, 2, 2, 2, 2, 2, 2, 2, 2, 2, 2, 2, 2, 2, 2, 2, 2, 2, 2, 2, 2, 2, 2, 2, 2, 2, 2, 2, 2, 2, 2, 2, 2, 2, 2, 2, 2, 2, 2, 2, 2, 2, 2, 2, 2, 2, 2, 2, 2, 2, 2, 2, 2, 2, 2, 2, 2, 2, 2, 2, 2, 2, 2, 2, 2, 2, 2, 2, 2, 2, 2, 2, 2, 2, 2, 2, 2, 2, 2, 2, 2, 2, 2, 2, 2, 2, 2, 2, 2, 2, 2, 2, 2, 2, 2, 2, 2, 2, 2, 2, 2, 2, 2, 2, 2, 2, 2, 2, 2, 2, 2, 2, 2, 2, 2, 2, 3 ),
 ( 0.000000000000000000, 1.000000000000000000 ),
 ( 0.000000000000000000, 0.002173913043478260896, 0.004347826086956521792, 0.006521739130434782254, 0.008695652173913043584, 0.01086956521739130405, 0.01304347826086956451, 0.01521739130434782671, 0.01739130434782608717, 0.01956521739130434936, 0.02173913043478260809, 0.02391304347826087029, 0.02608695652173912902, 0.02826086956521739121, 0.03043478260869565341, 0.03260869565217391214, 0.03478260869565217434, 0.03695652173913043653, 0.03913043478260869873, 0.04130434782608695399, 0.04347826086956521618, 0.04565217391304347838, 0.04782608695652174058, 0.05000000000000000278, 0.05217391304347825803, 0.05434782608695652023, 0.05652173913043478243, 0.05869565217391304462, 0.06086956521739130682, 0.06304347826086956208, 0.06521739130434782428, 0.06739130434782608647, 0.06956521739130434867, 0.07173913043478261087, 0.07391304347826087306, 0.07608695652173913526, 0.07826086956521739746, 0.08043478260869564578, 0.08260869565217390798, 0.08478260869565217017, 0.08695652173913043237, 0.08913043478260869457, 0.09130434782608695676, 0.09347826086956521896, 0.09565217391304348116, 0.09782608695652174335, 0.1000000000000000056, 0.1021739130434782677, 0.1043478260869565161, 0.1065217391304347783, 0.1086956521739130405, 0.1108695652173913027, 0.1130434782608695649, 0.1152173913043478271, 0.1173913043478260892, 0.1195652173913043514, 0.1217391304347826136, 0.1239130434782608758, 0.1260869565217391242, 0.1282608695652174002, 0.1304347826086956486, 0.1326086956521739246, 0.1347826086956521729, 0.1369565217391304213, 0.1391304347826086973, 0.1413043478260869457, 0.1434782608695652217, 0.1456521739130434701, 0.1478260869565217461, 0.1499999999999999944, 0.1521739130434782705, 0.1543478260869565188, 0.1565217391304347949, 0.1586956521739130432, 0.1608695652173912916, 0.1630434782608695676, 0.1652173913043478160, 0.1673913043478260920, 0.1695652173913043403, 0.1717391304347826164, 0.1739130434782608647, 0.1760869565217391408, 0.1782608695652173891, 0.1804347826086956652, 0.1826086956521739135, 0.1847826086956521618, 0.1869565217391304379, 0.1891304347826086862, 0.1913043478260869623, 0.1934782608695652106, 0.1956521739130434867, 0.1978260869565217350, 0.2000000000000000111, 0.2021739130434782594, 0.2043478260869565355, 0.2065217391304347838, 0.2086956521739130321, 0.2108695652173913082, 0.2130434782608695565, 0.2152173913043478326, 0.2173913043478260809, 0.2195652173913043570, 0.2217391304347826053, 0.2239130434782608814, 0.2260869565217391297, 0.2282608695652173780, 0.2304347826086956541, 0.2326086956521739024, 0.2347826086956521785, 0.2369565217391304268, 0.2391304347826087029, 0.2413043478260869512, 0.2434782608695652273, 0.2456521739130434756, 0.2478260869565217517, 0.2500000000000000000, 0.2521739130434782483, 0.2543478260869564966, 0.2565217391304348005, 0.2586956521739130488, 0.2608695652173912971, 0.2630434782608695454, 0.2652173913043478493, 0.2673913043478260976, 0.2695652173913043459, 0.2717391304347825942, 0.2739130434782608425, 0.2760869565217391464, 0.2782608695652173947, 0.2804347826086956430, 0.2826086956521738913, 0.2847826086956521952, 0.2869565217391304435, 0.2891304347826086918, 0.2913043478260869401, 0.2934782608695652439, 0.2956521739130434923, 0.2978260869565217406, 0.2999999999999999889, 0.3021739130434782372, 0.3043478260869565410, 0.3065217391304347894, 0.3086956521739130377, 0.3108695652173912860, 0.3130434782608695898, 0.3152173913043478382, 0.3173913043478260865, 0.3195652173913043348, 0.3217391304347825831, 0.3239130434782608869, 0.3260869565217391353, 0.3282608695652173836, 0.3304347826086956319, 0.3326086956521739357, 0.3347826086956521840, 0.3369565217391304324, 0.3391304347826086807, 0.3413043478260869290, 0.3434782608695652328, 0.3456521739130434812, 0.3478260869565217295, 0.3499999999999999778, 0.3521739130434782816, 0.3543478260869565299, 0.3565217391304347783, 0.3586956521739130266, 0.3608695652173913304, 0.3630434782608695787, 0.3652173913043478271, 0.3673913043478260754, 0.3695652173913043237, 0.3717391304347826275, 0.3739130434782608758, 0.3760869565217391242, 0.3782608695652173725, 0.3804347826086956763, 0.3826086956521739246, 0.3847826086956521729, 0.3869565217391304213, 0.3891304347826086696, 0.3913043478260869734, 0.3934782608695652217, 0.3956521739130434701, 0.3978260869565217184, 0.4000000000000000222, 0.4021739130434782705, 0.4043478260869565188, 0.4065217391304347672, 0.4086956521739130710, 0.4108695652173913193, 0.4130434782608695676, 0.4152173913043478160, 0.4173913043478260643, 0.4195652173913043681, 0.4217391304347826164, 0.4239130434782608647, 0.4260869565217391131, 0.4282608695652174169, 0.4304347826086956652, 0.4326086956521739135, 0.4347826086956521618, 0.4369565217391304102, 0.4391304347826087140, 0.4413043478260869623, 0.4434782608695652106, 0.4456521739130434590, 0.4478260869565217628, 0.4500000000000000111, 0.4521739130434782594, 0.4543478260869565077, 0.4565217391304347561, 0.4586956521739130599, 0.4608695652173913082, 0.4630434782608695565, 0.4652173913043478048, 0.4673913043478261087, 0.4695652173913043570, 0.4717391304347826053, 0.4739130434782608536, 0.4760869565217391575, 0.4782608695652174058, 0.4804347826086956541, 0.4826086956521739024, 0.4847826086956521507, 0.4869565217391304546, 0.4891304347826087029, 0.4913043478260869512, 0.4934782608695651995, 0.4956521739130435034, 0.4978260869565217517, 0.5000000000000000000, 0.5021739130434782483, 0.5043478260869564966, 0.5065217391304347450, 0.5086956521739129933, 0.5108695652173913526, 0.5130434782608696009, 0.5152173913043478493, 0.5173913043478260976, 0.5195652173913043459, 0.5217391304347825942, 0.5239130434782608425, 0.5260869565217390909, 0.5282608695652173392, 0.5304347826086956985, 0.5326086956521739468, 0.5347826086956521952, 0.5369565217391304435, 0.5391304347826086918, 0.5413043478260869401, 0.5434782608695651884, 0.5456521739130434367, 0.5478260869565216851, 0.5500000000000000444, 0.5521739130434782927, 0.5543478260869565410, 0.5565217391304347894, 0.5586956521739130377, 0.5608695652173912860, 0.5630434782608695343, 0.5652173913043477826, 0.5673913043478261420, 0.5695652173913043903, 0.5717391304347826386, 0.5739130434782608869, 0.5760869565217391353, 0.5782608695652173836, 0.5804347826086956319, 0.5826086956521738802, 0.5847826086956521285, 0.5869565217391304879, 0.5891304347826087362, 0.5913043478260869845, 0.5934782608695652328, 0.5956521739130434812, 0.5978260869565217295, 0.5999999999999999778, 0.6021739130434782261, 0.6043478260869564744, 0.6065217391304348338, 0.6086956521739130821, 0.6108695652173913304, 0.6130434782608695787, 0.6152173913043478271, 0.6173913043478260754, 0.6195652173913043237, 0.6217391304347825720, 0.6239130434782608203, 0.6260869565217391797, 0.6282608695652174280, 0.6304347826086956763, 0.6326086956521739246, 0.6347826086956521729, 0.6369565217391304213, 0.6391304347826086696, 0.6413043478260869179, 0.6434782608695651662, 0.6456521739130435256, 0.6478260869565217739, 0.6500000000000000222, 0.6521739130434782705, 0.6543478260869565188, 0.6565217391304347672, 0.6586956521739130155, 0.6608695652173912638, 0.6630434782608695121, 0.6652173913043478715, 0.6673913043478261198, 0.6695652173913043681, 0.6717391304347826164, 0.6739130434782608647, 0.6760869565217391131, 0.6782608695652173614, 0.6804347826086956097, 0.6826086956521738580, 0.6847826086956522174, 0.6869565217391304657, 0.6891304347826087140, 0.6913043478260869623, 0.6934782608695652106, 0.6956521739130434590, 0.6978260869565217073, 0.6999999999999999556, 0.7021739130434783149, 0.7043478260869565633, 0.7065217391304348116, 0.7086956521739130599, 0.7108695652173913082, 0.7130434782608695565, 0.7152173913043478048, 0.7173913043478260532, 0.7195652173913043015, 0.7217391304347826608, 0.7239130434782609091, 0.7260869565217391575, 0.7282608695652174058, 0.7304347826086956541, 0.7326086956521739024, 0.7347826086956521507, 0.7369565217391303991, 0.7391304347826086474, 0.7413043478260870067, 0.7434782608695652550, 0.7456521739130435034, 0.7478260869565217517, 0.7500000000000000000, 0.7521739130434782483, 0.7543478260869564966, 0.7565217391304347450, 0.7586956521739129933, 0.7608695652173913526, 0.7630434782608696009, 0.7652173913043478493, 0.7673913043478260976, 0.7695652173913043459, 0.7717391304347825942, 0.7739130434782608425, 0.7760869565217390909, 0.7782608695652173392, 0.7804347826086956985, 0.7826086956521739468, 0.7847826086956521952, 0.7869565217391304435, 0.7891304347826086918, 0.7913043478260869401, 0.7934782608695651884, 0.7956521739130434367, 0.7978260869565216851, 0.8000000000000000444, 0.8021739130434782927, 0.8043478260869565410, 0.8065217391304347894, 0.8086956521739130377, 0.8108695652173912860, 0.8130434782608695343, 0.8152173913043477826, 0.8173913043478261420, 0.8195652173913043903, 0.8217391304347826386, 0.8239130434782608869, 0.8260869565217391353, 0.8282608695652173836, 0.8304347826086956319, 0.8326086956521738802, 0.8347826086956521285, 0.8369565217391304879, 0.8391304347826087362, 0.8413043478260869845, 0.8434782608695652328, 0.8456521739130434812, 0.8478260869565217295, 0.8499999999999999778, 0.8521739130434782261, 0.8543478260869564744, 0.8565217391304348338, 0.8586956521739130821, 0.8608695652173913304, 0.8630434782608695787, 0.8652173913043478271, 0.8673913043478260754, 0.8695652173913043237, 0.8717391304347825720, 0.8739130434782608203, 0.8760869565217391797, 0.8782608695652174280, 0.8804347826086956763, 0.8826086956521739246, 0.8847826086956521729, 0.8869565217391304213, 0.8891304347826086696, 0.8913043478260869179, 0.8934782608695651662, 0.8956521739130435256, 0.8978260869565217739, 0.9000000000000000222, 0.9021739130434782705, 0.9043478260869565188, 0.9065217391304347672, 0.9086956521739130155, 0.9108695652173912638, 0.9130434782608695121, 0.9152173913043478715, 0.9173913043478261198, 0.9195652173913043681, 0.9217391304347826164, 0.9239130434782608647, 0.9260869565217391131, 0.9282608695652173614, 0.9304347826086956097, 0.9326086956521738580, 0.9347826086956522174, 0.9369565217391304657, 0.9391304347826087140, 0.9413043478260869623, 0.9434782608695652106, 0.9456521739130434590, 0.9478260869565217073, 0.9499999999999999556, 0.9521739130434783149, 0.9543478260869565633, 0.9565217391304348116, 0.9586956521739130599, 0.9608695652173913082, 0.9630434782608695565, 0.9652173913043478048, 0.9673913043478260532, 0.9695652173913043015, 0.9717391304347826608, 0.9739130434782609091, 0.9760869565217391575, 0.9782608695652174058, 0.9804347826086956541, 0.9826086956521739024, 0.9847826086956521507, 0.9869565217391303991, 0.9891304347826086474, 0.9913043478260870067 ),
 .UNSPECIFIED. ) 
 GEOMETRIC_REPRESENTATION_ITEM ( )  RATIONAL_B_SPLINE_SURFACE ( (
 ( 1.000000000000000000, 0.9510565162951535312, 1.000000000000000000, 0.9510565162951535312, 1.000000000000000000, 0.9510565162951535312, 1.000000000000000000, 0.9510565162951535312, 1.000000000000000000, 0.9510565162951535312, 1.000000000000000000, 0.9510565162951535312, 1.000000000000000000, 0.9510565162951535312, 1.000000000000000000, 0.9510565162951535312, 1.000000000000000000, 0.9510565162951535312, 1.000000000000000000, 0.9510565162951535312, 1.000000000000000000, 0.9510565162951535312, 1.000000000000000000, 0.9510565162951535312, 1.000000000000000000, 0.9510565162951535312, 1.000000000000000000, 0.9510565162951535312, 1.000000000000000000, 0.9510565162951535312, 1.000000000000000000, 0.9510565162951535312, 1.000000000000000000, 0.9510565162951535312, 1.000000000000000000, 0.9510565162951535312, 1.000000000000000000, 0.9510565162951535312, 1.000000000000000000, 0.9510565162951535312, 1.000000000000000000, 0.9510565162951535312, 1.000000000000000000, 0.9510565162951535312, 1.000000000000000000, 0.9510565162951535312, 1.000000000000000000, 0.9510565162951535312, 1.000000000000000000, 0.9510565162951535312, 1.000000000000000000, 0.9510565162951535312, 1.000000000000000000, 0.9510565162951535312, 1.000000000000000000, 0.9510565162951535312, 1.000000000000000000, 0.9510565162951535312, 1.000000000000000000, 0.9510565162951535312, 1.000000000000000000, 0.9510565162951535312, 1.000000000000000000, 0.9510565162951535312, 1.000000000000000000, 0.9510565162951535312, 1.000000000000000000, 0.9510565162951535312, 1.000000000000000000, 0.9510565162951535312, 1.000000000000000000, 0.9510565162951535312, 1.000000000000000000, 0.9510565162951535312, 1.000000000000000000, 0.9510565162951535312, 1.000000000000000000, 0.9510565162951535312, 1.000000000000000000, 0.9510565162951535312, 1.000000000000000000, 0.9510565162951535312, 1.000000000000000000, 0.9510565162951535312, 1.000000000000000000, 0.9510565162951535312, 1.000000000000000000, 0.9510565162951535312, 1.000000000000000000, 0.9510565162951535312, 1.000000000000000000, 0.9510565162951535312, 1.000000000000000000, 0.9510565162951535312, 1.000000000000000000, 0.9510565162951535312, 1.000000000000000000, 0.9510565162951535312, 1.000000000000000000, 0.9510565162951535312, 1.000000000000000000, 0.9510565162951535312, 1.000000000000000000, 0.9510565162951535312, 1.000000000000000000, 0.9510565162951535312, 1.000000000000000000, 0.9510565162951535312, 1.000000000000000000, 0.9510565162951535312, 1.000000000000000000, 0.9510565162951535312, 1.000000000000000000, 0.9510565162951535312, 1.000000000000000000, 0.9510565162951535312, 1.000000000000000000, 0.9510565162951535312, 1.000000000000000000, 0.9510565162951535312, 1.000000000000000000, 0.9510565162951535312, 1.000000000000000000, 0.9510565162951535312, 1.000000000000000000, 0.9510565162951535312, 1.000000000000000000, 0.9510565162951535312, 1.000000000000000000, 0.9510565162951535312, 1.000000000000000000, 0.9510565162951535312, 1.000000000000000000, 0.9510565162951535312, 1.000000000000000000, 0.9510565162951535312, 1.000000000000000000, 0.9510565162951535312, 1.000000000000000000, 0.9510565162951535312, 1.000000000000000000, 0.9510565162951535312, 1.000000000000000000, 0.9510565162951535312, 1.000000000000000000, 0.9510565162951535312, 1.000000000000000000, 0.9510565162951535312, 1.000000000000000000, 0.9510565162951535312, 1.000000000000000000, 0.9510565162951535312, 1.000000000000000000, 0.9510565162951535312, 1.000000000000000000, 0.9510565162951535312, 1.000000000000000000, 0.9510565162951535312, 1.000000000000000000, 0.9510565162951535312, 1.000000000000000000, 0.9510565162951535312, 1.000000000000000000, 0.9510565162951535312, 1.000000000000000000, 0.9510565162951535312, 1.000000000000000000, 0.9510565162951535312, 1.000000000000000000, 0.9510565162951535312, 1.000000000000000000, 0.9510565162951535312, 1.000000000000000000, 0.9510565162951535312, 1.000000000000000000, 0.9510565162951535312, 1.000000000000000000, 0.9510565162951535312, 1.000000000000000000, 0.9510565162951535312, 1.000000000000000000, 0.9510565162951535312, 1.000000000000000000, 0.9510565162951535312, 1.000000000000000000, 0.9510565162951535312, 1.000000000000000000, 0.9510565162951535312, 1.000000000000000000, 0.9510565162951535312, 1.000000000000000000, 0.9510565162951535312, 1.000000000000000000, 0.9510565162951535312, 1.000000000000000000, 0.9510565162951535312, 1.000000000000000000, 0.9510565162951535312, 1.000000000000000000, 0.9510565162951535312, 1.000000000000000000, 0.9510565162951535312, 1.000000000000000000, 0.9510565162951535312, 1.000000000000000000, 0.9510565162951535312, 1.000000000000000000, 0.9510565162951535312, 1.000000000000000000, 0.9510565162951535312, 1.000000000000000000, 0.9510565162951535312, 1.000000000000000000, 0.9510565162951535312, 1.000000000000000000, 0.9510565162951535312, 1.000000000000000000, 0.9510565162951535312, 1.000000000000000000, 0.9510565162951535312, 1.000000000000000000, 0.9510565162951535312, 1.000000000000000000, 0.9510565162951535312, 1.000000000000000000, 0.9510565162951535312, 1.000000000000000000, 0.9510565162951535312, 1.000000000000000000, 0.9510565162951535312, 1.000000000000000000, 0.9510565162951535312, 1.000000000000000000, 0.9510565162951535312, 1.000000000000000000, 0.9510565162951535312, 1.000000000000000000, 0.9510565162951535312, 1.000000000000000000, 0.9510565162951535312, 1.000000000000000000, 0.9510565162951535312, 1.000000000000000000, 0.9510565162951535312, 1.000000000000000000, 0.9510565162951535312, 1.000000000000000000, 0.9510565162951535312, 1.000000000000000000, 0.9510565162951535312, 1.000000000000000000, 0.9510565162951535312, 1.000000000000000000, 0.9510565162951535312, 1.000000000000000000, 0.9510565162951535312, 1.000000000000000000, 0.9510565162951535312, 1.000000000000000000, 0.9510565162951535312, 1.000000000000000000, 0.9510565162951535312, 1.000000000000000000, 0.9510565162951535312, 1.000000000000000000, 0.9510565162951535312, 1.000000000000000000, 0.9510565162951535312, 1.000000000000000000, 0.9510565162951535312, 1.000000000000000000, 0.9510565162951535312, 1.000000000000000000, 0.9510565162951535312, 1.000000000000000000, 0.9510565162951535312, 1.000000000000000000, 0.9510565162951535312, 1.000000000000000000, 0.9510565162951535312, 1.000000000000000000, 0.9510565162951535312, 1.000000000000000000, 0.9510565162951535312, 1.000000000000000000, 0.9510565162951535312, 1.000000000000000000, 0.9510565162951535312, 1.000000000000000000, 0.9510565162951535312, 1.000000000000000000, 0.9510565162951535312, 1.000000000000000000, 0.9510565162951535312, 1.000000000000000000, 0.9510565162951535312, 1.000000000000000000, 0.9510565162951535312, 1.000000000000000000, 0.9510565162951535312, 1.000000000000000000, 0.9510565162951535312, 1.000000000000000000, 0.9510565162951535312, 1.000000000000000000, 0.9510565162951535312, 1.000000000000000000, 0.9510565162951535312, 1.000000000000000000, 0.9510565162951535312, 1.000000000000000000, 0.9510565162951535312, 1.000000000000000000, 0.9510565162951535312, 1.000000000000000000, 0.9510565162951535312, 1.000000000000000000, 0.9510565162951535312, 1.000000000000000000, 0.9510565162951535312, 1.000000000000000000, 0.9510565162951535312, 1.000000000000000000, 0.9510565162951535312, 1.000000000000000000, 0.9510565162951535312, 1.000000000000000000, 0.9510565162951535312, 1.000000000000000000, 0.9510565162951535312, 1.000000000000000000, 0.9510565162951535312, 1.000000000000000000, 0.9510565162951535312, 1.000000000000000000, 0.9510565162951535312, 1.000000000000000000, 0.9510565162951535312, 1.000000000000000000, 0.9510565162951535312, 1.000000000000000000, 0.9510565162951535312, 1.000000000000000000, 0.9510565162951535312, 1.000000000000000000, 0.9510565162951535312, 1.000000000000000000, 0.9510565162951535312, 1.000000000000000000, 0.9510565162951535312, 1.000000000000000000, 0.9510565162951535312, 1.000000000000000000, 0.9510565162951535312, 1.000000000000000000, 0.9510565162951535312, 1.000000000000000000, 0.9510565162951535312, 1.000000000000000000, 0.9510565162951535312, 1.000000000000000000, 0.9510565162951535312, 1.000000000000000000, 0.9510565162951535312, 1.000000000000000000, 0.9510565162951535312, 1.000000000000000000, 0.9510565162951535312, 1.000000000000000000, 0.9510565162951535312, 1.000000000000000000, 0.9510565162951535312, 1.000000000000000000, 0.9510565162951535312, 1.000000000000000000, 0.9510565162951535312, 1.000000000000000000, 0.9510565162951535312, 1.000000000000000000, 0.9510565162951535312, 1.000000000000000000, 0.9510565162951535312, 1.000000000000000000, 0.9510565162951535312, 1.000000000000000000, 0.9510565162951535312, 1.000000000000000000, 0.9510565162951535312, 1.000000000000000000, 0.9510565162951535312, 1.000000000000000000, 0.9510565162951535312, 1.000000000000000000, 0.9510565162951535312, 1.000000000000000000, 0.9510565162951535312, 1.000000000000000000, 0.9510565162951535312, 1.000000000000000000, 0.9510565162951535312, 1.000000000000000000, 0.9510565162951535312, 1.000000000000000000, 0.9510565162951535312, 1.000000000000000000, 0.9510565162951535312, 1.000000000000000000, 0.9510565162951535312, 1.000000000000000000, 0.9510565162951535312, 1.000000000000000000, 0.9510565162951535312, 1.000000000000000000, 0.9510565162951535312, 1.000000000000000000, 0.9510565162951535312, 1.000000000000000000, 0.9510565162951535312, 1.000000000000000000, 0.9510565162951535312, 1.000000000000000000, 0.9510565162951535312, 1.000000000000000000, 0.9510565162951535312, 1.000000000000000000, 0.9510565162951535312, 1.000000000000000000, 0.9510565162951535312, 1.000000000000000000, 0.9510565162951535312, 1.000000000000000000, 0.9510565162951535312, 1.000000000000000000, 0.9510565162951535312, 1.000000000000000000, 0.9510565162951535312, 1.000000000000000000, 0.9510565162951535312, 1.000000000000000000, 0.9510565162951535312, 1.000000000000000000, 0.9510565162951535312, 1.000000000000000000, 0.9510565162951535312, 1.000000000000000000, 0.9510565162951535312, 1.000000000000000000, 0.9510565162951535312, 1.000000000000000000, 0.9510565162951535312, 1.000000000000000000, 0.9510565162951535312, 1.000000000000000000, 0.9510565162951535312, 1.000000000000000000, 0.9510565162951535312, 1.000000000000000000, 0.9510565162951535312, 1.000000000000000000, 0.9510565162951535312, 1.000000000000000000, 0.9510565162951535312, 1.000000000000000000, 0.9510565162951535312, 1.000000000000000000, 0.9510565162951535312, 1.000000000000000000, 0.9510565162951535312, 1.000000000000000000, 0.9510565162951535312, 1.000000000000000000, 0.9510565162951535312, 1.000000000000000000, 0.9510565162951535312, 1.000000000000000000, 0.9510565162951535312, 1.000000000000000000, 0.9510565162951535312, 1.000000000000000000, 0.9510565162951535312, 1.000000000000000000, 0.9510565162951535312, 1.000000000000000000, 0.9510565162951535312, 1.000000000000000000, 0.9510565162951535312, 1.000000000000000000, 0.9510565162951535312, 1.000000000000000000, 0.9510565162951535312, 1.000000000000000000, 0.9510565162951535312, 1.000000000000000000, 0.9510565162951535312, 1.000000000000000000, 0.9510565162951535312, 1.000000000000000000, 0.9510565162951535312, 1.000000000000000000, 0.9510565162951535312, 1.000000000000000000, 0.9510565162951535312, 1.000000000000000000, 0.9510565162951535312, 1.000000000000000000, 0.9510565162951535312, 1.000000000000000000, 0.9510565162951535312, 1.000000000000000000, 0.9510565162951535312, 1.000000000000000000, 0.9510565162951535312, 1.000000000000000000, 0.9510565162951535312, 1.000000000000000000, 0.9510565162951535312, 1.000000000000000000, 0.9510565162951535312, 1.000000000000000000, 0.9510565162951535312, 1.000000000000000000, 0.9510565162951535312, 1.000000000000000000, 0.9510565162951535312, 1.000000000000000000, 0.9510565162951535312, 1.000000000000000000, 0.9510565162951535312, 1.000000000000000000, 0.9510565162951535312, 1.000000000000000000, 0.9510565162951535312, 1.000000000000000000, 0.9510565162951535312, 1.000000000000000000, 0.9510565162951535312, 1.000000000000000000, 0.9510565162951535312, 1.000000000000000000, 0.9510565162951535312, 1.000000000000000000, 0.9510565162951535312, 1.000000000000000000, 0.9510565162951535312, 1.000000000000000000, 0.9510565162951535312, 1.000000000000000000, 0.9510565162951535312, 1.000000000000000000, 0.9510565162951535312, 1.000000000000000000, 0.9510565162951535312, 1.000000000000000000, 0.9510565162951535312, 1.000000000000000000, 0.9510565162951535312, 1.000000000000000000, 0.9510565162951535312, 1.000000000000000000, 0.9510565162951535312, 1.000000000000000000, 0.9510565162951535312, 1.000000000000000000, 0.9510565162951535312, 1.000000000000000000, 0.9510565162951535312, 1.000000000000000000, 0.9510565162951535312, 1.000000000000000000, 0.9510565162951535312, 1.000000000000000000, 0.9510565162951535312, 1.000000000000000000, 0.9510565162951535312, 1.000000000000000000, 0.9510565162951535312, 1.000000000000000000, 0.9510565162951535312, 1.000000000000000000, 0.9510565162951535312, 1.000000000000000000, 0.9510565162951535312, 1.000000000000000000, 0.9510565162951535312, 1.000000000000000000, 0.9510565162951535312, 1.000000000000000000, 0.9510565162951535312, 1.000000000000000000, 0.9510565162951535312, 1.000000000000000000, 0.9510565162951535312, 1.000000000000000000, 0.9510565162951535312, 1.000000000000000000, 0.9510565162951535312, 1.000000000000000000, 0.9510565162951535312, 1.000000000000000000, 0.9510565162951535312, 1.000000000000000000, 0.9510565162951535312, 1.000000000000000000, 0.9510565162951535312, 1.000000000000000000, 0.9510565162951535312, 1.000000000000000000, 0.9510565162951535312, 1.000000000000000000, 0.9510565162951535312, 1.000000000000000000, 0.9510565162951535312, 1.000000000000000000, 0.9510565162951535312, 1.000000000000000000, 0.9510565162951535312, 1.000000000000000000, 0.9510565162951535312, 1.000000000000000000, 0.9510565162951535312, 1.000000000000000000, 0.9510565162951535312, 1.000000000000000000, 0.9510565162951535312, 1.000000000000000000, 0.9510565162951535312, 1.000000000000000000, 0.9510565162951535312, 1.000000000000000000, 0.9510565162951535312, 1.000000000000000000, 0.9510565162951535312, 1.000000000000000000, 0.9510565162951535312, 1.000000000000000000, 0.9510565162951535312, 1.000000000000000000, 0.9510565162951535312, 1.000000000000000000, 0.9510565162951535312, 1.000000000000000000, 0.9510565162951535312, 1.000000000000000000, 0.9510565162951535312, 1.000000000000000000, 0.9510565162951535312, 1.000000000000000000, 0.9510565162951535312, 1.000000000000000000, 0.9510565162951535312, 1.000000000000000000, 0.9510565162951535312, 1.000000000000000000, 0.9510565162951535312, 1.000000000000000000, 0.9510565162951535312, 1.000000000000000000, 0.9510565162951535312, 1.000000000000000000, 0.9510565162951535312, 1.000000000000000000, 0.9510565162951535312, 1.000000000000000000, 0.9510565162951535312, 1.000000000000000000, 0.9510565162951535312, 1.000000000000000000, 0.9510565162951535312, 1.000000000000000000, 0.9510565162951535312, 1.000000000000000000, 0.9510565162951535312, 1.000000000000000000, 0.9510565162951535312, 1.000000000000000000, 0.9510565162951535312, 1.000000000000000000, 0.9510565162951535312, 1.000000000000000000, 0.9510565162951535312, 1.000000000000000000, 0.9510565162951535312, 1.000000000000000000, 0.9510565162951535312, 1.000000000000000000, 0.9510565162951535312, 1.000000000000000000, 0.9510565162951535312, 1.000000000000000000, 0.9510565162951535312, 1.000000000000000000, 0.9510565162951535312, 1.000000000000000000, 0.9510565162951535312, 1.000000000000000000, 0.9510565162951535312, 1.000000000000000000, 0.9510565162951535312, 1.000000000000000000, 0.9510565162951535312, 1.000000000000000000, 0.9510565162951535312, 1.000000000000000000, 0.9510565162951535312, 1.000000000000000000, 0.9510565162951535312, 1.000000000000000000, 0.9510565162951535312, 1.000000000000000000, 0.9510565162951535312, 1.000000000000000000, 0.9510565162951535312, 1.000000000000000000, 0.9510565162951535312, 1.000000000000000000, 0.9510565162951535312, 1.000000000000000000, 0.9510565162951535312, 1.000000000000000000, 0.9510565162951535312, 1.000000000000000000, 0.9510565162951535312, 1.000000000000000000, 0.9510565162951535312, 1.000000000000000000, 0.9510565162951535312, 1.000000000000000000, 0.9510565162951535312, 1.000000000000000000, 0.9510565162951535312, 1.000000000000000000, 0.9510565162951535312, 1.000000000000000000, 0.9510565162951535312, 1.000000000000000000, 0.9510565162951535312, 1.000000000000000000, 0.9510565162951535312, 1.000000000000000000, 0.9510565162951535312, 1.000000000000000000, 0.9510565162951535312, 1.000000000000000000, 0.9510565162951535312, 1.000000000000000000, 0.9510565162951535312, 1.000000000000000000, 0.9510565162951535312, 1.000000000000000000, 0.9510565162951535312, 1.000000000000000000, 0.9510565162951535312, 1.000000000000000000, 0.9510565162951535312, 1.000000000000000000, 0.9510565162951535312, 1.000000000000000000, 0.9510565162951535312, 1.000000000000000000, 0.9510565162951535312, 1.000000000000000000, 0.9510565162951535312, 1.000000000000000000, 0.9510565162951535312, 1.000000000000000000, 0.9510565162951535312, 1.000000000000000000, 0.9510565162951535312, 1.000000000000000000, 0.9510565162951535312, 1.000000000000000000, 0.9510565162951535312, 1.000000000000000000, 0.9510565162951535312, 1.000000000000000000, 0.9510565162951535312, 1.000000000000000000, 0.9510565162951535312, 1.000000000000000000, 0.9510565162951535312, 1.000000000000000000, 0.9510565162951535312, 1.000000000000000000, 0.9510565162951535312, 1.000000000000000000, 0.9510565162951535312, 1.000000000000000000, 0.9510565162951535312, 1.000000000000000000, 0.9510565162951535312, 1.000000000000000000, 0.9510565162951535312, 1.000000000000000000, 0.9510565162951535312, 1.000000000000000000, 0.9510565162951535312, 1.000000000000000000, 0.9510565162951535312, 1.000000000000000000, 0.9510565162951535312, 1.000000000000000000, 0.9510565162951535312, 1.000000000000000000, 0.9510565162951535312, 1.000000000000000000, 0.9510565162951535312, 1.000000000000000000, 0.9510565162951535312, 1.000000000000000000, 0.9510565162951535312, 1.000000000000000000, 0.9510565162951535312, 1.000000000000000000, 0.9510565162951535312, 1.000000000000000000, 0.9510565162951535312, 1.000000000000000000, 0.9510565162951535312, 1.000000000000000000, 0.9510565162951535312, 1.000000000000000000, 0.9510565162951535312, 1.000000000000000000, 0.9510565162951535312, 1.000000000000000000, 0.9510565162951535312, 1.000000000000000000, 0.9510565162951535312, 1.000000000000000000, 0.9510565162951535312, 1.000000000000000000, 0.9510565162951535312, 1.000000000000000000, 0.9510565162951535312, 1.000000000000000000, 0.9510565162951535312, 1.000000000000000000, 0.9510565162951535312, 1.000000000000000000, 0.9510565162951535312, 1.000000000000000000, 0.9510565162951535312, 1.000000000000000000, 0.9510565162951535312, 1.000000000000000000, 0.9510565162951535312, 1.000000000000000000, 0.9510565162951535312, 1.000000000000000000, 0.9510565162951535312, 1.000000000000000000, 0.9510565162951535312, 1.000000000000000000, 0.9510565162951535312, 1.000000000000000000, 0.9510565162951535312, 1.000000000000000000, 0.9510565162951535312, 1.000000000000000000, 0.9510565162951535312, 1.000000000000000000, 0.9510565162951535312, 1.000000000000000000, 0.9510565162951535312, 1.000000000000000000, 0.9510565162951535312, 1.000000000000000000, 0.9510565162951535312, 1.000000000000000000, 0.9510565162951535312, 1.000000000000000000, 0.9510565162951535312, 1.000000000000000000, 0.9510565162951535312, 1.000000000000000000, 0.9510565162951535312, 1.000000000000000000, 0.9510565162951535312, 1.000000000000000000, 0.9510565162951535312, 1.000000000000000000, 0.9510565162951535312, 1.000000000000000000, 0.9510565162951535312, 1.000000000000000000, 0.9510565162951535312, 1.000000000000000000, 0.9510565162951535312, 1.000000000000000000, 0.9510565162951535312, 1.000000000000000000, 0.9510565162951535312, 1.000000000000000000, 0.9510565162951535312, 1.000000000000000000, 0.9510565162951535312, 1.000000000000000000, 0.9510565162951535312, 1.000000000000000000, 0.9510565162951535312, 1.000000000000000000, 0.9510565162951535312, 1.000000000000000000, 0.9510565162951535312, 1.000000000000000000, 0.9510565162951535312, 1.000000000000000000, 0.9510565162951535312, 1.000000000000000000, 0.9510565162951535312, 1.000000000000000000, 0.9510565162951535312, 1.000000000000000000),
 ( 1.000000000000000000, 0.9510565162951535312, 1.000000000000000000, 0.9510565162951535312, 1.000000000000000000, 0.9510565162951535312, 1.000000000000000000, 0.9510565162951535312, 1.000000000000000000, 0.9510565162951535312, 1.000000000000000000, 0.9510565162951535312, 1.000000000000000000, 0.9510565162951535312, 1.000000000000000000, 0.9510565162951535312, 1.000000000000000000, 0.9510565162951535312, 1.000000000000000000, 0.9510565162951535312, 1.000000000000000000, 0.9510565162951535312, 1.000000000000000000, 0.9510565162951535312, 1.000000000000000000, 0.9510565162951535312, 1.000000000000000000, 0.9510565162951535312, 1.000000000000000000, 0.9510565162951535312, 1.000000000000000000, 0.9510565162951535312, 1.000000000000000000, 0.9510565162951535312, 1.000000000000000000, 0.9510565162951535312, 1.000000000000000000, 0.9510565162951535312, 1.000000000000000000, 0.9510565162951535312, 1.000000000000000000, 0.9510565162951535312, 1.000000000000000000, 0.9510565162951535312, 1.000000000000000000, 0.9510565162951535312, 1.000000000000000000, 0.9510565162951535312, 1.000000000000000000, 0.9510565162951535312, 1.000000000000000000, 0.9510565162951535312, 1.000000000000000000, 0.9510565162951535312, 1.000000000000000000, 0.9510565162951535312, 1.000000000000000000, 0.9510565162951535312, 1.000000000000000000, 0.9510565162951535312, 1.000000000000000000, 0.9510565162951535312, 1.000000000000000000, 0.9510565162951535312, 1.000000000000000000, 0.9510565162951535312, 1.000000000000000000, 0.9510565162951535312, 1.000000000000000000, 0.9510565162951535312, 1.000000000000000000, 0.9510565162951535312, 1.000000000000000000, 0.9510565162951535312, 1.000000000000000000, 0.9510565162951535312, 1.000000000000000000, 0.9510565162951535312, 1.000000000000000000, 0.9510565162951535312, 1.000000000000000000, 0.9510565162951535312, 1.000000000000000000, 0.9510565162951535312, 1.000000000000000000, 0.9510565162951535312, 1.000000000000000000, 0.9510565162951535312, 1.000000000000000000, 0.9510565162951535312, 1.000000000000000000, 0.9510565162951535312, 1.000000000000000000, 0.9510565162951535312, 1.000000000000000000, 0.9510565162951535312, 1.000000000000000000, 0.9510565162951535312, 1.000000000000000000, 0.9510565162951535312, 1.000000000000000000, 0.9510565162951535312, 1.000000000000000000, 0.9510565162951535312, 1.000000000000000000, 0.9510565162951535312, 1.000000000000000000, 0.9510565162951535312, 1.000000000000000000, 0.9510565162951535312, 1.000000000000000000, 0.9510565162951535312, 1.000000000000000000, 0.9510565162951535312, 1.000000000000000000, 0.9510565162951535312, 1.000000000000000000, 0.9510565162951535312, 1.000000000000000000, 0.9510565162951535312, 1.000000000000000000, 0.9510565162951535312, 1.000000000000000000, 0.9510565162951535312, 1.000000000000000000, 0.9510565162951535312, 1.000000000000000000, 0.9510565162951535312, 1.000000000000000000, 0.9510565162951535312, 1.000000000000000000, 0.9510565162951535312, 1.000000000000000000, 0.9510565162951535312, 1.000000000000000000, 0.9510565162951535312, 1.000000000000000000, 0.9510565162951535312, 1.000000000000000000, 0.9510565162951535312, 1.000000000000000000, 0.9510565162951535312, 1.000000000000000000, 0.9510565162951535312, 1.000000000000000000, 0.9510565162951535312, 1.000000000000000000, 0.9510565162951535312, 1.000000000000000000, 0.9510565162951535312, 1.000000000000000000, 0.9510565162951535312, 1.000000000000000000, 0.9510565162951535312, 1.000000000000000000, 0.9510565162951535312, 1.000000000000000000, 0.9510565162951535312, 1.000000000000000000, 0.9510565162951535312, 1.000000000000000000, 0.9510565162951535312, 1.000000000000000000, 0.9510565162951535312, 1.000000000000000000, 0.9510565162951535312, 1.000000000000000000, 0.9510565162951535312, 1.000000000000000000, 0.9510565162951535312, 1.000000000000000000, 0.9510565162951535312, 1.000000000000000000, 0.9510565162951535312, 1.000000000000000000, 0.9510565162951535312, 1.000000000000000000, 0.9510565162951535312, 1.000000000000000000, 0.9510565162951535312, 1.000000000000000000, 0.9510565162951535312, 1.000000000000000000, 0.9510565162951535312, 1.000000000000000000, 0.9510565162951535312, 1.000000000000000000, 0.9510565162951535312, 1.000000000000000000, 0.9510565162951535312, 1.000000000000000000, 0.9510565162951535312, 1.000000000000000000, 0.9510565162951535312, 1.000000000000000000, 0.9510565162951535312, 1.000000000000000000, 0.9510565162951535312, 1.000000000000000000, 0.9510565162951535312, 1.000000000000000000, 0.9510565162951535312, 1.000000000000000000, 0.9510565162951535312, 1.000000000000000000, 0.9510565162951535312, 1.000000000000000000, 0.9510565162951535312, 1.000000000000000000, 0.9510565162951535312, 1.000000000000000000, 0.9510565162951535312, 1.000000000000000000, 0.9510565162951535312, 1.000000000000000000, 0.9510565162951535312, 1.000000000000000000, 0.9510565162951535312, 1.000000000000000000, 0.9510565162951535312, 1.000000000000000000, 0.9510565162951535312, 1.000000000000000000, 0.9510565162951535312, 1.000000000000000000, 0.9510565162951535312, 1.000000000000000000, 0.9510565162951535312, 1.000000000000000000, 0.9510565162951535312, 1.000000000000000000, 0.9510565162951535312, 1.000000000000000000, 0.9510565162951535312, 1.000000000000000000, 0.9510565162951535312, 1.000000000000000000, 0.9510565162951535312, 1.000000000000000000, 0.9510565162951535312, 1.000000000000000000, 0.9510565162951535312, 1.000000000000000000, 0.9510565162951535312, 1.000000000000000000, 0.9510565162951535312, 1.000000000000000000, 0.9510565162951535312, 1.000000000000000000, 0.9510565162951535312, 1.000000000000000000, 0.9510565162951535312, 1.000000000000000000, 0.9510565162951535312, 1.000000000000000000, 0.9510565162951535312, 1.000000000000000000, 0.9510565162951535312, 1.000000000000000000, 0.9510565162951535312, 1.000000000000000000, 0.9510565162951535312, 1.000000000000000000, 0.9510565162951535312, 1.000000000000000000, 0.9510565162951535312, 1.000000000000000000, 0.9510565162951535312, 1.000000000000000000, 0.9510565162951535312, 1.000000000000000000, 0.9510565162951535312, 1.000000000000000000, 0.9510565162951535312, 1.000000000000000000, 0.9510565162951535312, 1.000000000000000000, 0.9510565162951535312, 1.000000000000000000, 0.9510565162951535312, 1.000000000000000000, 0.9510565162951535312, 1.000000000000000000, 0.9510565162951535312, 1.000000000000000000, 0.9510565162951535312, 1.000000000000000000, 0.9510565162951535312, 1.000000000000000000, 0.9510565162951535312, 1.000000000000000000, 0.9510565162951535312, 1.000000000000000000, 0.9510565162951535312, 1.000000000000000000, 0.9510565162951535312, 1.000000000000000000, 0.9510565162951535312, 1.000000000000000000, 0.9510565162951535312, 1.000000000000000000, 0.9510565162951535312, 1.000000000000000000, 0.9510565162951535312, 1.000000000000000000, 0.9510565162951535312, 1.000000000000000000, 0.9510565162951535312, 1.000000000000000000, 0.9510565162951535312, 1.000000000000000000, 0.9510565162951535312, 1.000000000000000000, 0.9510565162951535312, 1.000000000000000000, 0.9510565162951535312, 1.000000000000000000, 0.9510565162951535312, 1.000000000000000000, 0.9510565162951535312, 1.000000000000000000, 0.9510565162951535312, 1.000000000000000000, 0.9510565162951535312, 1.000000000000000000, 0.9510565162951535312, 1.000000000000000000, 0.9510565162951535312, 1.000000000000000000, 0.9510565162951535312, 1.000000000000000000, 0.9510565162951535312, 1.000000000000000000, 0.9510565162951535312, 1.000000000000000000, 0.9510565162951535312, 1.000000000000000000, 0.9510565162951535312, 1.000000000000000000, 0.9510565162951535312, 1.000000000000000000, 0.9510565162951535312, 1.000000000000000000, 0.9510565162951535312, 1.000000000000000000, 0.9510565162951535312, 1.000000000000000000, 0.9510565162951535312, 1.000000000000000000, 0.9510565162951535312, 1.000000000000000000, 0.9510565162951535312, 1.000000000000000000, 0.9510565162951535312, 1.000000000000000000, 0.9510565162951535312, 1.000000000000000000, 0.9510565162951535312, 1.000000000000000000, 0.9510565162951535312, 1.000000000000000000, 0.9510565162951535312, 1.000000000000000000, 0.9510565162951535312, 1.000000000000000000, 0.9510565162951535312, 1.000000000000000000, 0.9510565162951535312, 1.000000000000000000, 0.9510565162951535312, 1.000000000000000000, 0.9510565162951535312, 1.000000000000000000, 0.9510565162951535312, 1.000000000000000000, 0.9510565162951535312, 1.000000000000000000, 0.9510565162951535312, 1.000000000000000000, 0.9510565162951535312, 1.000000000000000000, 0.9510565162951535312, 1.000000000000000000, 0.9510565162951535312, 1.000000000000000000, 0.9510565162951535312, 1.000000000000000000, 0.9510565162951535312, 1.000000000000000000, 0.9510565162951535312, 1.000000000000000000, 0.9510565162951535312, 1.000000000000000000, 0.9510565162951535312, 1.000000000000000000, 0.9510565162951535312, 1.000000000000000000, 0.9510565162951535312, 1.000000000000000000, 0.9510565162951535312, 1.000000000000000000, 0.9510565162951535312, 1.000000000000000000, 0.9510565162951535312, 1.000000000000000000, 0.9510565162951535312, 1.000000000000000000, 0.9510565162951535312, 1.000000000000000000, 0.9510565162951535312, 1.000000000000000000, 0.9510565162951535312, 1.000000000000000000, 0.9510565162951535312, 1.000000000000000000, 0.9510565162951535312, 1.000000000000000000, 0.9510565162951535312, 1.000000000000000000, 0.9510565162951535312, 1.000000000000000000, 0.9510565162951535312, 1.000000000000000000, 0.9510565162951535312, 1.000000000000000000, 0.9510565162951535312, 1.000000000000000000, 0.9510565162951535312, 1.000000000000000000, 0.9510565162951535312, 1.000000000000000000, 0.9510565162951535312, 1.000000000000000000, 0.9510565162951535312, 1.000000000000000000, 0.9510565162951535312, 1.000000000000000000, 0.9510565162951535312, 1.000000000000000000, 0.9510565162951535312, 1.000000000000000000, 0.9510565162951535312, 1.000000000000000000, 0.9510565162951535312, 1.000000000000000000, 0.9510565162951535312, 1.000000000000000000, 0.9510565162951535312, 1.000000000000000000, 0.9510565162951535312, 1.000000000000000000, 0.9510565162951535312, 1.000000000000000000, 0.9510565162951535312, 1.000000000000000000, 0.9510565162951535312, 1.000000000000000000, 0.9510565162951535312, 1.000000000000000000, 0.9510565162951535312, 1.000000000000000000, 0.9510565162951535312, 1.000000000000000000, 0.9510565162951535312, 1.000000000000000000, 0.9510565162951535312, 1.000000000000000000, 0.9510565162951535312, 1.000000000000000000, 0.9510565162951535312, 1.000000000000000000, 0.9510565162951535312, 1.000000000000000000, 0.9510565162951535312, 1.000000000000000000, 0.9510565162951535312, 1.000000000000000000, 0.9510565162951535312, 1.000000000000000000, 0.9510565162951535312, 1.000000000000000000, 0.9510565162951535312, 1.000000000000000000, 0.9510565162951535312, 1.000000000000000000, 0.9510565162951535312, 1.000000000000000000, 0.9510565162951535312, 1.000000000000000000, 0.9510565162951535312, 1.000000000000000000, 0.9510565162951535312, 1.000000000000000000, 0.9510565162951535312, 1.000000000000000000, 0.9510565162951535312, 1.000000000000000000, 0.9510565162951535312, 1.000000000000000000, 0.9510565162951535312, 1.000000000000000000, 0.9510565162951535312, 1.000000000000000000, 0.9510565162951535312, 1.000000000000000000, 0.9510565162951535312, 1.000000000000000000, 0.9510565162951535312, 1.000000000000000000, 0.9510565162951535312, 1.000000000000000000, 0.9510565162951535312, 1.000000000000000000, 0.9510565162951535312, 1.000000000000000000, 0.9510565162951535312, 1.000000000000000000, 0.9510565162951535312, 1.000000000000000000, 0.9510565162951535312, 1.000000000000000000, 0.9510565162951535312, 1.000000000000000000, 0.9510565162951535312, 1.000000000000000000, 0.9510565162951535312, 1.000000000000000000, 0.9510565162951535312, 1.000000000000000000, 0.9510565162951535312, 1.000000000000000000, 0.9510565162951535312, 1.000000000000000000, 0.9510565162951535312, 1.000000000000000000, 0.9510565162951535312, 1.000000000000000000, 0.9510565162951535312, 1.000000000000000000, 0.9510565162951535312, 1.000000000000000000, 0.9510565162951535312, 1.000000000000000000, 0.9510565162951535312, 1.000000000000000000, 0.9510565162951535312, 1.000000000000000000, 0.9510565162951535312, 1.000000000000000000, 0.9510565162951535312, 1.000000000000000000, 0.9510565162951535312, 1.000000000000000000, 0.9510565162951535312, 1.000000000000000000, 0.9510565162951535312, 1.000000000000000000, 0.9510565162951535312, 1.000000000000000000, 0.9510565162951535312, 1.000000000000000000, 0.9510565162951535312, 1.000000000000000000, 0.9510565162951535312, 1.000000000000000000, 0.9510565162951535312, 1.000000000000000000, 0.9510565162951535312, 1.000000000000000000, 0.9510565162951535312, 1.000000000000000000, 0.9510565162951535312, 1.000000000000000000, 0.9510565162951535312, 1.000000000000000000, 0.9510565162951535312, 1.000000000000000000, 0.9510565162951535312, 1.000000000000000000, 0.9510565162951535312, 1.000000000000000000, 0.9510565162951535312, 1.000000000000000000, 0.9510565162951535312, 1.000000000000000000, 0.9510565162951535312, 1.000000000000000000, 0.9510565162951535312, 1.000000000000000000, 0.9510565162951535312, 1.000000000000000000, 0.9510565162951535312, 1.000000000000000000, 0.9510565162951535312, 1.000000000000000000, 0.9510565162951535312, 1.000000000000000000, 0.9510565162951535312, 1.000000000000000000, 0.9510565162951535312, 1.000000000000000000, 0.9510565162951535312, 1.000000000000000000, 0.9510565162951535312, 1.000000000000000000, 0.9510565162951535312, 1.000000000000000000, 0.9510565162951535312, 1.000000000000000000, 0.9510565162951535312, 1.000000000000000000, 0.9510565162951535312, 1.000000000000000000, 0.9510565162951535312, 1.000000000000000000, 0.9510565162951535312, 1.000000000000000000, 0.9510565162951535312, 1.000000000000000000, 0.9510565162951535312, 1.000000000000000000, 0.9510565162951535312, 1.000000000000000000, 0.9510565162951535312, 1.000000000000000000, 0.9510565162951535312, 1.000000000000000000, 0.9510565162951535312, 1.000000000000000000, 0.9510565162951535312, 1.000000000000000000, 0.9510565162951535312, 1.000000000000000000, 0.9510565162951535312, 1.000000000000000000, 0.9510565162951535312, 1.000000000000000000, 0.9510565162951535312, 1.000000000000000000, 0.9510565162951535312, 1.000000000000000000, 0.9510565162951535312, 1.000000000000000000, 0.9510565162951535312, 1.000000000000000000, 0.9510565162951535312, 1.000000000000000000, 0.9510565162951535312, 1.000000000000000000, 0.9510565162951535312, 1.000000000000000000, 0.9510565162951535312, 1.000000000000000000, 0.9510565162951535312, 1.000000000000000000, 0.9510565162951535312, 1.000000000000000000, 0.9510565162951535312, 1.000000000000000000, 0.9510565162951535312, 1.000000000000000000, 0.9510565162951535312, 1.000000000000000000, 0.9510565162951535312, 1.000000000000000000, 0.9510565162951535312, 1.000000000000000000, 0.9510565162951535312, 1.000000000000000000, 0.9510565162951535312, 1.000000000000000000, 0.9510565162951535312, 1.000000000000000000, 0.9510565162951535312, 1.000000000000000000, 0.9510565162951535312, 1.000000000000000000, 0.9510565162951535312, 1.000000000000000000, 0.9510565162951535312, 1.000000000000000000, 0.9510565162951535312, 1.000000000000000000, 0.9510565162951535312, 1.000000000000000000, 0.9510565162951535312, 1.000000000000000000, 0.9510565162951535312, 1.000000000000000000, 0.9510565162951535312, 1.000000000000000000, 0.9510565162951535312, 1.000000000000000000, 0.9510565162951535312, 1.000000000000000000, 0.9510565162951535312, 1.000000000000000000, 0.9510565162951535312, 1.000000000000000000, 0.9510565162951535312, 1.000000000000000000, 0.9510565162951535312, 1.000000000000000000, 0.9510565162951535312, 1.000000000000000000, 0.9510565162951535312, 1.000000000000000000, 0.9510565162951535312, 1.000000000000000000, 0.9510565162951535312, 1.000000000000000000, 0.9510565162951535312, 1.000000000000000000, 0.9510565162951535312, 1.000000000000000000, 0.9510565162951535312, 1.000000000000000000, 0.9510565162951535312, 1.000000000000000000, 0.9510565162951535312, 1.000000000000000000, 0.9510565162951535312, 1.000000000000000000, 0.9510565162951535312, 1.000000000000000000, 0.9510565162951535312, 1.000000000000000000, 0.9510565162951535312, 1.000000000000000000, 0.9510565162951535312, 1.000000000000000000, 0.9510565162951535312, 1.000000000000000000, 0.9510565162951535312, 1.000000000000000000, 0.9510565162951535312, 1.000000000000000000, 0.9510565162951535312, 1.000000000000000000, 0.9510565162951535312, 1.000000000000000000, 0.9510565162951535312, 1.000000000000000000, 0.9510565162951535312, 1.000000000000000000, 0.9510565162951535312, 1.000000000000000000, 0.9510565162951535312, 1.000000000000000000, 0.9510565162951535312, 1.000000000000000000, 0.9510565162951535312, 1.000000000000000000, 0.9510565162951535312, 1.000000000000000000, 0.9510565162951535312, 1.000000000000000000, 0.9510565162951535312, 1.000000000000000000, 0.9510565162951535312, 1.000000000000000000, 0.9510565162951535312, 1.000000000000000000, 0.9510565162951535312, 1.000000000000000000, 0.9510565162951535312, 1.000000000000000000, 0.9510565162951535312, 1.000000000000000000, 0.9510565162951535312, 1.000000000000000000, 0.9510565162951535312, 1.000000000000000000, 0.9510565162951535312, 1.000000000000000000, 0.9510565162951535312, 1.000000000000000000, 0.9510565162951535312, 1.000000000000000000, 0.9510565162951535312, 1.000000000000000000, 0.9510565162951535312, 1.000000000000000000, 0.9510565162951535312, 1.000000000000000000, 0.9510565162951535312, 1.000000000000000000, 0.9510565162951535312, 1.000000000000000000, 0.9510565162951535312, 1.000000000000000000, 0.9510565162951535312, 1.000000000000000000, 0.9510565162951535312, 1.000000000000000000, 0.9510565162951535312, 1.000000000000000000, 0.9510565162951535312, 1.000000000000000000, 0.9510565162951535312, 1.000000000000000000, 0.9510565162951535312, 1.000000000000000000, 0.9510565162951535312, 1.000000000000000000, 0.9510565162951535312, 1.000000000000000000, 0.9510565162951535312, 1.000000000000000000, 0.9510565162951535312, 1.000000000000000000, 0.9510565162951535312, 1.000000000000000000, 0.9510565162951535312, 1.000000000000000000, 0.9510565162951535312, 1.000000000000000000, 0.9510565162951535312, 1.000000000000000000, 0.9510565162951535312, 1.000000000000000000, 0.9510565162951535312, 1.000000000000000000, 0.9510565162951535312, 1.000000000000000000, 0.9510565162951535312, 1.000000000000000000, 0.9510565162951535312, 1.000000000000000000, 0.9510565162951535312, 1.000000000000000000, 0.9510565162951535312, 1.000000000000000000, 0.9510565162951535312, 1.000000000000000000, 0.9510565162951535312, 1.000000000000000000, 0.9510565162951535312, 1.000000000000000000, 0.9510565162951535312, 1.000000000000000000, 0.9510565162951535312, 1.000000000000000000, 0.9510565162951535312, 1.000000000000000000, 0.9510565162951535312, 1.000000000000000000, 0.9510565162951535312, 1.000000000000000000, 0.9510565162951535312, 1.000000000000000000, 0.9510565162951535312, 1.000000000000000000, 0.9510565162951535312, 1.000000000000000000, 0.9510565162951535312, 1.000000000000000000, 0.9510565162951535312, 1.000000000000000000, 0.9510565162951535312, 1.000000000000000000, 0.9510565162951535312, 1.000000000000000000, 0.9510565162951535312, 1.000000000000000000, 0.9510565162951535312, 1.000000000000000000, 0.9510565162951535312, 1.000000000000000000, 0.9510565162951535312, 1.000000000000000000, 0.9510565162951535312, 1.000000000000000000, 0.9510565162951535312, 1.000000000000000000, 0.9510565162951535312, 1.000000000000000000, 0.9510565162951535312, 1.000000000000000000, 0.9510565162951535312, 1.000000000000000000, 0.9510565162951535312, 1.000000000000000000, 0.9510565162951535312, 1.000000000000000000, 0.9510565162951535312, 1.000000000000000000, 0.9510565162951535312, 1.000000000000000000, 0.9510565162951535312, 1.000000000000000000, 0.9510565162951535312, 1.000000000000000000, 0.9510565162951535312, 1.000000000000000000, 0.9510565162951535312, 1.000000000000000000, 0.9510565162951535312, 1.000000000000000000, 0.9510565162951535312, 1.000000000000000000, 0.9510565162951535312, 1.000000000000000000, 0.9510565162951535312, 1.000000000000000000, 0.9510565162951535312, 1.000000000000000000, 0.9510565162951535312, 1.000000000000000000, 0.9510565162951535312, 1.000000000000000000, 0.9510565162951535312, 1.000000000000000000) ) ) 
 REPRESENTATION_ITEM ( '' )  SURFACE ( )  );
#61087 = ORIENTED_EDGE ( 'NONE', *, *, #63509, .F. ) ;
#61088 = AXIS2_PLACEMENT_3D ( 'NONE', #15352, #47363, #9711 ) ;
#61089 = CARTESIAN_POINT ( 'NONE',  ( -67.34292637653379643, -9.058813317711329915, 2.943386871421371787 ) ) ;
#61090 = CARTESIAN_POINT ( 'NONE',  ( -13.50000000000000355, 28.24999999999998934, 3.750000000000000000 ) ) ;
#61091 = CARTESIAN_POINT ( 'NONE',  ( 8.021777294149467608, -2.499999999999998224, -4.105874159530731760 ) ) ;
#61092 =( GEOMETRIC_REPRESENTATION_CONTEXT ( 3 ) GLOBAL_UNCERTAINTY_ASSIGNED_CONTEXT ( ( #67286 ) ) GLOBAL_UNIT_ASSIGNED_CONTEXT ( ( #13781, #2472, #40893 ) ) REPRESENTATION_CONTEXT ( 'NONE', 'WORKASPACE' ) );
#61093 = CARTESIAN_POINT ( 'NONE',  ( -71.75499999999998124, 4.716976649647091513, -6.492361379858946790 ) ) ;
#61094 = CARTESIAN_POINT ( 'NONE',  ( -36.50190183960178558, -11.99078436789255164, 3.069443153576023153 ) ) ;
#61095 = DIRECTION ( 'NONE',  ( 0.000000000000000000, 0.000000000000000000, -1.000000000000000000 ) ) ;
#61096 = VECTOR ( 'NONE', #5241, 1000.000000000000000 ) ;
#61097 = MECHANICAL_DESIGN_GEOMETRIC_PRESENTATION_REPRESENTATION (  '', ( #46603 ), #63366 ) ;
#61098 = CARTESIAN_POINT ( 'NONE',  ( -68.09499999999998465, -2.607480562269071545, -8.024999999999991473 ) ) ;
#61099 = CARTESIAN_POINT ( 'NONE',  ( 3.094860106618431583, 148.2050000000000125, 9.525000000000000355 ) ) ;
#61100 = EDGE_CURVE ( 'NONE', #18574, #38604, #6508, .T. ) ;
#61101 = DIRECTION ( 'NONE',  ( -0.000000000000000000, -0.000000000000000000, -1.000000000000000000 ) ) ;
#61102 = VECTOR ( 'NONE', #46845, 1000.000000000000000 ) ;
#61103 = CARTESIAN_POINT ( 'NONE',  ( 44.25000000000000000, 21.74999999999998579, 4.000000000000000000 ) ) ;
#61104 = EDGE_CURVE ( 'NONE', #37003, #36322, #53110, .T. ) ;
#61105 =( LENGTH_UNIT ( ) NAMED_UNIT ( * ) SI_UNIT ( .MILLI., .METRE. ) );
#61106 = VECTOR ( 'NONE', #43482, 1000.000000000000000 ) ;
#61107 = CARTESIAN_POINT ( 'NONE',  ( 48.25000000000000000, 22.24999999999998579, -3.750000000000000000 ) ) ;
#61108 = CARTESIAN_POINT ( 'NONE',  ( 71.50000000000000000, 14.49137674618942562, -9.500000000000000000 ) ) ;
#61109 = CIRCLE ( 'NONE', #58872, 0.2500000000000002220 ) ;
#61110 = DIRECTION ( 'NONE',  ( 0.000000000000000000, 1.000000000000000000, 0.000000000000000000 ) ) ;
#61111 =( NAMED_UNIT ( * ) SI_UNIT ( $, .STERADIAN. ) SOLID_ANGLE_UNIT ( ) );
#61112 = VERTEX_POINT ( 'NONE', #23749 ) ;
#61113 = VERTEX_POINT ( 'NONE', #49806 ) ;
#61114 = AXIS2_PLACEMENT_3D ( 'NONE', #8706, #30127, #3370 ) ;
#61115 = SURFACE_SIDE_STYLE ('',( #66386 ) ) ;
#61116 = LINE ( 'NONE', #49896, #30449 ) ;
#61117 = CARTESIAN_POINT ( 'NONE',  ( 57.74999999999998579, 30.74999999999999289, 4.000000000000000000 ) ) ;
#61118 = SURFACE_STYLE_USAGE ( .BOTH. , #18214 ) ;
#61119 = ORIENTED_EDGE ( 'NONE', *, *, #59447, .T. ) ;
#61120 = ORIENTED_EDGE ( 'NONE', *, *, #38326, .F. ) ;
#61121 = FILL_AREA_STYLE_COLOUR ( '', #51148 ) ;
#61122 = DIRECTION ( 'NONE',  ( 0.000000000000000000, 0.000000000000000000, -1.000000000000000000 ) ) ;
#61123 = COLOUR_RGB ( '', 0.09019608, 0.27058824, 0.51372549) ;
#61124 = ORIENTED_EDGE ( 'NONE', *, *, #30172, .F. ) ;
#61125 =( NAMED_UNIT ( * ) PLANE_ANGLE_UNIT ( ) SI_UNIT ( $, .RADIAN. ) );
#61126 = DIRECTION ( 'NONE',  ( 0.000000000000000000, 0.000000000000000000, 1.000000000000000000 ) ) ;
#61127 = ORIENTED_EDGE ( 'NONE', *, *, #9064, .T. ) ;
#61128 = EDGE_CURVE ( 'NONE', #42152, #45776, #39969, .T. ) ;
#61129 = AXIS2_PLACEMENT_3D ( 'NONE', #7864, #23703, #13140 ) ;
#61130 = DIRECTION ( 'NONE',  ( 0.000000000000000000, 0.000000000000000000, 1.000000000000000000 ) ) ;
#61131 = CARTESIAN_POINT ( 'NONE',  ( -124.7949999999999733, 2.607480562269068880, -8.024999999999993250 ) ) ;
#61132 = ORIENTED_EDGE ( 'NONE', *, *, #62095, .T. ) ;
#61133 = AXIS2_PLACEMENT_3D ( 'NONE', #41379, #58565, #4372 ) ;
#61134 = ORIENTED_EDGE ( 'NONE', *, *, #25323, .F. ) ;
#61135 = MECHANICAL_DESIGN_GEOMETRIC_PRESENTATION_REPRESENTATION (  '', ( #25195 ), #51309 ) ;
#61136 = SURFACE_STYLE_FILL_AREA ( #60770 ) ;
#61137 = DIRECTION ( 'NONE',  ( 0.000000000000000000, 0.000000000000000000, 1.000000000000000000 ) ) ;
#61138 = CARTESIAN_POINT ( 'NONE',  ( -10.00006165262988134, -11.99997431140458382, 0.3302327102163540307 ) ) ;
#61139 = EDGE_CURVE ( 'NONE', #61023, #8546, #23917, .T. ) ;
#61140 = CARTESIAN_POINT ( 'NONE',  ( -8.690363669209109077, -2.361802048420726496, -2.947848588679145454 ) ) ;
#61141 = AXIS2_PLACEMENT_3D ( 'NONE', #36922, #52400, #62561 ) ;
#61142 = ORIENTED_EDGE ( 'NONE', *, *, #10386, .F. ) ;
#61143 = CARTESIAN_POINT ( 'NONE',  ( 4.716976649647099507, 146.6429263765338078, -6.492361379858953008 ) ) ;
#61144 = DIRECTION ( 'NONE',  ( -1.000000000000000000, 0.000000000000000000, 0.000000000000000000 ) ) ;
#61145 = VECTOR ( 'NONE', #25545, 1000.000000000000000 ) ;
#61146 = EDGE_CURVE ( 'NONE', #65666, #43970, #36318, .T. ) ;
#61147 = CARTESIAN_POINT ( 'NONE',  ( 0.000000000000000000, 0.000000000000000000, 1.000000000000000000 ) ) ;
#61148 = ORIENTED_EDGE ( 'NONE', *, *, #43039, .T. ) ;
#61149 = SURFACE_STYLE_USAGE ( .BOTH. , #44338 ) ;
#61150 = ORIENTED_EDGE ( 'NONE', *, *, #49053, .T. ) ;
#61151 = CARTESIAN_POINT ( 'NONE',  ( 3.749999999999999556, 34.24999999999998579, -4.000000000000000000 ) ) ;
#61152 = CARTESIAN_POINT ( 'NONE',  ( -9.827790563157511022E-16, 140.5570736234661524, 8.025000000000000355 ) ) ;
#61153 = DIRECTION ( 'NONE',  ( -0.000000000000000000, -0.000000000000000000, -1.000000000000000000 ) ) ;
#61154 = CARTESIAN_POINT ( 'NONE',  ( -157.7070736234665276, -3.094860106623708251, -9.524999999996159872 ) ) ;
#61155 = CARTESIAN_POINT ( 'NONE',  ( -132.6550000000000011, -7.632228543268600340, -2.479861379858950166 ) ) ;
#61156 = DIRECTION ( 'NONE',  ( 0.000000000000000000, 1.000000000000000000, 0.000000000000000000 ) ) ;
#61157 = ORIENTED_EDGE ( 'NONE', *, *, #49981, .F. ) ;
#61158 = COLOUR_RGB ( '', 0.31764706, 0.68627451, 0.89019608) ;
#61159 = FACE_OUTER_BOUND ( 'NONE', #32029, .T. ) ;
#61160 = CARTESIAN_POINT ( 'NONE',  ( 0.4142135623730929250, 14.00000000000000355, 35.49999999999999289 ) ) ;
#61161 = DIRECTION ( 'NONE',  ( -2.168404344971007882E-16, 0.000000000000000000, -1.000000000000000000 ) ) ;
#61162 = VERTEX_POINT ( 'NONE', #60672 ) ;
#61163 = ORIENTED_EDGE ( 'NONE', *, *, #169, .T. ) ;
#61164 = DIRECTION ( 'NONE',  ( 0.000000000000000000, 0.000000000000000000, -1.000000000000000000 ) ) ;
#61165 = CARTESIAN_POINT ( 'NONE',  ( 5.710692600061823221, -2.500000000000000000, -4.108790270285303414 ) ) ;
#61166 = EDGE_CURVE ( 'NONE', #10616, #52417, #12489, .T. ) ;
#61167 = CARTESIAN_POINT ( 'NONE',  ( -108.7429263765338021, -5.598654528085803328, -7.705886871421366635 ) ) ;
#61169 = DIRECTION ( 'NONE',  ( 1.000000000000000000, -0.000000000000000000, -0.000000000000000000 ) ) ;
#61168 = AXIS2_PLACEMENT_3D ( 'NONE', #9561, #14830, #46882 ) ;
#61170 = ORIENTED_EDGE ( 'NONE', *, *, #21432, .F. ) ;
#61171 = CARTESIAN_POINT ( 'NONE',  ( -91.79292637653496456, -3.094860106599068406, 9.525000000014060220 ) ) ;
#61172 = CARTESIAN_POINT ( 'NONE',  ( 15.98999599679679839, 146.4999999999999716, -7.500000000000000000 ) ) ;
#61173 = AXIS2_PLACEMENT_3D ( 'NONE', #30220, #3464, #14078 ) ;
#61174 = AXIS2_PLACEMENT_3D ( 'NONE', #1557, #39979, #12854 ) ;
#61175 = DIRECTION ( 'NONE',  ( 0.000000000000000000, 0.000000000000000000, 1.000000000000000000 ) ) ;
#61176 = ORIENTED_EDGE ( 'NONE', *, *, #12062, .T. ) ;
#61177 = SURFACE_SIDE_STYLE ('',( #7378 ) ) ;
#61178 = CARTESIAN_POINT ( 'NONE',  ( 3.999798566743339556, 8.867945265733707672, 2.000000000000000000 ) ) ;
#61179 = CARTESIAN_POINT ( 'NONE',  ( 7.000000000000017764, 17.78868675966041835, -9.106839746483067901E-16 ) ) ;
#61180 = CARTESIAN_POINT ( 'NONE',  ( -106.5549999999999784, 0.000000000000000000, 8.024999999999991473 ) ) ;
#61181 = CARTESIAN_POINT ( 'NONE',  ( -27.32592744009309982, -8.499999999999996447, 0.03801221658426125888 ) ) ;
#61182 = PRESENTATION_STYLE_ASSIGNMENT (( #33749 ) ) ;
#61183 = DIRECTION ( 'NONE',  ( -9.376883653928687363E-17, -1.000000000000000000, 0.000000000000000000 ) ) ;
#61184 = TOROIDAL_SURFACE ( 'NONE', #32011, 14.49999999999999822, 0.5000000000000000000 ) ;
#61185 = CIRCLE ( 'NONE', #37641, 13.76969600708472008 ) ;
#61186 = CARTESIAN_POINT ( 'NONE',  ( -97.34499999999998465, 7.632228543268599452, -2.479861379858951942 ) ) ;
#61187 = CARTESIAN_POINT ( 'NONE',  ( -9.058813317711338797, 117.4549999999999841, 2.943386871421373563 ) ) ;
#61188 = CARTESIAN_POINT ( 'NONE',  ( -78.74499999999997613, 4.716976649647094177, 6.492361379858945902 ) ) ;
#61189 = FILL_AREA_STYLE_COLOUR ( '', #25199 ) ;
#61190 = CIRCLE ( 'NONE', #64566, 0.2500000000000002220 ) ;
#61191 = CARTESIAN_POINT ( 'NONE',  ( 0.000000000000000000, 13.00000000000000178, 36.50000000000000000 ) ) ;
#61192 = CYLINDRICAL_SURFACE ( 'NONE', #59777, 0.2500000000000002220 ) ;
#61193 =( BOUNDED_SURFACE ( )  B_SPLINE_SURFACE ( 3, 2, ( 
 ( #23818, #45323, #18560 ),
 ( #56162, #13250, #40042 ),
 ( #61430, #24162, #9668 ),
 ( #21216, #42398, #56515 ),
 ( #42050, #3000, #63454 ),
 ( #63788, #10682, #51258 ),
 ( #15631, #57844, #40362 ),
 ( #20179, #37111, #58179 ),
 ( #15306, #61774, #15989 ),
 ( #52909, #32132, #31416 ) ),
 .UNSPECIFIED., .F., .F., .F. ) 
 B_SPLINE_SURFACE_WITH_KNOTS ( ( 4, 2, 2, 2, 4 ),
 ( 3, 3 ),
 ( 0.0004231141141892710367, 0.0008386083364002310404, 0.001254102558611191152, 0.001669596780822151265, 0.002085091003033111377 ),
 ( 0.000000000000000000, 1.000000000000000000 ),
 .UNSPECIFIED. ) 
 GEOMETRIC_REPRESENTATION_ITEM ( )  RATIONAL_B_SPLINE_SURFACE ( (
 ( 1.000000000000000000, 0.7071067811865573427, 1.000000000000000000),
 ( 1.000000000000000000, 0.7275888720224806816, 1.000000000000000000),
 ( 1.000000000000000000, 0.7463828630404263365, 1.000000000000000000),
 ( 1.000000000000000000, 0.7812714640742435268, 1.000000000000000000),
 ( 1.000000000000000000, 0.7963642535525788935, 1.000000000000000000),
 ( 1.000000000000000000, 0.8224433532025096083, 1.000000000000000000),
 ( 1.000000000000000000, 0.8326146287104877475, 1.000000000000000000),
 ( 1.000000000000000000, 0.8468497872537316118, 1.000000000000000000),
 ( 1.000000000000000000, 0.8504932968929420634, 1.000000000000000000),
 ( 1.000000000000000000, 0.8505317485662416965, 1.000000000000000000) ) ) 
 REPRESENTATION_ITEM ( '' )  SURFACE ( )  );
#61194 = CARTESIAN_POINT ( 'NONE',  ( 29.00000000000002842, 0.000000000000000000, 89.00000000000000000 ) ) ;
#61195 = CARTESIAN_POINT ( 'NONE',  ( -195.0000000000000000, 0.000000000000000000, 0.000000000000000000 ) ) ;
#61196 = VERTEX_POINT ( 'NONE', #35000 ) ;
#61197 = CARTESIAN_POINT ( 'NONE',  ( -118.4929263765338021, -8.102448949553172852, 5.886773742842742685 ) ) ;
#61198 = CIRCLE ( 'NONE', #23051, 0.2500000000000002220 ) ;
#61199 = DIRECTION ( 'NONE',  ( 0.000000000000000000, 0.000000000000000000, 1.000000000000000000 ) ) ;
#61200 = CARTESIAN_POINT ( 'NONE',  ( -135.2950000000000159, -2.607480562269069768, 8.024999999999991473 ) ) ;
#61201 = DIRECTION ( 'NONE',  ( 0.000000000000000000, 0.000000000000000000, -1.000000000000000000 ) ) ;
#61202 = CARTESIAN_POINT ( 'NONE',  ( 16.00000000000001776, 15.00000000000000000, 34.68999999999999062 ) ) ;
#61203 = ORIENTED_EDGE ( 'NONE', *, *, #68679, .F. ) ;
#61204 = VERTEX_POINT ( 'NONE', #57861 ) ;
#61205 = CARTESIAN_POINT ( 'NONE',  ( -28.65793721421424323, -7.646217233412910375, -0.2644437612820810801 ) ) ;
#61206 = LINE ( 'NONE', #18656, #24082 ) ;
#61207 = AXIS2_PLACEMENT_3D ( 'NONE', #65775, #3073, #34788 ) ;
#61208 = PRESENTATION_LAYER_ASSIGNMENT (  '', '', ( #43300 ) ) ;
#61209 = SURFACE_STYLE_FILL_AREA ( #66494 ) ;
#61210 = CARTESIAN_POINT ( 'NONE',  ( -131.6070736234661922, -8.102448949553174629, 5.886773742842742685 ) ) ;
#61211 = DIRECTION ( 'NONE',  ( 1.000000000000000000, 0.000000000000000000, 0.000000000000000000 ) ) ;
#61212 = DIRECTION ( 'NONE',  ( -1.000000000000000000, 0.000000000000000000, 0.000000000000000000 ) ) ;
#61213 = VERTEX_POINT ( 'NONE', #30384 ) ;
#61214 = CARTESIAN_POINT ( 'NONE',  ( -129.0549999999999784, -9.827790563157499189E-16, -8.024999999999991473 ) ) ;
#61215 = ORIENTED_EDGE ( 'NONE', *, *, #6709, .T. ) ;
#61216 = CIRCLE ( 'NONE', #67972, 0.5000000000000000000 ) ;
#61217 = ORIENTED_EDGE ( 'NONE', *, *, #30657, .F. ) ;
#61218 = DIRECTION ( 'NONE',  ( -1.000000000000000000, 0.000000000000000000, 0.000000000000000000 ) ) ;
#61219 = LINE ( 'NONE', #17645, #64657 ) ;
#61220 = ORIENTED_EDGE ( 'NONE', *, *, #65591, .F. ) ;
#61221 = EDGE_CURVE ( 'NONE', #30521, #28945, #19505, .T. ) ;
#61222 = VECTOR ( 'NONE', #34722, 1000.000000000000000 ) ;
#61223 = COLOUR_RGB ( '', 0.40784314, 0.44705882, 0.49803922) ;
#61224 = DIRECTION ( 'NONE',  ( 1.156482317317873451E-16, -1.000000000000000000, -0.000000000000000000 ) ) ;
#61225 = DIRECTION ( 'NONE',  ( 0.000000000000000000, 0.000000000000000000, -1.000000000000000000 ) ) ;
#61226 = CARTESIAN_POINT ( 'NONE',  ( 3.094860106618435136, 142.2950000000000159, -9.525000000000000355 ) ) ;
#61227 = DIRECTION ( 'NONE',  ( 0.000000000000000000, -0.000000000000000000, 1.000000000000000000 ) ) ;
#61228 = ORIENTED_EDGE ( 'NONE', *, *, #28096, .F. ) ;
#61229 = DIRECTION ( 'NONE',  ( 0.000000000000000000, 0.000000000000000000, -1.000000000000000000 ) ) ;
#61230 = CARTESIAN_POINT ( 'NONE',  ( -5.598654528085806881, 140.8549999999999898, -7.705886871421374629 ) ) ;
#61231 = FACE_OUTER_BOUND ( 'NONE', #47868, .T. ) ;
#61232 = ORIENTED_EDGE ( 'NONE', *, *, #32031, .F. ) ;
#61233 = CARTESIAN_POINT ( 'NONE',  ( -9.058813317711338797, 153.4549999999999841, 2.943386871421373563 ) ) ;
#61234 = DIRECTION ( 'NONE',  ( 8.659560562354962440E-17, 0.7071067811865451302, -0.7071067811865500152 ) ) ;
#61235 = DIRECTION ( 'NONE',  ( 0.000000000000000000, 0.000000000000000000, -1.000000000000000000 ) ) ;
#61236 = AXIS2_PLACEMENT_3D ( 'NONE', #43781, #44486, #24015 ) ;
#61237 = EDGE_CURVE ( 'NONE', #46312, #42163, #24771, .T. ) ;
#61238 = ORIENTED_EDGE ( 'NONE', *, *, #29221, .F. ) ;
#61239 = EDGE_CURVE ( 'NONE', #32321, #21436, #49739, .T. ) ;
#61240 = AXIS2_PLACEMENT_3D ( 'NONE', #36371, #15254, #20491 ) ;
#61241 = SURFACE_STYLE_FILL_AREA ( #66523 ) ;
#61242 = ORIENTED_EDGE ( 'NONE', *, *, #2760, .F. ) ;
#61243 = SURFACE_STYLE_FILL_AREA ( #66161 ) ;
#61244 = CARTESIAN_POINT ( 'NONE',  ( -122.1570736234661751, -9.058813317711329915, -2.943386871421370898 ) ) ;
#61245 = DIRECTION ( 'NONE',  ( 1.000000000000000000, 0.000000000000000000, 0.000000000000000000 ) ) ;
#61246 = CARTESIAN_POINT ( 'NONE',  ( -160.2549999999999670, -4.716976649647092401, 6.492361379858946790 ) ) ;
#61248 = VERTEX_POINT ( 'NONE', #62427 ) ;
#61247 = ADVANCED_FACE ( 'NONE', ( #9682 ), #56500, .T. ) ;
#61249 = STYLED_ITEM ( 'NONE', ( #38856 ), #56460 ) ;
#61250 = EDGE_CURVE ( 'NONE', #13259, #66860, #12716, .T. ) ;
#61251 = CARTESIAN_POINT ( 'NONE',  ( -44.99999999999977973, 149.4999999999999716, 9.500000000000000000 ) ) ;
#61252 =( NAMED_UNIT ( * ) PLANE_ANGLE_UNIT ( ) SI_UNIT ( $, .RADIAN. ) );
#61253 = SURFACE_SIDE_STYLE ('',( #50706 ) ) ;
#61254 = ORIENTED_EDGE ( 'NONE', *, *, #45159, .T. ) ;
#61255 = ORIENTED_EDGE ( 'NONE', *, *, #42698, .F. ) ;
#61256 = DIRECTION ( 'NONE',  ( -1.000000000000000000, 0.000000000000000000, 0.000000000000000000 ) ) ;
#61257 = CARTESIAN_POINT ( 'NONE',  ( -77.45499999999998408, 7.632228543268599452, -2.479861379858951942 ) ) ;
#61258 = ORIENTED_EDGE ( 'NONE', *, *, #68364, .T. ) ;
#61259 = CARTESIAN_POINT ( 'NONE',  ( -64.55707362346618083, -1.166476076187852838E-15, -9.524999999999991473 ) ) ;
#61260 = CARTESIAN_POINT ( 'NONE',  ( 0.000000000000000000, 13.00000000000000178, 80.00402776293826435 ) ) ;
#61261 = AXIS2_PLACEMENT_3D ( 'NONE', #69055, #63062, #30007 ) ;
#61262 =( REPRESENTATION_RELATIONSHIP ('NONE','NONE', #5102, #6947 ) REPRESENTATION_RELATIONSHIP_WITH_TRANSFORMATION ( #68059 )SHAPE_REPRESENTATION_RELATIONSHIP( ) );
#61263 = PRESENTATION_LAYER_ASSIGNMENT (  '', '', ( #14130 ) ) ;
#61264 = ORIENTED_EDGE ( 'NONE', *, *, #53078, .T. ) ;
#61265 = CARTESIAN_POINT ( 'NONE',  ( -43.75000000000000000, 4.336808689942018722E-16, -5.099999999999999645 ) ) ;
#61266 = COLOUR_RGB ( '', 0.08235294, 0.09019608, 0.10196078) ;
#61267 = CARTESIAN_POINT ( 'NONE',  ( -8.102448949553181734, 142.8949999999999818, -5.886773742842749790 ) ) ;
#61268 = CARTESIAN_POINT ( 'NONE',  ( -109.4949999999999761, 6.826472737025113702, -4.959722759717902107 ) ) ;
#61269 = AXIS2_PLACEMENT_3D ( 'NONE', #20208, #69117, #25833 ) ;
#61270 = PRESENTATION_LAYER_ASSIGNMENT (  '', '', ( #56770 ) ) ;
#61271 = CARTESIAN_POINT ( 'NONE',  ( -72.50000000000000000, 35.92875272052971525, -9.500000000000000000 ) ) ;
#61273 = DIRECTION ( 'NONE',  ( 1.000000000000000000, 0.000000000000000000, 0.000000000000000000 ) ) ;
#61272 = DIRECTION ( 'NONE',  ( -0.000000000000000000, 0.000000000000000000, 1.000000000000000000 ) ) ;
#61274 = CARTESIAN_POINT ( 'NONE',  ( -141.8929263765337794, -8.102448949553172852, -5.886773742842741797 ) ) ;
#61275 = PRESENTATION_STYLE_ASSIGNMENT (( #40192 ) ) ;
#61276 = CARTESIAN_POINT ( 'NONE',  ( -166.9450000000000216, -9.827790563157499189E-16, -8.024999999999991473 ) ) ;
#61277 = CIRCLE ( 'NONE', #5130, 0.5000000000000004441 ) ;
#61278 = DIRECTION ( 'NONE',  ( 1.000000000000000000, 0.000000000000000000, 0.000000000000000000 ) ) ;
#61279 = PRESENTATION_LAYER_ASSIGNMENT (  '', '', ( #6252 ) ) ;
#61280 =( NAMED_UNIT ( * ) PLANE_ANGLE_UNIT ( ) SI_UNIT ( $, .RADIAN. ) );
#61281 = ORIENTED_EDGE ( 'NONE', *, *, #12860, .F. ) ;
#61282 = CARTESIAN_POINT ( 'NONE',  ( -4.716976649647098618, 128.2570736234661695, 6.492361379858953008 ) ) ;
#61283 = ORIENTED_EDGE ( 'NONE', *, *, #29777, .T. ) ;
#61284 =( GEOMETRIC_REPRESENTATION_CONTEXT ( 3 ) GLOBAL_UNCERTAINTY_ASSIGNED_CONTEXT ( ( #60157 ) ) GLOBAL_UNIT_ASSIGNED_CONTEXT ( ( #39117, #34488, #29188 ) ) REPRESENTATION_CONTEXT ( 'NONE', 'WORKASPACE' ) );
#61285 = PRESENTATION_STYLE_ASSIGNMENT (( #34549 ) ) ;
#61286 = DIRECTION ( 'NONE',  ( 0.000000000000000000, 0.000000000000000000, -1.000000000000000000 ) ) ;
#61287 = FILL_AREA_STYLE ('',( #60577 ) ) ;
#61288 = CARTESIAN_POINT ( 'NONE',  ( -71.18918918918917882, 14.09971791521133255, -7.500000000000000000 ) ) ;
#61289 = CARTESIAN_POINT ( 'NONE',  ( -71.74137931034481142, 36.89918356738973415, 10.00000000000000000 ) ) ;
#61290 = ORIENTED_EDGE ( 'NONE', *, *, #63392, .F. ) ;
#61291 = CARTESIAN_POINT ( 'NONE',  ( -160.8549999999999898, 4.716976649647094177, 6.492361379858945902 ) ) ;
#61292 = EDGE_LOOP ( 'NONE', ( #1376, #36648, #57427, #3190 ) ) ;
#61293 = CARTESIAN_POINT ( 'NONE',  ( -111.7429263765338163, -5.598654528085803328, -7.705886871421366635 ) ) ;
#61294 = ADVANCED_FACE ( 'NONE', ( #14242 ), #16120, .F. ) ;
#61295 = CYLINDRICAL_SURFACE ( 'NONE', #43947, 5.000000000000000888 ) ;
#61296 = FILL_AREA_STYLE ('',( #13451 ) ) ;
#61297 = CARTESIAN_POINT ( 'NONE',  ( 4.716976649647099507, 159.7570736234661695, -6.492361379858953008 ) ) ;
#61298 = EDGE_CURVE ( 'NONE', #51919, #23561, #62617, .T. ) ;
#61299 = AXIS2_PLACEMENT_3D ( 'NONE', #15009, #30434, #24470 ) ;
#61300 = ORIENTED_EDGE ( 'NONE', *, *, #173, .F. ) ;
#61301 = CARTESIAN_POINT ( 'NONE',  ( 73.01088739851488185, 5.000000000000000000, -65.71817553072278884 ) ) ;
#61302 = CARTESIAN_POINT ( 'NONE',  ( -8.102448949553179958, 114.6049999999999756, 5.886773742842747126 ) ) ;
#61303 = CARTESIAN_POINT ( 'NONE',  ( -85.85499999999998977, 4.716976649647094177, 6.492361379858945902 ) ) ;
#61304 = PRESENTATION_STYLE_ASSIGNMENT (( #2140 ) ) ;
#61305 = CARTESIAN_POINT ( 'NONE',  ( 3.094860106618435136, 128.4049999999999443, -9.525000000000000355 ) ) ;
#61306 = FILL_AREA_STYLE_COLOUR ( '', #16327 ) ;
#61307 =( GEOMETRIC_REPRESENTATION_CONTEXT ( 3 ) GLOBAL_UNCERTAINTY_ASSIGNED_CONTEXT ( ( #26315 ) ) GLOBAL_UNIT_ASSIGNED_CONTEXT ( ( #3529, #35948, #68300 ) ) REPRESENTATION_CONTEXT ( 'NONE', 'WORKASPACE' ) );
#61308 = EDGE_CURVE ( 'NONE', #59005, #10834, #2576, .T. ) ;
#61309 = PRESENTATION_LAYER_ASSIGNMENT (  '', '', ( #36677 ) ) ;
#61310 = VERTEX_POINT ( 'NONE', #43463 ) ;
#61311 = AXIS2_PLACEMENT_3D ( 'NONE', #27011, #36623, #27362 ) ;
#61312 = CYLINDRICAL_SURFACE ( 'NONE', #23884, 13.99999999999999822 ) ;
#61313 = SURFACE_SIDE_STYLE ('',( #34247 ) ) ;
#61314 = CARTESIAN_POINT ( 'NONE',  ( -54.89499999999997470, 6.826472737025116366, 4.959722759717898555 ) ) ;
#61315 = ORIENTED_EDGE ( 'NONE', *, *, #8958, .T. ) ;
#61316 =( LENGTH_UNIT ( ) NAMED_UNIT ( * ) SI_UNIT ( .MILLI., .METRE. ) );
#61317 = LINE ( 'NONE', #2157, #16215 ) ;
#61318 = EDGE_CURVE ( 'NONE', #17308, #57515, #11619, .T. ) ;
#61319 = DIRECTION ( 'NONE',  ( 0.000000000000000000, -1.000000000000000000, 0.000000000000000000 ) ) ;
#61320 = ORIENTED_EDGE ( 'NONE', *, *, #48887, .F. ) ;
#61321 = CARTESIAN_POINT ( 'NONE',  ( -52.84851010692981532, -10.65464120701058803, 2.183759428457559437 ) ) ;
#61322 = CARTESIAN_POINT ( 'NONE',  ( -50.99499999999998323, -6.826472737025113702, 4.959722759717902107 ) ) ;
#61323 = ORIENTED_EDGE ( 'NONE', *, *, #19040, .T. ) ;
#61324 = AXIS2_PLACEMENT_3D ( 'NONE', #36165, #31181, #68857 ) ;
#61325 = CARTESIAN_POINT ( 'NONE',  ( -75.00000000000000000, 8.189706559487058612, 5.659622407586515358 ) ) ;
#61326 = CARTESIAN_POINT ( 'NONE',  ( -105.9549999999999983, -7.632228543268599452, 2.479861379858951054 ) ) ;
#61327 = EDGE_LOOP ( 'NONE', ( #30722, #1262, #67427, #23101 ) ) ;
#61328 = SURFACE_STYLE_USAGE ( .BOTH. , #17752 ) ;
#61329 = CARTESIAN_POINT ( 'NONE',  ( -60.00000000000000000, -2.024042244987997205E-14, -10.49999999999999822 ) ) ;
#61330 = AXIS2_PLACEMENT_3D ( 'NONE', #12024, #59505, #32422 ) ;
#61331 = CARTESIAN_POINT ( 'NONE',  ( -145.2570736234661695, 5.598654528085800663, -7.705886871421367523 ) ) ;
#61332 = CARTESIAN_POINT ( 'NONE',  ( -58.55707362346616662, -1.166476076187852838E-15, -9.524999999999991473 ) ) ;
#61333 = CARTESIAN_POINT ( 'NONE',  ( -8.102448949553179958, 139.8949999999999818, -5.886773742842749790 ) ) ;
#61334 = AXIS2_PLACEMENT_3D ( 'NONE', #34055, #65379, #44660 ) ;
#61335 = CARTESIAN_POINT ( 'NONE',  ( -84.50707362346616947, 8.102448949553176405, 5.886773742842740909 ) ) ;
#61336 = CARTESIAN_POINT ( 'NONE',  ( -96.29292637653490772, 3.094860106600143101, -9.525000000013280399 ) ) ;
#61337 = CARTESIAN_POINT ( 'NONE',  ( 27.99999999999998934, 5.000000000000000000, -37.00402776293828566 ) ) ;
#61338 = CARTESIAN_POINT ( 'NONE',  ( 0.000000000000000000, 121.0570736234661524, -8.025000000000000355 ) ) ;
#61339 = CARTESIAN_POINT ( 'NONE',  ( -124.7049999999999841, 2.607480562269073321, 8.024999999999991473 ) ) ;
#61340 = CARTESIAN_POINT ( 'NONE',  ( -22.25000000000000711, 34.24999999999999289, 3.750000000000000000 ) ) ;
#61341 = CARTESIAN_POINT ( 'NONE',  ( 24.70577775730027881, 26.00000000000004619, -27.50000000000000711 ) ) ;
#61342 = CARTESIAN_POINT ( 'NONE',  ( -3.094860106618434248, 110.7949999999999733, 9.525000000000000355 ) ) ;
#61343 = CARTESIAN_POINT ( 'NONE',  ( -137.6949999999999932, -8.437984349512085203, 5.166775262442717831E-16 ) ) ;
#61344 = CARTESIAN_POINT ( 'NONE',  ( -128.2450000000000045, -4.716976649647093289, -6.492361379858945902 ) ) ;
#61345 = LINE ( 'NONE', #18788, #12204 ) ;
#61346 = EDGE_LOOP ( 'NONE', ( #10183, #13072, #69566, #46562 ) ) ;
#61347 = EDGE_CURVE ( 'NONE', #20689, #62163, #55398, .T. ) ;
#61348 = DIRECTION ( 'NONE',  ( 1.000000000000000000, 0.000000000000000000, 0.000000000000000000 ) ) ;
#61349 = STYLED_ITEM ( 'NONE', ( #33576 ), #8759 ) ;
#61350 = DIRECTION ( 'NONE',  ( 1.000000000000000000, -0.000000000000000000, -0.000000000000000000 ) ) ;
#61351 = LINE ( 'NONE', #61679, #36216 ) ;
#61352 = CARTESIAN_POINT ( 'NONE',  ( -178.0429263765338135, -9.058813317711329915, -2.943386871421370898 ) ) ;
#61353 = SHAPE_REPRESENTATION_RELATIONSHIP ( 'NONE' , 'NONE' ,  #6947, #14448 ) ;
#61354 = CARTESIAN_POINT ( 'NONE',  ( -52.64499999999999602, 4.716976649647091513, -6.492361379858946790 ) ) ;
#61355 = STYLED_ITEM ( 'NONE', ( #37598 ), #64822 ) ;
#61356 = VECTOR ( 'NONE', #34332, 1000.000000000000000 ) ;
#61357 =( NAMED_UNIT ( * ) SI_UNIT ( $, .STERADIAN. ) SOLID_ANGLE_UNIT ( ) );
#61358 = VECTOR ( 'NONE', #66153, 1000.000000000000000 ) ;
#61359 = DIRECTION ( 'NONE',  ( 0.000000000000000000, 0.000000000000000000, -1.000000000000000000 ) ) ;
#61360 = CARTESIAN_POINT ( 'NONE',  ( 29.00000000000002842, 42.00000000000000000, 80.00402776293826435 ) ) ;
#61361 = CARTESIAN_POINT ( 'NONE',  ( -97.34292637653379643, -9.058813317711329915, 2.943386871421371787 ) ) ;
#61362 = SHAPE_DEFINITION_REPRESENTATION ( #25409, #22166 ) ;
#61363 = SURFACE_STYLE_FILL_AREA ( #1537 ) ;
#61364 = DIRECTION ( 'NONE',  ( 1.000000000000000000, 0.000000000000000000, -0.000000000000000000 ) ) ;
#61365 = CARTESIAN_POINT ( 'NONE',  ( -71.50000000000000000, 35.92875272052971525, 7.500000000000000000 ) ) ;
#61366 =( NAMED_UNIT ( * ) PLANE_ANGLE_UNIT ( ) SI_UNIT ( $, .RADIAN. ) );
#61367 = CARTESIAN_POINT ( 'NONE',  ( -41.21596654039937846, 107.8367875949926713, 3.443506282739225988 ) ) ;
#61368 = ADVANCED_FACE ( 'NONE', ( #37127 ), #68880, .T. ) ;
#61369 = EDGE_CURVE ( 'NONE', #8081, #35716, #58775, .T. ) ;
#61370 = VERTEX_POINT ( 'NONE', #58191 ) ;
#61371 = DIRECTION ( 'NONE',  ( 0.000000000000000000, 0.000000000000000000, -1.000000000000000000 ) ) ;
#61372 = CARTESIAN_POINT ( 'NONE',  ( 9.827790563157511022E-16, 87.30187232391182306, -8.025000000000000355 ) ) ;
#61373 = ORIENTED_EDGE ( 'NONE', *, *, #13034, .T. ) ;
#61374 = CARTESIAN_POINT ( 'NONE',  ( -4.716976649647098618, 134.2570736234661695, 6.492361379858953008 ) ) ;
#61375 = CARTESIAN_POINT ( 'NONE',  ( 7.632228543268607446, 126.1570736234661467, 2.479861379858954606 ) ) ;
#61376 = EDGE_CURVE ( 'NONE', #35195, #65417, #65497, .T. ) ;
#61377 = CYLINDRICAL_SURFACE ( 'NONE', #4653, 17.42000000000001236 ) ;
#61378 =( NAMED_UNIT ( * ) SI_UNIT ( $, .STERADIAN. ) SOLID_ANGLE_UNIT ( ) );
#61379 = DIRECTION ( 'NONE',  ( 0.000000000000000000, 0.000000000000000000, 1.000000000000000000 ) ) ;
#61380 = ORIENTED_EDGE ( 'NONE', *, *, #48246, .T. ) ;
#61381 = DIRECTION ( 'NONE',  ( 0.000000000000000000, -0.000000000000000000, 1.000000000000000000 ) ) ;
#61382 = DIRECTION ( 'NONE',  ( 0.000000000000000000, 1.000000000000000000, 0.000000000000000000 ) ) ;
#61383 = DIRECTION ( 'NONE',  ( 0.000000000000000000, 0.000000000000000000, -1.000000000000000000 ) ) ;
#61384 = CARTESIAN_POINT ( 'NONE',  ( -178.9429263765338192, 0.000000000000000000, 9.524999999999991473 ) ) ;
#61385 = EDGE_CURVE ( 'NONE', #55490, #15666, #16007, .T. ) ;
#61386 = CARTESIAN_POINT ( 'NONE',  ( -80.39499999999998181, -6.826472737025115478, -4.959722759717899443 ) ) ;
#61387 = VERTEX_POINT ( 'NONE', #53275 ) ;
#61388 = FILL_AREA_STYLE ('',( #39991 ) ) ;
#61389 =( NAMED_UNIT ( * ) SI_UNIT ( $, .STERADIAN. ) SOLID_ANGLE_UNIT ( ) );
#61390 = EDGE_CURVE ( 'NONE', #18083, #24587, #30680, .T. ) ;
#61391 = UNCERTAINTY_MEASURE_WITH_UNIT (LENGTH_MEASURE( 1.000000000000000082E-05 ), #60699, 'distance_accuracy_value', 'NONE');
#61392 = ORIENTED_EDGE ( 'NONE', *, *, #24233, .T. ) ;
#61393 = SURFACE_STYLE_USAGE ( .BOTH. , #45275 ) ;
#61394 =( NAMED_UNIT ( * ) SI_UNIT ( $, .STERADIAN. ) SOLID_ANGLE_UNIT ( ) );
#61395 = ORIENTED_EDGE ( 'NONE', *, *, #32183, .T. ) ;
#61396 =( LENGTH_UNIT ( ) NAMED_UNIT ( * ) SI_UNIT ( .MILLI., .METRE. ) );
#61397 = ORIENTED_EDGE ( 'NONE', *, *, #35205, .T. ) ;
#61398 = CARTESIAN_POINT ( 'NONE',  ( -137.6929263765337623, 10.01517768586948698, -1.839758294383808966E-15 ) ) ;
#61399 =( GEOMETRIC_REPRESENTATION_CONTEXT ( 3 ) GLOBAL_UNCERTAINTY_ASSIGNED_CONTEXT ( ( #47593 ) ) GLOBAL_UNIT_ASSIGNED_CONTEXT ( ( #41028, #51541, #57157 ) ) REPRESENTATION_CONTEXT ( 'NONE', 'WORKASPACE' ) );
#61400 =( LENGTH_UNIT ( ) NAMED_UNIT ( * ) SI_UNIT ( .MILLI., .METRE. ) );
#61401 = CARTESIAN_POINT ( 'NONE',  ( -180.9570736234661865, 9.058813317711329915, -2.943386871421373119 ) ) ;
#61402 = CARTESIAN_POINT ( 'NONE',  ( -13.10261986875638129, 54.37406082015609599, -6.765796499695130528 ) ) ;
#61403 = CARTESIAN_POINT ( 'NONE',  ( 8.102448949553181734, 114.9949999999999903, -5.886773742842746238 ) ) ;
#61404 = CARTESIAN_POINT ( 'NONE',  ( -116.4570736234661723, -9.058813317711329915, 2.943386871421371787 ) ) ;
#61405 = CARTESIAN_POINT ( 'NONE',  ( -183.0586401562165975, 6.645247303096274649, -6.780310176063176542 ) ) ;
#61406 = DIRECTION ( 'NONE',  ( 1.224646799147353207E-16, 1.000000000000000000, -0.000000000000000000 ) ) ;
#61407 = ORIENTED_EDGE ( 'NONE', *, *, #24665, .F. ) ;
#61408 = DIRECTION ( 'NONE',  ( -1.000000000000000000, 0.000000000000000000, 0.000000000000000000 ) ) ;
#61409 = CARTESIAN_POINT ( 'NONE',  ( 45.02564408152620246, 10.00854802717538306, -3.127379285715777613 ) ) ;
#61410 = AXIS2_PLACEMENT_3D ( 'NONE', #12005, #29200, #66152 ) ;
#61411 = CARTESIAN_POINT ( 'NONE',  ( -162.8050000000000068, -8.437984349512085203, 5.166775262442717831E-16 ) ) ;
#61412 = CARTESIAN_POINT ( 'NONE',  ( 3.249999999999998668, 36.74999999999999289, 3.750000000000000000 ) ) ;
#61413 = CARTESIAN_POINT ( 'NONE',  ( -183.4829137129417234, -3.065004353576823881, -8.530224930386903992 ) ) ;
#61414 = CARTESIAN_POINT ( 'NONE',  ( -161.8449999999999989, -7.632228543268599452, 2.479861379858951054 ) ) ;
#61415 = CARTESIAN_POINT ( 'NONE',  ( -157.4950000000000045, 6.826472737025113702, -4.959722759717902107 ) ) ;
#61416 = ORIENTED_EDGE ( 'NONE', *, *, #23054, .T. ) ;
#61417 = EDGE_CURVE ( 'NONE', #55021, #28845, #54285, .T. ) ;
#61418 = DIRECTION ( 'NONE',  ( -1.000000000000000000, 0.000000000000000000, 0.000000000000000000 ) ) ;
#61419 = STYLED_ITEM ( 'NONE', ( #46749 ), #87 ) ;
#61420 = CARTESIAN_POINT ( 'NONE',  ( 7.794228634059946259, -2.500000000000000000, -4.500000000000001776 ) ) ;
#61421 = CARTESIAN_POINT ( 'NONE',  ( -73.55499999999997840, 0.000000000000000000, 8.024999999999991473 ) ) ;
#61422 = DIRECTION ( 'NONE',  ( -1.000000000000000000, 0.000000000000000000, 0.000000000000000000 ) ) ;
#61423 = CARTESIAN_POINT ( 'NONE',  ( 23.50000000000001776, -3.148064030671221758, -29.68999999999999417 ) ) ;
#61424 = CARTESIAN_POINT ( 'NONE',  ( -73.94499999999997897, -9.827790563157499189E-16, -8.024999999999991473 ) ) ;
#61425 = CARTESIAN_POINT ( 'NONE',  ( 5.598654528085805993, 148.3549999999999898, 7.705886871421374629 ) ) ;
#61426 = CARTESIAN_POINT ( 'NONE',  ( -60.00000000000000000, -2.024042244987997205E-14, -12.00000000000000000 ) ) ;
#61427 = PRESENTATION_STYLE_ASSIGNMENT (( #67080 ) ) ;
#61428 = UNCERTAINTY_MEASURE_WITH_UNIT (LENGTH_MEASURE( 1.000000000000000082E-05 ), #35686, 'distance_accuracy_value', 'NONE');
#61429 = FACE_OUTER_BOUND ( 'NONE', #40794, .T. ) ;
#61430 = CARTESIAN_POINT ( 'NONE',  ( -20.17690446313311625, 115.4776478016129460, -10.00000000000000000 ) ) ;
#61431 = EDGE_CURVE ( 'NONE', #62586, #58654, #10367, .T. ) ;
#61432 = MECHANICAL_DESIGN_GEOMETRIC_PRESENTATION_REPRESENTATION (  '', ( #26591 ), #42434 ) ;
#61433 = EDGE_CURVE ( 'NONE', #28127, #26382, #23969, .T. ) ;
#61434 = DIRECTION ( 'NONE',  ( 1.000000000000000000, 0.000000000000000000, 0.000000000000000000 ) ) ;
#61435 = EDGE_CURVE ( 'NONE', #823, #49817, #62119, .T. ) ;
#61436 = AXIS2_PLACEMENT_3D ( 'NONE', #28868, #55960, #8492 ) ;
#61437 = PRESENTATION_STYLE_ASSIGNMENT (( #50916 ) ) ;
#61438 = SURFACE_SIDE_STYLE ('',( #12563 ) ) ;
#61439 = ORIENTED_EDGE ( 'NONE', *, *, #46435, .F. ) ;
#61440 = ORIENTED_EDGE ( 'NONE', *, *, #50914, .F. ) ;
#61441 = CARTESIAN_POINT ( 'NONE',  ( -60.20707362346617231, 3.094860106618433360, 9.524999999999991473 ) ) ;
#61442 = CARTESIAN_POINT ( 'NONE',  ( 0.000000000000000000, 2.299999999999999822, -5.000000000000000000 ) ) ;
#61443 = ADVANCED_FACE ( 'NONE', ( #50664 ), #9378, .F. ) ;
#61444 = CARTESIAN_POINT ( 'NONE',  ( 4.750000000000002665, 22.24999999999998579, -4.000000000000000000 ) ) ;
#61445 =( BOUNDED_CURVE ( )  B_SPLINE_CURVE ( 2, ( #65718, #1285, #7333, #43962, #28397, #6277, #5922, #65377, #23166, #17559, #33367 ),
 .UNSPECIFIED., .F., .F. ) 
 B_SPLINE_CURVE_WITH_KNOTS ( ( 3, 2, 2, 2, 2, 3 ),
 ( 0.8260869565217391353, 0.8282608695652173836, 0.8304347826086956319, 0.8326086956521738802, 0.8347826086956521285, 0.8369565217391304879 ),
 .UNSPECIFIED. ) 
 CURVE ( )  GEOMETRIC_REPRESENTATION_ITEM ( )  RATIONAL_B_SPLINE_CURVE ( ( 1.000000000000000000, 0.9510565162951535312, 1.000000000000000000, 0.9510565162951535312, 1.000000000000000000, 0.9510565162951535312, 1.000000000000000000, 0.9510565162951535312, 1.000000000000000000, 0.9510565162951535312, 1.000000000000000000 ) ) 
 REPRESENTATION_ITEM ( '' )  );
#61446 = FACE_OUTER_BOUND ( 'NONE', #24715, .T. ) ;
#61447 = ADVANCED_FACE ( 'NONE', ( #67181 ), #60852, .F. ) ;
#61448 = VERTEX_POINT ( 'NONE', #29897 ) ;
#61449 = ORIENTED_EDGE ( 'NONE', *, *, #17869, .T. ) ;
#61450 = AXIS2_PLACEMENT_3D ( 'NONE', #2704, #56553, #23853 ) ;
#61451 = DIRECTION ( 'NONE',  ( -1.000000000000000000, -0.000000000000000000, -0.000000000000000000 ) ) ;
#61452 = ORIENTED_EDGE ( 'NONE', *, *, #26752, .F. ) ;
#61453 = CARTESIAN_POINT ( 'NONE',  ( -9.058813317711337021, 111.1549999999999869, -2.943386871421374895 ) ) ;
#61454 = CARTESIAN_POINT ( 'NONE',  ( -1.403516486455610890, 7.000000000000006217, 0.1310752030855656391 ) ) ;
#61455 = ORIENTED_EDGE ( 'NONE', *, *, #63847, .F. ) ;
#61456 = DIRECTION ( 'NONE',  ( 0.000000000000000000, 0.000000000000000000, -1.000000000000000000 ) ) ;
#61457 = CARTESIAN_POINT ( 'NONE',  ( -45.50000000000000000, 7.768687147774684831, 6.500000000000000000 ) ) ;
#61458 = CARTESIAN_POINT ( 'NONE',  ( -113.3949999999999818, -6.826472737025115478, -4.959722759717899443 ) ) ;
#61459 = ORIENTED_EDGE ( 'NONE', *, *, #68232, .F. ) ;
#61460 = VERTEX_POINT ( 'NONE', #40830 ) ;
#61461 = CARTESIAN_POINT ( 'NONE',  ( 0.000000000000000000, 110.4999999999999858, -9.525000000000000355 ) ) ;
#61462 = CARTESIAN_POINT ( 'NONE',  ( -54.29292637653379217, 3.094860106618428031, -9.524999999999993250 ) ) ;
#61463 = CARTESIAN_POINT ( 'NONE',  ( 24.68215867018893306, 26.35226335530614961, -27.48643897612095088 ) ) ;
#61464 = DIRECTION ( 'NONE',  ( -1.000000000000000000, 0.000000000000000000, 0.000000000000000000 ) ) ;
#61465 = ORIENTED_EDGE ( 'NONE', *, *, #8602, .F. ) ;
#61466 = CARTESIAN_POINT ( 'NONE',  ( -4.716976649647098618, 145.1429263765338078, 6.492361379858953008 ) ) ;
#61467 = CARTESIAN_POINT ( 'NONE',  ( -13.23915246117191025, 52.65078610323165265, 2.000000000000000000 ) ) ;
#61468 = CARTESIAN_POINT ( 'NONE',  ( 16.75000000000000711, 27.74999999999998224, 3.750000000000000000 ) ) ;
#61469 = ORIENTED_EDGE ( 'NONE', *, *, #45552, .T. ) ;
#61470 = SURFACE_SIDE_STYLE ('',( #35809 ) ) ;
#61471 = ORIENTED_EDGE ( 'NONE', *, *, #1201, .T. ) ;
#61472 =( LENGTH_UNIT ( ) NAMED_UNIT ( * ) SI_UNIT ( .MILLI., .METRE. ) );
#61473 = CYLINDRICAL_SURFACE ( 'NONE', #47931, 0.5000000000000004441 ) ;
#61474 = CARTESIAN_POINT ( 'NONE',  ( -137.7549999999999955, 4.716976649647091513, -6.492361379858946790 ) ) ;
#61475 = DIRECTION ( 'NONE',  ( 1.156482317317866302E-16, 1.000000000000000000, 0.000000000000000000 ) ) ;
#61476 = ADVANCED_FACE ( 'NONE', ( #38521 ), #43783, .T. ) ;
#61477 =( NAMED_UNIT ( * ) SI_UNIT ( $, .STERADIAN. ) SOLID_ANGLE_UNIT ( ) );
#61478 = ORIENTED_EDGE ( 'NONE', *, *, #33998, .T. ) ;
#61479 = DIRECTION ( 'NONE',  ( -0.000000000000000000, 0.000000000000000000, -1.000000000000000000 ) ) ;
#61480 = CARTESIAN_POINT ( 'NONE',  ( -107.1570736234661751, -9.058813317711329915, -2.943386871421370898 ) ) ;
#61481 = DIRECTION ( 'NONE',  ( -1.000000000000000000, 0.000000000000000000, 0.000000000000000000 ) ) ;
#61482 = VERTEX_POINT ( 'NONE', #65185 ) ;
#61483 = CIRCLE ( 'NONE', #13190, 0.5000000000000004441 ) ;
#61484 = EDGE_LOOP ( 'NONE', ( #39112, #10861, #56635 ) ) ;
#61485 = SURFACE_SIDE_STYLE ('',( #39745 ) ) ;
#61486 = MECHANICAL_DESIGN_GEOMETRIC_PRESENTATION_REPRESENTATION (  '', ( #21092 ), #7580 ) ;
#61487 = CARTESIAN_POINT ( 'NONE',  ( -20.86757785789463071, 115.0275815560950718, 10.00000000000000000 ) ) ;
#61488 = CARTESIAN_POINT ( 'NONE',  ( 8.082903768654761123, -1.417096231345241097, 9.294316082458970795E-16 ) ) ;
#61489 = DIRECTION ( 'NONE',  ( 1.000000000000000000, 2.127927463864883264E-14, 0.000000000000000000 ) ) ;
#61490 = VERTEX_POINT ( 'NONE', #51014 ) ;
#61491 = CIRCLE ( 'NONE', #34542, 1.000000000000000000 ) ;
#61492 = FILL_AREA_STYLE_COLOUR ( '', #58261 ) ;
#61493 = CARTESIAN_POINT ( 'NONE',  ( -51.20707362346615099, 3.094860106618433360, 9.524999999999991473 ) ) ;
#61494 = LINE ( 'NONE', #55898, #40804 ) ;
#61495 = CARTESIAN_POINT ( 'NONE',  ( 44.99999999999977973, 149.9999999999999716, 9.500000000000000000 ) ) ;
#61496 = ORIENTED_EDGE ( 'NONE', *, *, #2746, .T. ) ;
#61497 = LINE ( 'NONE', #24234, #52661 ) ;
#61498 = CARTESIAN_POINT ( 'NONE',  ( 0.000000000000000000, 112.0570736234661666, -8.025000000000000355 ) ) ;
#61499 = CARTESIAN_POINT ( 'NONE',  ( -97.85499999999998977, 4.716976649647094177, 6.492361379858945902 ) ) ;
#61500 = FACE_OUTER_BOUND ( 'NONE', #62702, .T. ) ;
#61502 = SURFACE_STYLE_FILL_AREA ( #40114 ) ;
#61501 =( GEOMETRIC_REPRESENTATION_CONTEXT ( 3 ) GLOBAL_UNCERTAINTY_ASSIGNED_CONTEXT ( ( #31156 ) ) GLOBAL_UNIT_ASSIGNED_CONTEXT ( ( #61759, #15021, #4401 ) ) REPRESENTATION_CONTEXT ( 'NONE', 'WORKASPACE' ) );
#61503 = CIRCLE ( 'NONE', #7638, 5.000000000000000000 ) ;
#61504 = CARTESIAN_POINT ( 'NONE',  ( -99.74499999999999034, 4.716976649647094177, 6.492361379858945902 ) ) ;
#61505 = CARTESIAN_POINT ( 'NONE',  ( -9.058813317711337021, 117.1549999999999869, -2.943386871421374895 ) ) ;
#61506 = CARTESIAN_POINT ( 'NONE',  ( -79.79500000000000171, 2.607480562269068880, -8.024999999999993250 ) ) ;
#61507 = EDGE_CURVE ( 'NONE', #60435, #55574, #64879, .T. ) ;
#61508 = DIRECTION ( 'NONE',  ( 0.000000000000000000, 1.000000000000000000, 0.000000000000000000 ) ) ;
#61509 = FILL_AREA_STYLE_COLOUR ( '', #22591 ) ;
#61510 = UNCERTAINTY_MEASURE_WITH_UNIT (LENGTH_MEASURE( 1.000000000000000082E-05 ), #760, 'distance_accuracy_value', 'NONE');
#61511 = CYLINDRICAL_SURFACE ( 'NONE', #48406, 3.000000000000000444 ) ;
#61512 = CARTESIAN_POINT ( 'NONE',  ( 66.74999999999998579, 34.24999999999999289, 3.750000000000000000 ) ) ;
#61513 = VERTEX_POINT ( 'NONE', #49065 ) ;
#61514 = ADVANCED_FACE ( 'NONE', ( #24593 ), #39797, .F. ) ;
#61515 = CARTESIAN_POINT ( 'NONE',  ( -114.2929263765338135, 3.094860106618428031, -9.524999999999993250 ) ) ;
#61516 = CARTESIAN_POINT ( 'NONE',  ( -138.7450000000000045, 4.716976649647094177, 6.492361379858945902 ) ) ;
#61517 = CARTESIAN_POINT ( 'NONE',  ( 29.00000000000002842, 38.70020753820971748, 89.00000000000000000 ) ) ;
#61518 = EDGE_CURVE ( 'NONE', #52256, #29481, #23570, .T. ) ;
#61519 = CARTESIAN_POINT ( 'NONE',  ( -4.357963766315036125, 6.451785339198147007, 0.7663918866669852115 ) ) ;
#61520 = CARTESIAN_POINT ( 'NONE',  ( 71.62068965517238439, 63.58603185604027885, -7.500000000000000000 ) ) ;
#61521 = CARTESIAN_POINT ( 'NONE',  ( -10.50000000000000178, 8.000000000000000000, 4.000000000000000000 ) ) ;
#61522 = EDGE_LOOP ( 'NONE', ( #53129, #19044, #29898, #25261 ) ) ;
#61523 = ORIENTED_EDGE ( 'NONE', *, *, #2107, .T. ) ;
#61524 = DIRECTION ( 'NONE',  ( -9.376883653928687363E-17, 1.000000000000000000, -0.000000000000000000 ) ) ;
#61525 = DIRECTION ( 'NONE',  ( -0.000000000000000000, -0.000000000000000000, 1.000000000000000000 ) ) ;
#61526 = CIRCLE ( 'NONE', #24429, 1.000000000000000000 ) ;
#61527 = DIRECTION ( 'NONE',  ( -0.000000000000000000, 0.000000000000000000, -1.000000000000000000 ) ) ;
#61528 = LINE ( 'NONE', #24263, #48387 ) ;
#61529 = COLOUR_RGB ( '', 0.31764706, 0.68627451, 0.89019608) ;
#61530 = CARTESIAN_POINT ( 'NONE',  ( 22.75000000000000711, 36.75000000000000000, -3.750000000000000000 ) ) ;
#61531 = AXIS2_PLACEMENT_3D ( 'NONE', #3687, #3330, #35046 ) ;
#61532 = EDGE_CURVE ( 'NONE', #18297, #56915, #12525, .T. ) ;
#61533 = ORIENTED_EDGE ( 'NONE', *, *, #20260, .T. ) ;
#61534 = CARTESIAN_POINT ( 'NONE',  ( -130.7049999999999841, 2.607480562269072433, 8.024999999999991473 ) ) ;
#61535 = VERTEX_POINT ( 'NONE', #15143 ) ;
#61536 = EDGE_LOOP ( 'NONE', ( #3994, #36052 ) ) ;
#61537 = CARTESIAN_POINT ( 'NONE',  ( 12.25000000000000355, 30.74999999999998579, -4.000000000000000000 ) ) ;
#61538 = DIRECTION ( 'NONE',  ( 0.000000000000000000, 0.000000000000000000, -1.000000000000000000 ) ) ;
#61539 = VERTEX_POINT ( 'NONE', #3459 ) ;
#61540 = CIRCLE ( 'NONE', #34595, 0.5000000000000004441 ) ;
#61541 = CARTESIAN_POINT ( 'NONE',  ( 86.21825843581756033, 5.000000000000000000, 39.83014742847163348 ) ) ;
#61542 =( LENGTH_UNIT ( ) NAMED_UNIT ( * ) SI_UNIT ( .MILLI., .METRE. ) );
#61543 = CARTESIAN_POINT ( 'NONE',  ( -8.102448949553181734, 143.4949999999999477, 5.886773742842747126 ) ) ;
#61544 = CARTESIAN_POINT ( 'NONE',  ( 7.647808743684392674, 154.4999999999999432, 5.677732506910178500 ) ) ;
#61545 = ORIENTED_EDGE ( 'NONE', *, *, #22023, .T. ) ;
#61546 =( NAMED_UNIT ( * ) SI_UNIT ( $, .STERADIAN. ) SOLID_ANGLE_UNIT ( ) );
#61547 = CARTESIAN_POINT ( 'NONE',  ( -3.094860106618432471, 143.7050000000000125, -9.525000000000000355 ) ) ;
#61548 = CARTESIAN_POINT ( 'NONE',  ( 18.25000000000000711, 33.99999999999999289, 3.750000000000000000 ) ) ;
#61549 = PLANE ( 'NONE',  #45327 ) ;
#61550 = VERTEX_POINT ( 'NONE', #25309 ) ;
#61551 = CARTESIAN_POINT ( 'NONE',  ( -2.607480562269075097, 118.2929263765338135, 8.025000000000000355 ) ) ;
#61552 = SURFACE_STYLE_USAGE ( .BOTH. , #3479 ) ;
#61553 = UNCERTAINTY_MEASURE_WITH_UNIT (LENGTH_MEASURE( 1.000000000000000082E-05 ), #11541, 'distance_accuracy_value', 'NONE');
#61554 =( GEOMETRIC_REPRESENTATION_CONTEXT ( 3 ) GLOBAL_UNCERTAINTY_ASSIGNED_CONTEXT ( ( #52320 ) ) GLOBAL_UNIT_ASSIGNED_CONTEXT ( ( #40269, #28979, #56789 ) ) REPRESENTATION_CONTEXT ( 'NONE', 'WORKASPACE' ) );
#61555 =( NAMED_UNIT ( * ) PLANE_ANGLE_UNIT ( ) SI_UNIT ( $, .RADIAN. ) );
#61556 = CYLINDRICAL_SURFACE ( 'NONE', #51165, 7.500000000000000000 ) ;
#61557 = EDGE_LOOP ( 'NONE', ( #10607, #23573, #28766, #41607 ) ) ;
#61558 = CARTESIAN_POINT ( 'NONE',  ( -6.938426666069068993, 1.982292489777645272, 0.2088670156639333142 ) ) ;
#61559 = ORIENTED_EDGE ( 'NONE', *, *, #12870, .F. ) ;
#61560 = CARTESIAN_POINT ( 'NONE',  ( 25.00000000000000355, 36.75000000000000000, -3.000000000000000000 ) ) ;
#61561 = DIRECTION ( 'NONE',  ( 0.000000000000000000, 0.000000000000000000, 1.000000000000000000 ) ) ;
#61562 = DIRECTION ( 'NONE',  ( 0.000000000000000000, -0.7071067811865496822, -0.7071067811865453523 ) ) ;
#61563 = CARTESIAN_POINT ( 'NONE',  ( -165.0550000000000068, -9.827790563157499189E-16, -8.024999999999991473 ) ) ;
#61564 = VERTEX_POINT ( 'NONE', #36618 ) ;
#61565 = ADVANCED_FACE ( 'NONE', ( #21070 ), #24957, .F. ) ;
#61566 = UNCERTAINTY_MEASURE_WITH_UNIT (LENGTH_MEASURE( 1.000000000000000082E-05 ), #18940, 'distance_accuracy_value', 'NONE');
#61567 = FACE_OUTER_BOUND ( 'NONE', #34734, .T. ) ;
#61568 = DIRECTION ( 'NONE',  ( -0.000000000000000000, -0.000000000000000000, 1.000000000000000000 ) ) ;
#61569 = DIRECTION ( 'NONE',  ( -0.000000000000000000, 1.000000000000000000, -0.000000000000000000 ) ) ;
#61570 =( NAMED_UNIT ( * ) PLANE_ANGLE_UNIT ( ) SI_UNIT ( $, .RADIAN. ) );
#61571 = VERTEX_POINT ( 'NONE', #26336 ) ;
#61572 = ORIENTED_EDGE ( 'NONE', *, *, #32371, .T. ) ;
#61573 = DIRECTION ( 'NONE',  ( 0.000000000000000000, 0.000000000000000000, -1.000000000000000000 ) ) ;
#61574 = DIRECTION ( 'NONE',  ( 1.000000000000000000, 0.000000000000000000, 0.000000000000000000 ) ) ;
#61575 = CARTESIAN_POINT ( 'NONE',  ( -75.50499999999998124, -6.826472737025115478, -4.959722759717899443 ) ) ;
#61576 = ORIENTED_EDGE ( 'NONE', *, *, #67032, .F. ) ;
#61577 = CIRCLE ( 'NONE', #31246, 4.000000000000000000 ) ;
#61578 = CARTESIAN_POINT ( 'NONE',  ( -63.35707362346617089, 5.598654528085804216, 7.705886871421366635 ) ) ;
#61579 =( BOUNDED_SURFACE ( )  B_SPLINE_SURFACE ( 3, 2, ( 
 ( #33491, #34525, #55981 ),
 ( #23973, #65502, #7790 ),
 ( #29239, #33828, #45488 ),
 ( #66906, #54920, #40182 ),
 ( #28178, #49690, #33162 ),
 ( #17688, #39155, #54597 ),
 ( #55289, #50042, #1777 ),
 ( #6403, #27832, #49337 ),
 ( #46528, #46885, #19739 ),
 ( #14131, #19022, #41233 ),
 ( #2826, #20072, #40534 ),
 ( #61946, #51071, #24646 ),
 ( #51412, #35588, #29600 ),
 ( #30981, #62633, #13411 ),
 ( #3156, #4220, #14456 ),
 ( #68285, #3513, #57028 ),
 ( #47215, #41572, #24319 ),
 ( #46164, #25694, #8846 ),
 ( #68634, #45812, #62994 ),
 ( #13773, #67234, #67955 ) ),
 .UNSPECIFIED., .F., .F., .F. ) 
 B_SPLINE_SURFACE_WITH_KNOTS ( ( 4, 2, 2, 2, 2, 2, 2, 2, 2, 4 ),
 ( 3, 3 ),
 ( 0.001620365016234695142, 0.002207270000664797102, 0.002500722492879848408, 0.002794174985094899279, 0.003087627477309950151, 0.003381079969525001457, 0.003527806215632527109, 0.003674532461740052328, 0.003821258707847577547, 0.003967984953955103200 ),
 ( 0.000000000000000000, 1.000000000000000000 ),
 .UNSPECIFIED. ) 
 GEOMETRIC_REPRESENTATION_ITEM ( )  RATIONAL_B_SPLINE_SURFACE ( (
 ( 1.000000000000000000, 0.7071067811865475727, 1.000000000000000000),
 ( 1.000000000000000000, 0.6778671762783700094, 1.000000000000000000),
 ( 1.000000000000000000, 0.6467717707951793349, 1.000000000000000000),
 ( 1.000000000000000000, 0.5961086003387628951, 1.000000000000000000),
 ( 1.000000000000000000, 0.5785481842580926237, 1.000000000000000000),
 ( 1.000000000000000000, 0.5417514570915383798, 1.000000000000000000),
 ( 1.000000000000000000, 0.5224568997730709707, 1.000000000000000000),
 ( 1.000000000000000000, 0.4825437615626911314, 1.000000000000000000),
 ( 1.000000000000000000, 0.4617081702731655191, 1.000000000000000000),
 ( 1.000000000000000000, 0.4191790061639760756, 1.000000000000000000),
 ( 1.000000000000000000, 0.3974966599962702629, 1.000000000000000000),
 ( 1.000000000000000000, 0.3653498311554840283, 1.000000000000000000),
 ( 1.000000000000000000, 0.3548631489840615716, 1.000000000000000000),
 ( 1.000000000000000000, 0.3350876751766880268, 1.000000000000000000),
 ( 1.000000000000000000, 0.3256829922529814181, 1.000000000000000000),
 ( 1.000000000000000000, 0.3094849113515590333, 1.000000000000000000),
 ( 1.000000000000000000, 0.3027429446061458695, 1.000000000000000000),
 ( 1.000000000000000000, 0.2932846354085155149, 1.000000000000000000),
 ( 1.000000000000000000, 0.2906862528187321160, 1.000000000000000000),
 ( 1.000000000000000000, 0.2907356542125049681, 1.000000000000000000) ) ) 
 REPRESENTATION_ITEM ( '' )  SURFACE ( )  );
#61580 = CARTESIAN_POINT ( 'NONE',  ( 9.827790563157511022E-16, 87.30187232391182306, -8.025000000000000355 ) ) ;
#61581 = ORIENTED_EDGE ( 'NONE', *, *, #42389, .T. ) ;
#61582 = DIRECTION ( 'NONE',  ( 0.000000000000000000, 0.000000000000000000, -1.000000000000000000 ) ) ;
#61583 = PRESENTATION_LAYER_ASSIGNMENT (  '', '', ( #20017 ) ) ;
#61585 =( LENGTH_UNIT ( ) NAMED_UNIT ( * ) SI_UNIT ( .MILLI., .METRE. ) );
#61584 = CARTESIAN_POINT ( 'NONE',  ( -53.30707362346617373, -10.01517768586948698, 6.132527647946031529E-16 ) ) ;
#61586 = PRESENTATION_LAYER_ASSIGNMENT (  '', '', ( #866 ) ) ;
#61587 = CARTESIAN_POINT ( 'NONE',  ( -3.094860106618434248, 143.7949999999999875, 9.525000000000000355 ) ) ;
#61588 = CARTESIAN_POINT ( 'NONE',  ( -111.2949999999999733, -2.607480562269069768, 8.024999999999991473 ) ) ;
#61589 = EDGE_CURVE ( 'NONE', #60674, #62454, #58036, .T. ) ;
#61590 = CARTESIAN_POINT ( 'NONE',  ( 48.75000000000000000, 22.24999999999998579, -4.000000000000000000 ) ) ;
#61591 = PRESENTATION_LAYER_ASSIGNMENT (  '', '', ( #5406 ) ) ;
#61592 = FILL_AREA_STYLE ('',( #44113 ) ) ;
#61593 = UNCERTAINTY_MEASURE_WITH_UNIT (LENGTH_MEASURE( 1.000000000000000082E-05 ), #26895, 'distance_accuracy_value', 'NONE');
#61594 = MECHANICAL_DESIGN_GEOMETRIC_PRESENTATION_REPRESENTATION (  '', ( #58257 ), #44796 ) ;
#61596 = CARTESIAN_POINT ( 'NONE',  ( -16.62603730713679795, 11.02523255763448873, 4.739503200942572825 ) ) ;
#61595 = CARTESIAN_POINT ( 'NONE',  ( -75.00000000000000000, 7.893193270153694208, -6.999999999999999112 ) ) ;
#61597 = CARTESIAN_POINT ( 'NONE',  ( -143.9929263765337737, 8.102448949553171076, -5.886773742842744461 ) ) ;
#61598 = CARTESIAN_POINT ( 'NONE',  ( -162.2949999999999875, -2.607480562269069768, 8.024999999999991473 ) ) ;
#61599 = CIRCLE ( 'NONE', #13306, 0.2500000000000002220 ) ;
#61600 = EDGE_CURVE ( 'NONE', #65395, #40140, #42570, .T. ) ;
#61601 =( NAMED_UNIT ( * ) PLANE_ANGLE_UNIT ( ) SI_UNIT ( $, .RADIAN. ) );
#61602 = PRESENTATION_STYLE_ASSIGNMENT (( #45148 ) ) ;
#61603 = EDGE_LOOP ( 'NONE', ( #4186, #54867, #38355, #55886 ) ) ;
#61604 = CARTESIAN_POINT ( 'NONE',  ( -20.71231517720798010, 114.9999999999999574, 10.50000000000000000 ) ) ;
#61605 = VERTEX_POINT ( 'NONE', #20377 ) ;
#61606 = EDGE_CURVE ( 'NONE', #20924, #23204, #37540, .T. ) ;
#61607 = UNCERTAINTY_MEASURE_WITH_UNIT (LENGTH_MEASURE( 1.000000000000000082E-05 ), #37077, 'distance_accuracy_value', 'NONE');
#61608 = ADVANCED_FACE ( 'NONE', ( #15819 ), #51709, .F. ) ;
#61609 = COLOUR_RGB ( '', 0.40784314, 0.44705882, 0.49803922) ;
#61610 = CARTESIAN_POINT ( 'NONE',  ( 30.99999999999998579, 0.000000000000000000, 72.00402776293822171 ) ) ;
#61611 = DIRECTION ( 'NONE',  ( 0.000000000000000000, 0.000000000000000000, -1.000000000000000000 ) ) ;
#61612 = LINE ( 'NONE', #56006, #46012 ) ;
#61613 = CARTESIAN_POINT ( 'NONE',  ( 0.000000000000000000, 152.9999999999999716, 0.000000000000000000 ) ) ;
#61614 = AXIS2_PLACEMENT_3D ( 'NONE', #31209, #66898, #8152 ) ;
#61615 = EDGE_CURVE ( 'NONE', #21177, #24543, #43160, .T. ) ;
#61616 = ORIENTED_EDGE ( 'NONE', *, *, #23282, .F. ) ;
#61617 = CARTESIAN_POINT ( 'NONE',  ( -158.6049999999999898, 6.826472737025113702, -4.959722759717902107 ) ) ;
#61618 = ORIENTED_EDGE ( 'NONE', *, *, #40603, .F. ) ;
#61619 = CARTESIAN_POINT ( 'NONE',  ( -44.99999999999998579, 119.9999999999999716, 9.500000000000000000 ) ) ;
#61620 = SURFACE_SIDE_STYLE ('',( #18734 ) ) ;
#61621 = VERTEX_POINT ( 'NONE', #14400 ) ;
#61622 =( GEOMETRIC_REPRESENTATION_CONTEXT ( 3 ) GLOBAL_UNCERTAINTY_ASSIGNED_CONTEXT ( ( #32194 ) ) GLOBAL_UNIT_ASSIGNED_CONTEXT ( ( #45735, #50977, #14368 ) ) REPRESENTATION_CONTEXT ( 'NONE', 'WORKASPACE' ) );
#61623 = AXIS2_PLACEMENT_3D ( 'NONE', #46116, #3832, #40484 ) ;
#61624 = SURFACE_SIDE_STYLE ('',( #40220 ) ) ;
#61625 = DIRECTION ( 'NONE',  ( 1.000000000000000000, 0.000000000000000000, 0.000000000000000000 ) ) ;
#61626 = CARTESIAN_POINT ( 'NONE',  ( 9.058813317711338797, 114.8449999999999847, -2.943386871421372675 ) ) ;
#61627 = STYLED_ITEM ( 'NONE', ( #23024 ), #4680 ) ;
#61628 = EDGE_LOOP ( 'NONE', ( #19161, #67733 ) ) ;
#61629 = CARTESIAN_POINT ( 'NONE',  ( 55.40000000000000568, 11.99999999999999822, -4.000000000000000000 ) ) ;
#61630 = DIRECTION ( 'NONE',  ( 0.000000000000000000, 0.000000000000000000, 1.000000000000000000 ) ) ;
#61631 = CARTESIAN_POINT ( 'NONE',  ( -72.95499999999999829, -7.632228543268599452, 2.479861379858951054 ) ) ;
#61632 = CARTESIAN_POINT ( 'NONE',  ( -13.75000000000000355, 28.24999999999998934, -3.750000000000000000 ) ) ;
#61633 = CARTESIAN_POINT ( 'NONE',  ( -10.01517768586949231, 141.3050000000000068, -6.132527647946036459E-16 ) ) ;
#61634 = UNCERTAINTY_MEASURE_WITH_UNIT (LENGTH_MEASURE( 1.000000000000000082E-05 ), #31344, 'distance_accuracy_value', 'NONE');
#61635 = PRESENTATION_STYLE_ASSIGNMENT (( #67287 ) ) ;
#61636 = VECTOR ( 'NONE', #42822, 1000.000000000000000 ) ;
#61637 = MECHANICAL_DESIGN_GEOMETRIC_PRESENTATION_REPRESENTATION (  '', ( #51515 ), #69537 ) ;
#61638 = EDGE_LOOP ( 'NONE', ( #14240, #49915, #54659, #47835 ) ) ;
#61639 = CARTESIAN_POINT ( 'NONE',  ( -52.34499999999997755, 7.632228543268599452, -2.479861379858951942 ) ) ;
#61640 = ORIENTED_EDGE ( 'NONE', *, *, #50690, .F. ) ;
#61641 = DIRECTION ( 'NONE',  ( 0.000000000000000000, 1.000000000000000000, 0.000000000000000000 ) ) ;
#61642 = STYLED_ITEM ( 'NONE', ( #24733 ), #19692 ) ;
#61643 = FILL_AREA_STYLE_COLOUR ( '', #44786 ) ;
#61644 = CYLINDRICAL_SURFACE ( 'NONE', #54369, 1.000000000000000000 ) ;
#61645 = LINE ( 'NONE', #34583, #7155 ) ;
#61646 = ORIENTED_EDGE ( 'NONE', *, *, #14449, .F. ) ;
#61647 = CARTESIAN_POINT ( 'NONE',  ( -56.54499999999998749, -7.632228543268600340, -2.479861379858950166 ) ) ;
#61648 = ORIENTED_EDGE ( 'NONE', *, *, #45557, .F. ) ;
#61649 = AXIS2_PLACEMENT_3D ( 'NONE', #26965, #21033, #10830 ) ;
#61650 = DIRECTION ( 'NONE',  ( 0.000000000000000000, 0.9396926207859082059, 0.3420201433256693790 ) ) ;
#61651 = CARTESIAN_POINT ( 'NONE',  ( -102.8049999999999784, -8.437984349512085203, 5.166775262442717831E-16 ) ) ;
#61652 = ORIENTED_EDGE ( 'NONE', *, *, #33297, .T. ) ;
#61653 = CARTESIAN_POINT ( 'NONE',  ( -2.607480562269020918, 118.2070736234661439, -8.025000000000037659 ) ) ;
#61654 = CARTESIAN_POINT ( 'NONE',  ( -142.1070736234661638, 8.102448949553171076, -5.886773742842744461 ) ) ;
#61655 = LINE ( 'NONE', #8583, #3569 ) ;
#61656 = CARTESIAN_POINT ( 'NONE',  ( 0.000000000000000000, 145.4449999999999932, -9.525000000000000355 ) ) ;
#61657 = CARTESIAN_POINT ( 'NONE',  ( -85.10707362346614957, 8.102448949553171076, -5.886773742842744461 ) ) ;
#61658 = COLOUR_RGB ( '', 0.66274510, 0.83137255, 0.94901961) ;
#61659 = CARTESIAN_POINT ( 'NONE',  ( -23.71231517720798010, 112.9999999999999858, 7.000000000000000000 ) ) ;
#61660 = CARTESIAN_POINT ( 'NONE',  ( -45.50000000000000000, 7.768687147774684831, -6.500000000000000000 ) ) ;
#61661 = DIRECTION ( 'NONE',  ( -0.000000000000000000, 1.000000000000000000, -0.000000000000000000 ) ) ;
#61662 = STYLED_ITEM ( 'NONE', ( #465 ), #42623 ) ;
#61663 = CARTESIAN_POINT ( 'NONE',  ( -118.7049999999999699, 2.607480562269073321, 8.024999999999991473 ) ) ;
#61664 = CARTESIAN_POINT ( 'NONE',  ( 23.67676504785522340, 24.55989583710076474, -27.19000000000005102 ) ) ;
#61665 = CARTESIAN_POINT ( 'NONE',  ( -8.102448949553181734, 109.8949999999999818, -5.886773742842749790 ) ) ;
#61666 = CARTESIAN_POINT ( 'NONE',  ( -133.3449999999999989, 7.632228543268599452, -2.479861379858951942 ) ) ;
#61667 = EDGE_CURVE ( 'NONE', #50347, #46312, #66703, .T. ) ;
#61668 = AXIS2_PLACEMENT_3D ( 'NONE', #29338, #28642, #19121 ) ;
#61669 = VECTOR ( 'NONE', #8994, 1000.000000000000000 ) ;
#61670 = CARTESIAN_POINT ( 'NONE',  ( -116.2449999999999903, -4.716976649647093289, -6.492361379858945902 ) ) ;
#61671 = CYLINDRICAL_SURFACE ( 'NONE', #9990, 0.2500000000000002220 ) ;
#61672 = CIRCLE ( 'NONE', #40375, 0.5000000000000004441 ) ;
#61673 = ORIENTED_EDGE ( 'NONE', *, *, #12206, .T. ) ;
#61674 = CIRCLE ( 'NONE', #46014, 6.999999999999997335 ) ;
#61675 = ADVANCED_FACE ( 'NONE', ( #9152 ), #30568, .T. ) ;
#61676 = CARTESIAN_POINT ( 'NONE',  ( -34.31243252642735087, -10.02680648607962510, -3.499999999999997335 ) ) ;
#61677 = COLOUR_RGB ( '', 0.31764706, 0.68627451, 0.89019608) ;
#61678 = ADVANCED_FACE ( 'NONE', ( #47161 ), #5559, .T. ) ;
#61679 = CARTESIAN_POINT ( 'NONE',  ( 22.99999999999995026, 0.000000000000000000, -32.00402776293824303 ) ) ;
#61680 = CARTESIAN_POINT ( 'NONE',  ( -169.3429263765337964, -9.058813317711329915, 2.943386871421371787 ) ) ;
#61681 = CARTESIAN_POINT ( 'NONE',  ( 29.00000000000000000, 35.42594141563417054, -80.00402776293826435 ) ) ;
#61682 = AXIS2_PLACEMENT_3D ( 'NONE', #10936, #64754, #59445 ) ;
#61683 = EDGE_CURVE ( 'NONE', #54714, #30521, #28459, .T. ) ;
#61684 = EDGE_CURVE ( 'NONE', #40912, #42981, #62212, .T. ) ;
#61685 =( NAMED_UNIT ( * ) PLANE_ANGLE_UNIT ( ) SI_UNIT ( $, .RADIAN. ) );
#61686 = DIRECTION ( 'NONE',  ( 0.000000000000000000, 0.000000000000000000, 1.000000000000000000 ) ) ;
#61687 = EDGE_CURVE ( 'NONE', #30380, #48589, #47637, .T. ) ;
#61688 = SURFACE_STYLE_FILL_AREA ( #19489 ) ;
#61689 = LINE ( 'NONE', #35343, #60839 ) ;
#61690 = ORIENTED_EDGE ( 'NONE', *, *, #62958, .T. ) ;
#61691 = CARTESIAN_POINT ( 'NONE',  ( -88.79292637653379927, -3.094860106618429807, 9.524999999999991473 ) ) ;
#61692 =( GEOMETRIC_REPRESENTATION_CONTEXT ( 3 ) GLOBAL_UNCERTAINTY_ASSIGNED_CONTEXT ( ( #15857 ) ) GLOBAL_UNIT_ASSIGNED_CONTEXT ( ( #2658, #34371, #35422 ) ) REPRESENTATION_CONTEXT ( 'NONE', 'WORKASPACE' ) );
#61693 = DIRECTION ( 'NONE',  ( 0.000000000000000000, 0.000000000000000000, 1.000000000000000000 ) ) ;
#61694 = EDGE_CURVE ( 'NONE', #61490, #59935, #37654, .T. ) ;
#61695 = SURFACE_STYLE_USAGE ( .BOTH. , #13885 ) ;
#61696 = FACE_OUTER_BOUND ( 'NONE', #64864, .T. ) ;
#61697 = CYLINDRICAL_SURFACE ( 'NONE', #41760, 1.000000000000000000 ) ;
#61698 = VERTEX_POINT ( 'NONE', #5915 ) ;
#61699 = FACE_OUTER_BOUND ( 'NONE', #8364, .T. ) ;
#61700 =( NAMED_UNIT ( * ) SI_UNIT ( $, .STERADIAN. ) SOLID_ANGLE_UNIT ( ) );
#61701 = CARTESIAN_POINT ( 'NONE',  ( -61.49999999999998579, 50.00000000000000000, 9.500000000000000000 ) ) ;
#61702 = ORIENTED_EDGE ( 'NONE', *, *, #62582, .F. ) ;
#61703 = CARTESIAN_POINT ( 'NONE',  ( -64.34292637653379643, -9.058813317711329915, 2.943386871421371787 ) ) ;
#61704 = AXIS2_PLACEMENT_3D ( 'NONE', #35388, #57163, #45277 ) ;
#61705 = CARTESIAN_POINT ( 'NONE',  ( -2.607480562269075097, 137.4070736234661183, 8.025000000000000355 ) ) ;
#61706 = CIRCLE ( 'NONE', #29174, 1.999999999999999112 ) ;
#61707 = PRESENTATION_STYLE_ASSIGNMENT (( #19861 ) ) ;
#61708 = CARTESIAN_POINT ( 'NONE',  ( -18.00000000000000711, 30.99999999999999289, 4.000000000000000000 ) ) ;
#61709 = DIRECTION ( 'NONE',  ( 0.000000000000000000, -0.000000000000000000, 1.000000000000000000 ) ) ;
#61711 = EDGE_LOOP ( 'NONE', ( #69627, #43681, #52418, #8336 ) ) ;
#61710 = MECHANICAL_DESIGN_GEOMETRIC_PRESENTATION_REPRESENTATION (  '', ( #48271 ), #57213 ) ;
#61712 = PRESENTATION_STYLE_ASSIGNMENT (( #62436 ) ) ;
#61713 = CARTESIAN_POINT ( 'NONE',  ( 3.249999999999998668, 36.74999999999999289, -3.750000000000000000 ) ) ;
#61714 = SURFACE_STYLE_USAGE ( .BOTH. , #40308 ) ;
#61715 = DIRECTION ( 'NONE',  ( -0.000000000000000000, 1.000000000000000000, -0.000000000000000000 ) ) ;
#61716 = AXIS2_PLACEMENT_3D ( 'NONE', #50653, #67882, #35162 ) ;
#61717 = AXIS2_PLACEMENT_3D ( 'NONE', #48626, #38423, #28478 ) ;
#61718 = CARTESIAN_POINT ( 'NONE',  ( -70.70707362346615810, -3.094860106618431139, -9.524999999999991473 ) ) ;
#61719 = CARTESIAN_POINT ( 'NONE',  ( -78.89499999999999602, 6.826472737025116366, 4.959722759717898555 ) ) ;
#61721 = VERTEX_POINT ( 'NONE', #59737 ) ;
#61720 = AXIS2_PLACEMENT_3D ( 'NONE', #26828, #59196, #37823 ) ;
#61722 = EDGE_CURVE ( 'NONE', #69443, #42429, #48287, .T. ) ;
#61723 = DIRECTION ( 'NONE',  ( -0.7071067811865543451, 8.659560562355015442E-17, 0.7071067811865408004 ) ) ;
#61724 = CARTESIAN_POINT ( 'NONE',  ( 28.00000000000000000, 5.569094604152798667, 2.026984667724099243 ) ) ;
#61725 = SURFACE_STYLE_FILL_AREA ( #14614 ) ;
#61726 = STYLED_ITEM ( 'NONE', ( #37438 ), #41858 ) ;
#61727 = EDGE_LOOP ( 'NONE', ( #22867, #15598, #20231, #16802 ) ) ;
#61728 = CARTESIAN_POINT ( 'NONE',  ( -48.00000000000000000, 13.41640786499872284, 7.000000000000000000 ) ) ;
#61729 = STYLED_ITEM ( 'NONE', ( #53746 ), #51534 ) ;
#61730 = CARTESIAN_POINT ( 'NONE',  ( -6.588738478070744975, 51.73049953470015083, -7.044582342571018785 ) ) ;
#61731 = ORIENTED_EDGE ( 'NONE', *, *, #54702, .T. ) ;
#61732 = FACE_OUTER_BOUND ( 'NONE', #4202, .T. ) ;
#61733 = EDGE_LOOP ( 'NONE', ( #50502, #47457, #34072, #17815 ) ) ;
#61734 = CARTESIAN_POINT ( 'NONE',  ( -4.500000000000002665, 22.24999999999998579, 3.750000000000000000 ) ) ;
#61735 = DIRECTION ( 'NONE',  ( 0.000000000000000000, -1.000000000000000000, 0.000000000000000000 ) ) ;
#61737 = CIRCLE ( 'NONE', #47211, 0.5000000000000004441 ) ;
#61736 = DIRECTION ( 'NONE',  ( 0.000000000000000000, -1.000000000000000000, 0.000000000000000000 ) ) ;
#61738 = CARTESIAN_POINT ( 'NONE',  ( -165.0570736234661524, 0.000000000000000000, 9.524999999999991473 ) ) ;
#61739 = DIRECTION ( 'NONE',  ( 1.000000000000000000, -0.000000000000000000, -1.300977106640434891E-16 ) ) ;
#61740 = MECHANICAL_DESIGN_GEOMETRIC_PRESENTATION_REPRESENTATION (  '', ( #42744 ), #66282 ) ;
#61741 = CARTESIAN_POINT ( 'NONE',  ( 5.598654528085805993, 111.2449999999999761, 7.705886871421374629 ) ) ;
#61742 = CARTESIAN_POINT ( 'NONE',  ( -116.3070736234661666, -10.01517768586948698, 6.132527647946031529E-16 ) ) ;
#61743 = CYLINDRICAL_SURFACE ( 'NONE', #68925, 0.5000000000000004441 ) ;
#61744 = CARTESIAN_POINT ( 'NONE',  ( -83.49999999999998579, -3.499999999999999556, 24.00000000000000000 ) ) ;
#61745 = ORIENTED_EDGE ( 'NONE', *, *, #2484, .F. ) ;
#61746 = AXIS2_PLACEMENT_3D ( 'NONE', #6325, #22520, #49259 ) ;
#61747 = DIRECTION ( 'NONE',  ( -1.000000000000000000, 0.000000000000000000, 0.000000000000000000 ) ) ;
#61748 = CARTESIAN_POINT ( 'NONE',  ( 22.25000000000000711, 34.24999999999999289, -4.000000000000000000 ) ) ;
#61749 = CARTESIAN_POINT ( 'NONE',  ( 19.00000000000000000, 8.000000000000000000, -3.500000000000017764 ) ) ;
#61750 = DIRECTION ( 'NONE',  ( -1.000000000000000000, 0.000000000000000000, 0.000000000000000000 ) ) ;
#61751 = CARTESIAN_POINT ( 'NONE',  ( -149.4550000000000125, 7.632228543268599452, -2.479861379858951942 ) ) ;
#61752 = EDGE_CURVE ( 'NONE', #67697, #26455, #10866, .T. ) ;
#61753 = CARTESIAN_POINT ( 'NONE',  ( -148.9429263765338192, 0.000000000000000000, 9.524999999999991473 ) ) ;
#61754 = CARTESIAN_POINT ( 'NONE',  ( -160.3449999999999989, 7.632228543268599452, -2.479861379858951942 ) ) ;
#61755 = CARTESIAN_POINT ( 'NONE',  ( -145.9449999999999932, -9.827790563157499189E-16, -8.024999999999991473 ) ) ;
#61756 = AXIS2_PLACEMENT_3D ( 'NONE', #6464, #43485, #8146 ) ;
#61757 = ORIENTED_EDGE ( 'NONE', *, *, #58769, .T. ) ;
#61758 = EDGE_CURVE ( 'NONE', #58318, #49290, #8265, .T. ) ;
#61759 =( LENGTH_UNIT ( ) NAMED_UNIT ( * ) SI_UNIT ( .MILLI., .METRE. ) );
#61760 = VECTOR ( 'NONE', #34886, 1000.000000000000000 ) ;
#61761 = CARTESIAN_POINT ( 'NONE',  ( -122.0929263765346064, 3.094860106631541985, 9.524999999990470201 ) ) ;
#61762 = CARTESIAN_POINT ( 'NONE',  ( -66.80499999999999261, -8.437984349512085203, 5.166775262442717831E-16 ) ) ;
#61763 =( LENGTH_UNIT ( ) NAMED_UNIT ( * ) SI_UNIT ( .MILLI., .METRE. ) );
#61764 = CARTESIAN_POINT ( 'NONE',  ( 13.50000000000000533, 30.99999999999999289, 3.750000000000000000 ) ) ;
#61765 = CARTESIAN_POINT ( 'NONE',  ( -69.74499999999999034, 4.716976649647094177, 6.492361379858945902 ) ) ;
#61766 = CARTESIAN_POINT ( 'NONE',  ( -8.102448949553181734, 150.0049999999999386, -5.886773742842749790 ) ) ;
#61767 = DIRECTION ( 'NONE',  ( 0.000000000000000000, 0.000000000000000000, -1.000000000000000000 ) ) ;
#61768 = CIRCLE ( 'NONE', #69677, 16.00000000000000711 ) ;
#61769 = EDGE_CURVE ( 'NONE', #52329, #23235, #20661, .T. ) ;
#61770 = AXIS2_PLACEMENT_3D ( 'NONE', #20430, #63341, #15196 ) ;
#61771 = DIRECTION ( 'NONE',  ( -1.000000000000000000, -0.000000000000000000, -0.000000000000000000 ) ) ;
#61772 = AXIS2_PLACEMENT_3D ( 'NONE', #9232, #30654, #36341 ) ;
#61773 = CARTESIAN_POINT ( 'NONE',  ( -74.99999999999998579, 50.00000000000000000, -12.00000000000000000 ) ) ;
#61774 = CARTESIAN_POINT ( 'NONE',  ( -20.71462257909523075, 114.5925267038606563, -10.00000000000000000 ) ) ;
#61776 = EDGE_CURVE ( 'NONE', #52976, #28531, #67096, .T. ) ;
#61775 = VECTOR ( 'NONE', #48876, 999.9999999999998863 ) ;
#61777 = CARTESIAN_POINT ( 'NONE',  ( -4.564701690882220220, 110.6597480665491133, 8.185492600733832447 ) ) ;
#61778 = LINE ( 'NONE', #2670, #58443 ) ;
#61779 = MECHANICAL_DESIGN_GEOMETRIC_PRESENTATION_REPRESENTATION (  '', ( #29202 ), #58448 ) ;
#61780 =( LENGTH_UNIT ( ) NAMED_UNIT ( * ) SI_UNIT ( .MILLI., .METRE. ) );
#61781 = FACE_OUTER_BOUND ( 'NONE', #9268, .T. ) ;
#61782 = EDGE_LOOP ( 'NONE', ( #26290, #51532, #17952, #28321 ) ) ;
#61783 = ORIENTED_EDGE ( 'NONE', *, *, #35355, .T. ) ;
#61784 = FILL_AREA_STYLE ('',( #34388 ) ) ;
#61785 = DIRECTION ( 'NONE',  ( 0.000000000000000000, 1.000000000000000000, -0.000000000000000000 ) ) ;
#61786 =( GEOMETRIC_REPRESENTATION_CONTEXT ( 3 ) GLOBAL_UNCERTAINTY_ASSIGNED_CONTEXT ( ( #45993 ) ) GLOBAL_UNIT_ASSIGNED_CONTEXT ( ( #66920, #25376, #13083 ) ) REPRESENTATION_CONTEXT ( 'NONE', 'WORKASPACE' ) );
#61787 = CARTESIAN_POINT ( 'NONE',  ( -45.00000000000000000, 9.708372675170618749, 6.000000000000000888 ) ) ;
#61788 = AXIS2_PLACEMENT_3D ( 'NONE', #42542, #47851, #21044 ) ;
#61789 =( NAMED_UNIT ( * ) SI_UNIT ( $, .STERADIAN. ) SOLID_ANGLE_UNIT ( ) );
#61790 = ORIENTED_EDGE ( 'NONE', *, *, #34328, .F. ) ;
#61791 = ORIENTED_EDGE ( 'NONE', *, *, #37221, .T. ) ;
#61792 = FILL_AREA_STYLE ('',( #40385 ) ) ;
#61793 = DIRECTION ( 'NONE',  ( 1.000000000000000000, 0.000000000000000000, -0.000000000000000000 ) ) ;
#61794 = ORIENTED_EDGE ( 'NONE', *, *, #52033, .T. ) ;
#61795 = CARTESIAN_POINT ( 'NONE',  ( -9.058813317711338797, 111.4549999999999841, 2.943386871421373563 ) ) ;
#61796 = CARTESIAN_POINT ( 'NONE',  ( -45.00000000000000000, -1.469576158976824302E-14, 4.000000000000000000 ) ) ;
#61797 = EDGE_LOOP ( 'NONE', ( #15095, #21679, #41618, #54343 ) ) ;
#61799 = CARTESIAN_POINT ( 'NONE',  ( -82.70707362346617231, -3.094860106618431139, -9.524999999999991473 ) ) ;
#61798 = CONICAL_SURFACE ( 'NONE', #41635, 7.000000000000000888, 0.7853981633974500554 ) ;
#61800 = CARTESIAN_POINT ( 'NONE',  ( 15.98999599679679839, 118.4999999999999716, -7.500000000000000000 ) ) ;
#61801 = CARTESIAN_POINT ( 'NONE',  ( -114.8949999999999818, 6.826472737025116366, 4.959722759717898555 ) ) ;
#61802 = VERTEX_POINT ( 'NONE', #66755 ) ;
#61803 = ADVANCED_FACE ( 'NONE', ( #61446 ), #8001, .T. ) ;
#61804 = CARTESIAN_POINT ( 'NONE',  ( 0.000000000000000000, 2.500000000000000000, 9.000000000000001776 ) ) ;
#61805 = CARTESIAN_POINT ( 'NONE',  ( -53.99292637653379501, 8.102448949553172852, -5.886773742842744461 ) ) ;
#61806 = CARTESIAN_POINT ( 'NONE',  ( -13.37774330277911794, -11.02468314135572491, -4.740767624907036293 ) ) ;
#61807 = AXIS2_PLACEMENT_3D ( 'NONE', #5029, #10997, #53899 ) ;
#61808 = DIRECTION ( 'NONE',  ( -0.000000000000000000, -0.000000000000000000, -1.000000000000000000 ) ) ;
#61809 = ORIENTED_EDGE ( 'NONE', *, *, #33620, .F. ) ;
#61810 = CARTESIAN_POINT ( 'NONE',  ( 6.826472737025119919, 142.8929263765338078, 4.959722759717908325 ) ) ;
#61811 = SURFACE_STYLE_FILL_AREA ( #29823 ) ;
#61812 = FILL_AREA_STYLE_COLOUR ( '', #22303 ) ;
#61813 = FILL_AREA_STYLE_COLOUR ( '', #22196 ) ;
#61814 = ORIENTED_EDGE ( 'NONE', *, *, #5055, .F. ) ;
#61815 = AXIS2_PLACEMENT_3D ( 'NONE', #24420, #31088, #13525 ) ;
#61816 = CARTESIAN_POINT ( 'NONE',  ( 57.00000000000000000, 16.00000000000000000, -60.00402776293825724 ) ) ;
#61817 = EDGE_LOOP ( 'NONE', ( #43806, #3555, #3954, #34313 ) ) ;
#61818 = DIRECTION ( 'NONE',  ( 0.000000000000000000, 0.000000000000000000, 1.000000000000000000 ) ) ;
#61819 = DIRECTION ( 'NONE',  ( 0.000000000000000000, 0.000000000000000000, 1.000000000000000000 ) ) ;
#61820 = CARTESIAN_POINT ( 'NONE',  ( 20.12916642283592950, 110.4999999999999858, 10.05319148936170137 ) ) ;
#61821 = DIRECTION ( 'NONE',  ( 0.000000000000000000, 0.000000000000000000, 1.000000000000000000 ) ) ;
#61822 = CARTESIAN_POINT ( 'NONE',  ( -132.2049999999999841, -2.607480562269071545, -8.024999999999991473 ) ) ;
#61823 = SPHERICAL_SURFACE ( 'NONE', #43245, 0.5000000000000000000 ) ;
#61824 = STYLED_ITEM ( 'NONE', ( #58353 ), #34550 ) ;
#61825 =( NAMED_UNIT ( * ) PLANE_ANGLE_UNIT ( ) SI_UNIT ( $, .RADIAN. ) );
#61826 = VERTEX_POINT ( 'NONE', #39017 ) ;
#61827 = DIRECTION ( 'NONE',  ( -0.000000000000000000, 1.000000000000000000, -0.000000000000000000 ) ) ;
#61828 = AXIS2_PLACEMENT_3D ( 'NONE', #56001, #34899, #67609 ) ;
#61829 = ADVANCED_FACE ( 'NONE', ( #46020, #23480 ), #13265, .F. ) ;
#61830 = DIRECTION ( 'NONE',  ( 1.000000000000000000, -0.000000000000000000, -0.000000000000000000 ) ) ;
#61831 = MECHANICAL_DESIGN_GEOMETRIC_PRESENTATION_REPRESENTATION (  '', ( #11286 ), #13538 ) ;
#61832 = DIRECTION ( 'NONE',  ( -0.000000000000000000, -0.000000000000000000, 1.000000000000000000 ) ) ;
#61833 = CARTESIAN_POINT ( 'NONE',  ( 24.00000000000000355, 36.75000000000000000, -3.000000000000000000 ) ) ;
#61834 = ORIENTED_EDGE ( 'NONE', *, *, #52862, .F. ) ;
#61835 = CIRCLE ( 'NONE', #43927, 5.000000000000000888 ) ;
#61836 = EDGE_LOOP ( 'NONE', ( #49338, #30934, #26198, #19608 ) ) ;
#61837 = FACE_OUTER_BOUND ( 'NONE', #2759, .T. ) ;
#61838 = CARTESIAN_POINT ( 'NONE',  ( -195.0000000000000000, 1.166476076187852838E-15, -9.524999999999991473 ) ) ;
#61839 = CARTESIAN_POINT ( 'NONE',  ( 27.00000000000001776, 15.00000000000000000, 35.50000000000000000 ) ) ;
#61840 = EDGE_CURVE ( 'NONE', #55377, #5413, #7151, .T. ) ;
#61841 = CARTESIAN_POINT ( 'NONE',  ( -48.65499999999997272, -7.632228543268600340, -2.479861379858950166 ) ) ;
#61842 = VERTEX_POINT ( 'NONE', #1643 ) ;
#61843 = CARTESIAN_POINT ( 'NONE',  ( -177.5049999999999670, -6.826472737025115478, -4.959722759717899443 ) ) ;
#61844 = ADVANCED_FACE ( 'NONE', ( #49899 ), #7325, .T. ) ;
#61845 = FILL_AREA_STYLE ('',( #66813 ) ) ;
#61846 = CARTESIAN_POINT ( 'NONE',  ( -37.50000000000000000, 58.31681314173471975, 6.349999999999996092 ) ) ;
#61847 = CARTESIAN_POINT ( 'NONE',  ( -57.65707362346616804, 9.058813317711329915, 2.943386871421369566 ) ) ;
#61848 = CARTESIAN_POINT ( 'NONE',  ( -175.7950000000000159, 2.607480562269069324, -8.024999999999993250 ) ) ;
#61849 = ADVANCED_FACE ( 'NONE', ( #39698 ), #42161, .T. ) ;
#61850 = DIRECTION ( 'NONE',  ( 0.000000000000000000, 0.000000000000000000, 1.000000000000000000 ) ) ;
#61851 =( GEOMETRIC_REPRESENTATION_CONTEXT ( 3 ) GLOBAL_UNCERTAINTY_ASSIGNED_CONTEXT ( ( #36246 ) ) GLOBAL_UNIT_ASSIGNED_CONTEXT ( ( #15037, #9400, #10772 ) ) REPRESENTATION_CONTEXT ( 'NONE', 'WORKASPACE' ) );
#61852 = ORIENTED_EDGE ( 'NONE', *, *, #31270, .F. ) ;
#61853 = AXIS2_PLACEMENT_3D ( 'NONE', #19917, #43178, #27255 ) ;
#61854 = CARTESIAN_POINT ( 'NONE',  ( -161.1570736234661751, -9.058813317711329915, -2.943386871421370898 ) ) ;
#61855 = EDGE_CURVE ( 'NONE', #64066, #8408, #66750, .T. ) ;
#61856 = PRESENTATION_STYLE_ASSIGNMENT (( #3070 ) ) ;
#61857 = CARTESIAN_POINT ( 'NONE',  ( 31.00000000000001421, 15.00000000000000000, 36.49999999999999289 ) ) ;
#61858 = CARTESIAN_POINT ( 'NONE',  ( -102.0549999999999926, -9.827790563157499189E-16, -8.024999999999991473 ) ) ;
#61859 = CARTESIAN_POINT ( 'NONE',  ( 0.000000000000000000, 154.5000000000000000, -9.524999999999998579 ) ) ;
#61861 =( NAMED_UNIT ( * ) PLANE_ANGLE_UNIT ( ) SI_UNIT ( $, .RADIAN. ) );
#61860 = AXIS2_PLACEMENT_3D ( 'NONE', #63862, #32535, #48090 ) ;
#61862 =( LENGTH_UNIT ( ) NAMED_UNIT ( * ) SI_UNIT ( .MILLI., .METRE. ) );
#61863 = EDGE_CURVE ( 'NONE', #29745, #12752, #19479, .T. ) ;
#61864 = CARTESIAN_POINT ( 'NONE',  ( -102.1449999999999818, -4.716976649647092401, 6.492361379858946790 ) ) ;
#61865 = CARTESIAN_POINT ( 'NONE',  ( 3.094860106618435136, 119.4049999999999727, -9.525000000000000355 ) ) ;
#61866 = CARTESIAN_POINT ( 'NONE',  ( -66.74499999999999034, 4.716976649647094177, 6.492361379858945902 ) ) ;
#61867 = CARTESIAN_POINT ( 'NONE',  ( -74.08452722063037754, 9.430195807687219656, -6.500000000000000000 ) ) ;
#61868 = EDGE_CURVE ( 'NONE', #67644, #26708, #19543, .T. ) ;
#61869 = DIRECTION ( 'NONE',  ( 0.000000000000000000, 0.000000000000000000, 1.000000000000000000 ) ) ;
#61870 = CIRCLE ( 'NONE', #4582, 0.5000000000000004441 ) ;
#61871 = CARTESIAN_POINT ( 'NONE',  ( -84.49999999999997158, 50.00000000000000000, 10.00000000000000000 ) ) ;
#61872 = LINE ( 'NONE', #13698, #15811 ) ;
#61874 = VERTEX_POINT ( 'NONE', #62502 ) ;
#61873 = AXIS2_PLACEMENT_3D ( 'NONE', #64068, #4983, #36707 ) ;
#61875 = CARTESIAN_POINT ( 'NONE',  ( -118.0429263765338135, -9.058813317711329915, -2.943386871421370898 ) ) ;
#61876 = CIRCLE ( 'NONE', #20303, 14.49999999999999822 ) ;
#61877 = ADVANCED_FACE ( 'NONE', ( #20286 ), #56891, .T. ) ;
#61878 =( BOUNDED_CURVE ( )  B_SPLINE_CURVE ( 2, ( #48821, #11821, #22042, #59658, #54381, #65291, #33293, #54718, #17139, #1207, #28319 ),
 .UNSPECIFIED., .F., .F. ) 
 B_SPLINE_CURVE_WITH_KNOTS ( ( 3, 2, 2, 2, 2, 3 ),
 ( 0.4411764705882353921, 0.4470588235294118973, 0.4529411764705883470, 0.4588235294117647967, 0.4647058823529413019, 0.4705882352941177516 ),
 .UNSPECIFIED. ) 
 CURVE ( )  GEOMETRIC_REPRESENTATION_ITEM ( )  RATIONAL_B_SPLINE_CURVE ( ( 0.9999999999999991118, 0.9510565162951544194, 1.000000000000000000, 0.9510565162951535312, 1.000000000000000000, 0.9510565162951535312, 1.000000000000000000, 0.9510565162951535312, 1.000000000000000000, 0.9510565162951526430, 1.000000000000000888 ) ) 
 REPRESENTATION_ITEM ( '' )  );
#61879 = CARTESIAN_POINT ( 'NONE',  ( -141.2949999999999875, -2.607480562269069768, 8.024999999999991473 ) ) ;
#61880 =( NAMED_UNIT ( * ) PLANE_ANGLE_UNIT ( ) SI_UNIT ( $, .RADIAN. ) );
#61881 = CIRCLE ( 'NONE', #31550, 0.5000000000000004441 ) ;
#61882 = DIRECTION ( 'NONE',  ( 1.000000000000000000, -0.000000000000000000, 0.000000000000000000 ) ) ;
#61883 = AXIS2_PLACEMENT_3D ( 'NONE', #4975, #47609, #47955 ) ;
#61885 = DIRECTION ( 'NONE',  ( -0.000000000000000000, 0.000000000000000000, -1.000000000000000000 ) ) ;
#61884 =( NAMED_UNIT ( * ) PLANE_ANGLE_UNIT ( ) SI_UNIT ( $, .RADIAN. ) );
#61886 = CARTESIAN_POINT ( 'NONE',  ( -174.2929263765339272, 3.094860106616311057, -9.525000000001533351 ) ) ;
#61887 = ORIENTED_EDGE ( 'NONE', *, *, #61385, .F. ) ;
#61888 = EDGE_LOOP ( 'NONE', ( #69256, #18768, #16612, #20649, #9522, #56445 ) ) ;
#61889 = DIRECTION ( 'NONE',  ( 0.000000000000000000, -0.000000000000000000, -1.000000000000000000 ) ) ;
#61890 = CONICAL_SURFACE ( 'NONE', #45079, 5.000000000000004441, 0.7853981633974587151 ) ;
#61891 = FACE_OUTER_BOUND ( 'NONE', #55443, .T. ) ;
#61892 = FILL_AREA_STYLE ('',( #40474 ) ) ;
#61893 = PRESENTATION_LAYER_ASSIGNMENT (  '', '', ( #46236 ) ) ;
#61894 = CARTESIAN_POINT ( 'NONE',  ( -74.99999999999998579, 50.00000000000000000, 10.00000000000000000 ) ) ;
#61895 = SURFACE_STYLE_FILL_AREA ( #18969 ) ;
#61896 = ORIENTED_EDGE ( 'NONE', *, *, #11825, .F. ) ;
#61897 = CARTESIAN_POINT ( 'NONE',  ( -127.7049999999999557, 2.607480562269072433, 8.024999999999991473 ) ) ;
#61898 = VERTEX_POINT ( 'NONE', #27625 ) ;
#61899 = DIRECTION ( 'NONE',  ( 0.000000000000000000, 0.000000000000000000, -1.000000000000000000 ) ) ;
#61900 = CARTESIAN_POINT ( 'NONE',  ( -122.3070736234661950, -10.01517768586948698, 6.132527647946031529E-16 ) ) ;
#61901 = VERTEX_POINT ( 'NONE', #21321 ) ;
#61902 = CARTESIAN_POINT ( 'NONE',  ( 4.041451884327379673, -7.000000000000002665, 7.500000000000000000 ) ) ;
#61903 = SURFACE_STYLE_USAGE ( .BOTH. , #62593 ) ;
#61904 = ORIENTED_EDGE ( 'NONE', *, *, #38417, .T. ) ;
#61905 = AXIS2_PLACEMENT_3D ( 'NONE', #40408, #61818, #50264 ) ;
#61906 = CARTESIAN_POINT ( 'NONE',  ( -102.1429263765337936, 5.598654528085800663, -7.705886871421367523 ) ) ;
#61907 = DIRECTION ( 'NONE',  ( -1.000000000000000000, -9.811390859391774840E-17, 0.000000000000000000 ) ) ;
#61908 = CARTESIAN_POINT ( 'NONE',  ( 5.598654528085805993, 144.2449999999999761, 7.705886871421374629 ) ) ;
#61909 =( NAMED_UNIT ( * ) SI_UNIT ( $, .STERADIAN. ) SOLID_ANGLE_UNIT ( ) );
#61910 = CIRCLE ( 'NONE', #49586, 0.2500000000000002220 ) ;
#61911 = ORIENTED_EDGE ( 'NONE', *, *, #15685, .F. ) ;
#61912 = CARTESIAN_POINT ( 'NONE',  ( 25.75000000000001066, 21.74999999999998224, 3.750000000000000000 ) ) ;
#61913 = CARTESIAN_POINT ( 'NONE',  ( -8.102448949553179958, 138.0049999999999670, -5.886773742842749790 ) ) ;
#61914 = DIRECTION ( 'NONE',  ( 1.000000000000000000, 0.000000000000000000, -0.000000000000000000 ) ) ;
#61915 = ORIENTED_EDGE ( 'NONE', *, *, #34625, .F. ) ;
#61916 = CARTESIAN_POINT ( 'NONE',  ( 4.716976649647096842, 115.7429263765338163, 6.492361379858953896 ) ) ;
#61917 = PRESENTATION_STYLE_ASSIGNMENT (( #13737 ) ) ;
#61918 = CIRCLE ( 'NONE', #29366, 0.5000000000000004441 ) ;
#61919 = CARTESIAN_POINT ( 'NONE',  ( 22.75000000000000711, 0.000000000000000000, 4.000000000000000000 ) ) ;
#61920 = ORIENTED_EDGE ( 'NONE', *, *, #18466, .F. ) ;
#61921 = ORIENTED_EDGE ( 'NONE', *, *, #4998, .F. ) ;
#61922 = FACE_OUTER_BOUND ( 'NONE', #53378, .T. ) ;
#61923 = LINE ( 'NONE', #13749, #68900 ) ;
#61925 = CARTESIAN_POINT ( 'NONE',  ( -162.3549999999999898, -4.716976649647093289, -6.492361379858945902 ) ) ;
#61924 = CONICAL_SURFACE ( 'NONE', #59657, 7.500000000000000000, 0.7853981633974518317 ) ;
#61926 = EDGE_LOOP ( 'NONE', ( #10548, #15820, #33157, #696 ) ) ;
#61927 = ADVANCED_FACE ( 'NONE', ( #26918 ), #15122, .F. ) ;
#61928 =( GEOMETRIC_REPRESENTATION_CONTEXT ( 3 ) GLOBAL_UNCERTAINTY_ASSIGNED_CONTEXT ( ( #8823 ) ) GLOBAL_UNIT_ASSIGNED_CONTEXT ( ( #25529, #36834, #36121 ) ) REPRESENTATION_CONTEXT ( 'NONE', 'WORKASPACE' ) );
#61929 = CARTESIAN_POINT ( 'NONE',  ( -53.60138881051016568, -9.947368421052630083, 2.722470280083837402 ) ) ;
#61930 = SURFACE_STYLE_USAGE ( .BOTH. , #55635 ) ;
#61931 = ORIENTED_EDGE ( 'NONE', *, *, #2755, .T. ) ;
#61932 = EDGE_CURVE ( 'NONE', #55787, #32128, #54380, .T. ) ;
#61933 = ORIENTED_EDGE ( 'NONE', *, *, #41103, .F. ) ;
#61934 = SURFACE_SIDE_STYLE ('',( #67225 ) ) ;
#61935 = CIRCLE ( 'NONE', #31605, 5.499999999999985789 ) ;
#61936 = DIRECTION ( 'NONE',  ( -1.000000000000000000, 0.000000000000000000, 0.000000000000000000 ) ) ;
#61937 = EDGE_CURVE ( 'NONE', #17044, #9702, #33072, .T. ) ;
#61938 = CARTESIAN_POINT ( 'NONE',  ( -73.25499999999998124, -4.716976649647092401, 6.492361379858946790 ) ) ;
#61939 = ORIENTED_EDGE ( 'NONE', *, *, #23515, .T. ) ;
#61940 =( LENGTH_UNIT ( ) NAMED_UNIT ( * ) SI_UNIT ( .MILLI., .METRE. ) );
#61941 = EDGE_CURVE ( 'NONE', #22202, #32736, #2678, .T. ) ;
#61942 = VECTOR ( 'NONE', #51269, 1000.000000000000000 ) ;
#61943 = STYLED_ITEM ( 'NONE', ( #65549 ), #35265 ) ;
#61944 = CARTESIAN_POINT ( 'NONE',  ( 15.48999599679679662, 117.9999999999999716, 7.000000000000000000 ) ) ;
#61945 = CARTESIAN_POINT ( 'NONE',  ( -67.49999999999998579, -1.929132118054077781E-14, -12.00000000000000000 ) ) ;
#61946 = CARTESIAN_POINT ( 'NONE',  ( -74.13336567797000498, 9.244254510420731208, -6.241797924670647646 ) ) ;
#61947 = EDGE_LOOP ( 'NONE', ( #51638, #38709, #20082, #12167 ) ) ;
#61948 = CARTESIAN_POINT ( 'NONE',  ( 22.29422224269975672, 26.00000000000000355, -27.50000000000000711 ) ) ;
#61949 = AXIS2_PLACEMENT_3D ( 'NONE', #24753, #62739, #19841 ) ;
#61951 = CARTESIAN_POINT ( 'NONE',  ( -71.62068965517238439, 63.58603185604027885, -9.500000000000000000 ) ) ;
#61950 = CARTESIAN_POINT ( 'NONE',  ( 31.00000000000000355, 43.00000000000000000, -36.50000000000000000 ) ) ;
#61952 = ADVANCED_FACE ( 'NONE', ( #69190 ), #37575, .T. ) ;
#61953 = CARTESIAN_POINT ( 'NONE',  ( -8.102448949553181734, 134.4949999999999477, 5.886773742842747126 ) ) ;
#61954 = CARTESIAN_POINT ( 'NONE',  ( -99.59499999999999886, 2.607480562269073321, 8.024999999999991473 ) ) ;
#61955 = AXIS2_PLACEMENT_3D ( 'NONE', #66897, #28876, #61573 ) ;
#61956 = CARTESIAN_POINT ( 'NONE',  ( -7.000000000000000888, 0.000000000000000000, 0.000000000000000000 ) ) ;
#61957 = DIRECTION ( 'NONE',  ( 1.734723475976805517E-15, 0.000000000000000000, -1.000000000000000000 ) ) ;
#61959 = DIRECTION ( 'NONE',  ( 0.000000000000000000, 0.000000000000000000, 1.000000000000000000 ) ) ;
#61958 = SURFACE_STYLE_FILL_AREA ( #40546 ) ;
#61960 = CARTESIAN_POINT ( 'NONE',  ( -143.3929263765338078, 8.102448949553176405, 5.886773742842740909 ) ) ;
#61961 = FILL_AREA_STYLE_COLOUR ( '', #52354 ) ;
#61962 = CARTESIAN_POINT ( 'NONE',  ( -163.6449999999999818, 4.716976649647091513, -6.492361379858946790 ) ) ;
#61963 = CIRCLE ( 'NONE', #33893, 0.2500000000000002220 ) ;
#61964 = EDGE_CURVE ( 'NONE', #68501, #17294, #4943, .T. ) ;
#61965 = FACE_OUTER_BOUND ( 'NONE', #18644, .T. ) ;
#61966 = FILL_AREA_STYLE_COLOUR ( '', #14806 ) ;
#61967 = ORIENTED_EDGE ( 'NONE', *, *, #4612, .F. ) ;
#61968 = CARTESIAN_POINT ( 'NONE',  ( -7.632228543268608334, 127.9570736234661439, 2.479861379858952830 ) ) ;
#61969 = ORIENTED_EDGE ( 'NONE', *, *, #24969, .T. ) ;
#61970 = STYLED_ITEM ( 'NONE', ( #21490 ), #60351 ) ;
#61971 = ADVANCED_FACE ( 'NONE', ( #32230 ), #53681, .F. ) ;
#61972 = DIRECTION ( 'NONE',  ( 0.000000000000000000, 1.000000000000000000, 0.000000000000000000 ) ) ;
#61973 = COLOUR_RGB ( '', 0.66274510, 0.83137255, 0.94901961) ;
#61974 = AXIS2_PLACEMENT_3D ( 'NONE', #43167, #17777, #17100 ) ;
#61975 = DIRECTION ( 'NONE',  ( -1.000000000000000000, 0.000000000000000000, 0.000000000000000000 ) ) ;
#61976 = CARTESIAN_POINT ( 'NONE',  ( 4.716976649647096842, 118.7429263765338163, 6.492361379858953896 ) ) ;
#61977 = CARTESIAN_POINT ( 'NONE',  ( -173.7570736234661695, -5.598654528085801552, 7.705886871421367523 ) ) ;
#61978 = VECTOR ( 'NONE', #67445, 1000.000000000000000 ) ;
#61980 = AXIS2_PLACEMENT_3D ( 'NONE', #64813, #21194, #26130 ) ;
#61979 = FACE_OUTER_BOUND ( 'NONE', #34358, .T. ) ;
#61981 = ORIENTED_EDGE ( 'NONE', *, *, #29852, .F. ) ;
#61982 = CARTESIAN_POINT ( 'NONE',  ( -162.5049999999999670, -6.826472737025113702, -4.959722759717900331 ) ) ;
#61983 = VERTEX_POINT ( 'NONE', #65631 ) ;
#61984 = VECTOR ( 'NONE', #7577, 1000.000000000000000 ) ;
#61985 = ORIENTED_EDGE ( 'NONE', *, *, #25548, .T. ) ;
#61986 = AXIS2_PLACEMENT_3D ( 'NONE', #28054, #5240, #26683 ) ;
#61987 =( NAMED_UNIT ( * ) SI_UNIT ( $, .STERADIAN. ) SOLID_ANGLE_UNIT ( ) );
#61988 = CARTESIAN_POINT ( 'NONE',  ( -9.058813317711338797, 113.3449999999999847, 2.943386871421373563 ) ) ;
#61989 = ORIENTED_EDGE ( 'NONE', *, *, #65044, .F. ) ;
#61990 = CARTESIAN_POINT ( 'NONE',  ( 9.058813317711338797, 115.9549999999999841, -2.943386871421372675 ) ) ;
#61991 = CARTESIAN_POINT ( 'NONE',  ( -73.85499999999998977, 4.716976649647094177, 6.492361379858945902 ) ) ;
#61992 = CARTESIAN_POINT ( 'NONE',  ( -9.000000000000003553, 27.74999999999998934, -3.750000000000000000 ) ) ;
#61993 = EDGE_LOOP ( 'NONE', ( #37124, #17084, #26479, #17230 ) ) ;
#61994 = CARTESIAN_POINT ( 'NONE',  ( 3.094860106618431583, 136.2049999999999557, 9.525000000000000355 ) ) ;
#61995 = AXIS2_PLACEMENT_3D ( 'NONE', #21937, #27169, #44473 ) ;
#61996 = SURFACE_STYLE_USAGE ( .BOTH. , #56748 ) ;
#61997 = AXIS2_PLACEMENT_3D ( 'NONE', #24900, #46413, #35819 ) ;
#61998 = CARTESIAN_POINT ( 'NONE',  ( 20.55683252178218723, 114.6388620567782084, 10.28289609742943078 ) ) ;
#61999 = CARTESIAN_POINT ( 'NONE',  ( -114.2929263765346803, 3.094860106603773531, -9.525000000010640733 ) ) ;
#62000 = COLOUR_RGB ( '', 0.40784314, 0.44705882, 0.49803922) ;
#62001 = EDGE_CURVE ( 'NONE', #20924, #46101, #60341, .T. ) ;
#62002 = ORIENTED_EDGE ( 'NONE', *, *, #48963, .T. ) ;
#62003 = CARTESIAN_POINT ( 'NONE',  ( 0.000000000000000000, 87.30187232391182306, 0.000000000000000000 ) ) ;
#62004 = CARTESIAN_POINT ( 'NONE',  ( -48.74499999999998323, 4.716976649647094177, 6.492361379858945902 ) ) ;
#62005 = ORIENTED_EDGE ( 'NONE', *, *, #5529, .F. ) ;
#62006 =( BOUNDED_CURVE ( )  B_SPLINE_CURVE ( 2, ( #45077, #2771, #13710, #18966, #40135, #57312, #56971, #13018, #56266, #8093, #14393 ),
 .UNSPECIFIED., .F., .F. ) 
 B_SPLINE_CURVE_WITH_KNOTS ( ( 3, 2, 2, 2, 2, 3 ),
 ( 0.8804347826086956763, 0.8826086956521739246, 0.8847826086956521729, 0.8869565217391304213, 0.8891304347826086696, 0.8913043478260869179 ),
 .UNSPECIFIED. ) 
 CURVE ( )  GEOMETRIC_REPRESENTATION_ITEM ( )  RATIONAL_B_SPLINE_CURVE ( ( 1.000000000000000000, 0.9510565162951535312, 1.000000000000000000, 0.9510565162951535312, 1.000000000000000000, 0.9510565162951535312, 1.000000000000000000, 0.9510565162951535312, 1.000000000000000000, 0.9510565162951535312, 1.000000000000000000 ) ) 
 REPRESENTATION_ITEM ( '' )  );
#62007 = COLOUR_RGB ( '', 0.09019608, 0.27058824, 0.51372549) ;
#62008 = DIRECTION ( 'NONE',  ( -0.000000000000000000, -1.000000000000000000, -0.000000000000000000 ) ) ;
#62009 = ORIENTED_EDGE ( 'NONE', *, *, #33077, .T. ) ;
#62010 = CARTESIAN_POINT ( 'NONE',  ( -53.39499999999998892, -6.826472737025113702, -4.959722759717900331 ) ) ;
#62011 = SURFACE_STYLE_FILL_AREA ( #7855 ) ;
#62012 = ORIENTED_EDGE ( 'NONE', *, *, #3460, .T. ) ;
#62014 = EDGE_CURVE ( 'NONE', #41120, #24031, #60680, .T. ) ;
#62013 = DIRECTION ( 'NONE',  ( -1.000000000000000000, 0.000000000000000000, 0.000000000000000000 ) ) ;
#62015 = CARTESIAN_POINT ( 'NONE',  ( -101.1550000000000011, 7.632228543268600340, 2.479861379858949277 ) ) ;
#62016 = ORIENTED_EDGE ( 'NONE', *, *, #15043, .F. ) ;
#62017 = CARTESIAN_POINT ( 'NONE',  ( -4.750000000000002665, 24.99999999999998579, 4.000000000000000000 ) ) ;
#62018 = CARTESIAN_POINT ( 'NONE',  ( 8.000000000000030198, 0.000000000000000000, -29.00402776293826079 ) ) ;
#62019 = CARTESIAN_POINT ( 'NONE',  ( -136.7070736234661297, -3.094860106618431139, -9.524999999999991473 ) ) ;
#62020 = AXIS2_PLACEMENT_3D ( 'NONE', #59727, #42560, #63962 ) ;
#62021 = CARTESIAN_POINT ( 'NONE',  ( -59.15707362346617515, -9.058813317711329915, -2.943386871421370898 ) ) ;
#62022 = CARTESIAN_POINT ( 'NONE',  ( -9.058813317711337021, 140.0449999999999875, -2.943386871421374895 ) ) ;
#62023 = CARTESIAN_POINT ( 'NONE',  ( -73.10707362346614957, 8.102448949553171076, -5.886773742842744461 ) ) ;
#62024 = PRESENTATION_LAYER_ASSIGNMENT (  '', '', ( #22724 ) ) ;
#62025 = DIRECTION ( 'NONE',  ( 0.7071067811865426878, 8.659560562354994488E-17, 0.7071067811865524577 ) ) ;
#62026 = FILL_AREA_STYLE ('',( #45887 ) ) ;
#62027 =( GEOMETRIC_REPRESENTATION_CONTEXT ( 3 ) GLOBAL_UNCERTAINTY_ASSIGNED_CONTEXT ( ( #65197 ) ) GLOBAL_UNIT_ASSIGNED_CONTEXT ( ( #40667, #1897, #45266 ) ) REPRESENTATION_CONTEXT ( 'NONE', 'WORKASPACE' ) );
#62029 = CARTESIAN_POINT ( 'NONE',  ( -99.59292637653487645, -3.094860106636313279, -9.524999999987000976 ) ) ;
#62028 = CARTESIAN_POINT ( 'NONE',  ( -9.827790563157511022E-16, 119.5570736234661524, 8.025000000000000355 ) ) ;
#62030 = ADVANCED_FACE ( 'NONE', ( #50167 ), #50500, .F. ) ;
#62031 = CARTESIAN_POINT ( 'NONE',  ( -121.8549999999999898, 4.716976649647094177, 6.492361379858945902 ) ) ;
#62032 = SURFACE_SIDE_STYLE ('',( #30029 ) ) ;
#62033 = VECTOR ( 'NONE', #17973, 1000.000000000000000 ) ;
#62034 = CARTESIAN_POINT ( 'NONE',  ( -138.8949999999999534, 6.826472737025116366, 4.959722759717898555 ) ) ;
#62035 = CARTESIAN_POINT ( 'NONE',  ( -121.0449999999999875, 7.632228543268600340, 2.479861379858949277 ) ) ;
#62036 = CIRCLE ( 'NONE', #55265, 5.500000000000005329 ) ;
#62037 = CARTESIAN_POINT ( 'NONE',  ( -23.71231517720798010, 117.4999999999999716, -7.000000000000000000 ) ) ;
#62038 = ORIENTED_EDGE ( 'NONE', *, *, #48431, .T. ) ;
#62039 = AXIS2_PLACEMENT_3D ( 'NONE', #48049, #53617, #37844 ) ;
#62040 = CARTESIAN_POINT ( 'NONE',  ( 48.25000000000000000, 21.99999999999998579, -3.750000000000000000 ) ) ;
#62041 = CARTESIAN_POINT ( 'NONE',  ( -174.8929263765337794, -8.102448949553172852, -5.886773742842741797 ) ) ;
#62042 = CARTESIAN_POINT ( 'NONE',  ( -53.09499999999997755, -2.607480562269071545, -8.024999999999991473 ) ) ;
#62043 = LINE ( 'NONE', #31078, #25294 ) ;
#62044 = STYLED_ITEM ( 'NONE', ( #36898 ), #19005 ) ;
#62045 = CARTESIAN_POINT ( 'NONE',  ( -74.99999999999998579, 64.49137674618943095, 6.500000000000000000 ) ) ;
#62046 = ORIENTED_EDGE ( 'NONE', *, *, #63772, .F. ) ;
#62047 = PRODUCT_DEFINITION_CONTEXT ( 'detailed design', #45596, 'design' ) ;
#62048 = CARTESIAN_POINT ( 'NONE',  ( -88.34292637653381064, -9.058813317711329915, 2.943386871421371787 ) ) ;
#62049 = PRODUCT_CONTEXT ( 'NONE', #38410, 'mechanical' ) ;
#62050 = DIRECTION ( 'NONE',  ( 0.000000000000000000, 0.000000000000000000, -1.000000000000000000 ) ) ;
#62051 = CARTESIAN_POINT ( 'NONE',  ( 3.749999999999999556, 33.74999999999998579, -3.750000000000000000 ) ) ;
#62052 = AXIS2_PLACEMENT_3D ( 'NONE', #30618, #57727, #52122 ) ;
#62053 = CARTESIAN_POINT ( 'NONE',  ( -180.4429263765338192, -1.166476076187852838E-15, -9.524999999999991473 ) ) ;
#62054 = CARTESIAN_POINT ( 'NONE',  ( 0.000000000000000000, 124.0570736234661524, -8.025000000000000355 ) ) ;
#62055 = STYLED_ITEM ( 'NONE', ( #20412 ), #24919 ) ;
#62056 = B_SPLINE_CURVE_WITH_KNOTS ( 'NONE', 3,
 ( #50555, #23451, #19204, #44958, #67074, #66364, #61091, #61420 ),
 .UNSPECIFIED., .F., .F.,
 ( 4, 2, 2, 4 ),
 ( 2.544313220892526165E-07, 0.002693395767724534023, 0.004039966435925755432, 0.005386537104126977275 ),
 .UNSPECIFIED. ) ;
#62057 = CARTESIAN_POINT ( 'NONE',  ( -157.4070736234665446, 3.094860106613151807, -9.525000000003830181 ) ) ;
#62058 = EDGE_LOOP ( 'NONE', ( #51413, #14739, #49737, #67309, #51308, #16184, #33062 ) ) ;
#62059 = CARTESIAN_POINT ( 'NONE',  ( -136.0429263765338135, -9.058813317711329915, -2.943386871421370898 ) ) ;
#62060 = PRESENTATION_STYLE_ASSIGNMENT (( #14956 ) ) ;
#62061 = DIRECTION ( 'NONE',  ( -0.000000000000000000, -0.000000000000000000, -1.000000000000000000 ) ) ;
#62062 = ORIENTED_EDGE ( 'NONE', *, *, #46446, .F. ) ;
#62063 = CYLINDRICAL_SURFACE ( 'NONE', #51046, 9.524999999999991473 ) ;
#62064 = VECTOR ( 'NONE', #64270, 1000.000000000000000 ) ;
#62065 = AXIS2_PLACEMENT_3D ( 'NONE', #48449, #15723, #21669 ) ;
#62066 = LINE ( 'NONE', #58194, #46640 ) ;
#62067 = CARTESIAN_POINT ( 'NONE',  ( -2.607480562269075097, 131.4070736234661467, 8.025000000000000355 ) ) ;
#62068 =( GEOMETRIC_REPRESENTATION_CONTEXT ( 3 ) GLOBAL_UNCERTAINTY_ASSIGNED_CONTEXT ( ( #14296 ) ) GLOBAL_UNIT_ASSIGNED_CONTEXT ( ( #11571, #27723, #23856 ) ) REPRESENTATION_CONTEXT ( 'NONE', 'WORKASPACE' ) );
#62069 = ORIENTED_EDGE ( 'NONE', *, *, #29859, .T. ) ;
#62070 = CARTESIAN_POINT ( 'NONE',  ( -98.15499999999998693, 7.632228543268600340, 2.479861379858949277 ) ) ;
#62071 = VECTOR ( 'NONE', #3948, 1000.000000000000000 ) ;
#62072 = ORIENTED_EDGE ( 'NONE', *, *, #11446, .F. ) ;
#62073 = FACE_OUTER_BOUND ( 'NONE', #35705, .T. ) ;
#62074 = CARTESIAN_POINT ( 'NONE',  ( 34.99999999999992895, 112.4999999999999858, -10.00000000000000000 ) ) ;
#62075 = DIRECTION ( 'NONE',  ( -0.000000000000000000, 1.000000000000000000, -0.000000000000000000 ) ) ;
#62076 = MECHANICAL_DESIGN_GEOMETRIC_PRESENTATION_REPRESENTATION (  '', ( #48688 ), #13793 ) ;
#62077 = EDGE_CURVE ( 'NONE', #20746, #5753, #2228, .T. ) ;
#62078 = DIRECTION ( 'NONE',  ( 8.659560562354932858E-17, -0.7071067811865474617, 0.7071067811865474617 ) ) ;
#62079 = CARTESIAN_POINT ( 'NONE',  ( -85.94499999999999318, -9.827790563157499189E-16, -8.024999999999991473 ) ) ;
#62080 = ORIENTED_EDGE ( 'NONE', *, *, #63133, .T. ) ;
#62081 = EDGE_CURVE ( 'NONE', #20853, #3957, #21873, .T. ) ;
#62082 = MECHANICAL_DESIGN_GEOMETRIC_PRESENTATION_REPRESENTATION (  '', ( #51972 ), #13798 ) ;
#62083 =( NAMED_UNIT ( * ) PLANE_ANGLE_UNIT ( ) SI_UNIT ( $, .RADIAN. ) );
#62084 =( NAMED_UNIT ( * ) SI_UNIT ( $, .STERADIAN. ) SOLID_ANGLE_UNIT ( ) );
#62085 = UNCERTAINTY_MEASURE_WITH_UNIT (LENGTH_MEASURE( 1.000000000000000082E-05 ), #52179, 'distance_accuracy_value', 'NONE');
#62086 = ORIENTED_EDGE ( 'NONE', *, *, #49184, .T. ) ;
#62087 =( NAMED_UNIT ( * ) SI_UNIT ( $, .STERADIAN. ) SOLID_ANGLE_UNIT ( ) );
#62088 = SURFACE_SIDE_STYLE ('',( #25164 ) ) ;
#62089 = EDGE_CURVE ( 'NONE', #24627, #53864, #66679, .T. ) ;
#62090 = COLOUR_RGB ( '', 0.40784314, 0.44705882, 0.49803922) ;
#62091 = ADVANCED_FACE ( 'NONE', ( #23758 ), #23079, .T. ) ;
#62092 = ORIENTED_EDGE ( 'NONE', *, *, #50584, .T. ) ;
#62093 = AXIS2_PLACEMENT_3D ( 'NONE', #59605, #22682, #33238 ) ;
#62094 = CYLINDRICAL_SURFACE ( 'NONE', #26241, 1.000000000000000888 ) ;
#62095 = EDGE_CURVE ( 'NONE', #17887, #40202, #57828, .T. ) ;
#62096 = ORIENTED_EDGE ( 'NONE', *, *, #9517, .F. ) ;
#62097 = PLANE ( 'NONE',  #38104 ) ;
#62098 =( LENGTH_UNIT ( ) NAMED_UNIT ( * ) SI_UNIT ( .MILLI., .METRE. ) );
#62099 = CARTESIAN_POINT ( 'NONE',  ( 19.00000000000000000, 8.000000000000000000, 3.500000000000003997 ) ) ;
#62100 = CARTESIAN_POINT ( 'NONE',  ( -168.8070736234661808, 10.01517768586948698, -1.839758294383808571E-15 ) ) ;
#62101 = EDGE_CURVE ( 'NONE', #59375, #25904, #460, .T. ) ;
#62102 = CARTESIAN_POINT ( 'NONE',  ( 51.49999999999998579, 2.837994680254535968E-15, -9.999999999999998224 ) ) ;
#62103 = CARTESIAN_POINT ( 'NONE',  ( 0.000000000000000000, 115.4449999999999932, -9.525000000000000355 ) ) ;
#62104 = CARTESIAN_POINT ( 'NONE',  ( -112.2570736234661837, 5.598654528085800663, -7.705886871421367523 ) ) ;
#62105 = COLOUR_RGB ( '', 0.31764706, 0.68627451, 0.89019608) ;
#62106 = CARTESIAN_POINT ( 'NONE',  ( -24.00000000000000000, 1.000000000000000000, -3.000000000000000000 ) ) ;
#62107 = ADVANCED_FACE ( 'NONE', ( #29367 ), #2602, .T. ) ;
#62108 = CARTESIAN_POINT ( 'NONE',  ( -75.00000000000000000, -2.215169945516535778E-14, 6.500000000000000000 ) ) ;
#62109 = ORIENTED_EDGE ( 'NONE', *, *, #57493, .F. ) ;
#62110 = LINE ( 'NONE', #18170, #44139 ) ;
#62111 = CARTESIAN_POINT ( 'NONE',  ( -81.89292637653380780, -8.102448949553174629, -5.886773742842741797 ) ) ;
#62113 = PRESENTATION_STYLE_ASSIGNMENT (( #4390 ) ) ;
#62112 = DIRECTION ( 'NONE',  ( 0.000000000000000000, 0.000000000000000000, 1.000000000000000000 ) ) ;
#62114 = SURFACE_STYLE_FILL_AREA ( #14284 ) ;
#62115 = CARTESIAN_POINT ( 'NONE',  ( -150.0550000000000068, -9.827790563157499189E-16, -8.024999999999991473 ) ) ;
#62116 = FACE_OUTER_BOUND ( 'NONE', #40867, .T. ) ;
#62117 = CARTESIAN_POINT ( 'NONE',  ( -162.8949999999999534, 6.826472737025116366, 4.959722759717898555 ) ) ;
#62118 = AXIS2_PLACEMENT_3D ( 'NONE', #26663, #30920, #41872 ) ;
#62119 = CIRCLE ( 'NONE', #36374, 0.2500000000000002220 ) ;
#62120 = CARTESIAN_POINT ( 'NONE',  ( -149.5449999999999875, -7.632228543268600340, -2.479861379858950166 ) ) ;
#62121 = ORIENTED_EDGE ( 'NONE', *, *, #23406, .F. ) ;
#62122 = CARTESIAN_POINT ( 'NONE',  ( -67.19292637653377653, -10.01517768586948698, 6.132527647946031529E-16 ) ) ;
#62123 = VECTOR ( 'NONE', #42183, 1000.000000000000000 ) ;
#62124 = FILL_AREA_STYLE_COLOUR ( '', #38000 ) ;
#62125 = CARTESIAN_POINT ( 'NONE',  ( 7.794228634059951588, -4.500000000000003553, 0.000000000000000000 ) ) ;
#62126 = CARTESIAN_POINT ( 'NONE',  ( -63.05499999999998550, -9.827790563157499189E-16, -8.024999999999991473 ) ) ;
#62127 = CARTESIAN_POINT ( 'NONE',  ( 12.75000000000000533, 27.74999999999998224, -3.750000000000000000 ) ) ;
#62128 = SURFACE_STYLE_FILL_AREA ( #7625 ) ;
#62129 = CARTESIAN_POINT ( 'NONE',  ( -63.59499999999997044, 2.607480562269072433, 8.024999999999991473 ) ) ;
#62130 = CARTESIAN_POINT ( 'NONE',  ( 3.094860106618431583, 157.2050000000000125, 9.525000000000000355 ) ) ;
#62131 = CIRCLE ( 'NONE', #3546, 110.0000000000000142 ) ;
#62132 = CARTESIAN_POINT ( 'NONE',  ( -142.7070736234666981, -3.094860106626767138, -9.524999999993935873 ) ) ;
#62133 = LINE ( 'NONE', #34377, #42483 ) ;
#62134 = UNCERTAINTY_MEASURE_WITH_UNIT (LENGTH_MEASURE( 1.000000000000000082E-05 ), #66825, 'distance_accuracy_value', 'NONE');
#62135 = CARTESIAN_POINT ( 'NONE',  ( -159.3570736234661922, 5.598654528085804216, 7.705886871421366635 ) ) ;
#62136 = VECTOR ( 'NONE', #60851, 1000.000000000000000 ) ;
#62137 = CARTESIAN_POINT ( 'NONE',  ( -4.886038412222122318, 110.6451352293558728, 8.015157697669311077 ) ) ;
#62138 = DIRECTION ( 'NONE',  ( 0.000000000000000000, 0.000000000000000000, 1.000000000000000000 ) ) ;
#62139 = AXIS2_PLACEMENT_3D ( 'NONE', #46924, #63039, #3937 ) ;
#62140 = CARTESIAN_POINT ( 'NONE',  ( 23.71231517720798010, 117.4999999999999716, -7.500000000000000000 ) ) ;
#62141 = DIRECTION ( 'NONE',  ( 0.000000000000000000, 0.000000000000000000, 1.000000000000000000 ) ) ;
#62142 = ORIENTED_EDGE ( 'NONE', *, *, #11086, .T. ) ;
#62143 = VERTEX_POINT ( 'NONE', #40304 ) ;
#62144 = AXIS2_PLACEMENT_3D ( 'NONE', #32981, #32603, #53407 ) ;
#62145 = DIRECTION ( 'NONE',  ( -0.6216216216216311485, 0.7833176619561784682, -5.204170427930414183E-15 ) ) ;
#62146 = DIRECTION ( 'NONE',  ( 0.000000000000000000, 0.000000000000000000, -1.000000000000000000 ) ) ;
#62147 = B_SPLINE_CURVE_WITH_KNOTS ( 'NONE', 3,
 ( #41821, #19958, #41458, #47093, #47458, #9789, #68179, #4827, #57613, #4458 ),
 .UNSPECIFIED., .F., .F.,
 ( 4, 2, 2, 2, 4 ),
 ( 0.000000000000000000, 0.0004222318702814410588, 0.0008444637405628821177, 0.001266695610844323231, 0.001688927481125764235 ),
 .UNSPECIFIED. ) ;
#62148 = EDGE_LOOP ( 'NONE', ( #60643, #20021, #1133, #3923 ) ) ;
#62149 = ORIENTED_EDGE ( 'NONE', *, *, #58444, .T. ) ;
#62150 = SURFACE_STYLE_FILL_AREA ( #29455 ) ;
#62151 =( NAMED_UNIT ( * ) SI_UNIT ( $, .STERADIAN. ) SOLID_ANGLE_UNIT ( ) );
#62152 = MECHANICAL_DESIGN_GEOMETRIC_PRESENTATION_REPRESENTATION (  '', ( #7144 ), #7304 ) ;
#62153 = EDGE_LOOP ( 'NONE', ( #28977, #12939, #54787, #54720 ) ) ;
#62154 = PRESENTATION_STYLE_ASSIGNMENT (( #40744 ) ) ;
#62155 = CARTESIAN_POINT ( 'NONE',  ( 23.50000000000001776, 43.00000000000000000, -29.68999999999999417 ) ) ;
#62156 = ORIENTED_EDGE ( 'NONE', *, *, #27286, .F. ) ;
#62157 = ADVANCED_FACE ( 'NONE', ( #35006 ), #62434, .F. ) ;
#62158 = COLOUR_RGB ( '', 0.09019608, 0.27058824, 0.51372549) ;
#62159 = VECTOR ( 'NONE', #37301, 1000.000000000000000 ) ;
#62160 = CARTESIAN_POINT ( 'NONE',  ( -157.5570736234661808, -1.166476076187852838E-15, -9.524999999999991473 ) ) ;
#62161 = DIRECTION ( 'NONE',  ( 0.5000000000000003331, -0.8660254037844383745, 0.000000000000000000 ) ) ;
#62162 = CARTESIAN_POINT ( 'NONE',  ( -113.6949999999999790, -8.437984349512085203, 5.166775262442717831E-16 ) ) ;
#62163 = VERTEX_POINT ( 'NONE', #56457 ) ;
#62164 = EDGE_CURVE ( 'NONE', #13621, #63169, #63444, .T. ) ;
#62165 = APPLICATION_CONTEXT ( 'automotive_design' ) ;
#62166 = MECHANICAL_DESIGN_GEOMETRIC_PRESENTATION_REPRESENTATION (  '', ( #61020 ), #26227 ) ;
#62167 = CARTESIAN_POINT ( 'NONE',  ( -9.534888206947428557, 110.4999999999999716, -0.06015242624886869144 ) ) ;
#62168 = CARTESIAN_POINT ( 'NONE',  ( -164.3070736234661808, -10.01517768586948698, 6.132527647946031529E-16 ) ) ;
#62169 = AXIS2_PLACEMENT_3D ( 'NONE', #22281, #44487, #6786 ) ;
#62170 = CARTESIAN_POINT ( 'NONE',  ( -9.827790563157511022E-16, 125.5570736234661524, 8.025000000000000355 ) ) ;
#62171 = VERTEX_POINT ( 'NONE', #67721 ) ;
#62172 = CARTESIAN_POINT ( 'NONE',  ( 7.632228543268608334, 149.3429263765338249, -2.479861379858951942 ) ) ;
#62173 = DIRECTION ( 'NONE',  ( 0.000000000000000000, 0.000000000000000000, -1.000000000000000000 ) ) ;
#62174 = SURFACE_STYLE_USAGE ( .BOTH. , #13288 ) ;
#62175 = PRESENTATION_STYLE_ASSIGNMENT (( #13645 ) ) ;
#62176 = CIRCLE ( 'NONE', #66667, 5.000000000000000000 ) ;
#62177 = VERTEX_POINT ( 'NONE', #68773 ) ;
#62178 =( LENGTH_UNIT ( ) NAMED_UNIT ( * ) SI_UNIT ( .MILLI., .METRE. ) );
#62179 = EDGE_CURVE ( 'NONE', #28517, #12794, #35329, .T. ) ;
#62180 = ORIENTED_EDGE ( 'NONE', *, *, #58859, .F. ) ;
#62181 = CARTESIAN_POINT ( 'NONE',  ( 4.716976649647099507, 128.6429263765338362, -6.492361379858953008 ) ) ;
#62182 = CARTESIAN_POINT ( 'NONE',  ( 57.00000000000000000, 5.000000000000000000, 65.00402776293825013 ) ) ;
#62183 = SURFACE_STYLE_USAGE ( .BOTH. , #51643 ) ;
#62184 = CYLINDRICAL_SURFACE ( 'NONE', #20904, 9.524999999999991473 ) ;
#62185 = CARTESIAN_POINT ( 'NONE',  ( -126.6549999999999869, -7.632228543268600340, -2.479861379858950166 ) ) ;
#62186 = COLOUR_RGB ( '', 0.66274510, 0.83137255, 0.94901961) ;
#62187 = CARTESIAN_POINT ( 'NONE',  ( -6.062177826491070398, -2.500000000000000000, -3.499999999999998224 ) ) ;
#62188 = CARTESIAN_POINT ( 'NONE',  ( 71.49999999999998579, 64.07124727947029896, 7.500000000000000000 ) ) ;
#62189 = DIRECTION ( 'NONE',  ( -1.000000000000000000, 0.000000000000000000, 1.300977106640434891E-16 ) ) ;
#62190 = MECHANICAL_DESIGN_GEOMETRIC_PRESENTATION_REPRESENTATION (  '', ( #48742 ), #8288 ) ;
#62191 = PRESENTATION_STYLE_ASSIGNMENT (( #29837 ) ) ;
#62192 = ADVANCED_FACE ( 'NONE', ( #30758 ), #3293, .F. ) ;
#62193 = CARTESIAN_POINT ( 'NONE',  ( -74.99999999999998579, 50.00000000000000000, 6.499999999999999112 ) ) ;
#62194 = CARTESIAN_POINT ( 'NONE',  ( -7.632228543268608334, 120.8429263765338249, 2.479861379858952830 ) ) ;
#62195 = ORIENTED_EDGE ( 'NONE', *, *, #9390, .F. ) ;
#62196 = ORIENTED_EDGE ( 'NONE', *, *, #23194, .F. ) ;
#62197 = CARTESIAN_POINT ( 'NONE',  ( -48.50000000000000000, 14.49137674618942562, 7.000000000000000000 ) ) ;
#62198 = AXIS2_PLACEMENT_3D ( 'NONE', #52776, #46128, #29914 ) ;
#62199 = CARTESIAN_POINT ( 'NONE',  ( -32.38698925772248316, -8.909055381080786873, -2.125700750517646398 ) ) ;
#62200 = FACE_OUTER_BOUND ( 'NONE', #23361, .T. ) ;
#62201 = CIRCLE ( 'NONE', #31866, 110.0000000000000142 ) ;
#62202 = CARTESIAN_POINT ( 'NONE',  ( -51.20499999999996277, -2.607480562269071545, -8.024999999999991473 ) ) ;
#62203 = ORIENTED_EDGE ( 'NONE', *, *, #61694, .T. ) ;
#62204 = LINE ( 'NONE', #14028, #69679 ) ;
#62205 = CARTESIAN_POINT ( 'NONE',  ( -179.1550000000000011, 7.632228543268600340, 2.479861379858949277 ) ) ;
#62206 = SURFACE_STYLE_USAGE ( .BOTH. , #29849 ) ;
#62207 = CARTESIAN_POINT ( 'NONE',  ( -56.30707362346618794, -10.01517768586948698, 6.132527647946031529E-16 ) ) ;
#62208 = AXIS2_PLACEMENT_3D ( 'NONE', #37408, #58811, #1013 ) ;
#62209 = CARTESIAN_POINT ( 'NONE',  ( -177.4449999999999932, 0.000000000000000000, 8.024999999999991473 ) ) ;
#62210 = CARTESIAN_POINT ( 'NONE',  ( 41.38221592241693259, 107.7000202725880769, 3.906946855746215697 ) ) ;
#62211 = ORIENTED_EDGE ( 'NONE', *, *, #735, .T. ) ;
#62212 =( BOUNDED_CURVE ( )  B_SPLINE_CURVE ( 2, ( #64325, #64683, #48194, #60084, #237, #16178, #58709, #27006, #48891, #38331, #22457 ),
 .UNSPECIFIED., .F., .F. ) 
 B_SPLINE_CURVE_WITH_KNOTS ( ( 3, 2, 2, 2, 2, 3 ),
 ( 0.5588235294117649410, 0.5647058823529413907, 0.5705882352941178404, 0.5764705882352942901, 0.5823529411764708508, 0.5882352941176473005 ),
 .UNSPECIFIED. ) 
 CURVE ( )  GEOMETRIC_REPRESENTATION_ITEM ( )  RATIONAL_B_SPLINE_CURVE ( ( 0.9999999999999981126, 0.9510565162951554186, 1.000000000000000000, 0.9510565162951535312, 1.000000000000000000, 0.9510565162951535312, 1.000000000000000000, 0.9510565162951535312, 1.000000000000000000, 0.9510565162951516438, 1.000000000000001776 ) ) 
 REPRESENTATION_ITEM ( '' )  );
#62213 = CARTESIAN_POINT ( 'NONE',  ( -161.6070736234661354, -8.102448949553174629, 5.886773742842742685 ) ) ;
#62214 = PRESENTATION_LAYER_ASSIGNMENT (  '', '', ( #22919 ) ) ;
#62215 = CARTESIAN_POINT ( 'NONE',  ( -163.5570736234661524, -1.166476076187852838E-15, -9.524999999999991473 ) ) ;
#62216 = CARTESIAN_POINT ( 'NONE',  ( -88.40499999999997272, -2.607480562269069768, 8.024999999999991473 ) ) ;
#62217 =( NAMED_UNIT ( * ) SI_UNIT ( $, .STERADIAN. ) SOLID_ANGLE_UNIT ( ) );
#62218 = DIRECTION ( 'NONE',  ( 0.000000000000000000, 0.000000000000000000, 1.000000000000000000 ) ) ;
#62219 = MECHANICAL_DESIGN_GEOMETRIC_PRESENTATION_REPRESENTATION (  '', ( #27346 ), #40920 ) ;
#62220 = CARTESIAN_POINT ( 'NONE',  ( -88.34499999999999886, 7.632228543268599452, -2.479861379858951942 ) ) ;
#62221 = CARTESIAN_POINT ( 'NONE',  ( -9.058813317711338797, 120.4549999999999983, 2.943386871421373563 ) ) ;
#62222 = CARTESIAN_POINT ( 'NONE',  ( -67.34499999999998465, 7.632228543268599452, -2.479861379858951942 ) ) ;
#62223 = CARTESIAN_POINT ( 'NONE',  ( 0.2500000000000000000, 36.74999999999999289, 4.000000000000000000 ) ) ;
#62224 = STYLED_ITEM ( 'NONE', ( #13541 ), #61971 ) ;
#62225 = DIRECTION ( 'NONE',  ( 1.000000000000000000, 0.000000000000000000, 0.000000000000000000 ) ) ;
#62226 = DIRECTION ( 'NONE',  ( 1.000000000000000000, -0.000000000000000000, 1.982541115402068561E-16 ) ) ;
#62227 = UNCERTAINTY_MEASURE_WITH_UNIT (LENGTH_MEASURE( 1.000000000000000082E-05 ), #49297, 'distance_accuracy_value', 'NONE');
#62228 = EDGE_CURVE ( 'NONE', #16390, #5105, #20564, .T. ) ;
#62229 = DIRECTION ( 'NONE',  ( 0.000000000000000000, 0.000000000000000000, 1.000000000000000000 ) ) ;
#62230 = CARTESIAN_POINT ( 'NONE',  ( 10.99999999999999645, 11.99999999999999289, 3.500000000000004885 ) ) ;
#62231 = VERTEX_POINT ( 'NONE', #41355 ) ;
#62232 = CARTESIAN_POINT ( 'NONE',  ( -112.3429263765337964, -9.058813317711329915, 2.943386871421371787 ) ) ;
#62233 = CARTESIAN_POINT ( 'NONE',  ( -127.6450000000000102, 4.716976649647091513, -6.492361379858946790 ) ) ;
#62234 = CYLINDRICAL_SURFACE ( 'NONE', #52801, 2.499999999999998668 ) ;
#62235 = AXIS2_PLACEMENT_3D ( 'NONE', #37738, #9590, #26420 ) ;
#62236 = LINE ( 'NONE', #35523, #66258 ) ;
#62238 = CARTESIAN_POINT ( 'NONE',  ( 98.00000000000000000, 14.00000000000000000, 12.50000000000000178 ) ) ;
#62237 = CARTESIAN_POINT ( 'NONE',  ( -131.0929263765344785, 3.094860106629860663, 9.524999999991687005 ) ) ;
#62239 = CARTESIAN_POINT ( 'NONE',  ( 23.71231517720798010, 113.4999999999999858, -9.500000000000000000 ) ) ;
#62240 = ORIENTED_EDGE ( 'NONE', *, *, #20519, .F. ) ;
#62241 = ORIENTED_EDGE ( 'NONE', *, *, #40681, .T. ) ;
#62242 = CIRCLE ( 'NONE', #30749, 0.5000000000000004441 ) ;
#62243 = DIRECTION ( 'NONE',  ( -1.000000000000000000, 0.000000000000000000, 0.000000000000000000 ) ) ;
#62244 = CARTESIAN_POINT ( 'NONE',  ( 28.00000000000000000, 38.70020753820971748, -89.00000000000000000 ) ) ;
#62245 = CARTESIAN_POINT ( 'NONE',  ( 52.75000000000000000, 24.99999999999998579, 3.750000000000000000 ) ) ;
#62246 = DIRECTION ( 'NONE',  ( 0.000000000000000000, 0.000000000000000000, 1.000000000000000000 ) ) ;
#62247 =( LENGTH_UNIT ( ) NAMED_UNIT ( * ) SI_UNIT ( .MILLI., .METRE. ) );
#62248 = VERTEX_POINT ( 'NONE', #9333 ) ;
#62249 = CARTESIAN_POINT ( 'NONE',  ( -133.5549999999999784, 0.000000000000000000, 8.024999999999991473 ) ) ;
#62251 = EDGE_CURVE ( 'NONE', #42518, #31691, #14598, .T. ) ;
#62250 = ORIENTED_EDGE ( 'NONE', *, *, #51381, .T. ) ;
#62252 = SURFACE_STYLE_FILL_AREA ( #65893 ) ;
#62253 = CARTESIAN_POINT ( 'NONE',  ( -125.1570736234661751, -9.058813317711329915, -2.943386871421370898 ) ) ;
#62254 = EDGE_CURVE ( 'NONE', #31566, #23198, #26312, .T. ) ;
#62255 = EDGE_LOOP ( 'NONE', ( #17210, #6888 ) ) ;
#62256 = DIRECTION ( 'NONE',  ( -0.000000000000000000, 1.000000000000000000, -0.000000000000000000 ) ) ;
#62257 = DIRECTION ( 'NONE',  ( 0.000000000000000000, 0.000000000000000000, 1.000000000000000000 ) ) ;
#62258 = VERTEX_POINT ( 'NONE', #68411 ) ;
#62259 = CARTESIAN_POINT ( 'NONE',  ( -74.08452722063037754, 9.430195807687216103, -6.000000000000000000 ) ) ;
#62260 = CARTESIAN_POINT ( 'NONE',  ( -5.598654528085808657, 137.6449999999999818, 7.705886871421373741 ) ) ;
#62261 = LINE ( 'NONE', #23933, #34020 ) ;
#62262 = VECTOR ( 'NONE', #7880, 1000.000000000000000 ) ;
#62263 = ORIENTED_EDGE ( 'NONE', *, *, #13410, .F. ) ;
#62264 = MECHANICAL_DESIGN_GEOMETRIC_PRESENTATION_REPRESENTATION (  '', ( #8404 ), #63434 ) ;
#62265 = CARTESIAN_POINT ( 'NONE',  ( 32.00000000000002132, 43.00000000000000000, 79.00402776293823592 ) ) ;
#62267 = EDGE_CURVE ( 'NONE', #16387, #44244, #42153, .T. ) ;
#62266 = CARTESIAN_POINT ( 'NONE',  ( 9.058813317711338797, 139.9549999999999841, -2.943386871421372675 ) ) ;
#62268 =( NAMED_UNIT ( * ) PLANE_ANGLE_UNIT ( ) SI_UNIT ( $, .RADIAN. ) );
#62269 = ORIENTED_EDGE ( 'NONE', *, *, #28386, .F. ) ;
#62270 = CARTESIAN_POINT ( 'NONE',  ( -2.607480562269073765, 120.0929263765337964, -8.025000000000000355 ) ) ;
#62271 = UNCERTAINTY_MEASURE_WITH_UNIT (LENGTH_MEASURE( 1.000000000000000082E-05 ), #38594, 'distance_accuracy_value', 'NONE');
#62272 = PRESENTATION_STYLE_ASSIGNMENT (( #39549 ) ) ;
#62273 = CARTESIAN_POINT ( 'NONE',  ( -72.00000000000000000, 36.32520566882265456, -7.000000000000000000 ) ) ;
#62274 = VECTOR ( 'NONE', #66545, 1000.000000000000000 ) ;
#62275 = SPHERICAL_SURFACE ( 'NONE', #11463, 0.5000000000000000000 ) ;
#62276 = DIRECTION ( 'NONE',  ( 0.000000000000000000, 1.000000000000000000, 0.000000000000000000 ) ) ;
#62277 = EDGE_LOOP ( 'NONE', ( #61618, #62851, #67478, #31371 ) ) ;
#62278 = CARTESIAN_POINT ( 'NONE',  ( -3.109213548236405611, -9.000000000000007105, 0.5129086262188669032 ) ) ;
#62279 = ADVANCED_FACE ( 'NONE', ( #41707 ), #63130, .T. ) ;
#62280 = ORIENTED_EDGE ( 'NONE', *, *, #64751, .F. ) ;
#62281 = CARTESIAN_POINT ( 'NONE',  ( -45.50000000000000000, -2.024042244987997205E-14, 6.500000000000000000 ) ) ;
#62282 = AXIS2_PLACEMENT_3D ( 'NONE', #68072, #30386, #46654 ) ;
#62283 = COLOUR_RGB ( '', 0.40784314, 0.44705882, 0.49803922) ;
#62284 = CARTESIAN_POINT ( 'NONE',  ( -30.41309959971616195, -7.810440804527638115, -1.036248593184375899 ) ) ;
#62285 = CARTESIAN_POINT ( 'NONE',  ( -48.74730009840026668, -11.41203371166892744, 3.454827790524563014 ) ) ;
#62286 = CARTESIAN_POINT ( 'NONE',  ( -153.6549999999999727, -7.632228543268600340, -2.479861379858950166 ) ) ;
#62287 = VERTEX_POINT ( 'NONE', #6116 ) ;
#62288 =( NAMED_UNIT ( * ) SI_UNIT ( $, .STERADIAN. ) SOLID_ANGLE_UNIT ( ) );
#62289 = UNCERTAINTY_MEASURE_WITH_UNIT (LENGTH_MEASURE( 1.000000000000000082E-05 ), #44266, 'distance_accuracy_value', 'NONE');
#62290 = SURFACE_SIDE_STYLE ('',( #40872 ) ) ;
#62291 = EDGE_CURVE ( 'NONE', #51395, #51817, #53611, .T. ) ;
#62292 = LINE ( 'NONE', #41555, #58562 ) ;
#62293 = CARTESIAN_POINT ( 'NONE',  ( 74.65811388299935913, 19.88603796099976151, 6.065461639931116089 ) ) ;
#62294 = DIRECTION ( 'NONE',  ( 0.000000000000000000, 1.000000000000000000, 6.938893903907234689E-15 ) ) ;
#62295 = ORIENTED_EDGE ( 'NONE', *, *, #60425, .F. ) ;
#62296 = DIRECTION ( 'NONE',  ( 0.000000000000000000, 0.000000000000000000, 1.000000000000000000 ) ) ;
#62297 = VERTEX_POINT ( 'NONE', #59209 ) ;
#62298 =( LENGTH_UNIT ( ) NAMED_UNIT ( * ) SI_UNIT ( .MILLI., .METRE. ) );
#62299 = SURFACE_STYLE_USAGE ( .BOTH. , #30970 ) ;
#62300 = CARTESIAN_POINT ( 'NONE',  ( -71.15499999999998693, 7.632228543268600340, 2.479861379858949277 ) ) ;
#62302 = VERTEX_POINT ( 'NONE', #31802 ) ;
#62301 = AXIS2_PLACEMENT_3D ( 'NONE', #7410, #44396, #6350 ) ;
#62303 = AXIS2_PLACEMENT_3D ( 'NONE', #22199, #16269, #33107 ) ;
#62304 = CARTESIAN_POINT ( 'NONE',  ( 14.98999599679679662, 146.4999999999999716, -10.00000000000000000 ) ) ;
#62305 = CARTESIAN_POINT ( 'NONE',  ( -18.25000000000000711, 31.24999999999999289, -4.000000000000000000 ) ) ;
#62306 = ORIENTED_EDGE ( 'NONE', *, *, #42396, .F. ) ;
#62307 = VECTOR ( 'NONE', #64746, 1000.000000000000114 ) ;
#62308 =( NAMED_UNIT ( * ) SI_UNIT ( $, .STERADIAN. ) SOLID_ANGLE_UNIT ( ) );
#62309 = FACE_OUTER_BOUND ( 'NONE', #3756, .T. ) ;
#62310 =( BOUNDED_CURVE ( )  B_SPLINE_CURVE ( 3, ( #50368, #24317, #12718, #23622 ),
 .UNSPECIFIED., .F., .T. ) 
 B_SPLINE_CURVE_WITH_KNOTS ( ( 4, 4 ),
 ( 4.712388980384691450, 5.550147021341966358 ),
 .UNSPECIFIED. ) 
 CURVE ( )  GEOMETRIC_REPRESENTATION_ITEM ( )  RATIONAL_B_SPLINE_CURVE ( ( 1.000000000000000000, 0.9423636384284010958, 0.9423636384284010958, 1.000000000000000000 ) ) 
 REPRESENTATION_ITEM ( '' )  );
#62312 = CARTESIAN_POINT ( 'NONE',  ( 22.99999999999996092, 5.000000000000000000, -77.00402776293825013 ) ) ;
#62311 = CARTESIAN_POINT ( 'NONE',  ( 14.98999599679679662, 146.9999999999999716, 10.00000000000000000 ) ) ;
#62313 = CARTESIAN_POINT ( 'NONE',  ( -5.598654528085808657, 137.6449999999999818, 7.705886871421373741 ) ) ;
#62314 = CARTESIAN_POINT ( 'NONE',  ( -99.89499999999998181, 6.826472737025116366, 4.959722759717898555 ) ) ;
#62315 = FILL_AREA_STYLE ('',( #24654 ) ) ;
#62316 = UNCERTAINTY_MEASURE_WITH_UNIT (LENGTH_MEASURE( 1.000000000000000082E-05 ), #32324, 'distance_accuracy_value', 'NONE');
#62317 = ADVANCED_FACE ( 'NONE', ( #27547 ), #26523, .T. ) ;
#62318 = CYLINDRICAL_SURFACE ( 'NONE', #42696, 5.000000000000000000 ) ;
#62319 =( GEOMETRIC_REPRESENTATION_CONTEXT ( 3 ) GLOBAL_UNCERTAINTY_ASSIGNED_CONTEXT ( ( #39835 ) ) GLOBAL_UNIT_ASSIGNED_CONTEXT ( ( #69086, #9993, #25802 ) ) REPRESENTATION_CONTEXT ( 'NONE', 'WORKASPACE' ) );
#62320 = VERTEX_POINT ( 'NONE', #5070 ) ;
#62321 = CARTESIAN_POINT ( 'NONE',  ( -141.4429263765337907, -1.166476076187852838E-15, -9.524999999999991473 ) ) ;
#62322 = LINE ( 'NONE', #49788, #32104 ) ;
#62323 = CARTESIAN_POINT ( 'NONE',  ( -155.6949999999999932, -8.437984349512085203, 5.166775262442717831E-16 ) ) ;
#62324 = AXIS2_PLACEMENT_3D ( 'NONE', #14452, #35930, #57376 ) ;
#62325 = AXIS2_PLACEMENT_3D ( 'NONE', #43784, #425, #17039 ) ;
#62326 = COLOUR_RGB ( '', 0.09019608, 0.27058824, 0.51372549) ;
#62327 = ORIENTED_EDGE ( 'NONE', *, *, #15131, .T. ) ;
#62328 = DIRECTION ( 'NONE',  ( 0.000000000000000000, 0.000000000000000000, -1.000000000000000000 ) ) ;
#62329 = ORIENTED_EDGE ( 'NONE', *, *, #50376, .F. ) ;
#62330 = TOROIDAL_SURFACE ( 'NONE', #48925, 0.5000000000000000000, 0.2500000000000000000 ) ;
#62331 =( BOUNDED_CURVE ( )  B_SPLINE_CURVE ( 2, ( #22588, #44090, #17342, #65844, #38804, #60217, #43411, #49678, #6054, #27823, #21900 ),
 .UNSPECIFIED., .F., .F. ) 
 B_SPLINE_CURVE_WITH_KNOTS ( ( 3, 2, 2, 2, 2, 3 ),
 ( 0.7717391304347825942, 0.7739130434782608425, 0.7760869565217390909, 0.7782608695652173392, 0.7804347826086956985, 0.7826086956521739468 ),
 .UNSPECIFIED. ) 
 CURVE ( )  GEOMETRIC_REPRESENTATION_ITEM ( )  RATIONAL_B_SPLINE_CURVE ( ( 1.000000000000000000, 0.9510565162951535312, 1.000000000000000000, 0.9510565162951535312, 1.000000000000000000, 0.9510565162951535312, 1.000000000000000000, 0.9510565162951535312, 1.000000000000000000, 0.9510565162951535312, 1.000000000000000000 ) ) 
 REPRESENTATION_ITEM ( '' )  );
#62332 = DIRECTION ( 'NONE',  ( 0.000000000000000000, 0.000000000000000000, -1.000000000000000000 ) ) ;
#62333 = EDGE_CURVE ( 'NONE', #45721, #16530, #1564, .T. ) ;
#62334 = SURFACE_STYLE_USAGE ( .BOTH. , #51435 ) ;
#62335 = CARTESIAN_POINT ( 'NONE',  ( -173.9070736234663173, -3.094860106616648121, 9.525000000001288214 ) ) ;
#62336 = DIRECTION ( 'NONE',  ( 0.000000000000000000, 0.000000000000000000, -1.000000000000000000 ) ) ;
#62337 = ORIENTED_EDGE ( 'NONE', *, *, #39023, .T. ) ;
#62338 = CARTESIAN_POINT ( 'NONE',  ( -159.5049999999999955, -6.826472737025113702, -4.959722759717900331 ) ) ;
#62339 = EDGE_CURVE ( 'NONE', #30128, #38068, #11034, .T. ) ;
#62340 = VECTOR ( 'NONE', #61371, 1000.000000000000000 ) ;
#62341 = EDGE_CURVE ( 'NONE', #54390, #43795, #69079, .T. ) ;
#62342 = EDGE_LOOP ( 'NONE', ( #63675, #8953, #9846, #50751 ) ) ;
#62343 = CARTESIAN_POINT ( 'NONE',  ( 0.000000000000000000, 114.4999999999999574, 0.000000000000000000 ) ) ;
#62344 = ORIENTED_EDGE ( 'NONE', *, *, #42331, .T. ) ;
#62345 = AXIS2_PLACEMENT_3D ( 'NONE', #20120, #9261, #25074 ) ;
#62346 = DIRECTION ( 'NONE',  ( -1.000000000000000000, -0.000000000000000000, -0.000000000000000000 ) ) ;
#62347 = DIRECTION ( 'NONE',  ( 0.000000000000000000, 0.000000000000000000, -1.000000000000000000 ) ) ;
#62348 = CARTESIAN_POINT ( 'NONE',  ( 4.716976649647096842, 158.8570736234661638, 6.492361379858953896 ) ) ;
#62349 = AXIS2_PLACEMENT_3D ( 'NONE', #25400, #31020, #51447 ) ;
#62350 = ORIENTED_EDGE ( 'NONE', *, *, #29628, .F. ) ;
#62351 = FACE_BOUND ( 'NONE', #16128, .T. ) ;
#62353 = EDGE_CURVE ( 'NONE', #58540, #849, #47713, .T. ) ;
#62352 = CARTESIAN_POINT ( 'NONE',  ( 10.01517768586949408, 112.8049999999999784, 1.839758294383810543E-15 ) ) ;
#62354 = CARTESIAN_POINT ( 'NONE',  ( -70.70499999999996987, 2.607480562269072433, 8.024999999999991473 ) ) ;
#62355 = AXIS2_PLACEMENT_3D ( 'NONE', #44964, #24484, #50561 ) ;
#62356 = ORIENTED_EDGE ( 'NONE', *, *, #27918, .F. ) ;
#62357 = CARTESIAN_POINT ( 'NONE',  ( 5.598654528085809545, 140.2549999999999955, -7.705886871421373741 ) ) ;
#62358 = UNCERTAINTY_MEASURE_WITH_UNIT (LENGTH_MEASURE( 1.000000000000000082E-05 ), #25013, 'distance_accuracy_value', 'NONE');
#62359 = DIRECTION ( 'NONE',  ( 0.000000000000000000, 0.000000000000000000, 1.000000000000000000 ) ) ;
#62360 =( NAMED_UNIT ( * ) PLANE_ANGLE_UNIT ( ) SI_UNIT ( $, .RADIAN. ) );
#62361 = EDGE_CURVE ( 'NONE', #1406, #40324, #42420, .T. ) ;
#62362 = CARTESIAN_POINT ( 'NONE',  ( 20.17690446313311625, 115.4776478016129460, 10.00000000000000000 ) ) ;
#62363 = FILL_AREA_STYLE_COLOUR ( '', #46373 ) ;
#62364 = ORIENTED_EDGE ( 'NONE', *, *, #54151, .T. ) ;
#62365 = CARTESIAN_POINT ( 'NONE',  ( -7.440601873764705054, -2.005109422339667269, -1.112499515747341183 ) ) ;
#62366 = CARTESIAN_POINT ( 'NONE',  ( -55.49499999999999034, 6.826472737025113702, -4.959722759717902107 ) ) ;
#62367 = ORIENTED_EDGE ( 'NONE', *, *, #31902, .T. ) ;
#62368 = CARTESIAN_POINT ( 'NONE',  ( 5.038399427696168331, 111.0805650589046820, 7.410012812680835559 ) ) ;
#62369 = COLOUR_RGB ( '', 0.40784314, 0.44705882, 0.49803922) ;
#62370 = CARTESIAN_POINT ( 'NONE',  ( 75.00000000000000000, -2.215169945516535778E-14, 9.500000000000000000 ) ) ;
#62371 = CARTESIAN_POINT ( 'NONE',  ( -34.75000000000000000, 0.000000000000000000, -2.000000000000000000 ) ) ;
#62372 = ORIENTED_EDGE ( 'NONE', *, *, #39993, .T. ) ;
#62373 = FACE_OUTER_BOUND ( 'NONE', #67968, .T. ) ;
#62374 = LINE ( 'NONE', #52541, #10832 ) ;
#62375 = ORIENTED_EDGE ( 'NONE', *, *, #46847, .F. ) ;
#62376 = DIRECTION ( 'NONE',  ( -0.000000000000000000, -0.000000000000000000, 1.000000000000000000 ) ) ;
#62377 = CARTESIAN_POINT ( 'NONE',  ( -101.9049999999999869, 2.607480562269068880, -8.024999999999993250 ) ) ;
#62378 = EDGE_LOOP ( 'NONE', ( #61581, #21036, #9238, #35263 ) ) ;
#62379 = EDGE_CURVE ( 'NONE', #23681, #56835, #12862, .T. ) ;
#62380 = SURFACE_STYLE_FILL_AREA ( #52547 ) ;
#62381 =( NAMED_UNIT ( * ) PLANE_ANGLE_UNIT ( ) SI_UNIT ( $, .RADIAN. ) );
#62382 = AXIS2_PLACEMENT_3D ( 'NONE', #52759, #4534, #68937 ) ;
#62383 = CARTESIAN_POINT ( 'NONE',  ( -140.0070736234661979, -8.102448949553172852, -5.886773742842741797 ) ) ;
#62384 = CIRCLE ( 'NONE', #19697, 22.50000000000000000 ) ;
#62385 = ADVANCED_FACE ( 'NONE', ( #54294 ), #37682, .T. ) ;
#62386 = CARTESIAN_POINT ( 'NONE',  ( -72.50000000000000000, 36.32520566882265456, 9.500000000000000000 ) ) ;
#62387 = CARTESIAN_POINT ( 'NONE',  ( 0.000000000000000000, 142.4449999999999932, -9.525000000000000355 ) ) ;
#62388 = CARTESIAN_POINT ( 'NONE',  ( -78.20707362346615810, 3.094860106618433360, 9.524999999999991473 ) ) ;
#62389 = CARTESIAN_POINT ( 'NONE',  ( 15.98999599679679839, 147.4999999999999716, -9.500000000000000000 ) ) ;
#62390 = VERTEX_POINT ( 'NONE', #31445 ) ;
#62391 = DIRECTION ( 'NONE',  ( 1.000000000000000000, -0.000000000000000000, 0.000000000000000000 ) ) ;
#62392 = CARTESIAN_POINT ( 'NONE',  ( -18.05714352263349909, -11.32599168300350279, -3.969768029961437072 ) ) ;
#62394 = CARTESIAN_POINT ( 'NONE',  ( -99.74292637653380211, -5.598654528085803328, -7.705886871421366635 ) ) ;
#62393 = LINE ( 'NONE', #56413, #8788 ) ;
#62395 = CARTESIAN_POINT ( 'NONE',  ( -122.4549999999999983, 7.632228543268599452, -2.479861379858951942 ) ) ;
#62396 = CARTESIAN_POINT ( 'NONE',  ( -158.5429263765338135, 9.058813317711329915, 2.943386871421369566 ) ) ;
#62397 = CARTESIAN_POINT ( 'NONE',  ( -5.598654528085808657, 110.6449999999999960, 7.705886871421373741 ) ) ;
#62398 = CARTESIAN_POINT ( 'NONE',  ( -129.4449999999999648, 0.000000000000000000, 8.024999999999991473 ) ) ;
#62399 = CARTESIAN_POINT ( 'NONE',  ( -120.1449999999999818, -4.716976649647092401, 6.492361379858946790 ) ) ;
#62400 =( LENGTH_UNIT ( ) NAMED_UNIT ( * ) SI_UNIT ( .MILLI., .METRE. ) );
#62401 = ORIENTED_EDGE ( 'NONE', *, *, #26199, .F. ) ;
#62402 = PRESENTATION_LAYER_ASSIGNMENT (  '', '', ( #27526 ) ) ;
#62403 = CARTESIAN_POINT ( 'NONE',  ( 74.50000000000000000, -2.135340797662720349E-14, 10.00000000000000000 ) ) ;
#62404 = VECTOR ( 'NONE', #2203, 1000.000000000000000 ) ;
#62405 = CARTESIAN_POINT ( 'NONE',  ( -176.9929263765337737, 8.102448949553171076, -5.886773742842744461 ) ) ;
#62406 =( NAMED_UNIT ( * ) SI_UNIT ( $, .STERADIAN. ) SOLID_ANGLE_UNIT ( ) );
#62407 = CARTESIAN_POINT ( 'NONE',  ( 8.252730563585677359, -3.705851362693088458, 0.03572125916567005927 ) ) ;
#62408 = SURFACE_SIDE_STYLE ('',( #45907 ) ) ;
#62409 = EDGE_CURVE ( 'NONE', #54497, #62454, #59952, .T. ) ;
#62410 = DIRECTION ( 'NONE',  ( -0.000000000000000000, -0.000000000000000000, -1.000000000000000000 ) ) ;
#62411 = CARTESIAN_POINT ( 'NONE',  ( -0.7098155475105565326, -7.000000000000003553, 0.02753250691854188317 ) ) ;
#62412 = ORIENTED_EDGE ( 'NONE', *, *, #29359, .T. ) ;
#62414 = CARTESIAN_POINT ( 'NONE',  ( -88.49292637653381632, -8.102448949553172852, 5.886773742842742685 ) ) ;
#62413 = B_SPLINE_CURVE_WITH_KNOTS ( 'NONE', 3,
 ( #30160, #34420, #35473, #2713, #50603, #40769, #45370, #13294 ),
 .UNSPECIFIED., .F., .F.,
 ( 4, 2, 2, 4 ),
 ( 0.000000000000000000, 0.0002391162403816553283, 0.0004782324807633106566, 0.0009564649615266002797 ),
 .UNSPECIFIED. ) ;
#62415 = SHAPE_DEFINITION_REPRESENTATION ( #15361, #40670 ) ;
#62416 = DIRECTION ( 'NONE',  ( -0.000000000000000000, -1.000000000000000000, -0.000000000000000000 ) ) ;
#62417 = CIRCLE ( 'NONE', #19681, 0.4999999999999991118 ) ;
#62418 = ADVANCED_FACE ( 'NONE', ( #6797 ), #12767, .T. ) ;
#62419 = CARTESIAN_POINT ( 'NONE',  ( 32.00000000000002132, 50.00000000000000000, 59.99999999999999289 ) ) ;
#62420 = CARTESIAN_POINT ( 'NONE',  ( -162.5929263765341091, -3.094860106623204210, -9.524999999996525801 ) ) ;
#62421 = VECTOR ( 'NONE', #69343, 1000.000000000000000 ) ;
#62422 = CARTESIAN_POINT ( 'NONE',  ( 1.000000000000000888, 1.000000000000000222, 4.000000000000000000 ) ) ;
#62423 = EDGE_CURVE ( 'NONE', #51271, #13202, #55441, .T. ) ;
#62424 = ORIENTED_EDGE ( 'NONE', *, *, #51404, .F. ) ;
#62425 = CARTESIAN_POINT ( 'NONE',  ( 5.356721384544675502, 4.721886399977926807, 0.1324414877861175011 ) ) ;
#62426 =( LENGTH_UNIT ( ) NAMED_UNIT ( * ) SI_UNIT ( .MILLI., .METRE. ) );
#62427 = CARTESIAN_POINT ( 'NONE',  ( -21.02379604162863913, 109.9999999999999858, 9.500000000000000000 ) ) ;
#62428 = ORIENTED_EDGE ( 'NONE', *, *, #66953, .F. ) ;
#62429 = CARTESIAN_POINT ( 'NONE',  ( -103.6429263765337936, -5.598654528085801552, 7.705886871421367523 ) ) ;
#62430 = CARTESIAN_POINT ( 'NONE',  ( -4.716976649647097730, 136.3570736234661638, -6.492361379858953896 ) ) ;
#62431 = VERTEX_POINT ( 'NONE', #55693 ) ;
#62432 = SURFACE_SIDE_STYLE ('',( #8631 ) ) ;
#62433 = CARTESIAN_POINT ( 'NONE',  ( -105.8049999999999926, -8.437984349512086979, 5.166775262442717831E-16 ) ) ;
#62434 = SPHERICAL_SURFACE ( 'NONE', #38773, 1.000000000000000000 ) ;
#62435 = VERTEX_POINT ( 'NONE', #44152 ) ;
#62436 = SURFACE_STYLE_USAGE ( .BOTH. , #2946 ) ;
#62437 = EDGE_CURVE ( 'NONE', #19491, #15394, #37532, .T. ) ;
#62438 = CIRCLE ( 'NONE', #43378, 5.499999999999976907 ) ;
#62439 = SURFACE_SIDE_STYLE ('',( #29737 ) ) ;
#62440 = CARTESIAN_POINT ( 'NONE',  ( 2.607480562269118174, 150.9070736234661751, -8.024999999999970157 ) ) ;
#62441 = PRESENTATION_LAYER_ASSIGNMENT (  '', '', ( #23141 ) ) ;
#62442 = AXIS2_PLACEMENT_3D ( 'NONE', #3867, #9191, #35575 ) ;
#62443 = FACE_OUTER_BOUND ( 'NONE', #43381, .T. ) ;
#62444 = CARTESIAN_POINT ( 'NONE',  ( -81.44499999999999318, 0.000000000000000000, 8.024999999999991473 ) ) ;
#62445 = EDGE_LOOP ( 'NONE', ( #115, #68869, #37383, #41049 ) ) ;
#62446 = VECTOR ( 'NONE', #50247, 1000.000000000000000 ) ;
#62447 = FILL_AREA_STYLE_COLOUR ( '', #62090 ) ;
#62448 = CIRCLE ( 'NONE', #63551, 0.5000000000000004441 ) ;
#62449 = ORIENTED_EDGE ( 'NONE', *, *, #12064, .F. ) ;
#62450 = DIRECTION ( 'NONE',  ( 0.000000000000000000, 0.000000000000000000, 1.000000000000000000 ) ) ;
#62451 = CARTESIAN_POINT ( 'NONE',  ( 71.49999999999998579, 64.07124727947029896, -9.500000000000000000 ) ) ;
#62452 = DIRECTION ( 'NONE',  ( 0.000000000000000000, 0.000000000000000000, 1.000000000000000000 ) ) ;
#62453 = ORIENTED_EDGE ( 'NONE', *, *, #59014, .T. ) ;
#62454 = VERTEX_POINT ( 'NONE', #29289 ) ;
#62455 = CARTESIAN_POINT ( 'NONE',  ( 12.50000000000000355, 30.99999999999998579, 3.750000000000000000 ) ) ;
#62456 = CARTESIAN_POINT ( 'NONE',  ( -173.6070736234661638, -8.102448949553172852, 5.886773742842742685 ) ) ;
#62457 = ADVANCED_FACE ( 'NONE', ( #39545 ), #7502, .F. ) ;
#62458 = DIRECTION ( 'NONE',  ( -1.000000000000000000, 0.000000000000000000, 0.000000000000000000 ) ) ;
#62459 = CARTESIAN_POINT ( 'NONE',  ( 8.102448949553181734, 117.9949999999999619, -5.886773742842746238 ) ) ;
#62460 = CARTESIAN_POINT ( 'NONE',  ( -105.2070736234661723, 3.094860106618433360, 9.524999999999991473 ) ) ;
#62461 =( GEOMETRIC_REPRESENTATION_CONTEXT ( 3 ) GLOBAL_UNCERTAINTY_ASSIGNED_CONTEXT ( ( #53135 ) ) GLOBAL_UNIT_ASSIGNED_CONTEXT ( ( #36484, #20605, #51574 ) ) REPRESENTATION_CONTEXT ( 'NONE', 'WORKASPACE' ) );
#62462 = CARTESIAN_POINT ( 'NONE',  ( -9.827790563157511022E-16, 133.4429263765338192, 8.025000000000000355 ) ) ;
#62463 = ORIENTED_EDGE ( 'NONE', *, *, #42389, .F. ) ;
#62464 = CARTESIAN_POINT ( 'NONE',  ( -108.2929263765347656, 3.094860106602562944, -9.525000000011520029 ) ) ;
#62466 = CARTESIAN_POINT ( 'NONE',  ( -114.2070736234670250, 3.094860106632685071, 9.524999999989637089 ) ) ;
#62465 = FACE_OUTER_BOUND ( 'NONE', #57892, .T. ) ;
#62468 = CARTESIAN_POINT ( 'NONE',  ( -60.00000000000000000, -2.024042244987997205E-14, 7.500000000000000000 ) ) ;
#62467 = CIRCLE ( 'NONE', #13064, 27.49999999999999645 ) ;
#62469 = CARTESIAN_POINT ( 'NONE',  ( -151.2549999999999955, -4.716976649647092401, 6.492361379858946790 ) ) ;
#62470 = SURFACE_STYLE_USAGE ( .BOTH. , #67760 ) ;
#62471 = CARTESIAN_POINT ( 'NONE',  ( -153.4449999999999932, 0.000000000000000000, 8.024999999999991473 ) ) ;
#62472 = CARTESIAN_POINT ( 'NONE',  ( -143.8449999999999989, -7.632228543268599452, 2.479861379858951054 ) ) ;
#62473 = VERTEX_POINT ( 'NONE', #50088 ) ;
#62474 = CARTESIAN_POINT ( 'NONE',  ( 98.00000000000000000, 5.000000000000000000, 5.000000000000004441 ) ) ;
#62475 = CARTESIAN_POINT ( 'NONE',  ( 22.00000000000002132, 50.00000000000000000, 59.99999999999999289 ) ) ;
#62476 = CARTESIAN_POINT ( 'NONE',  ( -74.99999999999998579, 50.00000000000000000, 6.500000000000000000 ) ) ;
#62477 = CARTESIAN_POINT ( 'NONE',  ( -65.00499999999998124, 6.826472737025116366, 4.959722759717898555 ) ) ;
#62478 = SURFACE_STYLE_USAGE ( .BOTH. , #57923 ) ;
#62479 = CARTESIAN_POINT ( 'NONE',  ( -168.4429263765337907, -1.166476076187852838E-15, -9.524999999999991473 ) ) ;
#62480 = VECTOR ( 'NONE', #17223, 1000.000000000000000 ) ;
#62481 = CARTESIAN_POINT ( 'NONE',  ( -65.99499999999997613, -6.826472737025113702, 4.959722759717902107 ) ) ;
#62482 = CARTESIAN_POINT ( 'NONE',  ( 3.094860106618435136, 152.4049999999999443, -9.525000000000000355 ) ) ;
#62483 = DIRECTION ( 'NONE',  ( 0.7292845505553197105, -0.6842105263157864936, 0.000000000000000000 ) ) ;
#62484 = ADVANCED_FACE ( 'NONE', ( #23674 ), #66597, .F. ) ;
#62485 = CARTESIAN_POINT ( 'NONE',  ( -1.113559396844004956, 154.5000000000000000, -9.459683423334018570 ) ) ;
#62486 = SHAPE_REPRESENTATION_RELATIONSHIP ( 'NONE' , 'NONE' ,  #12274, #5971 ) ;
#62487 = CARTESIAN_POINT ( 'NONE',  ( -52.50000000000000000, -2.024042244987997205E-14, -11.50000000000000000 ) ) ;
#62488 = CARTESIAN_POINT ( 'NONE',  ( 22.75000000000000711, 37.00000000000000000, -3.750000000000000000 ) ) ;
#62489 = PLANE ( 'NONE',  #69686 ) ;
#62490 = LINE ( 'NONE', #3358, #68647 ) ;
#62491 = ADVANCED_FACE ( 'NONE', ( #19440 ), #34928, .T. ) ;
#62492 = ADVANCED_FACE ( 'NONE', ( #24361 ), #9258, .F. ) ;
#62493 = DIRECTION ( 'NONE',  ( -1.000000000000000000, -0.000000000000000000, -0.000000000000000000 ) ) ;
#62494 = DIRECTION ( 'NONE',  ( -1.000000000000000000, 0.000000000000000000, 0.000000000000000000 ) ) ;
#62495 = VERTEX_POINT ( 'NONE', #25412 ) ;
#62496 = EDGE_LOOP ( 'NONE', ( #53625, #9769, #6026, #47162 ) ) ;
#62497 =( LENGTH_UNIT ( ) NAMED_UNIT ( * ) SI_UNIT ( .MILLI., .METRE. ) );
#62498 = ADVANCED_FACE ( 'NONE', ( #40936 ), #41626, .F. ) ;
#62499 = EDGE_CURVE ( 'NONE', #33108, #69671, #50646, .T. ) ;
#62500 =( NAMED_UNIT ( * ) SI_UNIT ( $, .STERADIAN. ) SOLID_ANGLE_UNIT ( ) );
#62501 = DIRECTION ( 'NONE',  ( -0.000000000000000000, -0.000000000000000000, 1.000000000000000000 ) ) ;
#62502 = CARTESIAN_POINT ( 'NONE',  ( -83.99999999999997158, 50.00000000000000000, -10.49999999999999822 ) ) ;
#62503 = ORIENTED_EDGE ( 'NONE', *, *, #36149, .F. ) ;
#62504 = ORIENTED_EDGE ( 'NONE', *, *, #42143, .F. ) ;
#62505 = EDGE_CURVE ( 'NONE', #60539, #17255, #2025, .T. ) ;
#62506 = CARTESIAN_POINT ( 'NONE',  ( 7.750000000000000000, 33.99999999999998579, -3.750000000000000000 ) ) ;
#62507 = ORIENTED_EDGE ( 'NONE', *, *, #29598, .T. ) ;
#62508 = CARTESIAN_POINT ( 'NONE',  ( -65.09292637653379643, 3.094860106618433360, 9.524999999999991473 ) ) ;
#62509 = DIRECTION ( 'NONE',  ( 0.000000000000000000, -1.000000000000000000, 3.469446951953611033E-15 ) ) ;
#62510 = AXIS2_PLACEMENT_3D ( 'NONE', #32577, #21334, #27636 ) ;
#62511 = ORIENTED_EDGE ( 'NONE', *, *, #7167, .F. ) ;
#62512 =( GEOMETRIC_REPRESENTATION_CONTEXT ( 3 ) GLOBAL_UNCERTAINTY_ASSIGNED_CONTEXT ( ( #69339 ) ) GLOBAL_UNIT_ASSIGNED_CONTEXT ( ( #27121, #1024, #59491 ) ) REPRESENTATION_CONTEXT ( 'NONE', 'WORKASPACE' ) );
#62513 = CARTESIAN_POINT ( 'NONE',  ( -74.50000000000000000, 9.708372675170615196, -6.000000000000000000 ) ) ;
#62514 = CARTESIAN_POINT ( 'NONE',  ( -111.2949999999999733, -2.607480562269069768, 8.024999999999991473 ) ) ;
#62515 = EDGE_LOOP ( 'NONE', ( #7102, #6404, #58323, #31580, #34365, #33444, #24010, #41881, #66777, #63647, #42587, #38022, #14893 ) ) ;
#62516 = CARTESIAN_POINT ( 'NONE',  ( 0.000000000000000000, 43.00000000000000000, 0.000000000000000000 ) ) ;
#62517 = CARTESIAN_POINT ( 'NONE',  ( -178.5570736234661808, -1.166476076187852838E-15, -9.524999999999991473 ) ) ;
#62518 = VERTEX_POINT ( 'NONE', #6675 ) ;
#62519 = CARTESIAN_POINT ( 'NONE',  ( -2.607480562269073765, 147.0929263765337964, -8.025000000000000355 ) ) ;
#62520 = CARTESIAN_POINT ( 'NONE',  ( -53.91508968758270726, -9.466447511857611019, -3.170070218111717075 ) ) ;
#62521 = CARTESIAN_POINT ( 'NONE',  ( 40.99999999999997868, 9.999999999999978684, 3.500000000000000000 ) ) ;
#62522 = LINE ( 'NONE', #62859, #62123 ) ;
#62523 = CIRCLE ( 'NONE', #34414, 3.499999999999999556 ) ;
#62524 = ORIENTED_EDGE ( 'NONE', *, *, #29563, .F. ) ;
#62525 = FACE_OUTER_BOUND ( 'NONE', #35756, .T. ) ;
#62526 = ORIENTED_EDGE ( 'NONE', *, *, #8726, .T. ) ;
#62527 = FACE_OUTER_BOUND ( 'NONE', #28143, .T. ) ;
#62528 = DIRECTION ( 'NONE',  ( 0.000000000000000000, 0.000000000000000000, 1.000000000000000000 ) ) ;
#62529 = DIRECTION ( 'NONE',  ( -0.000000000000000000, -0.000000000000000000, -1.000000000000000000 ) ) ;
#62530 = CARTESIAN_POINT ( 'NONE',  ( 41.11302593432304775, 107.5810679765800444, -3.326249178529582906 ) ) ;
#62531 = CARTESIAN_POINT ( 'NONE',  ( -120.8049999999999784, -8.437984349512085203, 5.166775262442717831E-16 ) ) ;
#62532 = CARTESIAN_POINT ( 'NONE',  ( -183.9999999999999432, -6.383969465318038772, 4.878217756231068236 ) ) ;
#62533 = DIRECTION ( 'NONE',  ( -0.000000000000000000, -0.000000000000000000, -1.000000000000000000 ) ) ;
#62534 =( NAMED_UNIT ( * ) PLANE_ANGLE_UNIT ( ) SI_UNIT ( $, .RADIAN. ) );
#62535 = CIRCLE ( 'NONE', #41246, 4.999999999999997335 ) ;
#62536 = CARTESIAN_POINT ( 'NONE',  ( -195.0000000000000000, 0.000000000000000000, 9.524999999999991473 ) ) ;
#62537 = CARTESIAN_POINT ( 'NONE',  ( 0.000000000000000000, 2.299999999999999822, 0.000000000000000000 ) ) ;
#62538 = ORIENTED_EDGE ( 'NONE', *, *, #46532, .T. ) ;
#62539 = ORIENTED_EDGE ( 'NONE', *, *, #2671, .T. ) ;
#62540 =( LENGTH_UNIT ( ) NAMED_UNIT ( * ) SI_UNIT ( .MILLI., .METRE. ) );
#62541 = SPHERICAL_SURFACE ( 'NONE', #6463, 0.2500000000000000000 ) ;
#62542 = EDGE_LOOP ( 'NONE', ( #53267, #45243, #69327, #34426 ) ) ;
#62543 = CARTESIAN_POINT ( 'NONE',  ( 1.000000000000000000, 42.00000000000000000, -80.00402776293826435 ) ) ;
#62544 = CARTESIAN_POINT ( 'NONE',  ( -183.5049999999999955, -6.826472737025115478, -4.959722759717899443 ) ) ;
#62545 = SURFACE_STYLE_FILL_AREA ( #46791 ) ;
#62546 = CARTESIAN_POINT ( 'NONE',  ( -54.50707362346614104, 8.102448949553176405, 5.886773742842740909 ) ) ;
#62547 = CARTESIAN_POINT ( 'NONE',  ( -179.3950000000000102, -6.826472737025113702, -4.959722759717900331 ) ) ;
#62548 = SURFACE_SIDE_STYLE ('',( #64563 ) ) ;
#62549 = ORIENTED_EDGE ( 'NONE', *, *, #46004, .F. ) ;
#62550 = DIRECTION ( 'NONE',  ( 0.000000000000000000, 1.000000000000000000, 0.000000000000000000 ) ) ;
#62551 = CARTESIAN_POINT ( 'NONE',  ( 7.632228543268608334, 117.4570736234661581, -2.479861379858951942 ) ) ;
#62552 = CARTESIAN_POINT ( 'NONE',  ( -93.35499999999998977, -4.716976649647093289, -6.492361379858945902 ) ) ;
#62553 = CARTESIAN_POINT ( 'NONE',  ( 9.061790287476755523, 154.4999999999999432, 2.966495600661384735 ) ) ;
#62554 = CARTESIAN_POINT ( 'NONE',  ( 0.000000000000000000, 114.9999999999999574, 0.000000000000000000 ) ) ;
#62555 = DIRECTION ( 'NONE',  ( 0.000000000000000000, 0.000000000000000000, -1.000000000000000000 ) ) ;
#62556 = COLOUR_RGB ( '', 0.09019608, 0.27058824, 0.51372549) ;
#62557 = CARTESIAN_POINT ( 'NONE',  ( -93.14499999999999602, -4.716976649647092401, 6.492361379858946790 ) ) ;
#62558 = CARTESIAN_POINT ( 'NONE',  ( 5.598654528085809545, 125.2549999999999812, -7.705886871421373741 ) ) ;
#62559 = CIRCLE ( 'NONE', #13099, 1.000000000000002442 ) ;
#62560 = CARTESIAN_POINT ( 'NONE',  ( -73.04499999999998749, 7.632228543268600340, 2.479861379858949277 ) ) ;
#62561 = DIRECTION ( 'NONE',  ( 0.000000000000000000, 0.000000000000000000, -1.000000000000000000 ) ) ;
#62562 = EDGE_CURVE ( 'NONE', #61621, #57494, #17941, .T. ) ;
#62563 =( GEOMETRIC_REPRESENTATION_CONTEXT ( 3 ) GLOBAL_UNCERTAINTY_ASSIGNED_CONTEXT ( ( #36320 ) ) GLOBAL_UNIT_ASSIGNED_CONTEXT ( ( #14261, #35725, #61389 ) ) REPRESENTATION_CONTEXT ( 'NONE', 'WORKASPACE' ) );
#62564 = CARTESIAN_POINT ( 'NONE',  ( 0.000000000000000000, 149.9999999999999716, 0.000000000000000000 ) ) ;
#62565 = FILL_AREA_STYLE ('',( #29874 ) ) ;
#62566 = EDGE_CURVE ( 'NONE', #54956, #44431, #62938, .T. ) ;
#62567 =( LENGTH_UNIT ( ) NAMED_UNIT ( * ) SI_UNIT ( .MILLI., .METRE. ) );
#62568 = ORIENTED_EDGE ( 'NONE', *, *, #6195, .F. ) ;
#62569 = CARTESIAN_POINT ( 'NONE',  ( -113.9929263765338021, 8.102448949553171076, -5.886773742842744461 ) ) ;
#62570 = CARTESIAN_POINT ( 'NONE',  ( -128.2450000000000045, -4.716976649647093289, -6.492361379858945902 ) ) ;
#62571 = CARTESIAN_POINT ( 'NONE',  ( -4.716976649647097730, 145.3570736234661638, -6.492361379858953896 ) ) ;
#62572 = EDGE_CURVE ( 'NONE', #14650, #19502, #43154, .T. ) ;
#62573 = VECTOR ( 'NONE', #52095, 1000.000000000000000 ) ;
#62574 =( NAMED_UNIT ( * ) PLANE_ANGLE_UNIT ( ) SI_UNIT ( $, .RADIAN. ) );
#62575 = ADVANCED_FACE ( 'NONE', ( #60480 ), #12650, .T. ) ;
#62577 = FILL_AREA_STYLE_COLOUR ( '', #52853 ) ;
#62576 = CARTESIAN_POINT ( 'NONE',  ( -9.827790563157511022E-16, 134.5570736234661808, 8.025000000000000355 ) ) ;
#62578 = SURFACE_STYLE_FILL_AREA ( #3449 ) ;
#62579 = ORIENTED_EDGE ( 'NONE', *, *, #20766, .T. ) ;
#62580 = VERTEX_POINT ( 'NONE', #18643 ) ;
#62581 = CARTESIAN_POINT ( 'NONE',  ( -45.00000000000000000, -2.024042244987997205E-14, -7.000000000000000888 ) ) ;
#62582 = EDGE_CURVE ( 'NONE', #34747, #61571, #2386, .T. ) ;
#62583 = DIRECTION ( 'NONE',  ( 0.000000000000000000, 0.000000000000000000, -1.000000000000000000 ) ) ;
#62584 = CARTESIAN_POINT ( 'NONE',  ( -74.99999999999998579, 50.00000000000000000, -6.999999999999988454 ) ) ;
#62585 = CARTESIAN_POINT ( 'NONE',  ( 12.50000000000000355, 30.99999999999998579, 4.000000000000000000 ) ) ;
#62586 = VERTEX_POINT ( 'NONE', #40123 ) ;
#62587 = CARTESIAN_POINT ( 'NONE',  ( -127.1049999999999898, -6.826472737025113702, 4.959722759717902107 ) ) ;
#62588 = ORIENTED_EDGE ( 'NONE', *, *, #31275, .T. ) ;
#62589 = FACE_OUTER_BOUND ( 'NONE', #19170, .T. ) ;
#62590 = CARTESIAN_POINT ( 'NONE',  ( -126.0570736234661808, 0.000000000000000000, 9.524999999999991473 ) ) ;
#62591 = ORIENTED_EDGE ( 'NONE', *, *, #40896, .F. ) ;
#62592 = CARTESIAN_POINT ( 'NONE',  ( -172.0429263765338135, -9.058813317711329915, -2.943386871421370898 ) ) ;
#62593 = SURFACE_SIDE_STYLE ('',( #41192 ) ) ;
#62594 = ORIENTED_EDGE ( 'NONE', *, *, #40538, .T. ) ;
#62595 = CARTESIAN_POINT ( 'NONE',  ( 18.25000000000000711, 31.24999999999999289, 3.750000000000000000 ) ) ;
#62596 = CARTESIAN_POINT ( 'NONE',  ( -1.166476076187854022E-15, 140.9449999999999932, 9.525000000000000355 ) ) ;
#62597 = DIRECTION ( 'NONE',  ( 0.000000000000000000, 1.000000000000000000, 0.000000000000000000 ) ) ;
#62598 = ORIENTED_EDGE ( 'NONE', *, *, #16704, .F. ) ;
#62599 = LINE ( 'NONE', #52438, #24000 ) ;
#62600 = CARTESIAN_POINT ( 'NONE',  ( -5.598654528085808657, 153.7549999999999670, 7.705886871421373741 ) ) ;
#62601 = SURFACE_STYLE_USAGE ( .BOTH. , #40496 ) ;
#62602 = PRESENTATION_STYLE_ASSIGNMENT (( #67550 ) ) ;
#62603 = EDGE_LOOP ( 'NONE', ( #17819, #3468, #41107, #28544, #65964 ) ) ;
#62604 = CARTESIAN_POINT ( 'NONE',  ( 6.826472737025121695, 119.4929263765338163, -4.959722759717905660 ) ) ;
#62605 = STYLED_ITEM ( 'NONE', ( #31900 ), #58619 ) ;
#62606 = AXIS2_PLACEMENT_3D ( 'NONE', #68892, #42524, #63925 ) ;
#62607 = CARTESIAN_POINT ( 'NONE',  ( 10.00000000000002132, 50.00000000000000000, 60.00000000000000000 ) ) ;
#62608 = AXIS2_PLACEMENT_3D ( 'NONE', #27391, #27728, #49230 ) ;
#62609 = ORIENTED_EDGE ( 'NONE', *, *, #48485, .F. ) ;
#62610 = CARTESIAN_POINT ( 'NONE',  ( 0.000000000000000000, -9.000000000000007105, 0.000000000000000000 ) ) ;
#62611 = ORIENTED_EDGE ( 'NONE', *, *, #55827, .F. ) ;
#62612 = CARTESIAN_POINT ( 'NONE',  ( -56.54292637653379927, 9.058813317711329915, 2.943386871421369566 ) ) ;
#62613 = CARTESIAN_POINT ( 'NONE',  ( 48.25000000000000000, 21.74999999999998579, -3.750000000000000000 ) ) ;
#62614 = CARTESIAN_POINT ( 'NONE',  ( -148.8549999999999898, 4.716976649647094177, 6.492361379858945902 ) ) ;
#62615 = ORIENTED_EDGE ( 'NONE', *, *, #14902, .F. ) ;
#62616 = SURFACE_STYLE_FILL_AREA ( #8496 ) ;
#62617 =( BOUNDED_CURVE ( )  B_SPLINE_CURVE ( 2, ( #5738, #26164, #26831, #63801, #64510, #42068, #25820, #16356, #69439, #31433, #37830 ),
 .UNSPECIFIED., .F., .F. ) 
 B_SPLINE_CURVE_WITH_KNOTS ( ( 3, 2, 2, 2, 2, 3 ),
 ( 0.7826086956521739468, 0.7847826086956521952, 0.7869565217391304435, 0.7891304347826086918, 0.7913043478260869401, 0.7934782608695651884 ),
 .UNSPECIFIED. ) 
 CURVE ( )  GEOMETRIC_REPRESENTATION_ITEM ( )  RATIONAL_B_SPLINE_CURVE ( ( 1.000000000000000000, 0.9510565162951535312, 1.000000000000000000, 0.9510565162951535312, 1.000000000000000000, 0.9510565162951535312, 1.000000000000000000, 0.9510565162951535312, 1.000000000000000000, 0.9510565162951535312, 1.000000000000000000 ) ) 
 REPRESENTATION_ITEM ( '' )  );
#62618 = ADVANCED_FACE ( 'NONE', ( #11968 ), #1709, .F. ) ;
#62619 = CARTESIAN_POINT ( 'NONE',  ( 0.000000000000000000, 151.0570736234661524, -8.025000000000000355 ) ) ;
#62620 = DIRECTION ( 'NONE',  ( -0.000000000000000000, 0.000000000000000000, -1.000000000000000000 ) ) ;
#62621 = DIRECTION ( 'NONE',  ( 1.000000000000000000, 0.000000000000000000, 0.000000000000000000 ) ) ;
#62622 = ORIENTED_EDGE ( 'NONE', *, *, #1057, .T. ) ;
#62623 = CARTESIAN_POINT ( 'NONE',  ( 0.000000000000000000, 87.30187232391182306, 0.000000000000000000 ) ) ;
#62624 = ORIENTED_EDGE ( 'NONE', *, *, #64472, .F. ) ;
#62625 = CARTESIAN_POINT ( 'NONE',  ( -17.75000000000000711, 30.99999999999999289, -3.750000000000000000 ) ) ;
#62626 = AXIS2_PLACEMENT_3D ( 'NONE', #24285, #67553, #9528 ) ;
#62627 = CARTESIAN_POINT ( 'NONE',  ( -66.65499999999998693, -7.632228543268600340, -2.479861379858950166 ) ) ;
#62628 = ORIENTED_EDGE ( 'NONE', *, *, #5524, .F. ) ;
#62629 = FACE_OUTER_BOUND ( 'NONE', #29391, .T. ) ;
#62630 = CARTESIAN_POINT ( 'NONE',  ( 39.24999999999999289, 15.99999999999997691, 3.750000000000000000 ) ) ;
#62631 = DIRECTION ( 'NONE',  ( 0.000000000000000000, 0.000000000000000000, 1.000000000000000000 ) ) ;
#62632 = VERTEX_POINT ( 'NONE', #40456 ) ;
#62633 = CARTESIAN_POINT ( 'NONE',  ( -75.00000000000000000, 8.442834901059200092, -5.542315673751891936 ) ) ;
#62634 = CARTESIAN_POINT ( 'NONE',  ( 71.99999999999998579, 119.9999999999997868, 7.000000000000000000 ) ) ;
#62635 = FACE_OUTER_BOUND ( 'NONE', #61603, .T. ) ;
#62636 = CARTESIAN_POINT ( 'NONE',  ( -20.71231517720798010, 149.9999999999999716, 10.00000000000000000 ) ) ;
#62637 = EDGE_CURVE ( 'NONE', #29016, #36102, #33425, .T. ) ;
#62638 = EDGE_CURVE ( 'NONE', #43970, #55156, #22885, .T. ) ;
#62639 = CARTESIAN_POINT ( 'NONE',  ( -5.598654528085808657, 146.6450000000000102, 7.705886871421373741 ) ) ;
#62640 = CARTESIAN_POINT ( 'NONE',  ( -98.24499999999999034, -4.716976649647093289, -6.492361379858945902 ) ) ;
#62641 = DIRECTION ( 'NONE',  ( -1.000000000000000000, 1.445602896647339656E-16, 0.000000000000000000 ) ) ;
#62642 = EDGE_CURVE ( 'NONE', #13573, #57372, #36889, .T. ) ;
#62643 = CARTESIAN_POINT ( 'NONE',  ( 32.00000000000000711, 43.00000000000000000, -75.00000000000001421 ) ) ;
#62644 = ORIENTED_EDGE ( 'NONE', *, *, #35437, .F. ) ;
#62645 = CARTESIAN_POINT ( 'NONE',  ( -142.3429263765338249, -9.058813317711329915, 2.943386871421371787 ) ) ;
#62646 = CARTESIAN_POINT ( 'NONE',  ( -159.7450000000000045, 4.716976649647094177, 6.492361379858945902 ) ) ;
#62647 =( GEOMETRIC_REPRESENTATION_CONTEXT ( 3 ) GLOBAL_UNCERTAINTY_ASSIGNED_CONTEXT ( ( #8855 ) ) GLOBAL_UNIT_ASSIGNED_CONTEXT ( ( #29747, #62083, #5411 ) ) REPRESENTATION_CONTEXT ( 'NONE', 'WORKASPACE' ) );
#62648 = VECTOR ( 'NONE', #62799, 1000.000000000000000 ) ;
#62649 = FILL_AREA_STYLE_COLOUR ( '', #8992 ) ;
#62650 = ADVANCED_FACE ( 'NONE', ( #4835 ), #15089, .F. ) ;
#62651 = DIRECTION ( 'NONE',  ( 0.000000000000000000, 0.000000000000000000, -1.000000000000000000 ) ) ;
#62652 = CARTESIAN_POINT ( 'NONE',  ( 0.000000000000000000, 154.9999999999999716, 0.000000000000000000 ) ) ;
#62653 = ORIENTED_EDGE ( 'NONE', *, *, #34773, .F. ) ;
#62654 = VECTOR ( 'NONE', #28651, 1000.000000000000000 ) ;
#62655 = CARTESIAN_POINT ( 'NONE',  ( 0.000000000000000000, 128.9429263765338192, -8.025000000000000355 ) ) ;
#62656 = ORIENTED_EDGE ( 'NONE', *, *, #10976, .F. ) ;
#62657 = CARTESIAN_POINT ( 'NONE',  ( 4.250000000000001776, 22.24999999999998579, 3.750000000000000000 ) ) ;
#62658 = ADVANCED_FACE ( 'NONE', ( #42875 ), #10129, .T. ) ;
#62659 = FACE_OUTER_BOUND ( 'NONE', #25063, .T. ) ;
#62660 = CARTESIAN_POINT ( 'NONE',  ( -195.0000000000000000, 0.000000000000000000, 0.000000000000000000 ) ) ;
#62661 = LINE ( 'NONE', #3182, #50562 ) ;
#62662 = VECTOR ( 'NONE', #28895, 1000.000000000000000 ) ;
#62663 =( NAMED_UNIT ( * ) PLANE_ANGLE_UNIT ( ) SI_UNIT ( $, .RADIAN. ) );
#62664 = CIRCLE ( 'NONE', #11010, 0.5000000000000004441 ) ;
#62665 = EDGE_LOOP ( 'NONE', ( #65632, #44729, #50440, #32248 ) ) ;
#62666 = CARTESIAN_POINT ( 'NONE',  ( -157.4050000000000011, -2.607480562269069768, 8.024999999999991473 ) ) ;
#62667 = ORIENTED_EDGE ( 'NONE', *, *, #41079, .T. ) ;
#62668 = DIRECTION ( 'NONE',  ( 0.000000000000000000, 0.000000000000000000, 1.000000000000000000 ) ) ;
#62669 = DIRECTION ( 'NONE',  ( 0.5000000000000003331, 0.000000000000000000, 0.8660254037844383745 ) ) ;
#62670 = ORIENTED_EDGE ( 'NONE', *, *, #25693, .T. ) ;
#62671 = CARTESIAN_POINT ( 'NONE',  ( 3.046771365092978190, 72.00000000000001421, -6.349999999999997868 ) ) ;
#62672 = CARTESIAN_POINT ( 'NONE',  ( -48.05707362346617373, 0.000000000000000000, 9.524999999999991473 ) ) ;
#62673 = CARTESIAN_POINT ( 'NONE',  ( -3.094860106618432471, 109.5949999999999847, -9.525000000000000355 ) ) ;
#62674 = ORIENTED_EDGE ( 'NONE', *, *, #26564, .F. ) ;
#62675 = CARTESIAN_POINT ( 'NONE',  ( -5.710692600061829438, 4.108790270285304302, 3.163668057994810583E-15 ) ) ;
#62676 = CARTESIAN_POINT ( 'NONE',  ( -5.598654528085806881, 119.8549999999999898, -7.705886871421374629 ) ) ;
#62677 = CARTESIAN_POINT ( 'NONE',  ( -73.70499999999998408, 2.607480562269072433, 8.024999999999991473 ) ) ;
#62678 = CARTESIAN_POINT ( 'NONE',  ( -80.15707362346617515, -9.058813317711329915, -2.943386871421370898 ) ) ;
#62679 = VERTEX_POINT ( 'NONE', #21710 ) ;
#62680 = CARTESIAN_POINT ( 'NONE',  ( 9.058813317711338797, 133.9549999999999841, -2.943386871421372675 ) ) ;
#62681 = CYLINDRICAL_SURFACE ( 'NONE', #47936, 9.524999999999991473 ) ;
#62682 = CARTESIAN_POINT ( 'NONE',  ( 31.00000000000002132, 42.00000000000000000, 79.00402776293823592 ) ) ;
#62683 = FACE_OUTER_BOUND ( 'NONE', #49755, .T. ) ;
#62684 = VERTEX_POINT ( 'NONE', #20322 ) ;
#62685 = CYLINDRICAL_SURFACE ( 'NONE', #51970, 0.5000000000000004441 ) ;
#62686 = CARTESIAN_POINT ( 'NONE',  ( 34.99999999999999289, 146.4999999999999716, -7.000000000000000000 ) ) ;
#62687 = CARTESIAN_POINT ( 'NONE',  ( -184.5550000000000068, 0.000000000000000000, 8.024999999999991473 ) ) ;
#62688 = ORIENTED_EDGE ( 'NONE', *, *, #11192, .F. ) ;
#62689 = CARTESIAN_POINT ( 'NONE',  ( 8.442136150874052447, 111.5033947631521585, -1.192225150237074205 ) ) ;
#62690 = EDGE_CURVE ( 'NONE', #67222, #20172, #12810, .T. ) ;
#62691 = CARTESIAN_POINT ( 'NONE',  ( 48.50000000000000000, 22.24999999999998579, -3.750000000000000000 ) ) ;
#62692 = CARTESIAN_POINT ( 'NONE',  ( 22.99999999999999645, 0.000000000000000000, -72.00402776293825013 ) ) ;
#62693 = VERTEX_POINT ( 'NONE', #26618 ) ;
#62694 = DIRECTION ( 'NONE',  ( -0.000000000000000000, -1.000000000000000000, -0.000000000000000000 ) ) ;
#62695 = DIRECTION ( 'NONE',  ( 1.000000000000000000, 0.000000000000000000, 0.000000000000000000 ) ) ;
#62696 = ORIENTED_EDGE ( 'NONE', *, *, #54325, .F. ) ;
#62697 = MECHANICAL_DESIGN_GEOMETRIC_PRESENTATION_REPRESENTATION (  '', ( #54861 ), #55984 ) ;
#62698 = VECTOR ( 'NONE', #61661, 1000.000000000000000 ) ;
#62699 =( NAMED_UNIT ( * ) SI_UNIT ( $, .STERADIAN. ) SOLID_ANGLE_UNIT ( ) );
#62700 = DIRECTION ( 'NONE',  ( -1.000000000000000000, 0.000000000000000000, 0.000000000000000000 ) ) ;
#62701 = CARTESIAN_POINT ( 'NONE',  ( -94.85499999999998977, 4.716976649647094177, 6.492361379858945902 ) ) ;
#62702 = EDGE_LOOP ( 'NONE', ( #50308, #55500, #18363, #49226 ) ) ;
#62703 = DIRECTION ( 'NONE',  ( 0.000000000000000000, 0.000000000000000000, 1.000000000000000000 ) ) ;
#62704 = AXIS2_PLACEMENT_3D ( 'NONE', #47686, #42051, #14571 ) ;
#62705 = CARTESIAN_POINT ( 'NONE',  ( -144.5070736234661695, 8.102448949553176405, 5.886773742842740909 ) ) ;
#62706 = CARTESIAN_POINT ( 'NONE',  ( -8.102448949553179958, 151.8950000000000102, -5.886773742842749790 ) ) ;
#62707 = CARTESIAN_POINT ( 'NONE',  ( -77.30707362346615241, -10.01517768586948698, 6.132527647946031529E-16 ) ) ;
#62708 = PRESENTATION_LAYER_ASSIGNMENT (  '', '', ( #53727 ) ) ;
#62709 = EDGE_CURVE ( 'NONE', #56663, #9275, #21021, .T. ) ;
#62711 = EDGE_CURVE ( 'NONE', #6425, #21392, #64267, .T. ) ;
#62710 =( LENGTH_UNIT ( ) NAMED_UNIT ( * ) SI_UNIT ( .MILLI., .METRE. ) );
#62712 = ORIENTED_EDGE ( 'NONE', *, *, #20176, .T. ) ;
#62713 = PLANE ( 'NONE',  #60820 ) ;
#62714 = CARTESIAN_POINT ( 'NONE',  ( -4.500000000000002665, 22.24999999999998579, -4.000000000000000000 ) ) ;
#62715 =( GEOMETRIC_REPRESENTATION_CONTEXT ( 3 ) GLOBAL_UNCERTAINTY_ASSIGNED_CONTEXT ( ( #52989 ) ) GLOBAL_UNIT_ASSIGNED_CONTEXT ( ( #64024, #21463, #56228 ) ) REPRESENTATION_CONTEXT ( 'NONE', 'WORKASPACE' ) );
#62716 = FILL_AREA_STYLE_COLOUR ( '', #11143 ) ;
#62717 = EDGE_CURVE ( 'NONE', #57711, #47180, #61109, .T. ) ;
#62718 = CARTESIAN_POINT ( 'NONE',  ( -122.3050000000000068, 8.437984349512085203, -1.550032578732815448E-15 ) ) ;
#62719 = EDGE_CURVE ( 'NONE', #37912, #4579, #45406, .T. ) ;
#62720 = CARTESIAN_POINT ( 'NONE',  ( 24.29733203266260944, 24.87668888026472658, -27.31792417249472749 ) ) ;
#62721 = CARTESIAN_POINT ( 'NONE',  ( 9.058813317711338797, 111.8449999999999847, -2.943386871421372675 ) ) ;
#62722 = CARTESIAN_POINT ( 'NONE',  ( -125.6950000000000074, -8.437984349512085203, 5.166775262442717831E-16 ) ) ;
#62723 = LINE ( 'NONE', #31069, #25783 ) ;
#62724 = EDGE_LOOP ( 'NONE', ( #14268, #41224, #2814, #30929 ) ) ;
#62725 =( NAMED_UNIT ( * ) PLANE_ANGLE_UNIT ( ) SI_UNIT ( $, .RADIAN. ) );
#62726 = ADVANCED_FACE ( 'NONE', ( #58648 ), #4464, .F. ) ;
#62727 = ORIENTED_EDGE ( 'NONE', *, *, #18189, .T. ) ;
#62728 = CARTESIAN_POINT ( 'NONE',  ( -195.0000000000000000, 0.000000000000000000, 0.000000000000000000 ) ) ;
#62729 = AXIS2_PLACEMENT_3D ( 'NONE', #42624, #37005, #31316 ) ;
#62730 = CARTESIAN_POINT ( 'NONE',  ( -168.5929263765337680, -3.094860106618431139, -9.524999999999991473 ) ) ;
#62731 =( NAMED_UNIT ( * ) SI_UNIT ( $, .STERADIAN. ) SOLID_ANGLE_UNIT ( ) );
#62732 = CARTESIAN_POINT ( 'NONE',  ( -182.8449999999999989, -7.632228543268599452, 2.479861379858951054 ) ) ;
#62733 = ADVANCED_FACE ( 'NONE', ( #52367 ), #47461, .T. ) ;
#62734 = VECTOR ( 'NONE', #45477, 1000.000000000000000 ) ;
#62735 = CARTESIAN_POINT ( 'NONE',  ( -7.632228543268608334, 124.9570736234661581, 2.479861379858952830 ) ) ;
#62736 = VECTOR ( 'NONE', #10149, 1000.000000000000000 ) ;
#62737 = PRESENTATION_LAYER_ASSIGNMENT (  '', '', ( #15630 ) ) ;
#62738 = CARTESIAN_POINT ( 'NONE',  ( 15.00000000000000000, 8.000000000000000000, 3.500000000000003997 ) ) ;
#62739 = DIRECTION ( 'NONE',  ( -0.000000000000000000, -1.000000000000000000, 0.000000000000000000 ) ) ;
#62740 = VERTEX_POINT ( 'NONE', #9794 ) ;
#62741 = CARTESIAN_POINT ( 'NONE',  ( -84.59292637653379643, -3.094860106618431139, -9.524999999999991473 ) ) ;
#62742 = CIRCLE ( 'NONE', #13278, 10.00000000000000000 ) ;
#62743 = DIRECTION ( 'NONE',  ( -0.000000000000000000, -1.000000000000000000, -0.000000000000000000 ) ) ;
#62744 = LINE ( 'NONE', #9674, #78 ) ;
#62745 = CARTESIAN_POINT ( 'NONE',  ( -195.0000000000000000, 0.000000000000000000, 9.524999999999991473 ) ) ;
#62746 = CARTESIAN_POINT ( 'NONE',  ( 60.99999999999998579, 50.00000000000000000, -9.500000000000000000 ) ) ;
#62747 = VECTOR ( 'NONE', #33831, 1000.000000000000000 ) ;
#62748 = DIRECTION ( 'NONE',  ( -0.000000000000000000, -0.000000000000000000, 1.000000000000000000 ) ) ;
#62749 = ORIENTED_EDGE ( 'NONE', *, *, #16706, .F. ) ;
#62750 = CARTESIAN_POINT ( 'NONE',  ( 4.358330484967979146, 6.451150163859158404, 0.7660251680141578756 ) ) ;
#62751 = FILL_AREA_STYLE_COLOUR ( '', #21708 ) ;
#62752 = VERTEX_POINT ( 'NONE', #42192 ) ;
#62753 = CARTESIAN_POINT ( 'NONE',  ( -111.1429263765338078, 5.598654528085800663, -7.705886871421367523 ) ) ;
#62754 = EDGE_CURVE ( 'NONE', #17724, #42390, #15429, .T. ) ;
#62755 = DIRECTION ( 'NONE',  ( 0.000000000000000000, 0.000000000000000000, -1.000000000000000000 ) ) ;
#62756 = CARTESIAN_POINT ( 'NONE',  ( 7.632228543268607446, 132.1570736234661467, 2.479861379858954606 ) ) ;
#62757 = CARTESIAN_POINT ( 'NONE',  ( -17.75000000000000355, -4.000000000000000000, 0.000000000000000000 ) ) ;
#62758 = ORIENTED_EDGE ( 'NONE', *, *, #14563, .F. ) ;
#62759 = CARTESIAN_POINT ( 'NONE',  ( 36.00000000000002842, 5.000000000000000000, 29.00402776293825724 ) ) ;
#62760 = CARTESIAN_POINT ( 'NONE',  ( -101.1550000000000011, 7.632228543268600340, 2.479861379858949277 ) ) ;
#62761 =( GEOMETRIC_REPRESENTATION_CONTEXT ( 3 ) GLOBAL_UNCERTAINTY_ASSIGNED_CONTEXT ( ( #66375 ) ) GLOBAL_UNIT_ASSIGNED_CONTEXT ( ( #52714, #19282, #51664 ) ) REPRESENTATION_CONTEXT ( 'NONE', 'WORKASPACE' ) );
#62762 = DIRECTION ( 'NONE',  ( 0.000000000000000000, 1.000000000000000000, 0.000000000000000000 ) ) ;
#62763 = VERTEX_POINT ( 'NONE', #60373 ) ;
#62764 = DIRECTION ( 'NONE',  ( 0.000000000000000000, 0.000000000000000000, -1.000000000000000000 ) ) ;
#62765 =( NAMED_UNIT ( * ) SI_UNIT ( $, .STERADIAN. ) SOLID_ANGLE_UNIT ( ) );
#62766 = CARTESIAN_POINT ( 'NONE',  ( -37.50000000000000000, 83.99999999999998579, -6.349999999999999645 ) ) ;
#62767 = CARTESIAN_POINT ( 'NONE',  ( 27.99999999999999289, 34.36176364315826248, -80.00402776293826435 ) ) ;
#62768 = ORIENTED_EDGE ( 'NONE', *, *, #9237, .T. ) ;
#62769 = CARTESIAN_POINT ( 'NONE',  ( 6.413663052920311358, 2.891209729714700138, -4.192813088908785199E-16 ) ) ;
#62770 = CARTESIAN_POINT ( 'NONE',  ( -76.19499999999999318, 8.437984349512085203, -1.550032578732815448E-15 ) ) ;
#62771 = ORIENTED_EDGE ( 'NONE', *, *, #19725, .T. ) ;
#62772 = DIRECTION ( 'NONE',  ( 0.000000000000000000, -1.000000000000000000, 0.000000000000000000 ) ) ;
#62773 = DIRECTION ( 'NONE',  ( -1.000000000000000000, 0.000000000000000000, 0.000000000000000000 ) ) ;
#62774 = DIRECTION ( 'NONE',  ( -0.000000000000000000, -0.000000000000000000, -1.000000000000000000 ) ) ;
#62775 = STYLED_ITEM ( 'NONE', ( #37622 ), #43661 ) ;
#62776 = UNCERTAINTY_MEASURE_WITH_UNIT (LENGTH_MEASURE( 1.000000000000000082E-05 ), #936, 'distance_accuracy_value', 'NONE');
#62777 = VERTEX_POINT ( 'NONE', #5861 ) ;
#62778 = CARTESIAN_POINT ( 'NONE',  ( 68.50000000000000000, 1.797044900979284448E-15, -10.49999999999999822 ) ) ;
#62779 = DIRECTION ( 'NONE',  ( 0.000000000000000000, 1.000000000000000000, -0.000000000000000000 ) ) ;
#62780 = CIRCLE ( 'NONE', #32448, 13.49999999999999822 ) ;
#62781 = DIRECTION ( 'NONE',  ( -0.000000000000000000, 1.000000000000000000, -0.000000000000000000 ) ) ;
#62782 = CARTESIAN_POINT ( 'NONE',  ( 9.000000000000003553, 27.74999999999998934, 4.000000000000000000 ) ) ;
#62783 = ORIENTED_EDGE ( 'NONE', *, *, #16151, .T. ) ;
#62784 = SURFACE_STYLE_USAGE ( .BOTH. , #19880 ) ;
#62785 = ORIENTED_EDGE ( 'NONE', *, *, #62095, .F. ) ;
#62786 = MECHANICAL_DESIGN_GEOMETRIC_PRESENTATION_REPRESENTATION (  '', ( #14494 ), #51555 ) ;
#62787 = DIRECTION ( 'NONE',  ( -0.000000000000000000, -0.000000000000000000, 1.000000000000000000 ) ) ;
#62788 = FACE_OUTER_BOUND ( 'NONE', #34506, .T. ) ;
#62789 = AXIS2_PLACEMENT_3D ( 'NONE', #39364, #49209, #27013 ) ;
#62790 = CARTESIAN_POINT ( 'NONE',  ( -166.2570736234661695, 5.598654528085800663, -7.705886871421367523 ) ) ;
#62791 = CARTESIAN_POINT ( 'NONE',  ( 9.058813317711337021, 126.5449999999999875, 2.943386871421375783 ) ) ;
#62792 =( GEOMETRIC_REPRESENTATION_CONTEXT ( 3 ) GLOBAL_UNCERTAINTY_ASSIGNED_CONTEXT ( ( #16637 ) ) GLOBAL_UNIT_ASSIGNED_CONTEXT ( ( #42793, #58225, #10047 ) ) REPRESENTATION_CONTEXT ( 'NONE', 'WORKASPACE' ) );
#62793 = CARTESIAN_POINT ( 'NONE',  ( -103.1070736234661638, 8.102448949553171076, -5.886773742842744461 ) ) ;
#62794 = EDGE_CURVE ( 'NONE', #58002, #35530, #23110, .T. ) ;
#62795 = DIRECTION ( 'NONE',  ( -1.000000000000000000, 0.000000000000000000, 0.000000000000000000 ) ) ;
#62796 = EDGE_LOOP ( 'NONE', ( #21237, #20008, #62568, #56815 ) ) ;
#62797 = LINE ( 'NONE', #63842, #1405 ) ;
#62798 = CARTESIAN_POINT ( 'NONE',  ( -82.19292637653380496, -10.01517768586948698, 6.132527647946031529E-16 ) ) ;
#62800 = CARTESIAN_POINT ( 'NONE',  ( -60.89292637653380069, -8.102448949553174629, -5.886773742842741797 ) ) ;
#62799 = DIRECTION ( 'NONE',  ( 0.000000000000000000, -1.000000000000000000, -0.000000000000000000 ) ) ;
#62801 = DIRECTION ( 'NONE',  ( -0.000000000000000000, -1.000000000000000000, 0.000000000000000000 ) ) ;
#62802 = EDGE_CURVE ( 'NONE', #55787, #45031, #34161, .T. ) ;
#62803 = CARTESIAN_POINT ( 'NONE',  ( -146.0050000000000239, 6.826472737025116366, 4.959722759717898555 ) ) ;
#62804 = SURFACE_STYLE_FILL_AREA ( #40704 ) ;
#62805 = CARTESIAN_POINT ( 'NONE',  ( -1.994734356760242244, 110.7119700403975884, -9.105933873098768672 ) ) ;
#62806 = CARTESIAN_POINT ( 'NONE',  ( -159.2949999999999875, -2.607480562269069768, 8.024999999999991473 ) ) ;
#62807 = CARTESIAN_POINT ( 'NONE',  ( -149.3949999999999818, -6.826472737025113702, -4.959722759717900331 ) ) ;
#62808 = ORIENTED_EDGE ( 'NONE', *, *, #37727, .F. ) ;
#62809 = DIRECTION ( 'NONE',  ( 1.000000000000000000, 0.000000000000000000, 0.000000000000000000 ) ) ;
#62810 = DIRECTION ( 'NONE',  ( -0.000000000000000000, 1.000000000000000000, 0.000000000000000000 ) ) ;
#62811 = UNCERTAINTY_MEASURE_WITH_UNIT (LENGTH_MEASURE( 1.000000000000000082E-05 ), #51900, 'distance_accuracy_value', 'NONE');
#62812 = CARTESIAN_POINT ( 'NONE',  ( -59.90499999999997982, 2.607480562269068880, -8.024999999999993250 ) ) ;
#62813 = FACE_OUTER_BOUND ( 'NONE', #47229, .T. ) ;
#62815 = LINE ( 'NONE', #11351, #26888 ) ;
#62814 =( GEOMETRIC_REPRESENTATION_CONTEXT ( 3 ) GLOBAL_UNCERTAINTY_ASSIGNED_CONTEXT ( ( #25536 ) ) GLOBAL_UNIT_ASSIGNED_CONTEXT ( ( #21640, #53987, #48420 ) ) REPRESENTATION_CONTEXT ( 'NONE', 'WORKASPACE' ) );
#62816 = ADVANCED_FACE ( 'NONE', ( #60711, #49498 ), #22402, .T. ) ;
#62817 = CARTESIAN_POINT ( 'NONE',  ( -59.99499999999996902, -6.826472737025113702, 4.959722759717902107 ) ) ;
#62818 = CARTESIAN_POINT ( 'NONE',  ( -8.102448949553181734, 159.6050000000000182, 5.886773742842747126 ) ) ;
#62819 = CARTESIAN_POINT ( 'NONE',  ( -60.00000000000000000, -2.024042244987997205E-14, -12.00000000000000000 ) ) ;
#62820 = CARTESIAN_POINT ( 'NONE',  ( -45.00000000000000000, -1.469576158976824302E-14, 10.00000000000000000 ) ) ;
#62821 = MECHANICAL_DESIGN_GEOMETRIC_PRESENTATION_REPRESENTATION (  '', ( #31391 ), #58366 ) ;
#62822 = UNCERTAINTY_MEASURE_WITH_UNIT (LENGTH_MEASURE( 1.000000000000000082E-05 ), #12110, 'distance_accuracy_value', 'NONE');
#62823 = DIRECTION ( 'NONE',  ( -4.021988422452565194E-16, 2.220446049250313081E-16, 1.000000000000000000 ) ) ;
#62824 = DIRECTION ( 'NONE',  ( -1.000000000000000000, -0.000000000000000000, -0.000000000000000000 ) ) ;
#62825 = AXIS2_PLACEMENT_3D ( 'NONE', #41320, #30357, #51861 ) ;
#62826 = CARTESIAN_POINT ( 'NONE',  ( -1.447422522083364749, 110.7948483342343593, 9.145303841767344011 ) ) ;
#62827 =( LENGTH_UNIT ( ) NAMED_UNIT ( * ) SI_UNIT ( .MILLI., .METRE. ) );
#62828 = MECHANICAL_DESIGN_GEOMETRIC_PRESENTATION_REPRESENTATION (  '', ( #31401 ), #44909 ) ;
#62829 = CARTESIAN_POINT ( 'NONE',  ( -48.00000000000000000, 14.49137674618942562, -7.000000000000000000 ) ) ;
#62830 = EDGE_CURVE ( 'NONE', #61802, #61535, #46564, .T. ) ;
#62831 = LINE ( 'NONE', #13017, #59103 ) ;
#62832 = CARTESIAN_POINT ( 'NONE',  ( -195.0000000000000000, 0.000000000000000000, 9.524999999999991473 ) ) ;
#62833 = LINE ( 'NONE', #35440, #45250 ) ;
#62834 = ORIENTED_EDGE ( 'NONE', *, *, #44604, .F. ) ;
#62835 = ORIENTED_EDGE ( 'NONE', *, *, #18590, .F. ) ;
#62836 = EDGE_CURVE ( 'NONE', #54396, #6517, #38631, .T. ) ;
#62837 = AXIS2_PLACEMENT_3D ( 'NONE', #37121, #43774, #6095 ) ;
#62838 = AXIS2_PLACEMENT_3D ( 'NONE', #14585, #13891, #56812 ) ;
#62840 = CARTESIAN_POINT ( 'NONE',  ( -21.02379601146600763, 114.6388938931947763, 10.00000000000000000 ) ) ;
#62839 = AXIS2_PLACEMENT_3D ( 'NONE', #1131, #33560, #65568 ) ;
#62841 = CARTESIAN_POINT ( 'NONE',  ( -45.50000000000000000, -1.469576158976824302E-14, 6.999999999999999112 ) ) ;
#62842 = MECHANICAL_DESIGN_GEOMETRIC_PRESENTATION_REPRESENTATION (  '', ( #61729 ), #21271 ) ;
#62843 = PRESENTATION_STYLE_ASSIGNMENT (( #30838 ) ) ;
#62844 = ORIENTED_EDGE ( 'NONE', *, *, #64414, .F. ) ;
#62845 = VERTEX_POINT ( 'NONE', #28342 ) ;
#62846 = CARTESIAN_POINT ( 'NONE',  ( -108.8070736234661666, 10.01517768586948698, -1.839758294383808966E-15 ) ) ;
#62847 = CARTESIAN_POINT ( 'NONE',  ( -75.50000000000000000, 35.50862325381056905, -41.30495168499704306 ) ) ;
#62848 = ORIENTED_EDGE ( 'NONE', *, *, #51484, .F. ) ;
#62849 = CARTESIAN_POINT ( 'NONE',  ( -3.094860106618434248, 123.9049999999999727, 9.525000000000000355 ) ) ;
#62850 = CARTESIAN_POINT ( 'NONE',  ( 4.383776131304275125, 1.496531397472843361, -9.000000000000007105 ) ) ;
#62851 = ORIENTED_EDGE ( 'NONE', *, *, #51566, .T. ) ;
#62852 = DIRECTION ( 'NONE',  ( 0.000000000000000000, 1.000000000000000000, -0.000000000000000000 ) ) ;
#62853 = CARTESIAN_POINT ( 'NONE',  ( -108.5949999999999847, 2.607480562269073321, 8.024999999999991473 ) ) ;
#62854 = EDGE_LOOP ( 'NONE', ( #3450, #58278, #32044, #53218 ) ) ;
#62855 = DIRECTION ( 'NONE',  ( 0.000000000000000000, 1.000000000000000000, -0.000000000000000000 ) ) ;
#62856 =( NAMED_UNIT ( * ) PLANE_ANGLE_UNIT ( ) SI_UNIT ( $, .RADIAN. ) );
#62857 = VERTEX_POINT ( 'NONE', #858 ) ;
#62858 = CARTESIAN_POINT ( 'NONE',  ( -4.716976649647097730, 156.2429263765338021, -6.492361379858953896 ) ) ;
#62859 = CARTESIAN_POINT ( 'NONE',  ( 8.319377385370872346, -3.000000000000000888, -2.000000000000000000 ) ) ;
#62860 = CARTESIAN_POINT ( 'NONE',  ( 10.00000000000001954, 50.00000000000000000, 60.00000000000000000 ) ) ;
#62861 = ORIENTED_EDGE ( 'NONE', *, *, #30307, .F. ) ;
#62862 = EDGE_CURVE ( 'NONE', #43499, #42596, #64954, .T. ) ;
#62863 = CARTESIAN_POINT ( 'NONE',  ( -71.62068965517238439, 63.58603185604027885, 7.000000000000000000 ) ) ;
#62864 = EDGE_LOOP ( 'NONE', ( #21854, #12226 ) ) ;
#62865 = SURFACE_SIDE_STYLE ('',( #47094 ) ) ;
#62866 =( NAMED_UNIT ( * ) PLANE_ANGLE_UNIT ( ) SI_UNIT ( $, .RADIAN. ) );
#62867 = DIRECTION ( 'NONE',  ( 0.000000000000000000, 0.000000000000000000, 1.000000000000000000 ) ) ;
#62868 = CARTESIAN_POINT ( 'NONE',  ( -122.6049999999999898, 6.826472737025113702, -4.959722759717902107 ) ) ;
#62869 = CYLINDRICAL_SURFACE ( 'NONE', #9523, 0.5000000000000004441 ) ;
#62870 = MECHANICAL_DESIGN_GEOMETRIC_PRESENTATION_REPRESENTATION (  '', ( #16869 ), #32542 ) ;
#62871 = DIRECTION ( 'NONE',  ( -0.000000000000000000, 1.000000000000000000, -0.000000000000000000 ) ) ;
#62872 = CARTESIAN_POINT ( 'NONE',  ( 71.50000000000000000, 36.32520566882265456, -7.500000000000000000 ) ) ;
#62873 = MECHANICAL_DESIGN_GEOMETRIC_PRESENTATION_REPRESENTATION (  '', ( #44957 ), #7906 ) ;
#62874 = DIRECTION ( 'NONE',  ( -0.9486832980505138790, -0.3162277660168378857, 0.000000000000000000 ) ) ;
#62875 = CARTESIAN_POINT ( 'NONE',  ( 10.00000000000000178, 43.00000000000000000, -90.00000000000000000 ) ) ;
#62876 = DIRECTION ( 'NONE',  ( 0.000000000000000000, 0.000000000000000000, -1.000000000000000000 ) ) ;
#62877 = ORIENTED_EDGE ( 'NONE', *, *, #61139, .T. ) ;
#62878 = VERTEX_POINT ( 'NONE', #49161 ) ;
#62879 = FACE_OUTER_BOUND ( 'NONE', #25991, .T. ) ;
#62880 =( NAMED_UNIT ( * ) SI_UNIT ( $, .STERADIAN. ) SOLID_ANGLE_UNIT ( ) );
#62881 = DIRECTION ( 'NONE',  ( -0.000000000000000000, -0.000000000000000000, -1.000000000000000000 ) ) ;
#62882 = DIRECTION ( 'NONE',  ( -4.336808689941999001E-16, 1.000000000000000000, 0.000000000000000000 ) ) ;
#62883 = ORIENTED_EDGE ( 'NONE', *, *, #44446, .T. ) ;
#62884 = ADVANCED_FACE ( 'NONE', ( #33315 ), #11498, .F. ) ;
#62885 = CARTESIAN_POINT ( 'NONE',  ( -174.9550000000000125, -7.632228543268599452, 2.479861379858951054 ) ) ;
#62886 = CARTESIAN_POINT ( 'NONE',  ( -195.0000000000000000, 1.166476076187852838E-15, -9.524999999999991473 ) ) ;
#62887 = DIRECTION ( 'NONE',  ( 0.000000000000000000, 0.9944852160011111719, -0.1048768571002353378 ) ) ;
#62888 =( GEOMETRIC_REPRESENTATION_CONTEXT ( 3 ) GLOBAL_UNCERTAINTY_ASSIGNED_CONTEXT ( ( #25830 ) ) GLOBAL_UNIT_ASSIGNED_CONTEXT ( ( #3612, #41675, #41322 ) ) REPRESENTATION_CONTEXT ( 'NONE', 'WORKASPACE' ) );
#62889 = CARTESIAN_POINT ( 'NONE',  ( -48.35707362346617089, 5.598654528085804216, 7.705886871421366635 ) ) ;
#62890 = VECTOR ( 'NONE', #6689, 1000.000000000000000 ) ;
#62891 = EDGE_CURVE ( 'NONE', #51540, #22849, #18453, .T. ) ;
#62892 = CARTESIAN_POINT ( 'NONE',  ( -175.6449999999999818, 4.716976649647091513, -6.492361379858946790 ) ) ;
#62893 = FILL_AREA_STYLE_COLOUR ( '', #27505 ) ;
#62894 = ORIENTED_EDGE ( 'NONE', *, *, #45228, .F. ) ;
#62895 = DIRECTION ( 'NONE',  ( 1.000000000000000000, 0.000000000000000000, 0.000000000000000000 ) ) ;
#62896 = FILL_AREA_STYLE_COLOUR ( '', #16772 ) ;
#62897 = CARTESIAN_POINT ( 'NONE',  ( -13.69084439013661303, 10.98233027600763023, 4.836677785638663352 ) ) ;
#62898 = CARTESIAN_POINT ( 'NONE',  ( -91.40500000000000114, -2.607480562269069768, 8.024999999999991473 ) ) ;
#62899 = SURFACE_STYLE_USAGE ( .BOTH. , #14042 ) ;
#62900 = SURFACE_SIDE_STYLE ('',( #3074 ) ) ;
#62901 = CIRCLE ( 'NONE', #16900, 26.49999999999999645 ) ;
#62902 = EDGE_CURVE ( 'NONE', #66069, #61310, #57772, .T. ) ;
#62903 = CARTESIAN_POINT ( 'NONE',  ( -89.99499999999999034, -6.826472737025113702, 4.959722759717902107 ) ) ;
#62904 = CARTESIAN_POINT ( 'NONE',  ( -9.058813317711338797, 123.4549999999999841, 2.943386871421373563 ) ) ;
#62905 = CARTESIAN_POINT ( 'NONE',  ( -68.69500000000000739, -8.437984349512085203, 5.166775262442717831E-16 ) ) ;
#62906 = DIRECTION ( 'NONE',  ( -1.000000000000000000, 0.000000000000000000, 0.000000000000000000 ) ) ;
#62907 = AXIS2_PLACEMENT_3D ( 'NONE', #35526, #41868, #46457 ) ;
#62908 = PRESENTATION_STYLE_ASSIGNMENT (( #4148 ) ) ;
#62909 = UNCERTAINTY_MEASURE_WITH_UNIT (LENGTH_MEASURE( 1.000000000000000082E-05 ), #53041, 'distance_accuracy_value', 'NONE');
#62910 = PLANE ( 'NONE',  #23646 ) ;
#62911 = CARTESIAN_POINT ( 'NONE',  ( 24.21231517720798010, 113.4999999999999858, 7.500000000000000000 ) ) ;
#62912 = VERTEX_POINT ( 'NONE', #54404 ) ;
#62913 = CARTESIAN_POINT ( 'NONE',  ( -103.4929263765337879, -8.102448949553172852, 5.886773742842742685 ) ) ;
#62914 = CARTESIAN_POINT ( 'NONE',  ( -132.5949999999999989, 2.607480562269073321, 8.024999999999991473 ) ) ;
#62915 = VECTOR ( 'NONE', #26307, 1000.000000000000000 ) ;
#62916 = CARTESIAN_POINT ( 'NONE',  ( 27.00000000000001776, 15.00000000000000000, 29.68999999999999417 ) ) ;
#62918 = DIRECTION ( 'NONE',  ( 0.000000000000000000, 1.000000000000000000, 0.000000000000000000 ) ) ;
#62917 = CARTESIAN_POINT ( 'NONE',  ( 7.632228543268608334, 135.4570736234661581, -2.479861379858951942 ) ) ;
#62919 = ORIENTED_EDGE ( 'NONE', *, *, #53728, .F. ) ;
#62920 = EDGE_LOOP ( 'NONE', ( #39020, #6043, #26418, #31710 ) ) ;
#62921 = CARTESIAN_POINT ( 'NONE',  ( -45.89999098806710975, 9.371467124235310919, -6.143012557965069398 ) ) ;
#62922 = AXIS2_PLACEMENT_3D ( 'NONE', #42231, #16509, #54090 ) ;
#62923 =( BOUNDED_SURFACE ( )  B_SPLINE_SURFACE ( 3, 2, ( 
 ( #22237, #33154, #38806 ),
 ( #59507, #55278, #49681 ),
 ( #65136, #6057, #60895 ),
 ( #33482, #54911, #6739 ),
 ( #27140, #44777, #11329 ),
 ( #27494, #54587, #66175 ),
 ( #48673, #1418, #44442 ),
 ( #43733, #6393, #39149 ) ),
 .UNSPECIFIED., .F., .F., .F. ) 
 B_SPLINE_SURFACE_WITH_KNOTS ( ( 4, 2, 2, 4 ),
 ( 3, 3 ),
 ( 4.336808689942017736E-19, 0.0003058805084468733276, 0.0004588207626703098016, 0.0006117610168937462215 ),
 ( 0.000000000000000000, 1.000000000000000000 ),
 .UNSPECIFIED. ) 
 GEOMETRIC_REPRESENTATION_ITEM ( )  RATIONAL_B_SPLINE_SURFACE ( (
 ( 1.000000000000000000, 0.3766558475679906981, 1.000000000000000000),
 ( 1.000000000000000000, 0.3767717614668182335, 1.000000000000000000),
 ( 1.000000000000000000, 0.3678485930275403604, 1.000000000000000000),
 ( 1.000000000000000000, 0.3444746654570013944, 1.000000000000000000),
 ( 1.000000000000000000, 0.3350482327563981677, 1.000000000000000000),
 ( 1.000000000000000000, 0.3140847209475624568, 1.000000000000000000),
 ( 1.000000000000000000, 0.3025536022197361508, 1.000000000000000000),
 ( 1.000000000000000000, 0.2907356542125085763, 1.000000000000000000) ) ) 
 REPRESENTATION_ITEM ( '' )  SURFACE ( )  );
#62924 = DIRECTION ( 'NONE',  ( 0.000000000000000000, -0.8823529411764736707, -0.4705882352941119229 ) ) ;
#62925 = UNCERTAINTY_MEASURE_WITH_UNIT (LENGTH_MEASURE( 1.000000000000000082E-05 ), #18196, 'distance_accuracy_value', 'NONE');
#62926 = CIRCLE ( 'NONE', #25875, 0.5000000000000004441 ) ;
#62927 = CARTESIAN_POINT ( 'NONE',  ( -4.750000000000002665, 24.74999999999998579, 4.000000000000000000 ) ) ;
#62928 =( LENGTH_UNIT ( ) NAMED_UNIT ( * ) SI_UNIT ( .MILLI., .METRE. ) );
#62929 = DIRECTION ( 'NONE',  ( 5.782411586589351722E-16, -1.000000000000000000, 0.000000000000000000 ) ) ;
#62930 = ORIENTED_EDGE ( 'NONE', *, *, #25804, .F. ) ;
#62931 = CARTESIAN_POINT ( 'NONE',  ( -126.8050000000000068, -8.437984349512086979, 5.166775262442717831E-16 ) ) ;
#62932 = ORIENTED_EDGE ( 'NONE', *, *, #57514, .T. ) ;
#62933 = CARTESIAN_POINT ( 'NONE',  ( -126.5070736234661979, 8.102448949553176405, 5.886773742842740909 ) ) ;
#62934 = VERTEX_POINT ( 'NONE', #27992 ) ;
#62935 = DIRECTION ( 'NONE',  ( 1.000000000000000000, -0.000000000000000000, -1.300977106640434891E-16 ) ) ;
#62936 = CARTESIAN_POINT ( 'NONE',  ( -84.44292637653380496, -1.166476076187852838E-15, -9.524999999999991473 ) ) ;
#62937 = ORIENTED_EDGE ( 'NONE', *, *, #67338, .T. ) ;
#62938 = B_SPLINE_CURVE_WITH_KNOTS ( 'NONE', 3,
 ( #60833, #66475, #44383, #28110, #13003, #55213, #23906, #45060, #29159, #39431 ),
 .UNSPECIFIED., .F., .F.,
 ( 4, 2, 2, 2, 4 ),
 ( 0.000000000000000000, 0.0004706383985570294502, 0.0009412767971140589005, 0.001411915195671088405, 0.001882553594228117801 ),
 .UNSPECIFIED. ) ;
#62939 = CIRCLE ( 'NONE', #48384, 4.999999999999990230 ) ;
#62940 = DIRECTION ( 'NONE',  ( -1.000000000000000000, -0.000000000000000000, -0.000000000000000000 ) ) ;
#62941 = AXIS2_PLACEMENT_3D ( 'NONE', #234, #43283, #55844 ) ;
#62942 = CARTESIAN_POINT ( 'NONE',  ( -5.598654528085806881, 151.7450000000000045, -7.705886871421374629 ) ) ;
#62943 = DIRECTION ( 'NONE',  ( 0.000000000000000000, 0.000000000000000000, -1.000000000000000000 ) ) ;
#62944 = ORIENTED_EDGE ( 'NONE', *, *, #15448, .T. ) ;
#62945 = CARTESIAN_POINT ( 'NONE',  ( 60.00000000000000000, 1.797044900979284448E-15, -11.50000000000001066 ) ) ;
#62946 = CARTESIAN_POINT ( 'NONE',  ( -9.058813317711338797, 147.4550000000000125, 2.943386871421373563 ) ) ;
#62947 = FACE_OUTER_BOUND ( 'NONE', #53091, .T. ) ;
#62948 =( GEOMETRIC_REPRESENTATION_CONTEXT ( 3 ) GLOBAL_UNCERTAINTY_ASSIGNED_CONTEXT ( ( #62271 ) ) GLOBAL_UNIT_ASSIGNED_CONTEXT ( ( #38594, #31864, #32549 ) ) REPRESENTATION_CONTEXT ( 'NONE', 'WORKASPACE' ) );
#62949 = VERTEX_POINT ( 'NONE', #44256 ) ;
#62950 = CARTESIAN_POINT ( 'NONE',  ( -4.716976649647097730, 114.2429263765338163, -6.492361379858953896 ) ) ;
#62951 = DIRECTION ( 'NONE',  ( 0.000000000000000000, 0.7071067811865474617, 0.7071067811865474617 ) ) ;
#62952 = UNCERTAINTY_MEASURE_WITH_UNIT (LENGTH_MEASURE( 1.000000000000000082E-05 ), #31119, 'distance_accuracy_value', 'NONE');
#62953 = CARTESIAN_POINT ( 'NONE',  ( 16.75000000000000711, 27.74999999999998224, 3.750000000000000000 ) ) ;
#62954 = CARTESIAN_POINT ( 'NONE',  ( -98.99292637653378790, 8.102448949553172852, -5.886773742842744461 ) ) ;
#62955 = DIRECTION ( 'NONE',  ( 0.000000000000000000, 0.000000000000000000, 1.000000000000000000 ) ) ;
#62956 = ORIENTED_EDGE ( 'NONE', *, *, #33137, .T. ) ;
#62957 = AXIS2_PLACEMENT_3D ( 'NONE', #64358, #38012, #27727 ) ;
#62958 = EDGE_CURVE ( 'NONE', #62777, #60435, #50190, .T. ) ;
#62959 = CARTESIAN_POINT ( 'NONE',  ( 40.99999999999998579, 107.7459666924148252, 3.000000000000000000 ) ) ;
#62960 = ORIENTED_EDGE ( 'NONE', *, *, #53231, .F. ) ;
#62961 = CARTESIAN_POINT ( 'NONE',  ( -62.39292637653379359, 8.102448949553176405, 5.886773742842740909 ) ) ;
#62962 = SURFACE_SIDE_STYLE ('',( #9183 ) ) ;
#62963 = CARTESIAN_POINT ( 'NONE',  ( -153.2049999999999272, -2.607480562269071545, -8.024999999999991473 ) ) ;
#62964 = VERTEX_POINT ( 'NONE', #6225 ) ;
#62965 = CARTESIAN_POINT ( 'NONE',  ( 0.000000000000000000, 0.000000000000000000, 0.000000000000000000 ) ) ;
#62966 = UNCERTAINTY_MEASURE_WITH_UNIT (LENGTH_MEASURE( 1.000000000000000082E-05 ), #48576, 'distance_accuracy_value', 'NONE');
#62967 = AXIS2_PLACEMENT_3D ( 'NONE', #39338, #64986, #17538 ) ;
#62968 = EDGE_CURVE ( 'NONE', #62495, #7517, #67058, .T. ) ;
#62969 = AXIS2_PLACEMENT_3D ( 'NONE', #19579, #31157, #62823 ) ;
#62970 = EDGE_CURVE ( 'NONE', #33122, #2387, #26260, .T. ) ;
#62971 = DIRECTION ( 'NONE',  ( 0.000000000000000000, -1.000000000000000000, 0.000000000000000000 ) ) ;
#62972 = DIRECTION ( 'NONE',  ( 0.000000000000000000, 0.000000000000000000, -1.000000000000000000 ) ) ;
#62973 = PLANE ( 'NONE',  #26899 ) ;
#62974 =( NAMED_UNIT ( * ) PLANE_ANGLE_UNIT ( ) SI_UNIT ( $, .RADIAN. ) );
#62975 = ORIENTED_EDGE ( 'NONE', *, *, #42630, .F. ) ;
#62976 = MECHANICAL_DESIGN_GEOMETRIC_PRESENTATION_REPRESENTATION (  '', ( #32635 ), #19172 ) ;
#62977 = ORIENTED_EDGE ( 'NONE', *, *, #56829, .T. ) ;
#62978 = CARTESIAN_POINT ( 'NONE',  ( 22.41794263251858155, 25.31045447836329743, 27.43560882268856815 ) ) ;
#62979 = SURFACE_SIDE_STYLE ('',( #40881 ) ) ;
#62980 = CARTESIAN_POINT ( 'NONE',  ( -69.80499999999996419, -8.437984349512085203, 5.166775262442717831E-16 ) ) ;
#62981 = EDGE_LOOP ( 'NONE', ( #62783, #35497, #33562, #5067 ) ) ;
#62982 = FACE_OUTER_BOUND ( 'NONE', #69242, .T. ) ;
#62983 = EDGE_CURVE ( 'NONE', #42335, #63323, #40330, .T. ) ;
#62984 =( NAMED_UNIT ( * ) PLANE_ANGLE_UNIT ( ) SI_UNIT ( $, .RADIAN. ) );
#62985 = EDGE_CURVE ( 'NONE', #66402, #10860, #28499, .T. ) ;
#62986 = PRESENTATION_LAYER_ASSIGNMENT (  '', '', ( #30420 ) ) ;
#62987 = EDGE_CURVE ( 'NONE', #10808, #28945, #44299, .T. ) ;
#62988 = DIRECTION ( 'NONE',  ( -0.000000000000000000, -0.000000000000000000, -1.000000000000000000 ) ) ;
#62989 = CARTESIAN_POINT ( 'NONE',  ( -17.75000000000000711, 30.74999999999999289, 4.000000000000000000 ) ) ;
#62990 = VERTEX_POINT ( 'NONE', #25099 ) ;
#62991 = AXIS2_PLACEMENT_3D ( 'NONE', #35273, #24350, #34228 ) ;
#62992 = ADVANCED_FACE ( 'NONE', ( #21191 ), #44101, .F. ) ;
#62993 = VECTOR ( 'NONE', #68204, 1000.000000000000000 ) ;
#62994 = CARTESIAN_POINT ( 'NONE',  ( -75.00000000000000000, 9.708372671850062474, -6.049000248777010036 ) ) ;
#62995 = CARTESIAN_POINT ( 'NONE',  ( 22.70255002340108774, 27.12311843165924330, -27.31797491105104569 ) ) ;
#62996 = PLANE ( 'NONE',  #65120 ) ;
#62997 = CARTESIAN_POINT ( 'NONE',  ( 3.094860106618431583, 153.0949999999999989, 9.525000000000000355 ) ) ;
#62998 = CARTESIAN_POINT ( 'NONE',  ( -97.34499999999998465, 7.632228543268599452, -2.479861379858951942 ) ) ;
#62999 = CARTESIAN_POINT ( 'NONE',  ( 8.082903768654762899, -1.105959442090949618E-15, 7.500000000000000000 ) ) ;
#63000 = AXIS2_PLACEMENT_3D ( 'NONE', #20987, #10785, #68846 ) ;
#63001 = UNCERTAINTY_MEASURE_WITH_UNIT (LENGTH_MEASURE( 1.000000000000000082E-05 ), #38503, 'distance_accuracy_value', 'NONE');
#63002 = CIRCLE ( 'NONE', #25935, 0.4999999999999994449 ) ;
#63003 = CARTESIAN_POINT ( 'NONE',  ( 22.75000000000000711, 34.24999999999999289, 3.750000000000000000 ) ) ;
#63004 = ORIENTED_EDGE ( 'NONE', *, *, #69275, .T. ) ;
#63005 = CARTESIAN_POINT ( 'NONE',  ( -132.1429263765338078, 5.598654528085800663, -7.705886871421367523 ) ) ;
#63006 =( NAMED_UNIT ( * ) SI_UNIT ( $, .STERADIAN. ) SOLID_ANGLE_UNIT ( ) );
#63007 = CARTESIAN_POINT ( 'NONE',  ( -34.03832277083918711, -9.867028709848661094, -3.272567082151741857 ) ) ;
#63008 = CARTESIAN_POINT ( 'NONE',  ( -154.4949999999999477, 6.826472737025113702, -4.959722759717902107 ) ) ;
#63010 = DIRECTION ( 'NONE',  ( 0.000000000000000000, 0.000000000000000000, 1.000000000000000000 ) ) ;
#63009 = STYLED_ITEM ( 'NONE', ( #6008 ), #52676 ) ;
#63011 = LINE ( 'NONE', #14850, #25846 ) ;
#63012 = CARTESIAN_POINT ( 'NONE',  ( -81.05707362346618083, 0.000000000000000000, 9.524999999999991473 ) ) ;
#63013 = ORIENTED_EDGE ( 'NONE', *, *, #26056, .F. ) ;
#63014 = SURFACE_STYLE_FILL_AREA ( #43602 ) ;
#63015 = ORIENTED_EDGE ( 'NONE', *, *, #44992, .T. ) ;
#63016 = CIRCLE ( 'NONE', #41717, 7.500000000000007105 ) ;
#63017 = CARTESIAN_POINT ( 'NONE',  ( 6.062177826491067734, -2.500000000000000000, 3.500000000000000000 ) ) ;
#63018 = DIRECTION ( 'NONE',  ( 0.000000000000000000, 0.000000000000000000, -1.000000000000000000 ) ) ;
#63019 = DIRECTION ( 'NONE',  ( -2.312964634635740689E-15, 1.000000000000000000, 0.000000000000000000 ) ) ;
#63020 = DIRECTION ( 'NONE',  ( -0.000000000000000000, 1.000000000000000000, -0.000000000000000000 ) ) ;
#63021 = CARTESIAN_POINT ( 'NONE',  ( -60.70461754965442935, -8.499999999999992895, 1.000000000000000222 ) ) ;
#63022 = ORIENTED_EDGE ( 'NONE', *, *, #60988, .T. ) ;
#63023 = CARTESIAN_POINT ( 'NONE',  ( -153.6549999999999727, -7.632228543268600340, -2.479861379858950166 ) ) ;
#63024 = EDGE_LOOP ( 'NONE', ( #13922, #11678 ) ) ;
#63025 = DIRECTION ( 'NONE',  ( 1.000000000000000000, 0.000000000000000000, 0.000000000000000000 ) ) ;
#63026 = DIRECTION ( 'NONE',  ( 0.000000000000000000, 0.000000000000000000, -1.000000000000000000 ) ) ;
#63027 = ORIENTED_EDGE ( 'NONE', *, *, #54007, .F. ) ;
#63028 = MECHANICAL_DESIGN_GEOMETRIC_PRESENTATION_REPRESENTATION (  '', ( #10280 ), #51860 ) ;
#63029 = DIRECTION ( 'NONE',  ( 0.000000000000000000, 0.000000000000000000, -1.000000000000000000 ) ) ;
#63030 = CARTESIAN_POINT ( 'NONE',  ( 6.062177826491071286, -3.500000000000002220, 0.000000000000000000 ) ) ;
#63031 = CARTESIAN_POINT ( 'NONE',  ( -5.598654528085806881, 121.7449999999999903, -7.705886871421374629 ) ) ;
#63032 =( BOUNDED_CURVE ( )  B_SPLINE_CURVE ( 2, ( #15318, #47330, #42062, #32145, #53598, #16353, #64144, #5384, #16000, #20905, #37483, #32466, #68757, #48364, #69435, #10361, #5733, #53, #37123, #25817, #20548, #58529, #15644, #36777, #58886, #27180, #53931, #10694, #21586, #5060, #11022, #64506, #48716, #48031, #31791, #42411, #37825, #63466, #57857, #43098, #21225, #53273, #69103, #26507, #59198, #58187, #42750, #418, #4712, #21951, #43458, #63797, #64840, #16687, #9679, #31090, #52585, #4334, #26160, #10008, #31428, #52923, #47697, #11726, #50076, #66582, #12751, #44813, #38151, #22986, #50402, #60259, #44483, #55321, #33193, #27865, #17384, #17032, #45161, #65182, #54627, #65887, #49373, #38850, #6439, #22277, #1093, #6783, #38516, #34222, #23318, #39528, #60582, #55676, #17715, #18043, #1804, #66216, #22633, #54281, #33528, #60933, #39185, #7490, #12399, #6098, #28917, #49716, #27536, #2126, #12061, #54957, #7143, #44136, #59553, #28572, #11376, #23657, #28211, #49061, #1455, #33858, #65538, #43778, #32839, #747, #59908, #66939, #67265, #30296, #8190, #46910, #29975, #8545, #57058, #7825, #51800, #18398, #67621, #24344, #35966, #51441, #34558, #3550, #19058, #61982, #8874, #45840, #39886, #25052, #25394, #52164, #3186, #56010, #24678, #29271, #61291, #45520, #40565, #18731, #50752, #46563, #2501, #67986, #24011, #62338, #35621, #14163, #19771, #30659, #40213, #61617, #13444, #34910, #13097, #41267, #13804, #35264, #56355, #62666, #56727, #9236, #46202, #29639, #19422, #51108, #2853, #40919, #14489, #57411, #3921, #20099, #53852, #15566, #5649, #9930, #15914, #58450, #53189, #4977, #42333, #41606, #64062, #58119, #63023, #57771, #14865, #47958, #10274, #63716, #36702, #27100, #53523, #9597, #31347, #52848, #10948, #37038, #31709, #32385, #36346, #26426, #32064, #4625, #47251, #5306, #26080, #47613, #42658, #69360, #69017, #31014, #68322, #21151, #52508, #37394, #20826, #58799, #68671, #4251, #10614, #26754, #48273, #69692, #21501, #43017, #63381, #25730, #64422, #16271, #37745, #59126, #20469, #41973, #15234, #44404, #60176, #1001, #66132, #60499, #27788, #65088, #65806, #49291, #6358, #27450, #28128, #17964, #23244, #49635, #22909, #65458, #1730, #55233, #44739, #38766, #22547, #33109, #7057, #59463, #48633, #33445, #54876, #44049, #59829, #17307, #28486, #48979, #11985, #49994, #16943, #17641, #39452, #54546, #6697, #1375, #39108, #60855, #12311, #33781, #38432, #12669, #34135, #64767, #55592, #22201, #7418, #331, #21865, #43376, #16607, #38069, #11294, #32748, #54200, #6015, #43699, #11642, #673, #7741, #35872, #29180, #2047, #13718, #40141, #29547, #2409, #13024, #23923, #67183, #50666, #3462, #14075, #30218, #51358, #46469, #8463, #8791, #62249, #40832, #45437, #18972, #67532, #18318, #35538, #28842, #29899, #34819, #67896, #51016, #57318, #56636, #19332, #41185, #51711, #66857, #18661, #61534, #23572, #34481, #50327, #45086, #40478, #39800, #66499, #55935, #56274, #13360, #61214, #8100, #3101, #24595, #56977, #2777, #24267, #35175, #45765, #61897, #46111, #24959, #19687, #62587, #14402, #62931, #36948, #68583, #16180, #57679, #58038, #21072, #20379, #37656, #20741, #68935, #47879, #68238, #42572, #9154, #58356, #15146, #26670, #30571, #10182, #69277, #21411, #31970, #25643, #9508, #47163, #52072, #14776, #3826, #36255, #42929, #63973, #31622, #4169, #69602, #15821, #53443, #41880, #53102, #4890, #37303, #15482, #26338, #58711, #63298, #10532, #5225, #20020, #48196, #42252, #31258, #64327, #25311, #9845, #46832, #41518, #30928, #36620, #52424, #52757, #4532, #25992, #47520, #63640, #6272, #12225, #65713, #55138, #49205, #11548, #43610, #17553, #239, #59051, #33360, #909, #49549, #10868, #38335, #39019, #59370, #22459, #60417, #5917, #6599, #49902, #65003, #17219, #38683, #43956, #1645, #59739, #1279, #27360, #27008, #22115, #33695, #591, #32651, #22815, #17876, #6968, #28391, #32310, #65372, #23160, #33019, #60086, #28041, #54108, #48893, #54458, #37990, #66045, #16525, #11207, #48544, #43287, #5561, #44651, #21772, #54788, #44313, #53766, #64685, #16861, #27704, #11899, #35368, #55501, #39360, #9332, #14249, #67720, #56822, #36064, #41014, #19514, #25146, #13901, #62433, #3291, #66398, #60759, #30062, #46997, #35713, #12576, #25829, #57143, #47342, #51528, #57507, #30393, #46660, #68079, #8975, #24780, #30755, #46297, #34045, #28754, #7328, #19862, #51897, #3651, #8632, #68770, #25483, #50239, #41354, #62760, #52599, #14597, #52258, #4346, #1960, #4015, #68409, #20204, #18217, #41706, #63127, #14968, #36450, #57870, #9692, #23482, #44988, #31101, #39700, #62070, #5069, #26521, #69114, #63481, #5397, #31801, #32155, #43111, #430, #53282, #15653, #32852, #4724, #48375, #10375, #27546, #20921, #69445, #32480, #48043, #49070, #53610, #10705, #59208, #10023, #53941, #38164, #21598, #36788, #11386, #26836, #58199, #5745, #21235, #64157, #11032, #42763, #42078, #27189, #20563, #54293, #65, #31443, #64518, #52935, #15329, #6113, #21962, #37133, #37837, #26174, #16013, #16362, #48730, #43467, #47711, #37493, #64851, #58542, #42419, #58898, #16697, #59567, #63807, #34235, #38860, #45174, #7498, #29285, #55333, #13115, #22999, #7158, #18056, #65550, #60272, #49730, #49382, #7837, #27877, #17396, #61303, #28586, #28927, #12409, #23328, #12071, #39196, #1105, #66593, #55690, #2139, #44826, #18412, #50085, #50414, #23670, #12764, #33536, #17047, #65897, #60591, #39896, #1813, #34567, #66230, #56020, #1472, #755, #39541, #60945, #22289, #43790, #54968, #22644, #6795, #65196, #54641, #38527, #6448, #59920, #11736, #33204, #28221, #44150, #44494, #17727, #33869, #66949, #57425, #18745, #25066, #68000, #46575, #30671, #63038, #13456, #24356, #45851, #40226, #50766, #19786, #24695, #8555, #67282, #41279, #56741, #41621, #35634, #19071, #29988, #13818, #8207, #2515, #40577, #9254, #51452, #24024, #36364, #67634, #57784, #61991, #62677, #40933, #57070, #8885, #45531, #61631, #14504, #35280, #34924, #56371, #68332, #35980, #3202, #29653, #51120, #3564, #46214, #14881, #30311, #19435, #62354, #14176, #2867, #51814, #3935, #52178, #46923, #25407, #20113, #9609, #37761, #41990, #31026, #5322, #21163, #21515, #52520, #4265, #26764, #20843, #25745, #20483, #47263, #10628, #21880, #37050, #58813, #32078, #42675, #43390, #10288, #43033, #69033, #68683, #63728, #59138, #42343, #37410, #64437, #15575, #9940, #10963, #58465, #31721, #64781, #53205, #53536, #48291, #26094, #4990, #26443, #31363, #38084, #58130, #47626, #16619, #33794, #32400, #64077, #16285, #53866, #47974, #69373, #59482, #5665, #27113, #48647, #346, #63400, #15246, #36714, #52861, #15930, #4639, #6713, #49650, #60870, #39123, #28855, #12325, #27468, #2062, #22922, #48993, #1746, #23589, #34153, #27799, #59847, #49304, #54215, #65106, #11309, #16960, #45100, #50008, #33798, #6370, #66513, #17977, #55611, #1015, #44753, #684, #39466, #17655, #7075, #60511, #44066, #55249, #7434, #22216, #28506, #44421, #33461, #1394, #23256, #43711, #66147, #32765, #12682, #17321, #50338, #12001, #38447, #18335, #60193, #54887, #39815, #38782, #6031, #11656, #33126, #54562, #65822, #22563, #65470, #28141, #13041, #18676, #18987, #40154, #50684, #45452, #7752, #67912, #29195, #35554, #8804, #56992, #41200, #3842, #23937, #34835 ),
 .UNSPECIFIED., .F., .F. ) 
 B_SPLINE_CURVE_WITH_KNOTS ( ( 3, 2, 2, 2, 2, 2, 2, 2, 2, 2, 2, 2, 2, 2, 2, 2, 2, 2, 2, 2, 2, 2, 2, 2, 2, 2, 2, 2, 2, 2, 2, 2, 2, 2, 2, 2, 2, 2, 2, 2, 2, 2, 2, 2, 2, 2, 2, 2, 2, 2, 2, 2, 2, 2, 2, 2, 2, 2, 2, 2, 2, 2, 2, 2, 2, 2, 2, 2, 2, 2, 2, 2, 2, 2, 2, 2, 2, 2, 2, 2, 2, 2, 2, 2, 2, 2, 2, 2, 2, 2, 2, 2, 2, 2, 2, 2, 2, 2, 2, 2, 2, 2, 2, 2, 2, 2, 2, 2, 2, 2, 2, 2, 2, 2, 2, 2, 2, 2, 2, 2, 2, 2, 2, 2, 2, 2, 2, 2, 2, 2, 2, 2, 2, 2, 2, 2, 2, 2, 2, 2, 2, 2, 2, 2, 2, 2, 2, 2, 2, 2, 2, 2, 2, 2, 2, 2, 2, 2, 2, 2, 2, 2, 2, 2, 2, 2, 2, 2, 2, 2, 2, 2, 2, 2, 2, 2, 2, 2, 2, 2, 2, 2, 2, 2, 2, 2, 2, 2, 2, 2, 2, 2, 2, 2, 2, 2, 2, 2, 2, 2, 2, 2, 2, 2, 2, 2, 2, 2, 2, 2, 2, 2, 2, 2, 2, 2, 2, 2, 2, 2, 2, 2, 2, 2, 2, 2, 2, 2, 2, 2, 2, 2, 2, 2, 2, 2, 2, 2, 2, 2, 2, 2, 2, 2, 2, 2, 2, 2, 2, 2, 2, 2, 2, 2, 2, 2, 2, 2, 2, 2, 2, 2, 2, 2, 2, 2, 2, 2, 2, 2, 2, 2, 2, 2, 2, 2, 2, 2, 2, 2, 2, 2, 2, 2, 2, 2, 2, 2, 2, 2, 2, 2, 2, 2, 2, 2, 2, 2, 2, 2, 2, 2, 2, 2, 2, 2, 2, 2, 2, 2, 2, 2, 2, 2, 2, 2, 2, 2, 2, 2, 2, 2, 2, 2, 2, 2, 2, 2, 2, 2, 2, 2, 2, 2, 2, 2, 2, 2, 2, 2, 2, 2, 2, 2, 2, 2, 2, 2, 2, 2, 2, 2, 2, 2, 2, 2, 2, 2, 2, 2, 2, 2, 2, 2, 2, 2, 2, 2, 2, 2, 2, 2, 2, 2, 2, 2, 2, 2, 2, 2, 2, 2, 2, 2, 2, 2, 2, 2, 2, 2, 2, 2, 2, 2, 2, 2, 2, 2, 2, 2, 2, 2, 2, 2, 2, 2, 2, 2, 2, 2, 2, 2, 2, 2, 2, 2, 2, 2, 2, 2, 2, 2, 2, 2, 2, 2, 2, 2, 2, 2, 2, 2, 2, 2, 2, 2, 2, 2, 2, 2, 2, 2, 2, 2, 2, 2, 2, 2, 2, 2, 2, 2, 2, 2, 2, 3 ),
 ( 0.004012011224361215593, 0.004347826086956521792, 0.006521739130434782254, 0.008695652173913043584, 0.01086956521739130405, 0.01304347826086956624, 0.01521739130434782844, 0.01739130434782608717, 0.01956521739130434936, 0.02173913043478260809, 0.02391304347826087029, 0.02608695652173912902, 0.02826086956521739121, 0.03043478260869565341, 0.03260869565217391214, 0.03478260869565217434, 0.03695652173913043653, 0.03913043478260869873, 0.04130434782608695399, 0.04347826086956521618, 0.04565217391304347838, 0.04782608695652174058, 0.05000000000000000278, 0.05217391304347825803, 0.05434782608695652023, 0.05652173913043478243, 0.05869565217391304462, 0.06086956521739130682, 0.06304347826086956208, 0.06521739130434782428, 0.06739130434782608647, 0.06956521739130434867, 0.07173913043478261087, 0.07391304347826087306, 0.07608695652173913526, 0.07826086956521739746, 0.08043478260869564578, 0.08260869565217390798, 0.08478260869565217017, 0.08695652173913043237, 0.08913043478260869457, 0.09130434782608695676, 0.09347826086956521896, 0.09565217391304348116, 0.09782608695652174335, 0.1000000000000000056, 0.1021739130434782677, 0.1043478260869565161, 0.1065217391304347783, 0.1086956521739130405, 0.1108695652173913027, 0.1130434782608695649, 0.1152173913043478271, 0.1173913043478260892, 0.1195652173913043514, 0.1217391304347826136, 0.1239130434782608758, 0.1260869565217391242, 0.1282608695652174002, 0.1304347826086956486, 0.1326086956521739246, 0.1347826086956521729, 0.1369565217391304213, 0.1391304347826086973, 0.1413043478260869457, 0.1434782608695652217, 0.1456521739130434701, 0.1478260869565217461, 0.1499999999999999944, 0.1521739130434782705, 0.1543478260869565188, 0.1565217391304347949, 0.1586956521739130432, 0.1608695652173912916, 0.1630434782608695676, 0.1652173913043478160, 0.1673913043478260920, 0.1695652173913043403, 0.1717391304347826164, 0.1739130434782608647, 0.1760869565217391408, 0.1782608695652173891, 0.1804347826086956652, 0.1826086956521739135, 0.1847826086956521618, 0.1869565217391304379, 0.1891304347826086862, 0.1913043478260869623, 0.1934782608695652106, 0.1956521739130434867, 0.1978260869565217350, 0.2000000000000000111, 0.2021739130434782594, 0.2043478260869565355, 0.2065217391304347838, 0.2086956521739130321, 0.2108695652173913082, 0.2130434782608695565, 0.2152173913043478326, 0.2173913043478260809, 0.2195652173913043570, 0.2217391304347826053, 0.2239130434782608814, 0.2260869565217391297, 0.2282608695652173780, 0.2304347826086956541, 0.2326086956521739024, 0.2347826086956521785, 0.2369565217391304268, 0.2391304347826087029, 0.2413043478260869512, 0.2434782608695652273, 0.2456521739130434756, 0.2478260869565217517, 0.2500000000000000000, 0.2521739130434782483, 0.2543478260869564966, 0.2565217391304348005, 0.2586956521739130488, 0.2608695652173912971, 0.2630434782608695454, 0.2652173913043478493, 0.2673913043478260976, 0.2695652173913043459, 0.2717391304347825942, 0.2739130434782608425, 0.2760869565217391464, 0.2782608695652173947, 0.2804347826086956430, 0.2826086956521738913, 0.2847826086956521952, 0.2869565217391304435, 0.2891304347826086918, 0.2913043478260869401, 0.2934782608695652439, 0.2956521739130434923, 0.2978260869565217406, 0.2999999999999999889, 0.3021739130434782372, 0.3043478260869565410, 0.3065217391304347894, 0.3086956521739130377, 0.3108695652173912860, 0.3130434782608695898, 0.3152173913043478382, 0.3173913043478260865, 0.3195652173913043348, 0.3217391304347825831, 0.3239130434782608869, 0.3260869565217391353, 0.3282608695652173836, 0.3304347826086956319, 0.3326086956521739357, 0.3347826086956521840, 0.3369565217391304324, 0.3391304347826086807, 0.3413043478260869290, 0.3434782608695652328, 0.3456521739130434812, 0.3478260869565217295, 0.3499999999999999778, 0.3521739130434782816, 0.3543478260869565299, 0.3565217391304347783, 0.3586956521739130266, 0.3608695652173913304, 0.3630434782608695787, 0.3652173913043478271, 0.3673913043478260754, 0.3695652173913043237, 0.3717391304347826275, 0.3739130434782608758, 0.3760869565217391242, 0.3782608695652173725, 0.3804347826086956763, 0.3826086956521739246, 0.3847826086956521729, 0.3869565217391304213, 0.3891304347826086696, 0.3913043478260869734, 0.3934782608695652217, 0.3956521739130434701, 0.3978260869565217184, 0.4000000000000000222, 0.4021739130434782705, 0.4043478260869565188, 0.4065217391304347672, 0.4086956521739130710, 0.4108695652173913193, 0.4130434782608695676, 0.4152173913043478160, 0.4173913043478260643, 0.4195652173913043681, 0.4217391304347826164, 0.4239130434782608647, 0.4260869565217391131, 0.4282608695652174169, 0.4304347826086956652, 0.4326086956521739135, 0.4347826086956521618, 0.4369565217391304102, 0.4391304347826087140, 0.4413043478260869623, 0.4434782608695652106, 0.4456521739130434590, 0.4478260869565217628, 0.4500000000000000111, 0.4521739130434782594, 0.4543478260869565077, 0.4565217391304347561, 0.4586956521739130599, 0.4608695652173913082, 0.4630434782608695565, 0.4652173913043478048, 0.4673913043478261087, 0.4695652173913043570, 0.4717391304347826053, 0.4739130434782608536, 0.4760869565217391575, 0.4782608695652174058, 0.4804347826086956541, 0.4826086956521739024, 0.4847826086956521507, 0.4869565217391304546, 0.4891304347826087029, 0.4913043478260869512, 0.4934782608695651995, 0.4956521739130435034, 0.4978260869565217517, 0.5000000000000000000, 0.5021739130434782483, 0.5043478260869564966, 0.5065217391304347450, 0.5086956521739129933, 0.5108695652173913526, 0.5130434782608696009, 0.5152173913043478493, 0.5173913043478260976, 0.5195652173913043459, 0.5217391304347825942, 0.5239130434782608425, 0.5260869565217390909, 0.5282608695652173392, 0.5304347826086956985, 0.5326086956521739468, 0.5347826086956521952, 0.5369565217391304435, 0.5391304347826086918, 0.5413043478260869401, 0.5434782608695651884, 0.5456521739130434367, 0.5478260869565216851, 0.5500000000000000444, 0.5521739130434782927, 0.5543478260869565410, 0.5565217391304347894, 0.5586956521739130377, 0.5608695652173912860, 0.5630434782608695343, 0.5652173913043477826, 0.5673913043478261420, 0.5695652173913043903, 0.5717391304347826386, 0.5739130434782608869, 0.5760869565217391353, 0.5782608695652173836, 0.5804347826086956319, 0.5826086956521738802, 0.5847826086956521285, 0.5869565217391304879, 0.5891304347826087362, 0.5913043478260869845, 0.5934782608695652328, 0.5956521739130434812, 0.5978260869565217295, 0.5999999999999999778, 0.6021739130434782261, 0.6043478260869564744, 0.6065217391304348338, 0.6086956521739130821, 0.6108695652173913304, 0.6130434782608695787, 0.6152173913043478271, 0.6173913043478260754, 0.6195652173913043237, 0.6217391304347825720, 0.6239130434782608203, 0.6260869565217391797, 0.6282608695652174280, 0.6304347826086956763, 0.6326086956521739246, 0.6347826086956521729, 0.6369565217391304213, 0.6391304347826086696, 0.6413043478260869179, 0.6434782608695651662, 0.6456521739130435256, 0.6478260869565217739, 0.6500000000000000222, 0.6521739130434782705, 0.6543478260869565188, 0.6565217391304347672, 0.6586956521739130155, 0.6608695652173912638, 0.6630434782608695121, 0.6652173913043478715, 0.6673913043478261198, 0.6695652173913043681, 0.6717391304347826164, 0.6739130434782608647, 0.6760869565217391131, 0.6782608695652173614, 0.6804347826086956097, 0.6826086956521738580, 0.6847826086956522174, 0.6869565217391304657, 0.6891304347826087140, 0.6913043478260869623, 0.6934782608695652106, 0.6956521739130434590, 0.6978260869565217073, 0.6999999999999999556, 0.7021739130434783149, 0.7043478260869565633, 0.7065217391304348116, 0.7086956521739130599, 0.7108695652173913082, 0.7130434782608695565, 0.7152173913043478048, 0.7173913043478260532, 0.7195652173913043015, 0.7217391304347826608, 0.7239130434782609091, 0.7260869565217391575, 0.7282608695652174058, 0.7304347826086956541, 0.7326086956521739024, 0.7347826086956521507, 0.7369565217391303991, 0.7391304347826086474, 0.7413043478260870067, 0.7434782608695652550, 0.7456521739130435034, 0.7478260869565217517, 0.7500000000000000000, 0.7521739130434782483, 0.7543478260869564966, 0.7565217391304347450, 0.7586956521739129933, 0.7608695652173913526, 0.7630434782608696009, 0.7652173913043478493, 0.7673913043478260976, 0.7695652173913043459, 0.7717391304347825942, 0.7739130434782608425, 0.7760869565217390909, 0.7782608695652173392, 0.7804347826086956985, 0.7826086956521739468, 0.7847826086956521952, 0.7869565217391304435, 0.7891304347826086918, 0.7913043478260869401, 0.7934782608695651884, 0.7956521739130434367, 0.7978260869565216851, 0.8000000000000000444, 0.8021739130434782927, 0.8043478260869565410, 0.8065217391304347894, 0.8086956521739130377, 0.8108695652173912860, 0.8130434782608695343, 0.8152173913043477826, 0.8173913043478261420, 0.8195652173913043903, 0.8217391304347826386, 0.8239130434782608869, 0.8260869565217391353, 0.8282608695652173836, 0.8304347826086956319, 0.8326086956521738802, 0.8347826086956521285, 0.8369565217391304879, 0.8391304347826087362, 0.8413043478260869845, 0.8434782608695652328, 0.8456521739130434812, 0.8478260869565217295, 0.8499999999999999778, 0.8521739130434782261, 0.8543478260869564744, 0.8565217391304348338, 0.8586956521739130821, 0.8608695652173913304, 0.8630434782608695787, 0.8652173913043478271, 0.8673913043478260754, 0.8695652173913043237, 0.8717391304347825720, 0.8739130434782608203, 0.8760869565217391797, 0.8782608695652174280, 0.8804347826086956763, 0.8826086956521739246, 0.8847826086956521729, 0.8869565217391304213, 0.8891304347826086696, 0.8913043478260869179, 0.8934782608695651662, 0.8956521739130435256, 0.8978260869565217739, 0.9000000000000000222, 0.9021739130434782705, 0.9043478260869565188, 0.9065217391304347672, 0.9086956521739130155, 0.9108695652173912638, 0.9130434782608695121, 0.9152173913043478715, 0.9173913043478261198, 0.9195652173913043681, 0.9217391304347826164, 0.9239130434782608647, 0.9260869565217391131, 0.9282608695652173614, 0.9304347826086956097, 0.9326086956521738580, 0.9347826086956522174, 0.9369565217391304657, 0.9391304347826087140, 0.9413043478260869623, 0.9434782608695652106, 0.9456521739130434590, 0.9478260869565217073, 0.9499999999999999556, 0.9521739130434783149, 0.9543478260869565633, 0.9565217391304348116, 0.9586956521739130599, 0.9608695652173913082, 0.9630434782608695565, 0.9652173913043478048, 0.9673913043478260532, 0.9695652173913043015, 0.9717391304347826608, 0.9739130434782609091, 0.9760869565217391575, 0.9782608695652174058, 0.9804347826086956541, 0.9826086956521739024, 0.9847826086956521507, 0.9869565217391303991, 0.9891304347826086474, 0.9913043478260870067 ),
 .UNSPECIFIED. ) 
 CURVE ( )  GEOMETRIC_REPRESENTATION_ITEM ( )  RATIONAL_B_SPLINE_CURVE ( ( 0.9872147520176037805, 0.9924394633425718260, 1.000000000000000000, 0.9510565162951535312, 1.000000000000000000, 0.9510565162951535312, 1.000000000000000000, 0.9510565162951535312, 1.000000000000000000, 0.9510565162951535312, 1.000000000000000000, 0.9510565162951535312, 1.000000000000000000, 0.9510565162951535312, 1.000000000000000000, 0.9510565162951535312, 1.000000000000000000, 0.9510565162951535312, 1.000000000000000000, 0.9510565162951535312, 1.000000000000000000, 0.9510565162951535312, 1.000000000000000000, 0.9510565162951535312, 1.000000000000000000, 0.9510565162951535312, 1.000000000000000000, 0.9510565162951535312, 1.000000000000000000, 0.9510565162951535312, 1.000000000000000000, 0.9510565162951535312, 1.000000000000000000, 0.9510565162951535312, 1.000000000000000000, 0.9510565162951535312, 1.000000000000000000, 0.9510565162951535312, 1.000000000000000000, 0.9510565162951535312, 1.000000000000000000, 0.9510565162951535312, 1.000000000000000000, 0.9510565162951535312, 1.000000000000000000, 0.9510565162951535312, 1.000000000000000000, 0.9510565162951535312, 1.000000000000000000, 0.9510565162951535312, 1.000000000000000000, 0.9510565162951535312, 1.000000000000000000, 0.9510565162951535312, 1.000000000000000000, 0.9510565162951535312, 1.000000000000000000, 0.9510565162951535312, 1.000000000000000000, 0.9510565162951535312, 1.000000000000000000, 0.9510565162951535312, 1.000000000000000000, 0.9510565162951535312, 1.000000000000000000, 0.9510565162951535312, 1.000000000000000000, 0.9510565162951535312, 1.000000000000000000, 0.9510565162951535312, 1.000000000000000000, 0.9510565162951535312, 1.000000000000000000, 0.9510565162951535312, 1.000000000000000000, 0.9510565162951535312, 1.000000000000000000, 0.9510565162951535312, 1.000000000000000000, 0.9510565162951535312, 1.000000000000000000, 0.9510565162951535312, 1.000000000000000000, 0.9510565162951535312, 1.000000000000000000, 0.9510565162951535312, 1.000000000000000000, 0.9510565162951535312, 1.000000000000000000, 0.9510565162951535312, 1.000000000000000000, 0.9510565162951535312, 1.000000000000000000, 0.9510565162951535312, 1.000000000000000000, 0.9510565162951535312, 1.000000000000000000, 0.9510565162951535312, 1.000000000000000000, 0.9510565162951535312, 1.000000000000000000, 0.9510565162951535312, 1.000000000000000000, 0.9510565162951535312, 1.000000000000000000, 0.9510565162951535312, 1.000000000000000000, 0.9510565162951535312, 1.000000000000000000, 0.9510565162951535312, 1.000000000000000000, 0.9510565162951535312, 1.000000000000000000, 0.9510565162951535312, 1.000000000000000000, 0.9510565162951535312, 1.000000000000000000, 0.9510565162951535312, 1.000000000000000000, 0.9510565162951535312, 1.000000000000000000, 0.9510565162951535312, 1.000000000000000000, 0.9510565162951535312, 1.000000000000000000, 0.9510565162951535312, 1.000000000000000000, 0.9510565162951535312, 1.000000000000000000, 0.9510565162951535312, 1.000000000000000000, 0.9510565162951535312, 1.000000000000000000, 0.9510565162951535312, 1.000000000000000000, 0.9510565162951535312, 1.000000000000000000, 0.9510565162951535312, 1.000000000000000000, 0.9510565162951535312, 1.000000000000000000, 0.9510565162951535312, 1.000000000000000000, 0.9510565162951535312, 1.000000000000000000, 0.9510565162951535312, 1.000000000000000000, 0.9510565162951535312, 1.000000000000000000, 0.9510565162951535312, 1.000000000000000000, 0.9510565162951535312, 1.000000000000000000, 0.9510565162951535312, 1.000000000000000000, 0.9510565162951535312, 1.000000000000000000, 0.9510565162951535312, 1.000000000000000000, 0.9510565162951535312, 1.000000000000000000, 0.9510565162951535312, 1.000000000000000000, 0.9510565162951535312, 1.000000000000000000, 0.9510565162951535312, 1.000000000000000000, 0.9510565162951535312, 1.000000000000000000, 0.9510565162951535312, 1.000000000000000000, 0.9510565162951535312, 1.000000000000000000, 0.9510565162951535312, 1.000000000000000000, 0.9510565162951535312, 1.000000000000000000, 0.9510565162951535312, 1.000000000000000000, 0.9510565162951535312, 1.000000000000000000, 0.9510565162951535312, 1.000000000000000000, 0.9510565162951535312, 1.000000000000000000, 0.9510565162951535312, 1.000000000000000000, 0.9510565162951535312, 1.000000000000000000, 0.9510565162951535312, 1.000000000000000000, 0.9510565162951535312, 1.000000000000000000, 0.9510565162951535312, 1.000000000000000000, 0.9510565162951535312, 1.000000000000000000, 0.9510565162951535312, 1.000000000000000000, 0.9510565162951535312, 1.000000000000000000, 0.9510565162951535312, 1.000000000000000000, 0.9510565162951535312, 1.000000000000000000, 0.9510565162951535312, 1.000000000000000000, 0.9510565162951535312, 1.000000000000000000, 0.9510565162951535312, 1.000000000000000000, 0.9510565162951535312, 1.000000000000000000, 0.9510565162951535312, 1.000000000000000000, 0.9510565162951535312, 1.000000000000000000, 0.9510565162951535312, 1.000000000000000000, 0.9510565162951535312, 1.000000000000000000, 0.9510565162951535312, 1.000000000000000000, 0.9510565162951535312, 1.000000000000000000, 0.9510565162951535312, 1.000000000000000000, 0.9510565162951535312, 1.000000000000000000, 0.9510565162951535312, 1.000000000000000000, 0.9510565162951535312, 1.000000000000000000, 0.9510565162951535312, 1.000000000000000000, 0.9510565162951535312, 1.000000000000000000, 0.9510565162951535312, 1.000000000000000000, 0.9510565162951535312, 1.000000000000000000, 0.9510565162951535312, 1.000000000000000000, 0.9510565162951535312, 1.000000000000000000, 0.9510565162951535312, 1.000000000000000000, 0.9510565162951535312, 1.000000000000000000, 0.9510565162951535312, 1.000000000000000000, 0.9510565162951535312, 1.000000000000000000, 0.9510565162951535312, 1.000000000000000000, 0.9510565162951535312, 1.000000000000000000, 0.9510565162951535312, 1.000000000000000000, 0.9510565162951535312, 1.000000000000000000, 0.9510565162951535312, 1.000000000000000000, 0.9510565162951535312, 1.000000000000000000, 0.9510565162951535312, 1.000000000000000000, 0.9510565162951535312, 1.000000000000000000, 0.9510565162951535312, 1.000000000000000000, 0.9510565162951535312, 1.000000000000000000, 0.9510565162951535312, 1.000000000000000000, 0.9510565162951535312, 1.000000000000000000, 0.9510565162951535312, 1.000000000000000000, 0.9510565162951535312, 1.000000000000000000, 0.9510565162951535312, 1.000000000000000000, 0.9510565162951535312, 1.000000000000000000, 0.9510565162951535312, 1.000000000000000000, 0.9510565162951535312, 1.000000000000000000, 0.9510565162951535312, 1.000000000000000000, 0.9510565162951535312, 1.000000000000000000, 0.9510565162951535312, 1.000000000000000000, 0.9510565162951535312, 1.000000000000000000, 0.9510565162951535312, 1.000000000000000000, 0.9510565162951535312, 1.000000000000000000, 0.9510565162951535312, 1.000000000000000000, 0.9510565162951535312, 1.000000000000000000, 0.9510565162951535312, 1.000000000000000000, 0.9510565162951535312, 1.000000000000000000, 0.9510565162951535312, 1.000000000000000000, 0.9510565162951535312, 1.000000000000000000, 0.9510565162951535312, 1.000000000000000000, 0.9510565162951535312, 1.000000000000000000, 0.9510565162951535312, 1.000000000000000000, 0.9510565162951535312, 1.000000000000000000, 0.9510565162951535312, 1.000000000000000000, 0.9510565162951535312, 1.000000000000000000, 0.9510565162951535312, 1.000000000000000000, 0.9510565162951535312, 1.000000000000000000, 0.9510565162951535312, 1.000000000000000000, 0.9510565162951535312, 1.000000000000000000, 0.9510565162951535312, 1.000000000000000000, 0.9510565162951535312, 1.000000000000000000, 0.9510565162951535312, 1.000000000000000000, 0.9510565162951535312, 1.000000000000000000, 0.9510565162951535312, 1.000000000000000000, 0.9510565162951535312, 1.000000000000000000, 0.9510565162951535312, 1.000000000000000000, 0.9510565162951535312, 1.000000000000000000, 0.9510565162951535312, 1.000000000000000000, 0.9510565162951535312, 1.000000000000000000, 0.9510565162951535312, 1.000000000000000000, 0.9510565162951535312, 1.000000000000000000, 0.9510565162951535312, 1.000000000000000000, 0.9510565162951535312, 1.000000000000000000, 0.9510565162951535312, 1.000000000000000000, 0.9510565162951535312, 1.000000000000000000, 0.9510565162951535312, 1.000000000000000000, 0.9510565162951535312, 1.000000000000000000, 0.9510565162951535312, 1.000000000000000000, 0.9510565162951535312, 1.000000000000000000, 0.9510565162951535312, 1.000000000000000000, 0.9510565162951535312, 1.000000000000000000, 0.9510565162951535312, 1.000000000000000000, 0.9510565162951535312, 1.000000000000000000, 0.9510565162951535312, 1.000000000000000000, 0.9510565162951535312, 1.000000000000000000, 0.9510565162951535312, 1.000000000000000000, 0.9510565162951535312, 1.000000000000000000, 0.9510565162951535312, 1.000000000000000000, 0.9510565162951535312, 1.000000000000000000, 0.9510565162951535312, 1.000000000000000000, 0.9510565162951535312, 1.000000000000000000, 0.9510565162951535312, 1.000000000000000000, 0.9510565162951535312, 1.000000000000000000, 0.9510565162951535312, 1.000000000000000000, 0.9510565162951535312, 1.000000000000000000, 0.9510565162951535312, 1.000000000000000000, 0.9510565162951535312, 1.000000000000000000, 0.9510565162951535312, 1.000000000000000000, 0.9510565162951535312, 1.000000000000000000, 0.9510565162951535312, 1.000000000000000000, 0.9510565162951535312, 1.000000000000000000, 0.9510565162951535312, 1.000000000000000000, 0.9510565162951535312, 1.000000000000000000, 0.9510565162951535312, 1.000000000000000000, 0.9510565162951535312, 1.000000000000000000, 0.9510565162951535312, 1.000000000000000000, 0.9510565162951535312, 1.000000000000000000, 0.9510565162951535312, 1.000000000000000000, 0.9510565162951535312, 1.000000000000000000, 0.9510565162951535312, 1.000000000000000000, 0.9510565162951535312, 1.000000000000000000, 0.9510565162951535312, 1.000000000000000000, 0.9510565162951535312, 1.000000000000000000, 0.9510565162951535312, 1.000000000000000000, 0.9510565162951535312, 1.000000000000000000, 0.9510565162951535312, 1.000000000000000000, 0.9510565162951535312, 1.000000000000000000, 0.9510565162951535312, 1.000000000000000000, 0.9510565162951535312, 1.000000000000000000, 0.9510565162951535312, 1.000000000000000000, 0.9510565162951535312, 1.000000000000000000, 0.9510565162951535312, 1.000000000000000000, 0.9510565162951535312, 1.000000000000000000, 0.9510565162951535312, 1.000000000000000000, 0.9510565162951535312, 1.000000000000000000, 0.9510565162951535312, 1.000000000000000000, 0.9510565162951535312, 1.000000000000000000, 0.9510565162951535312, 1.000000000000000000, 0.9510565162951535312, 1.000000000000000000, 0.9510565162951535312, 1.000000000000000000, 0.9510565162951535312, 1.000000000000000000, 0.9510565162951535312, 1.000000000000000000, 0.9510565162951535312, 1.000000000000000000, 0.9510565162951535312, 1.000000000000000000, 0.9510565162951535312, 1.000000000000000000, 0.9510565162951535312, 1.000000000000000000, 0.9510565162951535312, 1.000000000000000000, 0.9510565162951535312, 1.000000000000000000, 0.9510565162951535312, 1.000000000000000000, 0.9510565162951535312, 1.000000000000000000, 0.9510565162951535312, 1.000000000000000000, 0.9510565162951535312, 1.000000000000000000, 0.9510565162951535312, 1.000000000000000000, 0.9510565162951535312, 1.000000000000000000, 0.9510565162951535312, 1.000000000000000000, 0.9510565162951535312, 1.000000000000000000, 0.9510565162951535312, 1.000000000000000000, 0.9510565162951535312, 1.000000000000000000, 0.9510565162951535312, 1.000000000000000000, 0.9510565162951535312, 1.000000000000000000, 0.9510565162951535312, 1.000000000000000000, 0.9510565162951535312, 1.000000000000000000, 0.9510565162951535312, 1.000000000000000000, 0.9510565162951535312, 1.000000000000000000, 0.9510565162951535312, 1.000000000000000000, 0.9510565162951535312, 1.000000000000000000, 0.9510565162951535312, 1.000000000000000000, 0.9510565162951535312, 1.000000000000000000, 0.9510565162951535312, 1.000000000000000000, 0.9510565162951535312, 1.000000000000000000, 0.9510565162951535312, 1.000000000000000000, 0.9510565162951535312, 1.000000000000000000, 0.9510565162951535312, 1.000000000000000000, 0.9510565162951535312, 1.000000000000000000, 0.9510565162951535312, 1.000000000000000000, 0.9510565162951535312, 1.000000000000000000, 0.9510565162951535312, 1.000000000000000000, 0.9510565162951535312, 1.000000000000000000, 0.9510565162951535312, 1.000000000000000000, 0.9510565162951535312, 1.000000000000000000, 0.9510565162951535312, 1.000000000000000000, 0.9510565162951535312, 1.000000000000000000, 0.9510565162951535312, 1.000000000000000000, 0.9510565162951535312, 1.000000000000000000, 0.9510565162951535312, 1.000000000000000000, 0.9510565162951535312, 1.000000000000000000, 0.9510565162951535312, 1.000000000000000000, 0.9510565162951535312, 1.000000000000000000, 0.9510565162951535312, 1.000000000000000000, 0.9510565162951535312, 1.000000000000000000, 0.9510565162951535312, 1.000000000000000000, 0.9510565162951535312, 1.000000000000000000, 0.9510565162951535312, 1.000000000000000000, 0.9510565162951535312, 1.000000000000000000, 0.9510565162951535312, 1.000000000000000000, 0.9510565162951535312, 1.000000000000000000, 0.9510565162951535312, 1.000000000000000000, 0.9510565162951535312, 1.000000000000000000, 0.9510565162951535312, 1.000000000000000000, 0.9510565162951535312, 1.000000000000000000, 0.9510565162951535312, 1.000000000000000000, 0.9510565162951535312, 1.000000000000000000, 0.9510565162951535312, 1.000000000000000000, 0.9510565162951535312, 1.000000000000000000, 0.9510565162951535312, 1.000000000000000000, 0.9510565162951535312, 1.000000000000000000, 0.9510565162951535312, 1.000000000000000000, 0.9510565162951535312, 1.000000000000000000, 0.9510565162951535312, 1.000000000000000000, 0.9510565162951535312, 1.000000000000000000, 0.9510565162951535312, 1.000000000000000000, 0.9510565162951535312, 1.000000000000000000, 0.9510565162951535312, 1.000000000000000000, 0.9510565162951535312, 1.000000000000000000, 0.9510565162951535312, 1.000000000000000000, 0.9510565162951535312, 1.000000000000000000, 0.9510565162951535312, 1.000000000000000000, 0.9510565162951535312, 1.000000000000000000, 0.9510565162951535312, 1.000000000000000000, 0.9510565162951535312, 1.000000000000000000, 0.9510565162951535312, 1.000000000000000000, 0.9510565162951535312, 1.000000000000000000, 0.9510565162951535312, 1.000000000000000000, 0.9510565162951535312, 1.000000000000000000, 0.9510565162951535312, 1.000000000000000000, 0.9510565162951535312, 1.000000000000000000, 0.9510565162951535312, 1.000000000000000000, 0.9510565162951535312, 1.000000000000000000, 0.9510565162951535312, 1.000000000000000000, 0.9510565162951535312, 1.000000000000000000, 0.9510565162951535312, 1.000000000000000000, 0.9510565162951535312, 1.000000000000000000, 0.9510565162951535312, 1.000000000000000000, 0.9510565162951535312, 1.000000000000000000, 0.9510565162951535312, 1.000000000000000000, 0.9510565162951535312, 1.000000000000000000, 0.9510565162951535312, 1.000000000000000000, 0.9510565162951535312, 1.000000000000000000, 0.9510565162951535312, 1.000000000000000000, 0.9510565162951535312, 1.000000000000000000, 0.9510565162951535312, 1.000000000000000000, 0.9510565162951535312, 1.000000000000000000, 0.9510565162951535312, 1.000000000000000000, 0.9510565162951535312, 1.000000000000000000, 0.9510565162951535312, 1.000000000000000000, 0.9510565162951535312, 1.000000000000000000, 0.9510565162951535312, 1.000000000000000000, 0.9510565162951535312, 1.000000000000000000, 0.9510565162951535312, 1.000000000000000000, 0.9510565162951535312, 1.000000000000000000, 0.9510565162951535312, 1.000000000000000000, 0.9510565162951535312, 1.000000000000000000, 0.9510565162951535312, 1.000000000000000000, 0.9510565162951535312, 1.000000000000000000, 0.9510565162951535312, 1.000000000000000000, 0.9510565162951535312, 1.000000000000000000, 0.9510565162951535312, 1.000000000000000000, 0.9510565162951535312, 1.000000000000000000, 0.9510565162951535312, 1.000000000000000000, 0.9510565162951535312, 1.000000000000000000, 0.9510565162951535312, 1.000000000000000000, 0.9510565162951535312, 1.000000000000000000, 0.9510565162951535312, 1.000000000000000000, 0.9510565162951535312, 1.000000000000000000, 0.9510565162951535312, 1.000000000000000000, 0.9510565162951535312, 1.000000000000000000, 0.9510565162951535312, 1.000000000000000000, 0.9510565162951535312, 1.000000000000000000, 0.9510565162951535312, 1.000000000000000000, 0.9510565162951535312, 1.000000000000000000, 0.9510565162951535312, 1.000000000000000000, 0.9510565162951535312, 1.000000000000000000, 0.9510565162951535312, 1.000000000000000000, 0.9510565162951535312, 1.000000000000000000, 0.9510565162951535312, 1.000000000000000000, 0.9510565162951535312, 1.000000000000000000, 0.9510565162951535312, 1.000000000000000000, 0.9510565162951535312, 1.000000000000000000, 0.9510565162951535312, 1.000000000000000000, 0.9510565162951535312, 1.000000000000000000, 0.9510565162951535312, 1.000000000000000000, 0.9510565162951535312, 1.000000000000000000, 0.9510565162951535312, 1.000000000000000000, 0.9510565162951535312, 1.000000000000000000, 0.9510565162951535312, 1.000000000000000000, 0.9510565162951535312, 1.000000000000000000, 0.9510565162951535312, 1.000000000000000000, 0.9510565162951535312, 1.000000000000000000, 0.9510565162951535312, 1.000000000000000000, 0.9510565162951535312, 1.000000000000000000, 0.9510565162951535312, 1.000000000000000000, 0.9510565162951535312, 1.000000000000000000, 0.9510565162951535312, 1.000000000000000000, 0.9510565162951535312, 1.000000000000000000, 0.9510565162951535312, 1.000000000000000000, 0.9510565162951535312, 1.000000000000000000, 0.9510565162951535312, 1.000000000000000000, 0.9510565162951535312, 1.000000000000000000, 0.9510565162951535312, 1.000000000000000000, 0.9510565162951535312, 1.000000000000000000, 0.9510565162951535312, 1.000000000000000000, 0.9510565162951535312, 1.000000000000000000, 0.9510565162951535312, 1.000000000000000000, 0.9510565162951535312, 1.000000000000000000, 0.9510565162951535312, 1.000000000000000000, 0.9510565162951535312, 1.000000000000000000, 0.9510565162951535312, 1.000000000000000000, 0.9510565162951535312, 1.000000000000000000, 0.9510565162951535312, 1.000000000000000000, 0.9510565162951535312, 1.000000000000000000, 0.9510565162951535312, 1.000000000000000000, 0.9510565162951535312, 1.000000000000000000, 0.9510565162951535312, 1.000000000000000000, 0.9510565162951535312, 1.000000000000000000, 0.9510565162951535312, 1.000000000000000000, 0.9510565162951535312, 1.000000000000000000, 0.9510565162951535312, 1.000000000000000000, 0.9510565162951535312, 1.000000000000000000, 0.9510565162951535312, 1.000000000000000000, 0.9510565162951535312, 1.000000000000000000, 0.9510565162951535312, 1.000000000000000000, 0.9510565162951535312, 1.000000000000000000, 0.9510565162951535312, 1.000000000000000000, 0.9510565162951535312, 1.000000000000000000, 0.9510565162951535312, 1.000000000000000000, 0.9510565162951535312, 1.000000000000000000, 0.9510565162951535312, 1.000000000000000000, 0.9510565162951535312, 1.000000000000000000, 0.9510565162951535312, 1.000000000000000000, 0.9510565162951535312, 1.000000000000000000, 0.9510565162951535312, 1.000000000000000000, 0.9510565162951535312, 1.000000000000000000, 0.9510565162951535312, 1.000000000000000000, 0.9510565162951535312, 1.000000000000000000, 0.9510565162951535312, 1.000000000000000000, 0.9510565162951535312, 1.000000000000000000, 0.9510565162951535312, 1.000000000000000000, 0.9510565162951535312, 1.000000000000000000, 0.9510565162951535312, 1.000000000000000000, 0.9510565162951535312, 1.000000000000000000, 0.9510565162951535312, 1.000000000000000000, 0.9510565162951535312, 1.000000000000000000, 0.9510565162951535312, 1.000000000000000000, 0.9510565162951535312, 1.000000000000000000, 0.9510565162951535312, 1.000000000000000000, 0.9510565162951535312, 1.000000000000000000, 0.9510565162951535312, 1.000000000000000000, 0.9510565162951535312, 1.000000000000000000, 0.9510565162951535312, 1.000000000000000000, 0.9510565162951535312, 1.000000000000000000, 0.9510565162951535312, 1.000000000000000000, 0.9510565162951535312, 1.000000000000000000, 0.9510565162951535312, 1.000000000000000000, 0.9510565162951535312, 1.000000000000000000, 0.9510565162951535312, 1.000000000000000000, 0.9510565162951535312, 1.000000000000000000, 0.9510565162951535312, 1.000000000000000000, 0.9510565162951535312, 1.000000000000000000 ) ) 
 REPRESENTATION_ITEM ( '' )  );
#63033 = ORIENTED_EDGE ( 'NONE', *, *, #58004, .T. ) ;
#63034 = PRESENTATION_LAYER_ASSIGNMENT (  '', '', ( #58575 ) ) ;
#63035 = CYLINDRICAL_SURFACE ( 'NONE', #47723, 3.000000000000000444 ) ;
#63036 = CARTESIAN_POINT ( 'NONE',  ( -8.102448949553179958, 120.0049999999999812, -5.886773742842749790 ) ) ;
#63037 =( GEOMETRIC_REPRESENTATION_CONTEXT ( 3 ) GLOBAL_UNCERTAINTY_ASSIGNED_CONTEXT ( ( #67218 ) ) GLOBAL_UNIT_ASSIGNED_CONTEXT ( ( #43924, #54754, #558 ) ) REPRESENTATION_CONTEXT ( 'NONE', 'WORKASPACE' ) );
#63038 = CARTESIAN_POINT ( 'NONE',  ( -77.75499999999999545, 4.716976649647091513, -6.492361379858946790 ) ) ;
#63039 = DIRECTION ( 'NONE',  ( -0.000000000000000000, 1.000000000000000000, -0.000000000000000000 ) ) ;
#63040 = PRODUCT_DEFINITION_SHAPE ( 'NONE', 'NONE',  #59698 ) ;
#63041 = ORIENTED_EDGE ( 'NONE', *, *, #40603, .T. ) ;
#63042 = CARTESIAN_POINT ( 'NONE',  ( -3.094860106618434248, 141.9050000000000011, 9.525000000000000355 ) ) ;
#63043 = UNCERTAINTY_MEASURE_WITH_UNIT (LENGTH_MEASURE( 1.000000000000000082E-05 ), #5685, 'distance_accuracy_value', 'NONE');
#63044 = CARTESIAN_POINT ( 'NONE',  ( -57.99999999999997868, 50.00000000000000000, 6.500000000000000000 ) ) ;
#63045 = VECTOR ( 'NONE', #63618, 1000.000000000000000 ) ;
#63046 = EDGE_CURVE ( 'NONE', #46046, #47926, #36464, .T. ) ;
#63047 = CARTESIAN_POINT ( 'NONE',  ( -41.30888752411017606, 107.2690689356287663, 3.464811251346369581 ) ) ;
#63048 = CIRCLE ( 'NONE', #20364, 17.00000000000000000 ) ;
#63049 = FILL_AREA_STYLE ('',( #62363 ) ) ;
#63050 = ORIENTED_EDGE ( 'NONE', *, *, #28325, .T. ) ;
#63051 = DIRECTION ( 'NONE',  ( -0.000000000000000000, 1.000000000000000000, 0.000000000000000000 ) ) ;
#63052 = SURFACE_STYLE_USAGE ( .BOTH. , #58476 ) ;
#63053 = DIRECTION ( 'NONE',  ( 0.000000000000000000, 0.000000000000000000, 1.000000000000000000 ) ) ;
#63054 = CARTESIAN_POINT ( 'NONE',  ( -177.2050000000000125, -2.607480562269071545, -8.024999999999991473 ) ) ;
#63056 = ORIENTED_EDGE ( 'NONE', *, *, #2299, .F. ) ;
#63055 = VECTOR ( 'NONE', #36063, 1000.000000000000000 ) ;
#63057 = CARTESIAN_POINT ( 'NONE',  ( 5.871527698221330027, 111.7477971676043609, -5.859198738425208219 ) ) ;
#63058 = EDGE_CURVE ( 'NONE', #61698, #52342, #9531, .T. ) ;
#63059 = DIRECTION ( 'NONE',  ( 0.000000000000000000, 1.000000000000000000, 0.000000000000000000 ) ) ;
#63060 =( LENGTH_UNIT ( ) NAMED_UNIT ( * ) SI_UNIT ( .MILLI., .METRE. ) );
#63061 = EDGE_LOOP ( 'NONE', ( #14869, #56390, #62785, #36874 ) ) ;
#63062 = DIRECTION ( 'NONE',  ( 0.000000000000000000, -1.000000000000000000, 0.000000000000000000 ) ) ;
#63063 = CARTESIAN_POINT ( 'NONE',  ( -195.0000000000000000, 1.166476076187852838E-15, -9.524999999999991473 ) ) ;
#63064 = PRESENTATION_LAYER_ASSIGNMENT (  '', '', ( #9150 ) ) ;
#63065 = VERTEX_POINT ( 'NONE', #64469 ) ;
#63066 = CARTESIAN_POINT ( 'NONE',  ( 45.65811388300841855, 10.21937129433612235, 3.999999999999999112 ) ) ;
#63067 = CARTESIAN_POINT ( 'NONE',  ( -98.15499999999998693, 7.632228543268600340, 2.479861379858949277 ) ) ;
#63068 = ORIENTED_EDGE ( 'NONE', *, *, #54713, .T. ) ;
#63069 = AXIS2_PLACEMENT_3D ( 'NONE', #60027, #58647, #54051 ) ;
#63070 = EDGE_CURVE ( 'NONE', #10224, #26613, #48864, .T. ) ;
#63071 = DIRECTION ( 'NONE',  ( 0.000000000000000000, 0.000000000000000000, -1.000000000000000000 ) ) ;
#63072 = CARTESIAN_POINT ( 'NONE',  ( -135.3570736234661638, 5.598654528085804216, 7.705886871421366635 ) ) ;
#63073 = SURFACE_STYLE_FILL_AREA ( #69065 ) ;
#63074 = MECHANICAL_DESIGN_GEOMETRIC_PRESENTATION_REPRESENTATION (  '', ( #4616 ), #27093 ) ;
#63075 = CARTESIAN_POINT ( 'NONE',  ( -9.058813317711338797, 149.3449999999999989, 2.943386871421373563 ) ) ;
#63076 = CARTESIAN_POINT ( 'NONE',  ( -75.95707362346617231, 9.058813317711329915, -2.943386871421373119 ) ) ;
#63077 = VECTOR ( 'NONE', #59085, 1000.000000000000000 ) ;
#63078 = EDGE_CURVE ( 'NONE', #60536, #4324, #20709, .T. ) ;
#63079 = ORIENTED_EDGE ( 'NONE', *, *, #30195, .T. ) ;
#63080 = LINE ( 'NONE', #13855, #6902 ) ;
#63081 = DIRECTION ( 'NONE',  ( -1.000000000000000000, 0.000000000000000000, 0.000000000000000000 ) ) ;
#63082 = VECTOR ( 'NONE', #57362, 1000.000000000000000 ) ;
#63083 = CARTESIAN_POINT ( 'NONE',  ( 98.00000000000000000, 16.00000000000000000, 0.000000000000000000 ) ) ;
#63084 = CARTESIAN_POINT ( 'NONE',  ( -109.5549999999999926, 0.000000000000000000, 8.024999999999991473 ) ) ;
#63085 = CARTESIAN_POINT ( 'NONE',  ( 60.00000000000000000, 1.797044900979284448E-15, -12.00000000000000000 ) ) ;
#63086 = CARTESIAN_POINT ( 'NONE',  ( 8.102448949553183510, 120.9949999999999761, -5.886773742842746238 ) ) ;
#63087 = CARTESIAN_POINT ( 'NONE',  ( -124.7949999999999733, 2.607480562269068880, -8.024999999999993250 ) ) ;
#63088 = AXIS2_PLACEMENT_3D ( 'NONE', #23913, #65795, #50313 ) ;
#63089 = CARTESIAN_POINT ( 'NONE',  ( 57.24999999999999289, 27.74999999999998934, 4.000000000000000000 ) ) ;
#63090 = CARTESIAN_POINT ( 'NONE',  ( -11.99999999999999822, -6.499999999999999112, 3.000000000000000000 ) ) ;
#63091 = ORIENTED_EDGE ( 'NONE', *, *, #26062, .T. ) ;
#63093 = VECTOR ( 'NONE', #32208, 1000.000000000000000 ) ;
#63092 = CARTESIAN_POINT ( 'NONE',  ( 15.98999599679679839, 146.4999999999999716, 10.00000000000000000 ) ) ;
#63094 = CARTESIAN_POINT ( 'NONE',  ( -176.0929263765338249, 3.094860106618433360, 9.524999999999991473 ) ) ;
#63095 =( NAMED_UNIT ( * ) PLANE_ANGLE_UNIT ( ) SI_UNIT ( $, .RADIAN. ) );
#63096 = CARTESIAN_POINT ( 'NONE',  ( -195.0000000000000000, 1.166476076187852838E-15, -9.524999999999991473 ) ) ;
#63097 = AXIS2_PLACEMENT_3D ( 'NONE', #41663, #14543, #8246 ) ;
#63098 = DIRECTION ( 'NONE',  ( -0.3361263392814427542, 0.000000000000000000, 0.9418169057949938860 ) ) ;
#63099 = VECTOR ( 'NONE', #233, 1000.000000000000000 ) ;
#63100 = DIRECTION ( 'NONE',  ( 0.000000000000000000, 0.000000000000000000, -1.000000000000000000 ) ) ;
#63101 = FILL_AREA_STYLE_COLOUR ( '', #59333 ) ;
#63102 =( NAMED_UNIT ( * ) SI_UNIT ( $, .STERADIAN. ) SOLID_ANGLE_UNIT ( ) );
#63103 = ORIENTED_EDGE ( 'NONE', *, *, #49349, .T. ) ;
#63104 = COLOUR_RGB ( '', 0.40784314, 0.44705882, 0.49803922) ;
#63105 = CARTESIAN_POINT ( 'NONE',  ( -87.59292637653381064, -3.094860106618431139, -9.524999999999991473 ) ) ;
#63106 = ITEM_DEFINED_TRANSFORMATION ( 'NONE', 'NONE', #61853,  #42840 ) ;
#63107 = SURFACE_STYLE_USAGE ( .BOTH. , #19845 ) ;
#63108 = CARTESIAN_POINT ( 'NONE',  ( -35.00000000000003553, 10.49999999999998224, 3.000000000000000000 ) ) ;
#63109 = ADVANCED_FACE ( 'NONE', ( #48326 ), #53306, .T. ) ;
#63110 = CARTESIAN_POINT ( 'NONE',  ( -7.511572993685801073E-16, 7.000000000000000888, 0.000000000000000000 ) ) ;
#63111 = CARTESIAN_POINT ( 'NONE',  ( 0.000000000000000000, 43.00000000000000000, 0.000000000000000000 ) ) ;
#63112 = LINE ( 'NONE', #24764, #13435 ) ;
#63113 = EDGE_CURVE ( 'NONE', #63408, #17554, #44448, .T. ) ;
#63114 = AXIS2_PLACEMENT_3D ( 'NONE', #12048, #67256, #46552 ) ;
#63115 = DIRECTION ( 'NONE',  ( 0.000000000000000000, 0.000000000000000000, 1.000000000000000000 ) ) ;
#63116 = VECTOR ( 'NONE', #13303, 1000.000000000000000 ) ;
#63117 = ORIENTED_EDGE ( 'NONE', *, *, #50316, .T. ) ;
#63118 = CARTESIAN_POINT ( 'NONE',  ( 45.07697505292422591, 10.02565835097472480, -3.091949714863345910 ) ) ;
#63119 = SURFACE_STYLE_FILL_AREA ( #31093 ) ;
#63120 = ORIENTED_EDGE ( 'NONE', *, *, #21755, .T. ) ;
#63121 = CARTESIAN_POINT ( 'NONE',  ( -102.7429263765338021, -5.598654528085803328, -7.705886871421366635 ) ) ;
#63122 = CARTESIAN_POINT ( 'NONE',  ( -6.826472737025120807, 134.1070736234661638, 4.959722759717906548 ) ) ;
#63123 = DIRECTION ( 'NONE',  ( 1.000000000000000000, 0.000000000000000000, 0.000000000000000000 ) ) ;
#63124 = MECHANICAL_DESIGN_GEOMETRIC_PRESENTATION_REPRESENTATION (  '', ( #44042 ), #13659 ) ;
#63125 = ORIENTED_EDGE ( 'NONE', *, *, #8962, .T. ) ;
#63126 = CARTESIAN_POINT ( 'NONE',  ( 0.000000000000000000, 0.000000000000000000, 7.500000000000000000 ) ) ;
#63127 = CARTESIAN_POINT ( 'NONE',  ( -99.50499999999996703, -6.826472737025113702, -4.959722759717900331 ) ) ;
#63128 = UNCERTAINTY_MEASURE_WITH_UNIT (LENGTH_MEASURE( 1.000000000000000082E-05 ), #5209, 'distance_accuracy_value', 'NONE');
#63129 = CONICAL_SURFACE ( 'NONE', #28241, 3.100000000000005418, 0.7853981633974445042 ) ;
#63130 = CYLINDRICAL_SURFACE ( 'NONE', #53315, 0.9999999999999993339 ) ;
#63131 = ORIENTED_EDGE ( 'NONE', *, *, #6039, .T. ) ;
#63132 = CARTESIAN_POINT ( 'NONE',  ( -36.38551735505326690, -11.91035241884531182, 1.483988443825274617 ) ) ;
#63133 = EDGE_CURVE ( 'NONE', #14152, #63323, #8358, .T. ) ;
#63134 = CARTESIAN_POINT ( 'NONE',  ( 4.716976649647096842, 142.7429263765338305, 6.492361379858953896 ) ) ;
#63135 = EDGE_CURVE ( 'NONE', #26634, #32528, #27830, .T. ) ;
#63136 = CARTESIAN_POINT ( 'NONE',  ( 0.000000000000000000, 27.74999999999998224, 4.000000000000000000 ) ) ;
#63137 = CARTESIAN_POINT ( 'NONE',  ( -31.71532887107914789, -8.500000000000000000, 5.997393757699852834 ) ) ;
#63138 = ORIENTED_EDGE ( 'NONE', *, *, #54713, .F. ) ;
#63139 = SURFACE_SIDE_STYLE ('',( #16025 ) ) ;
#63140 = CARTESIAN_POINT ( 'NONE',  ( -76.04499999999998749, 7.632228543268600340, 2.479861379858949277 ) ) ;
#63141 = ORIENTED_EDGE ( 'NONE', *, *, #64981, .F. ) ;
#63142 = LINE ( 'NONE', #42430, #55229 ) ;
#63143 = STYLED_ITEM ( 'NONE', ( #54221 ), #46200 ) ;
#63144 = CARTESIAN_POINT ( 'NONE',  ( -121.5570736234661808, -1.166476076187852838E-15, -9.524999999999991473 ) ) ;
#63145 = ADVANCED_FACE ( 'NONE', ( #11688 ), #1560, .T. ) ;
#63146 = CIRCLE ( 'NONE', #65407, 20.42000000000000526 ) ;
#63147 = DIRECTION ( 'NONE',  ( 0.000000000000000000, 0.000000000000000000, 1.000000000000000000 ) ) ;
#63148 = ORIENTED_EDGE ( 'NONE', *, *, #48401, .F. ) ;
#63149 = CARTESIAN_POINT ( 'NONE',  ( 68.99999999999998579, 36.75000000000000000, 4.000000000000000000 ) ) ;
#63150 = DIRECTION ( 'NONE',  ( 0.000000000000000000, -0.000000000000000000, 1.000000000000000000 ) ) ;
#63151 = AXIS2_PLACEMENT_3D ( 'NONE', #30401, #31809, #58907 ) ;
#63152 = EDGE_CURVE ( 'NONE', #37934, #43795, #11336, .T. ) ;
#63153 = CARTESIAN_POINT ( 'NONE',  ( 21.75000000000001066, 22.24999999999998224, 4.000000000000000000 ) ) ;
#63154 = SPHERICAL_SURFACE ( 'NONE', #57056, 0.5000000000000000000 ) ;
#63155 = ORIENTED_EDGE ( 'NONE', *, *, #5453, .F. ) ;
#63156 = CIRCLE ( 'NONE', #28269, 18.00000000000000355 ) ;
#63157 = DIRECTION ( 'NONE',  ( -1.000000000000000000, 0.000000000000000000, 0.000000000000000000 ) ) ;
#63158 = ORIENTED_EDGE ( 'NONE', *, *, #40859, .T. ) ;
#63159 = EDGE_CURVE ( 'NONE', #20856, #22897, #3154, .T. ) ;
#63160 = CARTESIAN_POINT ( 'NONE',  ( -149.2429263765338021, 5.598654528085804216, 7.705886871421366635 ) ) ;
#63161 = CARTESIAN_POINT ( 'NONE',  ( -4.041451884327381450, -7.000000000000002665, 7.500000000000000000 ) ) ;
#63162 = CARTESIAN_POINT ( 'NONE',  ( -171.2070736234661865, 3.094860106618433360, 9.524999999999991473 ) ) ;
#63163 =( GEOMETRIC_REPRESENTATION_CONTEXT ( 3 ) GLOBAL_UNCERTAINTY_ASSIGNED_CONTEXT ( ( #64443 ) ) GLOBAL_UNIT_ASSIGNED_CONTEXT ( ( #46756, #62856, #63569 ) ) REPRESENTATION_CONTEXT ( 'NONE', 'WORKASPACE' ) );
#63164 = CARTESIAN_POINT ( 'NONE',  ( -5.598654528085806881, 127.7450000000000045, -7.705886871421374629 ) ) ;
#63165 = CARTESIAN_POINT ( 'NONE',  ( -103.5570736234661808, -1.166476076187852838E-15, -9.524999999999991473 ) ) ;
#63166 = AXIS2_PLACEMENT_3D ( 'NONE', #34573, #49388, #7507 ) ;
#63167 = EDGE_CURVE ( 'NONE', #65737, #58659, #7788, .T. ) ;
#63168 = DIRECTION ( 'NONE',  ( -0.000000000000000000, -0.000000000000000000, -1.000000000000000000 ) ) ;
#63169 = VERTEX_POINT ( 'NONE', #2462 ) ;
#63170 = PRESENTATION_STYLE_ASSIGNMENT (( #35405 ) ) ;
#63171 = CARTESIAN_POINT ( 'NONE',  ( -55.55707362346618083, -1.166476076187852838E-15, -9.524999999999991473 ) ) ;
#63172 = DIRECTION ( 'NONE',  ( 0.000000000000000000, 0.000000000000000000, -1.000000000000000000 ) ) ;
#63173 = COLOUR_RGB ( '', 0.31764706, 0.68627451, 0.89019608) ;
#63174 = CARTESIAN_POINT ( 'NONE',  ( -143.9050000000000011, 2.607480562269068880, -8.024999999999993250 ) ) ;
#63175 = FILL_AREA_STYLE_COLOUR ( '', #51634 ) ;
#63176 = AXIS2_PLACEMENT_3D ( 'NONE', #9890, #68277, #15191 ) ;
#63177 = CARTESIAN_POINT ( 'NONE',  ( -157.4950000000000045, 6.826472737025113702, -4.959722759717902107 ) ) ;
#63178 = CARTESIAN_POINT ( 'NONE',  ( -152.0949999999999420, -2.607480562269071545, -8.024999999999991473 ) ) ;
#63179 = EDGE_LOOP ( 'NONE', ( #32642, #53720, #16510, #46577, #38698, #58804, #30300, #23392, #53687, #44441, #11816, #36442, #60401, #5237, #32633, #66888, #29046, #9487, #4718, #33033, #41623, #2592, #58510, #36759, #28240, #42622, #2220, #4702, #53151, #30123, #35030, #61058, #44169, #14520, #40295, #52881, #49005, #62203, #43237, #6716, #17761, #4880, #4729, #47214, #40513, #40372 ) ) ;
#63180 = CARTESIAN_POINT ( 'NONE',  ( 44.34845674352008871, 9.782818914506675512, -3.509226550553885549 ) ) ;
#63181 =( GEOMETRIC_REPRESENTATION_CONTEXT ( 3 ) GLOBAL_UNCERTAINTY_ASSIGNED_CONTEXT ( ( #27878 ) ) GLOBAL_UNIT_ASSIGNED_CONTEXT ( ( #7861, #13139, #2541 ) ) REPRESENTATION_CONTEXT ( 'NONE', 'WORKASPACE' ) );
#63182 = CARTESIAN_POINT ( 'NONE',  ( -15.98999599679679839, 118.4999999999999716, 9.500000000000000000 ) ) ;
#63183 = CARTESIAN_POINT ( 'NONE',  ( 34.99999999999999289, 113.4999999999999858, 7.500000000000000000 ) ) ;
#63184 = CARTESIAN_POINT ( 'NONE',  ( -63.35499999999998266, -4.716976649647093289, -6.492361379858945902 ) ) ;
#63185 = DIRECTION ( 'NONE',  ( -0.000000000000000000, -0.000000000000000000, -1.000000000000000000 ) ) ;
#63186 = CIRCLE ( 'NONE', #32854, 1.000000000000000000 ) ;
#63187 = CARTESIAN_POINT ( 'NONE',  ( -65.24499999999999034, -4.716976649647093289, -6.492361379858945902 ) ) ;
#63188 = CARTESIAN_POINT ( 'NONE',  ( -3.094860106618434248, 156.9050000000000011, 9.525000000000000355 ) ) ;
#63189 = DIRECTION ( 'NONE',  ( -0.000000000000000000, -1.000000000000000000, -0.000000000000000000 ) ) ;
#63190 = AXIS2_PLACEMENT_3D ( 'NONE', #15185, #16216, #42965 ) ;
#63191 = PRESENTATION_LAYER_ASSIGNMENT (  '', '', ( #17127 ) ) ;
#63192 = SURFACE_STYLE_FILL_AREA ( #20267 ) ;
#63193 = CARTESIAN_POINT ( 'NONE',  ( -152.0929263765342512, 3.094860106625323404, 9.524999999994985700 ) ) ;
#63194 = ADVANCED_FACE ( 'NONE', ( #2098 ), #13409, .F. ) ;
#63195 = PRESENTATION_LAYER_ASSIGNMENT (  '', '', ( #49744 ) ) ;
#63196 = DIRECTION ( 'NONE',  ( -0.000000000000000000, -0.000000000000000000, -1.000000000000000000 ) ) ;
#63197 = CARTESIAN_POINT ( 'NONE',  ( 0.000000000000000000, 114.9999999999999574, 0.000000000000000000 ) ) ;
#63198 = SURFACE_SIDE_STYLE ('',( #8359 ) ) ;
#63199 =( NAMED_UNIT ( * ) PLANE_ANGLE_UNIT ( ) SI_UNIT ( $, .RADIAN. ) );
#63200 = PRESENTATION_STYLE_ASSIGNMENT (( #24493 ) ) ;
#63201 = CARTESIAN_POINT ( 'NONE',  ( -75.33578643762689353, -4.000000000000000000, 18.58578643762690419 ) ) ;
#63202 = ORIENTED_EDGE ( 'NONE', *, *, #39843, .T. ) ;
#63203 = ORIENTED_EDGE ( 'NONE', *, *, #26199, .T. ) ;
#63204 = DIRECTION ( 'NONE',  ( 8.705236002253083981E-17, -0.7431448254773934670, 0.6691306063588592368 ) ) ;
#63205 = TOROIDAL_SURFACE ( 'NONE', #18269, 9.500000000000005329, 0.5000000000000000000 ) ;
#63206 = SURFACE_SIDE_STYLE ('',( #13614 ) ) ;
#63207 = EDGE_CURVE ( 'NONE', #34526, #9180, #2367, .T. ) ;
#63208 = CARTESIAN_POINT ( 'NONE',  ( 0.7098900097155632638, -7.000000000000000888, -2.373649839567916678E-14 ) ) ;
#63209 = DIRECTION ( 'NONE',  ( 0.000000000000000000, 0.000000000000000000, -1.000000000000000000 ) ) ;
#63210 = SURFACE_SIDE_STYLE ('',( #41792 ) ) ;
#63211 = ORIENTED_EDGE ( 'NONE', *, *, #23304, .F. ) ;
#63212 = EDGE_LOOP ( 'NONE', ( #30578, #34909, #23533, #20906 ) ) ;
#63213 = STYLED_ITEM ( 'NONE', ( #9778 ), #7080 ) ;
#63214 = DIRECTION ( 'NONE',  ( 1.000000000000000000, 0.000000000000000000, 0.000000000000000000 ) ) ;
#63215 = FACE_OUTER_BOUND ( 'NONE', #55982, .T. ) ;
#63216 = EDGE_CURVE ( 'NONE', #59935, #48045, #34209, .T. ) ;
#63217 = AXIS2_PLACEMENT_3D ( 'NONE', #21466, #22512, #11256 ) ;
#63218 = VERTEX_POINT ( 'NONE', #61945 ) ;
#63219 = EDGE_CURVE ( 'NONE', #19879, #47797, #18005, .T. ) ;
#63220 = CARTESIAN_POINT ( 'NONE',  ( 0.000000000000000000, 119.5549999999999926, -9.525000000000000355 ) ) ;
#63221 = CARTESIAN_POINT ( 'NONE',  ( -84.59292637653378222, -3.094860106618431139, -9.524999999999991473 ) ) ;
#63222 = CIRCLE ( 'NONE', #55324, 4.499999999999997335 ) ;
#63223 = DIRECTION ( 'NONE',  ( 0.000000000000000000, 0.000000000000000000, -1.000000000000000000 ) ) ;
#63224 = CARTESIAN_POINT ( 'NONE',  ( -105.7449999999999903, 4.716976649647094177, 6.492361379858945902 ) ) ;
#63225 = VERTEX_POINT ( 'NONE', #56686 ) ;
#63226 = VECTOR ( 'NONE', #64805, 1000.000000000000000 ) ;
#63227 = CARTESIAN_POINT ( 'NONE',  ( -163.7070736234664139, -3.094860106622296936, -9.524999999997184830 ) ) ;
#63228 = EDGE_CURVE ( 'NONE', #7688, #31048, #33825, .T. ) ;
#63229 = ORIENTED_EDGE ( 'NONE', *, *, #36524, .T. ) ;
#63230 = CARTESIAN_POINT ( 'NONE',  ( -6.826472737025120807, 150.9929263765338305, 4.959722759717906548 ) ) ;
#63231 = DIRECTION ( 'NONE',  ( 0.000000000000000000, 0.000000000000000000, 1.000000000000000000 ) ) ;
#63232 = AXIS2_PLACEMENT_3D ( 'NONE', #9880, #25344, #13753 ) ;
#63233 = EDGE_CURVE ( 'NONE', #18424, #62171, #67586, .T. ) ;
#63234 = VERTEX_POINT ( 'NONE', #7460 ) ;
#63235 = ORIENTED_EDGE ( 'NONE', *, *, #69485, .T. ) ;
#63236 = SURFACE_STYLE_USAGE ( .BOTH. , #36555 ) ;
#63237 = COLOUR_RGB ( '', 0.08235294, 0.09019608, 0.10196078) ;
#63239 = CARTESIAN_POINT ( 'NONE',  ( -119.4549999999999983, 7.632228543268599452, -2.479861379858951942 ) ) ;
#63238 = VECTOR ( 'NONE', #32930, 1000.000000000000000 ) ;
#63240 = CARTESIAN_POINT ( 'NONE',  ( 12.72792206135785698, 114.9999999999999574, 10.50000000000000000 ) ) ;
#63241 = CARTESIAN_POINT ( 'NONE',  ( 7.632228543268608334, 141.4570736234661581, -2.479861379858951942 ) ) ;
#63242 =( NAMED_UNIT ( * ) PLANE_ANGLE_UNIT ( ) SI_UNIT ( $, .RADIAN. ) );
#63243 = AXIS2_PLACEMENT_3D ( 'NONE', #68872, #41453, #24886 ) ;
#63244 = CARTESIAN_POINT ( 'NONE',  ( 24.21231517720798010, 117.4999999999999716, -7.000000000000000000 ) ) ;
#63245 = DIRECTION ( 'NONE',  ( -0.000000000000000000, -0.000000000000000000, -1.000000000000000000 ) ) ;
#63246 = DIRECTION ( 'NONE',  ( 0.000000000000000000, 0.000000000000000000, -1.000000000000000000 ) ) ;
#63247 = ORIENTED_EDGE ( 'NONE', *, *, #2861, .F. ) ;
#63248 = VERTEX_POINT ( 'NONE', #23287 ) ;
#63249 = FACE_OUTER_BOUND ( 'NONE', #7681, .T. ) ;
#63250 = CARTESIAN_POINT ( 'NONE',  ( -182.9194972100727625, 8.570615872132687940, -4.445904112569770916 ) ) ;
#63251 = CARTESIAN_POINT ( 'NONE',  ( 48.50000000000000000, 14.49137674618942562, -10.00000000000000000 ) ) ;
#63252 = ORIENTED_EDGE ( 'NONE', *, *, #3354, .F. ) ;
#63253 = FACE_OUTER_BOUND ( 'NONE', #35620, .T. ) ;
#63254 = CARTESIAN_POINT ( 'NONE',  ( -178.4050000000000011, -2.607480562269069768, 8.024999999999991473 ) ) ;
#63255 = LINE ( 'NONE', #52382, #10513 ) ;
#63256 = EDGE_CURVE ( 'NONE', #23604, #51230, #2672, .T. ) ;
#63257 = AXIS2_PLACEMENT_3D ( 'NONE', #47530, #68944, #26680 ) ;
#63258 = CARTESIAN_POINT ( 'NONE',  ( -181.0449999999999875, 7.632228543268600340, 2.479861379858949277 ) ) ;
#63259 = CIRCLE ( 'NONE', #17251, 0.2500000000000002220 ) ;
#63260 = CARTESIAN_POINT ( 'NONE',  ( -173.3949999999999818, -6.826472737025113702, -4.959722759717900331 ) ) ;
#63261 = EDGE_CURVE ( 'NONE', #360, #44696, #14126, .T. ) ;
#63262 = ORIENTED_EDGE ( 'NONE', *, *, #45899, .T. ) ;
#63263 = AXIS2_PLACEMENT_3D ( 'NONE', #53466, #48218, #21096 ) ;
#63264 = SURFACE_STYLE_FILL_AREA ( #57642 ) ;
#63265 = DIRECTION ( 'NONE',  ( 0.000000000000000000, 1.000000000000000000, 1.224646799147352961E-16 ) ) ;
#63266 = CARTESIAN_POINT ( 'NONE',  ( -11.03071027638185697, 11.60717996540982888, 3.057800190812369312 ) ) ;
#63267 = CARTESIAN_POINT ( 'NONE',  ( -87.80500000000000682, -8.437984349512085203, 5.166775262442717831E-16 ) ) ;
#63268 =( NAMED_UNIT ( * ) SI_UNIT ( $, .STERADIAN. ) SOLID_ANGLE_UNIT ( ) );
#63269 = SURFACE_STYLE_FILL_AREA ( #29864 ) ;
#63270 = VECTOR ( 'NONE', #4266, 1000.000000000000000 ) ;
#63271 = VECTOR ( 'NONE', #37732, 1000.000000000000000 ) ;
#63272 = CARTESIAN_POINT ( 'NONE',  ( -93.44499999999999318, 0.000000000000000000, 8.024999999999991473 ) ) ;
#63273 = CARTESIAN_POINT ( 'NONE',  ( -10.01517768586949231, 123.3049999999999926, -6.132527647946036459E-16 ) ) ;
#63274 = CARTESIAN_POINT ( 'NONE',  ( -68.39499999999999602, -6.826472737025115478, -4.959722759717899443 ) ) ;
#63275 = DIRECTION ( 'NONE',  ( -1.000000000000000000, -0.000000000000000000, -0.000000000000000000 ) ) ;
#63276 = FACE_OUTER_BOUND ( 'NONE', #51310, .T. ) ;
#63277 = CARTESIAN_POINT ( 'NONE',  ( 1.999798566743339334, 49.09558629977726696, 2.000000000000000000 ) ) ;
#63278 =( NAMED_UNIT ( * ) PLANE_ANGLE_UNIT ( ) SI_UNIT ( $, .RADIAN. ) );
#63279 = EDGE_LOOP ( 'NONE', ( #37936, #49206, #11377, #10886 ) ) ;
#63280 = CARTESIAN_POINT ( 'NONE',  ( -105.5929263765338106, -3.094860106618431139, -9.524999999999991473 ) ) ;
#63281 = CARTESIAN_POINT ( 'NONE',  ( -132.8950000000000102, 6.826472737025116366, 4.959722759717898555 ) ) ;
#63282 = CARTESIAN_POINT ( 'NONE',  ( -6.826472737025120807, 145.5070736234661410, -4.959722759717907437 ) ) ;
#63283 = B_SPLINE_CURVE_WITH_KNOTS ( 'NONE', 3,
 ( #49153, #60021, #33637, #17149, #28331, #6216 ),
 .UNSPECIFIED., .F., .F.,
 ( 4, 2, 4 ),
 ( 0.005386537104126977275, 0.008060814333094818568, 0.01073509156206266073 ),
 .UNSPECIFIED. ) ;
#63284 = ADVANCED_FACE ( 'NONE', ( #68631 ), #3882, .T. ) ;
#63286 = CARTESIAN_POINT ( 'NONE',  ( -72.00000000000000000, 14.49137674618942562, -10.00000000000000000 ) ) ;
#63285 = CARTESIAN_POINT ( 'NONE',  ( -130.9429263765338192, 0.000000000000000000, 9.524999999999991473 ) ) ;
#63287 =( NAMED_UNIT ( * ) PLANE_ANGLE_UNIT ( ) SI_UNIT ( $, .RADIAN. ) );
#63288 = VERTEX_POINT ( 'NONE', #62305 ) ;
#63290 = ORIENTED_EDGE ( 'NONE', *, *, #69580, .T. ) ;
#63289 = PRESENTATION_LAYER_ASSIGNMENT (  '', '', ( #39708 ) ) ;
#63291 = CARTESIAN_POINT ( 'NONE',  ( -174.9570736234661865, 9.058813317711329915, -2.943386871421373119 ) ) ;
#63292 = AXIS2_PLACEMENT_3D ( 'NONE', #20859, #42012, #42699 ) ;
#63293 = ADVANCED_FACE ( 'NONE', ( #36308, #41937 ), #4584, .F. ) ;
#63294 = CYLINDRICAL_SURFACE ( 'NONE', #58585, 3.499999999999999556 ) ;
#63295 = CARTESIAN_POINT ( 'NONE',  ( 7.750000000000000000, 33.74999999999998579, -3.750000000000000000 ) ) ;
#63296 = CARTESIAN_POINT ( 'NONE',  ( -9.984889265949528081, -1.515110734050472141, 0.7056644834263087196 ) ) ;
#63297 = ORIENTED_EDGE ( 'NONE', *, *, #54693, .F. ) ;
#63298 = CARTESIAN_POINT ( 'NONE',  ( -120.2049999999999983, -2.607480562269071545, -8.024999999999991473 ) ) ;
#63299 = ORIENTED_EDGE ( 'NONE', *, *, #243, .T. ) ;
#63300 = CARTESIAN_POINT ( 'NONE',  ( -137.0070736234661410, -8.102448949553174629, -5.886773742842741797 ) ) ;
#63301 = ADVANCED_FACE ( 'NONE', ( #57025 ), #35586, .T. ) ;
#63302 = VECTOR ( 'NONE', #42745, 1000.000000000000000 ) ;
#63303 = ORIENTED_EDGE ( 'NONE', *, *, #34655, .F. ) ;
#63304 = SURFACE_STYLE_FILL_AREA ( #9850 ) ;
#63305 = FILL_AREA_STYLE ('',( #47885 ) ) ;
#63306 = ORIENTED_EDGE ( 'NONE', *, *, #63207, .F. ) ;
#63307 = PRESENTATION_LAYER_ASSIGNMENT (  '', '', ( #57688 ) ) ;
#63308 = CARTESIAN_POINT ( 'NONE',  ( -3.094860106618432471, 148.5949999999999704, -9.525000000000000355 ) ) ;
#63309 = LINE ( 'NONE', #36631, #9339 ) ;
#63310 = PRESENTATION_LAYER_ASSIGNMENT (  '', '', ( #66676 ) ) ;
#63311 = ORIENTED_EDGE ( 'NONE', *, *, #28307, .T. ) ;
#63312 = DIRECTION ( 'NONE',  ( 0.000000000000000000, 1.000000000000000000, 0.000000000000000000 ) ) ;
#63313 = CARTESIAN_POINT ( 'NONE',  ( -8.102448949553179958, 147.0049999999999955, -5.886773742842749790 ) ) ;
#63314 = ORIENTED_EDGE ( 'NONE', *, *, #16069, .F. ) ;
#63315 = CARTESIAN_POINT ( 'NONE',  ( -2.607480562269075097, 127.2929263765337993, 8.025000000000000355 ) ) ;
#63316 = DIRECTION ( 'NONE',  ( 0.000000000000000000, 1.000000000000000000, 0.000000000000000000 ) ) ;
#63317 = ADVANCED_FACE ( 'NONE', ( #4946 ), #8842, .F. ) ;
#63318 =( GEOMETRIC_REPRESENTATION_CONTEXT ( 3 ) GLOBAL_UNCERTAINTY_ASSIGNED_CONTEXT ( ( #14508 ) ) GLOBAL_UNIT_ASSIGNED_CONTEXT ( ( #22104, #10857, #5906 ) ) REPRESENTATION_CONTEXT ( 'NONE', 'WORKASPACE' ) );
#63319 = FACE_OUTER_BOUND ( 'NONE', #24796, .T. ) ;
#63320 = FACE_OUTER_BOUND ( 'NONE', #19622, .T. ) ;
#63321 = ORIENTED_EDGE ( 'NONE', *, *, #31616, .F. ) ;
#63322 = CARTESIAN_POINT ( 'NONE',  ( -40.78947368421051323, 108.1536491499103505, -3.157942443983132730 ) ) ;
#63323 = VERTEX_POINT ( 'NONE', #63345 ) ;
#63324 = CARTESIAN_POINT ( 'NONE',  ( -62.99292637653378080, 8.102448949553171076, -5.886773742842744461 ) ) ;
#63325 = DIRECTION ( 'NONE',  ( 0.000000000000000000, -0.000000000000000000, 1.000000000000000000 ) ) ;
#63326 = DIRECTION ( 'NONE',  ( 0.000000000000000000, 0.000000000000000000, 1.000000000000000000 ) ) ;
#63327 = CARTESIAN_POINT ( 'NONE',  ( -156.2050000000000125, -2.607480562269071545, -8.024999999999991473 ) ) ;
#63328 = ORIENTED_EDGE ( 'NONE', *, *, #19846, .F. ) ;
#63329 = MECHANICAL_DESIGN_GEOMETRIC_PRESENTATION_REPRESENTATION (  '', ( #21750 ), #10515 ) ;
#63330 = LINE ( 'NONE', #26379, #56612 ) ;
#63331 = CARTESIAN_POINT ( 'NONE',  ( -65.00000000000000000, -1.962809905030629631E-14, 6.999999999999995559 ) ) ;
#63332 = CARTESIAN_POINT ( 'NONE',  ( -69.74292637653380211, -5.598654528085803328, -7.705886871421366635 ) ) ;
#63333 = SURFACE_STYLE_FILL_AREA ( #68975 ) ;
#63334 = ORIENTED_EDGE ( 'NONE', *, *, #15128, .T. ) ;
#63335 = ORIENTED_EDGE ( 'NONE', *, *, #25038, .T. ) ;
#63336 = CARTESIAN_POINT ( 'NONE',  ( -66.49999999999998579, 50.00000000000000000, -11.50000000000000000 ) ) ;
#63337 = CARTESIAN_POINT ( 'NONE',  ( 24.00000000000000000, 1.000000000000000000, 4.000000000000000000 ) ) ;
#63339 = CARTESIAN_POINT ( 'NONE',  ( -63.80499999999998550, -8.437984349512085203, 5.166775262442717831E-16 ) ) ;
#63338 = AXIS2_PLACEMENT_3D ( 'NONE', #32970, #12524, #39648 ) ;
#63340 = ORIENTED_EDGE ( 'NONE', *, *, #16783, .T. ) ;
#63341 = DIRECTION ( 'NONE',  ( -0.000000000000000000, -1.000000000000000000, -0.000000000000000000 ) ) ;
#63342 =( GEOMETRIC_REPRESENTATION_CONTEXT ( 3 ) GLOBAL_UNCERTAINTY_ASSIGNED_CONTEXT ( ( #120 ) ) GLOBAL_UNIT_ASSIGNED_CONTEXT ( ( #23829, #34715, #24172 ) ) REPRESENTATION_CONTEXT ( 'NONE', 'WORKASPACE' ) );
#63343 =( GEOMETRIC_REPRESENTATION_CONTEXT ( 3 ) GLOBAL_UNCERTAINTY_ASSIGNED_CONTEXT ( ( #38310 ) ) GLOBAL_UNIT_ASSIGNED_CONTEXT ( ( #36946, #68236, #31620 ) ) REPRESENTATION_CONTEXT ( 'NONE', 'WORKASPACE' ) );
#63344 = CARTESIAN_POINT ( 'NONE',  ( 35.99999999999999289, 5.000000000000000000, -24.00402776293825369 ) ) ;
#63345 = CARTESIAN_POINT ( 'NONE',  ( 22.25000000000000711, 33.99999999999999289, -3.750000000000000000 ) ) ;
#63346 = ORIENTED_EDGE ( 'NONE', *, *, #20920, .T. ) ;
#63347 = MECHANICAL_DESIGN_GEOMETRIC_PRESENTATION_REPRESENTATION (  '', ( #26123 ), #12759 ) ;
#63348 = CARTESIAN_POINT ( 'NONE',  ( 4.750000000000002665, 24.74999999999998579, 3.750000000000000000 ) ) ;
#63349 = LINE ( 'NONE', #297, #26032 ) ;
#63350 = DIRECTION ( 'NONE',  ( 0.000000000000000000, 0.000000000000000000, 1.000000000000000000 ) ) ;
#63351 = DIRECTION ( 'NONE',  ( 0.000000000000000000, 1.000000000000000000, -0.000000000000000000 ) ) ;
#63352 = CARTESIAN_POINT ( 'NONE',  ( 5.598654528085809545, 148.1450000000000102, -7.705886871421373741 ) ) ;
#63353 = CARTESIAN_POINT ( 'NONE',  ( -100.7950000000000017, 2.607480562269068880, -8.024999999999993250 ) ) ;
#63354 = CARTESIAN_POINT ( 'NONE',  ( 44.99999999999998579, 119.9999999999999716, -9.500000000000000000 ) ) ;
#63355 = AXIS2_PLACEMENT_3D ( 'NONE', #50871, #2628, #56483 ) ;
#63356 = DIRECTION ( 'NONE',  ( 1.000000000000000000, -0.000000000000000000, 2.592503555346955593E-15 ) ) ;
#63357 =( BOUNDED_CURVE ( )  B_SPLINE_CURVE ( 2, ( #62479, #7982, #40718, #55819, #12906, #66368, #34699, #51589, #9031, #13593, #50558 ),
 .UNSPECIFIED., .F., .F. ) 
 B_SPLINE_CURVE_WITH_KNOTS ( ( 3, 2, 2, 2, 2, 3 ),
 ( 0.1195652173913016036, 0.1217391304347798103, 0.1239130434782580309, 0.1260869565217362376, 0.1282608695652144581, 0.1304347826086926510 ),
 .UNSPECIFIED. ) 
 CURVE ( )  GEOMETRIC_REPRESENTATION_ITEM ( )  RATIONAL_B_SPLINE_CURVE ( ( 1.000000000000061728, 0.9510565162950915807, 1.000000000000000000, 0.9510565162951535312, 1.000000000000000000, 0.9510565162951535312, 1.000000000000000000, 0.9510565162951535312, 1.000000000000000000, 0.9510565162952210327, 0.9999999999999324984 ) ) 
 REPRESENTATION_ITEM ( '' )  );
#63358 = STYLED_ITEM ( 'NONE', ( #778 ), #56073 ) ;
#63359 = CARTESIAN_POINT ( 'NONE',  ( 0.000000000000000000, 143.9429263765338192, -8.025000000000000355 ) ) ;
#63360 = VERTEX_POINT ( 'NONE', #41230 ) ;
#63361 = CARTESIAN_POINT ( 'NONE',  ( -134.8429263765337964, 9.058813317711329915, -2.943386871421373119 ) ) ;
#63362 = AXIS2_PLACEMENT_3D ( 'NONE', #63354, #14464, #4598 ) ;
#63363 = CARTESIAN_POINT ( 'NONE',  ( -33.02102729337801890, -9.244539245506066649, -2.264342667812435206 ) ) ;
#63364 = CARTESIAN_POINT ( 'NONE',  ( -156.7450000000000045, 4.716976649647094177, 6.492361379858945902 ) ) ;
#63365 = CYLINDRICAL_SURFACE ( 'NONE', #17833, 14.00000000000001243 ) ;
#63366 =( GEOMETRIC_REPRESENTATION_CONTEXT ( 3 ) GLOBAL_UNCERTAINTY_ASSIGNED_CONTEXT ( ( #51819 ) ) GLOBAL_UNIT_ASSIGNED_CONTEXT ( ( #52654, #56884, #9046 ) ) REPRESENTATION_CONTEXT ( 'NONE', 'WORKASPACE' ) );
#63367 = DIRECTION ( 'NONE',  ( 0.000000000000000000, -1.000000000000000000, 0.000000000000000000 ) ) ;
#63368 = EDGE_CURVE ( 'NONE', #32850, #27009, #16272, .T. ) ;
#63369 = DIRECTION ( 'NONE',  ( -1.000000000000000000, -1.445602896647337931E-16, 0.000000000000000000 ) ) ;
#63370 = DIRECTION ( 'NONE',  ( 1.000000000000000000, 0.000000000000000000, 0.000000000000000000 ) ) ;
#63371 = ORIENTED_EDGE ( 'NONE', *, *, #58951, .T. ) ;
#63373 = VERTEX_POINT ( 'NONE', #68986 ) ;
#63372 = PRESENTATION_LAYER_ASSIGNMENT (  '', '', ( #24054 ) ) ;
#63374 = CARTESIAN_POINT ( 'NONE',  ( -74.99999999999998579, 50.00000000000000000, 7.500000000000000000 ) ) ;
#63375 = AXIS2_PLACEMENT_3D ( 'NONE', #5757, #69128, #20581 ) ;
#63376 = FACE_OUTER_BOUND ( 'NONE', #17651, .T. ) ;
#63377 = CARTESIAN_POINT ( 'NONE',  ( -45.00000000000000000, 8.253551290271557761, 5.607507417892153789 ) ) ;
#63378 = CARTESIAN_POINT ( 'NONE',  ( 44.64649554404039122, 9.999999999999978684, 3.314804571885168638 ) ) ;
#63379 = FACE_OUTER_BOUND ( 'NONE', #2046, .T. ) ;
#63380 = VERTEX_POINT ( 'NONE', #67952 ) ;
#63381 = CARTESIAN_POINT ( 'NONE',  ( -147.3549999999999898, -4.716976649647093289, -6.492361379858945902 ) ) ;
#63382 = AXIS2_PLACEMENT_3D ( 'NONE', #6400, #382, #1055 ) ;
#63383 = EDGE_CURVE ( 'NONE', #46789, #64160, #69018, .T. ) ;
#63384 = ORIENTED_EDGE ( 'NONE', *, *, #27860, .F. ) ;
#63385 = CARTESIAN_POINT ( 'NONE',  ( 4.682380833558962507, 5.889878495889167453, 0.4967607073414696539 ) ) ;
#63386 = CARTESIAN_POINT ( 'NONE',  ( -141.8070736234661808, 10.01517768586948698, -1.839758294383808966E-15 ) ) ;
#63388 = ORIENTED_EDGE ( 'NONE', *, *, #66373, .F. ) ;
#63387 = EDGE_CURVE ( 'NONE', #28627, #42069, #47736, .T. ) ;
#63389 = MECHANICAL_DESIGN_GEOMETRIC_PRESENTATION_REPRESENTATION (  '', ( #4982 ), #12816 ) ;
#63390 = PRESENTATION_LAYER_ASSIGNMENT (  '', '', ( #39830 ) ) ;
#63391 = CARTESIAN_POINT ( 'NONE',  ( 3.499999999999999112, 34.24999999999998579, -4.000000000000000000 ) ) ;
#63392 = EDGE_CURVE ( 'NONE', #65027, #13063, #42299, .T. ) ;
#63393 =( LENGTH_UNIT ( ) NAMED_UNIT ( * ) SI_UNIT ( .MILLI., .METRE. ) );
#63394 = CARTESIAN_POINT ( 'NONE',  ( -3.094860106618434248, 125.7949999999999733, 9.525000000000000355 ) ) ;
#63395 = DIRECTION ( 'NONE',  ( 0.000000000000000000, 0.000000000000000000, 1.000000000000000000 ) ) ;
#63396 = ORIENTED_EDGE ( 'NONE', *, *, #6756, .F. ) ;
#63397 = CARTESIAN_POINT ( 'NONE',  ( -4.683753779217435742, 5.887500484252664812, 0.4948905776603345075 ) ) ;
#63399 = EDGE_CURVE ( 'NONE', #54282, #19551, #56659, .T. ) ;
#63398 = CARTESIAN_POINT ( 'NONE',  ( -1.166476076187854022E-15, 121.0549999999999784, 9.525000000000000355 ) ) ;
#63400 = CARTESIAN_POINT ( 'NONE',  ( -60.50499999999998124, -6.826472737025113702, -4.959722759717900331 ) ) ;
#63401 = FILL_AREA_STYLE ('',( #20484 ) ) ;
#63402 = ORIENTED_EDGE ( 'NONE', *, *, #16332, .T. ) ;
#63403 = CARTESIAN_POINT ( 'NONE',  ( -8.102448949553181734, 150.6050000000000182, 5.886773742842747126 ) ) ;
#63404 = DIRECTION ( 'NONE',  ( 0.000000000000000000, 1.000000000000000000, 0.000000000000000000 ) ) ;
#63405 = DIRECTION ( 'NONE',  ( -1.000000000000000000, 0.000000000000000000, 0.000000000000000000 ) ) ;
#63406 = VECTOR ( 'NONE', #13354, 1000.000000000000000 ) ;
#63407 = CARTESIAN_POINT ( 'NONE',  ( 0.000000000000000000, 18.74999999999997868, 4.000000000000000000 ) ) ;
#63408 = VERTEX_POINT ( 'NONE', #58411 ) ;
#63409 = SURFACE_STYLE_USAGE ( .BOTH. , #15256 ) ;
#63411 = CARTESIAN_POINT ( 'NONE',  ( 74.65811388300841145, 19.88603796100278487, -6.000000000000000000 ) ) ;
#63410 = PRESENTATION_LAYER_ASSIGNMENT (  '', '', ( #37647 ) ) ;
#63412 = CARTESIAN_POINT ( 'NONE',  ( 15.48999599679679662, 146.9999999999999716, -9.500000000000000000 ) ) ;
#63413 = CARTESIAN_POINT ( 'NONE',  ( -177.0549999999999784, -9.827790563157499189E-16, -8.024999999999991473 ) ) ;
#63414 = ORIENTED_EDGE ( 'NONE', *, *, #485, .T. ) ;
#63415 = CARTESIAN_POINT ( 'NONE',  ( 1.085428990800034299, 110.8977621029158769, 9.078527738363955990 ) ) ;
#63416 = AXIS2_PLACEMENT_3D ( 'NONE', #58892, #59561, #37129 ) ;
#63417 = AXIS2_PLACEMENT_3D ( 'NONE', #35509, #58334, #58015 ) ;
#63418 = DIRECTION ( 'NONE',  ( 0.000000000000000000, 0.000000000000000000, -1.000000000000000000 ) ) ;
#63419 = EDGE_LOOP ( 'NONE', ( #2952, #47084, #31543, #20098 ) ) ;
#63420 = DIRECTION ( 'NONE',  ( 0.000000000000000000, 0.000000000000000000, -1.000000000000000000 ) ) ;
#63421 = FILL_AREA_STYLE ('',( #9271 ) ) ;
#63422 = ORIENTED_EDGE ( 'NONE', *, *, #1733, .T. ) ;
#63423 = SURFACE_SIDE_STYLE ('',( #15601 ) ) ;
#63424 = CIRCLE ( 'NONE', #2706, 0.2500000000000002220 ) ;
#63425 = CARTESIAN_POINT ( 'NONE',  ( 66.74999999999998579, 37.00000000000000000, -3.750000000000000000 ) ) ;
#63426 = CARTESIAN_POINT ( 'NONE',  ( -99.20499999999999829, -2.607480562269071545, -8.024999999999991473 ) ) ;
#63427 = ORIENTED_EDGE ( 'NONE', *, *, #10119, .T. ) ;
#63428 = DIRECTION ( 'NONE',  ( -0.000000000000000000, -0.000000000000000000, 1.000000000000000000 ) ) ;
#63429 = SURFACE_STYLE_FILL_AREA ( #42021 ) ;
#63430 = CARTESIAN_POINT ( 'NONE',  ( -134.1570736234661751, -9.058813317711329915, -2.943386871421370898 ) ) ;
#63431 = CARTESIAN_POINT ( 'NONE',  ( -10.01517768586949408, 149.1949999999999932, -6.132527647946036459E-16 ) ) ;
#63432 = CARTESIAN_POINT ( 'NONE',  ( -71.15707362346617515, -9.058813317711329915, -2.943386871421370898 ) ) ;
#63433 = MECHANICAL_DESIGN_GEOMETRIC_PRESENTATION_REPRESENTATION (  '', ( #30821 ), #56701 ) ;
#63434 =( GEOMETRIC_REPRESENTATION_CONTEXT ( 3 ) GLOBAL_UNCERTAINTY_ASSIGNED_CONTEXT ( ( #36292 ) ) GLOBAL_UNIT_ASSIGNED_CONTEXT ( ( #7679, #52008, #51646 ) ) REPRESENTATION_CONTEXT ( 'NONE', 'WORKASPACE' ) );
#63435 = LINE ( 'NONE', #51485, #51597 ) ;
#63436 = EDGE_LOOP ( 'NONE', ( #65089, #3267, #51888 ) ) ;
#63437 = CARTESIAN_POINT ( 'NONE',  ( -4.000000000000000000, -2.499999999999999556, 24.00000000000000000 ) ) ;
#63438 = CARTESIAN_POINT ( 'NONE',  ( -48.50000000000000000, 14.49137674618942562, 7.500000000000000000 ) ) ;
#63439 = AXIS2_PLACEMENT_3D ( 'NONE', #10919, #48597, #59423 ) ;
#63440 = CARTESIAN_POINT ( 'NONE',  ( -115.5549999999999926, 0.000000000000000000, 8.024999999999991473 ) ) ;
#63441 = LINE ( 'NONE', #15288, #40462 ) ;
#63442 = CARTESIAN_POINT ( 'NONE',  ( 3.094860106618435136, 115.2949999999999733, -9.525000000000000355 ) ) ;
#63443 = CARTESIAN_POINT ( 'NONE',  ( -127.3449999999999847, 7.632228543268599452, -2.479861379858951942 ) ) ;
#63444 = CIRCLE ( 'NONE', #67929, 9.000000000000000000 ) ;
#63445 = CARTESIAN_POINT ( 'NONE',  ( -112.1070736234661354, 8.102448949553172852, -5.886773742842744461 ) ) ;
#63446 = ORIENTED_EDGE ( 'NONE', *, *, #6901, .T. ) ;
#63447 = CARTESIAN_POINT ( 'NONE',  ( -158.8429263765337964, 9.058813317711329915, -2.943386871421373119 ) ) ;
#63448 =( NAMED_UNIT ( * ) PLANE_ANGLE_UNIT ( ) SI_UNIT ( $, .RADIAN. ) );
#63449 = CARTESIAN_POINT ( 'NONE',  ( -182.6949999999999648, -8.437984349512085203, 5.166775262442717831E-16 ) ) ;
#63450 = CIRCLE ( 'NONE', #12872, 13.99999999999999822 ) ;
#63451 = FACE_BOUND ( 'NONE', #45292, .T. ) ;
#63452 = CIRCLE ( 'NONE', #33278, 0.5000000000000004441 ) ;
#63453 = ADVANCED_FACE ( 'NONE', ( #31674 ), #30266, .T. ) ;
#63454 = CARTESIAN_POINT ( 'NONE',  ( -20.30121256018846765, 114.9093931177592509, -10.36597400192487939 ) ) ;
#63455 = DIRECTION ( 'NONE',  ( 0.000000000000000000, 1.000000000000000000, 0.000000000000000000 ) ) ;
#63456 = PRESENTATION_STYLE_ASSIGNMENT (( #58518 ) ) ;
#63457 = VERTEX_POINT ( 'NONE', #62989 ) ;
#63458 = CARTESIAN_POINT ( 'NONE',  ( -78.44292637653380496, -1.166476076187852838E-15, -9.524999999999991473 ) ) ;
#63459 = ITEM_DEFINED_TRANSFORMATION ( 'NONE', 'NONE', #2239,  #42840 ) ;
#63460 = VECTOR ( 'NONE', #31715, 1000.000000000000000 ) ;
#63462 = EDGE_CURVE ( 'NONE', #52251, #36619, #52214, .T. ) ;
#63461 = DIRECTION ( 'NONE',  ( -1.156482317317870344E-15, 1.000000000000000000, 0.000000000000000000 ) ) ;
#63463 =( BOUNDED_CURVE ( )  B_SPLINE_CURVE ( 2, ( #19152, #7918, #24100, #45607, #61703, #34314, #67356, #55768, #40653, #35002, #29361 ),
 .UNSPECIFIED., .F., .F. ) 
 B_SPLINE_CURVE_WITH_KNOTS ( ( 3, 2, 2, 2, 2, 3 ),
 ( 0.8695652173913043237, 0.8717391304347825720, 0.8739130434782608203, 0.8760869565217391797, 0.8782608695652174280, 0.8804347826086956763 ),
 .UNSPECIFIED. ) 
 CURVE ( )  GEOMETRIC_REPRESENTATION_ITEM ( )  RATIONAL_B_SPLINE_CURVE ( ( 1.000000000000000000, 0.9510565162951535312, 1.000000000000000000, 0.9510565162951535312, 1.000000000000000000, 0.9510565162951535312, 1.000000000000000000, 0.9510565162951535312, 1.000000000000000000, 0.9510565162951535312, 1.000000000000000000 ) ) 
 REPRESENTATION_ITEM ( '' )  );
#63464 = CARTESIAN_POINT ( 'NONE',  ( 1.000000000000000000, 43.00000000000000000, -79.00402776293826435 ) ) ;
#63465 = VECTOR ( 'NONE', #127, 1000.000000000000000 ) ;
#63466 = CARTESIAN_POINT ( 'NONE',  ( -178.7050000000000125, 2.607480562269072433, 8.024999999999991473 ) ) ;
#63467 = EDGE_LOOP ( 'NONE', ( #21780, #52800, #46417 ) ) ;
#63468 =( LENGTH_UNIT ( ) NAMED_UNIT ( * ) SI_UNIT ( .MILLI., .METRE. ) );
#63469 = LINE ( 'NONE', #38154, #60072 ) ;
#63470 = EDGE_CURVE ( 'NONE', #45684, #65886, #4978, .T. ) ;
#63471 =( NAMED_UNIT ( * ) PLANE_ANGLE_UNIT ( ) SI_UNIT ( $, .RADIAN. ) );
#63472 = ORIENTED_EDGE ( 'NONE', *, *, #19245, .T. ) ;
#63473 = DIRECTION ( 'NONE',  ( 0.000000000000000000, 0.000000000000000000, -1.000000000000000000 ) ) ;
#63474 = DIRECTION ( 'NONE',  ( 1.000000000000000000, 0.000000000000000000, 0.000000000000000000 ) ) ;
#63475 = CARTESIAN_POINT ( 'NONE',  ( 6.826472737025119919, 144.0070736234661126, 4.959722759717908325 ) ) ;
#63476 =( NAMED_UNIT ( * ) SI_UNIT ( $, .STERADIAN. ) SOLID_ANGLE_UNIT ( ) );
#63477 = AXIS2_PLACEMENT_3D ( 'NONE', #47484, #58008, #67864 ) ;
#63478 = ORIENTED_EDGE ( 'NONE', *, *, #43018, .T. ) ;
#63480 = EDGE_CURVE ( 'NONE', #40163, #60087, #61216, .T. ) ;
#63479 = CARTESIAN_POINT ( 'NONE',  ( -65.99999999999998579, 50.00000000000000000, 12.00000000000000000 ) ) ;
#63481 = CARTESIAN_POINT ( 'NONE',  ( -97.55499999999999261, 0.000000000000000000, 8.024999999999991473 ) ) ;
#63482 = DIRECTION ( 'NONE',  ( 0.000000000000000000, 0.000000000000000000, -1.000000000000000000 ) ) ;
#63483 = ORIENTED_EDGE ( 'NONE', *, *, #65202, .F. ) ;
#63484 = CARTESIAN_POINT ( 'NONE',  ( 75.00000000000000000, 20.36037961002804764, -6.585786437626907741 ) ) ;
#63485 = DIRECTION ( 'NONE',  ( -1.000000000000000000, 0.000000000000000000, 0.000000000000000000 ) ) ;
#63486 =( NAMED_UNIT ( * ) SI_UNIT ( $, .STERADIAN. ) SOLID_ANGLE_UNIT ( ) );
#63487 = ORIENTED_EDGE ( 'NONE', *, *, #59001, .T. ) ;
#63488 = MECHANICAL_DESIGN_GEOMETRIC_PRESENTATION_REPRESENTATION (  '', ( #28620 ), #17427 ) ;
#63489 = CARTESIAN_POINT ( 'NONE',  ( 72.49999999999998579, 64.07124727947029896, 9.500000000000000000 ) ) ;
#63490 = CARTESIAN_POINT ( 'NONE',  ( -73.79499999999997328, 2.607480562269068880, -8.024999999999993250 ) ) ;
#63491 = EDGE_LOOP ( 'NONE', ( #13647, #3724, #36769, #15281, #45959, #60465 ) ) ;
#63492 = CARTESIAN_POINT ( 'NONE',  ( 70.87837837837835764, 13.70805908423324482, -9.500000000000000000 ) ) ;
#63493 = CARTESIAN_POINT ( 'NONE',  ( 0.000000000000000000, 109.9999999999999858, 0.000000000000000000 ) ) ;
#63494 = CARTESIAN_POINT ( 'NONE',  ( -124.7070736234668829, -3.094860106630464180, -9.524999999991248245 ) ) ;
#63495 = ORIENTED_EDGE ( 'NONE', *, *, #19245, .F. ) ;
#63496 = CARTESIAN_POINT ( 'NONE',  ( 68.99999999999998579, 1.000000000000008438, 3.000000000000000000 ) ) ;
#63497 = CYLINDRICAL_SURFACE ( 'NONE', #15710, 11.99999999999999645 ) ;
#63498 = SURFACE_STYLE_FILL_AREA ( #14991 ) ;
#63499 = ORIENTED_EDGE ( 'NONE', *, *, #23420, .F. ) ;
#63500 = PRESENTATION_LAYER_ASSIGNMENT (  '', '', ( #38835 ) ) ;
#63501 = ORIENTED_EDGE ( 'NONE', *, *, #52479, .F. ) ;
#63502 = FILL_AREA_STYLE_COLOUR ( '', #60532 ) ;
#63503 = DIRECTION ( 'NONE',  ( 0.000000000000000000, 0.000000000000000000, 1.000000000000000000 ) ) ;
#63504 = CARTESIAN_POINT ( 'NONE',  ( -41.38256758237925936, 107.6997254016901451, 3.907089461173326672 ) ) ;
#63505 = CARTESIAN_POINT ( 'NONE',  ( -163.2570736234661695, 5.598654528085800663, -7.705886871421367523 ) ) ;
#63506 = CARTESIAN_POINT ( 'NONE',  ( 9.058813317711338797, 120.8449999999999847, -2.943386871421372675 ) ) ;
#63507 = STYLED_ITEM ( 'NONE', ( #5234 ), #57035 ) ;
#63508 = CARTESIAN_POINT ( 'NONE',  ( -105.0570736234661666, 0.000000000000000000, 9.524999999999991473 ) ) ;
#63509 = EDGE_CURVE ( 'NONE', #13443, #12003, #52262, .T. ) ;
#63510 = CARTESIAN_POINT ( 'NONE',  ( 5.590169943749474513, 0.000000000000000000, 0.000000000000000000 ) ) ;
#63511 = ORIENTED_EDGE ( 'NONE', *, *, #48508, .F. ) ;
#63512 = CARTESIAN_POINT ( 'NONE',  ( 23.71231517720798010, 112.9999999999999858, 9.500000000000000000 ) ) ;
#63513 = CARTESIAN_POINT ( 'NONE',  ( -145.1049999999999898, -6.826472737025115478, 4.959722759717900331 ) ) ;
#63514 = CARTESIAN_POINT ( 'NONE',  ( -154.6450000000000102, 4.716976649647091513, -6.492361379858946790 ) ) ;
#63515 = CARTESIAN_POINT ( 'NONE',  ( -142.9449999999999932, -9.827790563157499189E-16, -8.024999999999991473 ) ) ;
#63516 = ORIENTED_EDGE ( 'NONE', *, *, #68416, .T. ) ;
#63517 =( GEOMETRIC_REPRESENTATION_CONTEXT ( 3 ) GLOBAL_UNCERTAINTY_ASSIGNED_CONTEXT ( ( #63043 ) ) GLOBAL_UNIT_ASSIGNED_CONTEXT ( ( #5685, #22587, #1042 ) ) REPRESENTATION_CONTEXT ( 'NONE', 'WORKASPACE' ) );
#63518 = CARTESIAN_POINT ( 'NONE',  ( -180.5070736234661979, 8.102448949553176405, 5.886773742842740909 ) ) ;
#63519 = APPLICATION_CONTEXT ( 'automotive_design' ) ;
#63520 = LINE ( 'NONE', #20256, #64885 ) ;
#63521 = DIRECTION ( 'NONE',  ( 1.000000000000000000, -0.000000000000000000, -0.000000000000000000 ) ) ;
#63522 = UNCERTAINTY_MEASURE_WITH_UNIT (LENGTH_MEASURE( 1.000000000000000082E-05 ), #170, 'distance_accuracy_value', 'NONE');
#63523 = CARTESIAN_POINT ( 'NONE',  ( -50.75499999999999545, 4.716976649647091513, -6.492361379858946790 ) ) ;
#63524 = B_SPLINE_CURVE_WITH_KNOTS ( 'NONE', 3,
 ( #61787, #13618, #51613, #34718, #40738, #24501, #1955, #55843, #19594, #44981, #41091, #45338 ),
 .UNSPECIFIED., .F., .F.,
 ( 4, 2, 2, 2, 2, 4 ),
 ( 0.000000000000000000, 0.0002999083533514614692, 0.0005998167067029229384, 0.001199633413405845877, 0.001799450120108768815, 0.002399266826811691754 ),
 .UNSPECIFIED. ) ;
#63525 =( LENGTH_UNIT ( ) NAMED_UNIT ( * ) SI_UNIT ( .MILLI., .METRE. ) );
#63526 = EDGE_CURVE ( 'NONE', #12224, #30865, #9658, .T. ) ;
#63527 = VECTOR ( 'NONE', #67471, 1000.000000000000000 ) ;
#63528 = EDGE_CURVE ( 'NONE', #22472, #36852, #65054, .T. ) ;
#63529 = CARTESIAN_POINT ( 'NONE',  ( 10.01517768586949231, 154.8050000000000352, 1.839758294383810543E-15 ) ) ;
#63530 =( NAMED_UNIT ( * ) PLANE_ANGLE_UNIT ( ) SI_UNIT ( $, .RADIAN. ) );
#63531 = CARTESIAN_POINT ( 'NONE',  ( -40.99999999999997868, 9.999999999999978684, 3.500000000000000000 ) ) ;
#63532 = CIRCLE ( 'NONE', #10765, 13.49999999999999822 ) ;
#63533 = CIRCLE ( 'NONE', #25318, 3.100000000000001865 ) ;
#63534 = UNCERTAINTY_MEASURE_WITH_UNIT (LENGTH_MEASURE( 1.000000000000000082E-05 ), #53578, 'distance_accuracy_value', 'NONE');
#63535 = DIRECTION ( 'NONE',  ( 1.000000000000000000, -1.202395036544009525E-16, -8.041998848429300809E-17 ) ) ;
#63536 = EDGE_CURVE ( 'NONE', #39475, #37240, #26253, .T. ) ;
#63537 = SURFACE_SIDE_STYLE ('',( #57933 ) ) ;
#63538 = EDGE_CURVE ( 'NONE', #47699, #55021, #11754, .T. ) ;
#63539 = CARTESIAN_POINT ( 'NONE',  ( 17.25000000000000711, 25.24999999999998224, 3.750000000000000000 ) ) ;
#63540 = CARTESIAN_POINT ( 'NONE',  ( -178.0429263765338135, -9.058813317711329915, -2.943386871421370898 ) ) ;
#63541 = AXIS2_PLACEMENT_3D ( 'NONE', #3484, #3851, #24986 ) ;
#63542 = LINE ( 'NONE', #29801, #21850 ) ;
#63543 = EDGE_CURVE ( 'NONE', #49361, #65027, #31991, .T. ) ;
#63544 = CARTESIAN_POINT ( 'NONE',  ( 0.000000000000000000, 0.000000000000000000, 0.7500000000000000000 ) ) ;
#63545 = ORIENTED_EDGE ( 'NONE', *, *, #58146, .T. ) ;
#63546 = TOROIDAL_SURFACE ( 'NONE', #28733, 13.49999999999999822, 0.5000000000000000000 ) ;
#63547 = ORIENTED_EDGE ( 'NONE', *, *, #64532, .F. ) ;
#63548 = SURFACE_SIDE_STYLE ('',( #47782 ) ) ;
#63550 = CARTESIAN_POINT ( 'NONE',  ( -9.827790563157511022E-16, 116.5570736234661666, 8.025000000000000355 ) ) ;
#63549 = STYLED_ITEM ( 'NONE', ( #249 ), #57094 ) ;
#63551 = AXIS2_PLACEMENT_3D ( 'NONE', #27165, #53262, #32131 ) ;
#63553 = ADVANCED_FACE ( 'NONE', ( #16231 ), #37355, .T. ) ;
#63552 = FILL_AREA_STYLE_COLOUR ( '', #19153 ) ;
#63554 = DIRECTION ( 'NONE',  ( -1.000000000000000000, 0.000000000000000000, 0.000000000000000000 ) ) ;
#63555 = PRESENTATION_STYLE_ASSIGNMENT (( #19595 ) ) ;
#63556 = VERTEX_POINT ( 'NONE', #42980 ) ;
#63557 = ORIENTED_EDGE ( 'NONE', *, *, #5546, .T. ) ;
#63558 =( NAMED_UNIT ( * ) SI_UNIT ( $, .STERADIAN. ) SOLID_ANGLE_UNIT ( ) );
#63559 = CARTESIAN_POINT ( 'NONE',  ( -101.6929263765337765, 10.01517768586948698, -1.839758294383808966E-15 ) ) ;
#63560 = ORIENTED_EDGE ( 'NONE', *, *, #42617, .T. ) ;
#63561 = CARTESIAN_POINT ( 'NONE',  ( 5.598654528085805993, 121.3549999999999898, 7.705886871421374629 ) ) ;
#63562 = CARTESIAN_POINT ( 'NONE',  ( 0.9126302363881977353, 2.499999999999996447, -9.000000000000007105 ) ) ;
#63563 = CYLINDRICAL_SURFACE ( 'NONE', #34474, 1.000000000000000000 ) ;
#63564 = DIRECTION ( 'NONE',  ( 0.000000000000000000, 0.000000000000000000, -1.000000000000000000 ) ) ;
#63565 = CARTESIAN_POINT ( 'NONE',  ( -97.64499999999999602, 4.716976649647091513, -6.492361379858946790 ) ) ;
#63566 = ORIENTED_EDGE ( 'NONE', *, *, #68859, .T. ) ;
#63567 = VECTOR ( 'NONE', #38204, 1000.000000000000000 ) ;
#63568 =( NAMED_UNIT ( * ) SI_UNIT ( $, .STERADIAN. ) SOLID_ANGLE_UNIT ( ) );
#63569 =( NAMED_UNIT ( * ) SI_UNIT ( $, .STERADIAN. ) SOLID_ANGLE_UNIT ( ) );
#63570 = UNCERTAINTY_MEASURE_WITH_UNIT (LENGTH_MEASURE( 1.000000000000000082E-05 ), #29101, 'distance_accuracy_value', 'NONE');
#63571 = ORIENTED_EDGE ( 'NONE', *, *, #64673, .F. ) ;
#63572 = CARTESIAN_POINT ( 'NONE',  ( -7.632228543268608334, 153.8429263765338249, 2.479861379858952830 ) ) ;
#63573 = PRESENTATION_STYLE_ASSIGNMENT (( #43215 ) ) ;
#63574 = CARTESIAN_POINT ( 'NONE',  ( 34.99999999999999289, 99.99999999999997158, 4.000000000000000000 ) ) ;
#63575 = DIRECTION ( 'NONE',  ( -1.982541115402068561E-16, 0.000000000000000000, 1.000000000000000000 ) ) ;
#63576 = VERTEX_POINT ( 'NONE', #28093 ) ;
#63577 = COLOUR_RGB ( '', 0.66274510, 0.83137255, 0.94901961) ;
#63578 = COLOUR_RGB ( '', 0.66274510, 0.83137255, 0.94901961) ;
#63579 = CARTESIAN_POINT ( 'NONE',  ( -45.91547277936962246, 9.430195807687219656, 3.611004237778671744 ) ) ;
#63580 = SURFACE_STYLE_FILL_AREA ( #42188 ) ;
#63581 = DIRECTION ( 'NONE',  ( -1.000000000000000000, -0.000000000000000000, -0.000000000000000000 ) ) ;
#63582 =( GEOMETRIC_REPRESENTATION_CONTEXT ( 3 ) GLOBAL_UNCERTAINTY_ASSIGNED_CONTEXT ( ( #57884 ) ) GLOBAL_UNIT_ASSIGNED_CONTEXT ( ( #60377, #24467, #55458 ) ) REPRESENTATION_CONTEXT ( 'NONE', 'WORKASPACE' ) );
#63583 = DIRECTION ( 'NONE',  ( -0.000000000000000000, -0.000000000000000000, 1.000000000000000000 ) ) ;
#63584 = SURFACE_STYLE_FILL_AREA ( #5497 ) ;
#63585 = EDGE_CURVE ( 'NONE', #9347, #14945, #493, .T. ) ;
#63586 =( NAMED_UNIT ( * ) PLANE_ANGLE_UNIT ( ) SI_UNIT ( $, .RADIAN. ) );
#63587 = FACE_OUTER_BOUND ( 'NONE', #5080, .T. ) ;
#63588 = CARTESIAN_POINT ( 'NONE',  ( 26.00000000000001066, 21.74999999999998224, 4.000000000000000000 ) ) ;
#63589 = CARTESIAN_POINT ( 'NONE',  ( -13.25000000000000355, 27.74999999999998934, 3.750000000000000000 ) ) ;
#63590 = ORIENTED_EDGE ( 'NONE', *, *, #45312, .F. ) ;
#63591 = ORIENTED_EDGE ( 'NONE', *, *, #32750, .F. ) ;
#63592 = DIRECTION ( 'NONE',  ( 0.000000000000000000, 0.000000000000000000, 1.000000000000000000 ) ) ;
#63593 = CARTESIAN_POINT ( 'NONE',  ( 60.00000000000000000, 1.797044900979284448E-15, 6.500000000000000000 ) ) ;
#63594 = PRESENTATION_STYLE_ASSIGNMENT (( #52709 ) ) ;
#63595 = ORIENTED_EDGE ( 'NONE', *, *, #9243, .F. ) ;
#63596 = CARTESIAN_POINT ( 'NONE',  ( -154.6429263765338078, -5.598654528085801552, 7.705886871421367523 ) ) ;
#63597 = CARTESIAN_POINT ( 'NONE',  ( -171.3550000000000182, -4.716976649647093289, -6.492361379858945902 ) ) ;
#63598 = DIRECTION ( 'NONE',  ( -2.312964634635740689E-15, 1.000000000000000000, -0.000000000000000000 ) ) ;
#63599 = CARTESIAN_POINT ( 'NONE',  ( 18.25000000000000711, 33.74999999999999289, -3.750000000000000000 ) ) ;
#63600 = CARTESIAN_POINT ( 'NONE',  ( -48.80707362346616662, 10.01517768586948698, -1.839758294383808571E-15 ) ) ;
#63601 = CARTESIAN_POINT ( 'NONE',  ( -168.8949999999999818, 6.826472737025115478, 4.959722759717899443 ) ) ;
#63602 = CIRCLE ( 'NONE', #38791, 0.5000000000000004441 ) ;
#63603 = ORIENTED_EDGE ( 'NONE', *, *, #12935, .T. ) ;
#63604 = PRODUCT_RELATED_PRODUCT_CATEGORY ( 'part', '', ( #51816 ) ) ;
#63605 = EDGE_CURVE ( 'NONE', #4180, #835, #47775, .T. ) ;
#63606 = CARTESIAN_POINT ( 'NONE',  ( -3.542344102440326825, -1.863645424029198194, 9.000000000000000000 ) ) ;
#63607 = CARTESIAN_POINT ( 'NONE',  ( -14.34071883355357535, 10.92737318490738474, -4.959116828949759359 ) ) ;
#63608 = CARTESIAN_POINT ( 'NONE',  ( -90.20499999999999829, -2.607480562269071545, -8.024999999999991473 ) ) ;
#63609 = CARTESIAN_POINT ( 'NONE',  ( 9.452512629751957718, 154.4999999999999432, 1.251363035250141920 ) ) ;
#63610 = FILL_AREA_STYLE_COLOUR ( '', #16857 ) ;
#63611 = CARTESIAN_POINT ( 'NONE',  ( -74.61046851513155787, 36.28146479779877609, -9.990989611816710081 ) ) ;
#63612 = ADVANCED_FACE ( 'NONE', ( #64383 ), #38033, .T. ) ;
#63613 = CARTESIAN_POINT ( 'NONE',  ( -92.09499999999998465, -2.607480562269071545, -8.024999999999991473 ) ) ;
#63614 = ADVANCED_FACE ( 'NONE', ( #293 ), #59794, .F. ) ;
#63615 = CARTESIAN_POINT ( 'NONE',  ( 8.102448949553181734, 130.5049999999999670, 5.886773742842750679 ) ) ;
#63616 = CARTESIAN_POINT ( 'NONE',  ( -71.50000000000000000, 35.92875272052971525, -9.500000000000000000 ) ) ;
#63617 = DIRECTION ( 'NONE',  ( -0.000000000000000000, 0.000000000000000000, -1.000000000000000000 ) ) ;
#63618 = DIRECTION ( 'NONE',  ( 0.000000000000000000, 0.000000000000000000, -1.000000000000000000 ) ) ;
#63619 = UNCERTAINTY_MEASURE_WITH_UNIT (LENGTH_MEASURE( 1.000000000000000082E-05 ), #57073, 'distance_accuracy_value', 'NONE');
#63620 = VERTEX_POINT ( 'NONE', #5974 ) ;
#63621 = ADVANCED_FACE ( 'NONE', ( #27750 ), #961, .F. ) ;
#63622 = PRODUCT_DEFINITION_SHAPE ( 'NONE', 'NONE',  #6411 ) ;
#63623 = DIRECTION ( 'NONE',  ( 1.000000000000000000, 0.000000000000000000, 0.000000000000000000 ) ) ;
#63624 = EDGE_CURVE ( 'NONE', #57014, #50171, #39757, .T. ) ;
#63625 = MECHANICAL_DESIGN_GEOMETRIC_PRESENTATION_REPRESENTATION (  '', ( #27642 ), #65848 ) ;
#63626 = CARTESIAN_POINT ( 'NONE',  ( 4.500000000000002665, 22.24999999999998579, -3.750000000000000000 ) ) ;
#63627 = CIRCLE ( 'NONE', #60260, 1.000000000000000888 ) ;
#63628 = CARTESIAN_POINT ( 'NONE',  ( -132.1429263765338078, 5.598654528085800663, -7.705886871421367523 ) ) ;
#63629 = STYLED_ITEM ( 'NONE', ( #16966 ), #50074 ) ;
#63630 = DIRECTION ( 'NONE',  ( 0.000000000000000000, 0.000000000000000000, -1.000000000000000000 ) ) ;
#63631 = VERTEX_POINT ( 'NONE', #39073 ) ;
#63632 = ORIENTED_EDGE ( 'NONE', *, *, #46362, .T. ) ;
#63633 = CARTESIAN_POINT ( 'NONE',  ( 53.24999999999999289, 27.99999999999998579, -3.750000000000000000 ) ) ;
#63634 = CARTESIAN_POINT ( 'NONE',  ( -134.6929263765337907, 10.01517768586948698, -1.839758294383808966E-15 ) ) ;
#63635 = CARTESIAN_POINT ( 'NONE',  ( -4.250000000000001776, 22.24999999999998579, -3.750000000000000000 ) ) ;
#63636 = FILL_AREA_STYLE ('',( #64322 ) ) ;
#63637 = CARTESIAN_POINT ( 'NONE',  ( 8.750000000000001776, 24.74999999999998579, 4.000000000000000000 ) ) ;
#63638 = PRESENTATION_STYLE_ASSIGNMENT (( #20739 ) ) ;
#63639 = ORIENTED_EDGE ( 'NONE', *, *, #39088, .T. ) ;
#63640 = CARTESIAN_POINT ( 'NONE',  ( -117.3549999999999898, -4.716976649647093289, -6.492361379858945902 ) ) ;
#63641 = EDGE_LOOP ( 'NONE', ( #24016, #22914, #50958, #22944, #4690, #2163 ) ) ;
#63642 = SURFACE_SIDE_STYLE ('',( #52426 ) ) ;
#63643 = FACE_BOUND ( 'NONE', #5176, .T. ) ;
#63644 = ORIENTED_EDGE ( 'NONE', *, *, #5650, .F. ) ;
#63645 = SURFACE_STYLE_USAGE ( .BOTH. , #47168 ) ;
#63646 = LINE ( 'NONE', #10538, #66973 ) ;
#63647 = ORIENTED_EDGE ( 'NONE', *, *, #2230, .T. ) ;
#63648 = EDGE_CURVE ( 'NONE', #47061, #6428, #55594, .T. ) ;
#63649 = DIRECTION ( 'NONE',  ( 1.000000000000000000, 0.000000000000000000, 0.000000000000000000 ) ) ;
#63650 = CARTESIAN_POINT ( 'NONE',  ( -5.598654528085806881, 145.7449999999999761, -7.705886871421374629 ) ) ;
#63651 = FILL_AREA_STYLE ('',( #42262 ) ) ;
#63652 = EDGE_LOOP ( 'NONE', ( #37253, #40624, #13699 ) ) ;
#63653 = CARTESIAN_POINT ( 'NONE',  ( -54.95707362346616520, 9.058813317711329915, -2.943386871421373119 ) ) ;
#63654 = CARTESIAN_POINT ( 'NONE',  ( 5.598654528085809545, 149.2549999999999955, -7.705886871421373741 ) ) ;
#63655 = CARTESIAN_POINT ( 'NONE',  ( 9.000000000000003553, 25.24999999999998934, 3.750000000000000000 ) ) ;
#63656 = EDGE_LOOP ( 'NONE', ( #15651, #5766, #63015, #62653 ) ) ;
#63657 = CARTESIAN_POINT ( 'NONE',  ( -8.437984349512095861, 126.6929263765338050, -5.166775262442723748E-16 ) ) ;
#63658 = LINE ( 'NONE', #21429, #30042 ) ;
#63659 = UNCERTAINTY_MEASURE_WITH_UNIT (LENGTH_MEASURE( 1.000000000000000082E-05 ), #52851, 'distance_accuracy_value', 'NONE');
#63660 = CARTESIAN_POINT ( 'NONE',  ( -74.50000000000000000, 36.50926243676796190, -10.00000000000000000 ) ) ;
#63661 = PRESENTATION_STYLE_ASSIGNMENT (( #31992 ) ) ;
#63662 = ORIENTED_EDGE ( 'NONE', *, *, #45609, .T. ) ;
#63663 = CARTESIAN_POINT ( 'NONE',  ( 6.062177826491071286, -3.500000000000002220, 0.000000000000000000 ) ) ;
#63664 = ORIENTED_EDGE ( 'NONE', *, *, #4694, .F. ) ;
#63665 = CARTESIAN_POINT ( 'NONE',  ( -62.84292637653379643, 9.058813317711329915, -2.943386871421373119 ) ) ;
#63666 = DIRECTION ( 'NONE',  ( -1.000000000000000000, 0.000000000000000000, 0.000000000000000000 ) ) ;
#63667 = CARTESIAN_POINT ( 'NONE',  ( -7.441974819423180065, 1.110121504110840762, 0.4967607073414712637 ) ) ;
#63668 = CARTESIAN_POINT ( 'NONE',  ( -151.2549999999999955, -4.716976649647092401, 6.492361379858946790 ) ) ;
#63669 = LINE ( 'NONE', #64010, #14843 ) ;
#63670 = UNCERTAINTY_MEASURE_WITH_UNIT (LENGTH_MEASURE( 1.000000000000000082E-05 ), #57685, 'distance_accuracy_value', 'NONE');
#63671 = CARTESIAN_POINT ( 'NONE',  ( 68.99999999999998579, 37.00000000000000000, -3.000000000000000000 ) ) ;
#63672 = SURFACE_STYLE_USAGE ( .BOTH. , #38020 ) ;
#63673 = CARTESIAN_POINT ( 'NONE',  ( 25.00000000000000355, 37.00000000000000000, 4.000000000000000000 ) ) ;
#63674 = FACE_OUTER_BOUND ( 'NONE', #2049, .T. ) ;
#63675 = ORIENTED_EDGE ( 'NONE', *, *, #65094, .F. ) ;
#63676 = ORIENTED_EDGE ( 'NONE', *, *, #36440, .T. ) ;
#63677 = CARTESIAN_POINT ( 'NONE',  ( 22.54460582735575969, 26.91484815598150604, 27.37908301411970768 ) ) ;
#63678 = AXIS2_PLACEMENT_3D ( 'NONE', #49840, #21706, #1581 ) ;
#63679 = CARTESIAN_POINT ( 'NONE',  ( -4.750000000000000000, 0.000000000000000000, 0.7500000000000000000 ) ) ;
#63680 = CARTESIAN_POINT ( 'NONE',  ( -68.75499999999998124, 4.716976649647091513, -6.492361379858946790 ) ) ;
#63681 = ORIENTED_EDGE ( 'NONE', *, *, #9158, .F. ) ;
#63682 = FILL_AREA_STYLE_COLOUR ( '', #4484 ) ;
#63683 = FILL_AREA_STYLE_COLOUR ( '', #29208 ) ;
#63684 = DIRECTION ( 'NONE',  ( -0.000000000000000000, -0.000000000000000000, 1.000000000000000000 ) ) ;
#63685 = PRESENTATION_STYLE_ASSIGNMENT (( #67585 ) ) ;
#63686 = CARTESIAN_POINT ( 'NONE',  ( -75.48275862068965125, 36.00832590023089352, -41.30495168499704306 ) ) ;
#63687 = ORIENTED_EDGE ( 'NONE', *, *, #14663, .T. ) ;
#63688 = EDGE_CURVE ( 'NONE', #15520, #24259, #60464, .T. ) ;
#63689 = PRESENTATION_STYLE_ASSIGNMENT (( #10583 ) ) ;
#63690 = CARTESIAN_POINT ( 'NONE',  ( 9.000000000000003553, 27.99999999999998934, 3.750000000000000000 ) ) ;
#63691 = DIRECTION ( 'NONE',  ( 0.000000000000000000, 0.000000000000000000, 1.000000000000000000 ) ) ;
#63692 = B_SPLINE_CURVE_WITH_KNOTS ( 'NONE', 3,
 ( #32279, #58326, #48509, #63607, #53731, #10152, #68547, #4858, #47848, #5196, #15450, #30894, #64292, #9468, #19981, #52393, #68905, #5523, #26976, #41848, #15113, #31583, #42540, #69245, #53066, #20706, #41481, #63266, #42217, #21375, #15787, #4139, #63939, #25607, #62897, #47121, #4490, #37269 ),
 .UNSPECIFIED., .F., .F.,
 ( 4, 2, 2, 2, 2, 2, 2, 2, 2, 2, 2, 2, 2, 2, 2, 2, 2, 2, 4 ),
 ( 0.01581385303085219851, 0.01630764152937332415, 0.01680143002789444631, 0.01778900702493669064, 0.01828279552345780934, 0.01877658402197893150, 0.01976416101902116890, 0.02075173801606340629, 0.02173931501310564368, 0.02272689201014788107, 0.02371446900719011500, 0.02470204600423234892, 0.02568962300127458631, 0.02667719999831682370, 0.02766477699535906110, 0.02865235399240129849, 0.02963993098944353588, 0.03062750798648576980, 0.03161508498352800373 ),
 .UNSPECIFIED. ) ;
#63693 = TOROIDAL_SURFACE ( 'NONE', #68223, 14.49999999999999822, 0.5000000000000000000 ) ;
#63694 = ADVANCED_FACE ( 'NONE', ( #56233 ), #50287, .T. ) ;
#63695 = CARTESIAN_POINT ( 'NONE',  ( -114.7449999999999903, 4.716976649647094177, 6.492361379858945902 ) ) ;
#63696 = CARTESIAN_POINT ( 'NONE',  ( 8.102448949553181734, 150.3949999999999818, 5.886773742842750679 ) ) ;
#63697 = CARTESIAN_POINT ( 'NONE',  ( -86.24499999999999034, -4.716976649647093289, -6.492361379858945902 ) ) ;
#63698 = DIRECTION ( 'NONE',  ( 0.000000000000000000, 0.000000000000000000, 1.000000000000000000 ) ) ;
#63699 = FACE_OUTER_BOUND ( 'NONE', #69349, .T. ) ;
#63700 = UNCERTAINTY_MEASURE_WITH_UNIT (LENGTH_MEASURE( 1.000000000000000082E-05 ), #58831, 'distance_accuracy_value', 'NONE');
#63701 = CARTESIAN_POINT ( 'NONE',  ( 108.3664351561509420, 1.000000000000000000, -18.43563588791578667 ) ) ;
#63702 = ORIENTED_EDGE ( 'NONE', *, *, #47719, .T. ) ;
#63703 = CARTESIAN_POINT ( 'NONE',  ( -133.0429263765338135, -9.058813317711329915, -2.943386871421370898 ) ) ;
#63704 = CARTESIAN_POINT ( 'NONE',  ( -161.6950000000000216, -8.437984349512085203, 5.166775262442717831E-16 ) ) ;
#63705 = CARTESIAN_POINT ( 'NONE',  ( -1.403516486455610890, 7.000000000000006217, 0.1310752030855656391 ) ) ;
#63706 = EDGE_CURVE ( 'NONE', #51098, #19619, #35723, .T. ) ;
#63707 =( LENGTH_UNIT ( ) NAMED_UNIT ( * ) SI_UNIT ( .MILLI., .METRE. ) );
#63708 = ORIENTED_EDGE ( 'NONE', *, *, #7716, .T. ) ;
#63709 = ORIENTED_EDGE ( 'NONE', *, *, #68633, .F. ) ;
#63710 = FACE_OUTER_BOUND ( 'NONE', #7740, .T. ) ;
#63711 = CARTESIAN_POINT ( 'NONE',  ( -6.826472737025120807, 117.9929263765338021, 4.959722759717906548 ) ) ;
#63712 = CARTESIAN_POINT ( 'NONE',  ( -45.00000000000033396, 8.701466902705615070, 5.869459488307998463 ) ) ;
#63713 = PLANE ( 'NONE',  #22956 ) ;
#63714 = VECTOR ( 'NONE', #22322, 1000.000000000000000 ) ;
#63715 = EDGE_LOOP ( 'NONE', ( #59102, #64441, #13400, #6506 ) ) ;
#63716 = CARTESIAN_POINT ( 'NONE',  ( -152.9049999999999727, 2.607480562269069324, -8.024999999999993250 ) ) ;
#63717 = AXIS2_PLACEMENT_3D ( 'NONE', #8817, #63666, #52455 ) ;
#63718 = VERTEX_POINT ( 'NONE', #45395 ) ;
#63719 = PRESENTATION_STYLE_ASSIGNMENT (( #336 ) ) ;
#63720 = VERTEX_POINT ( 'NONE', #12984 ) ;
#63721 = DIRECTION ( 'NONE',  ( 0.000000000000000000, 1.350863103983176297E-16, 1.000000000000000000 ) ) ;
#63722 = EDGE_CURVE ( 'NONE', #7643, #68674, #65769, .T. ) ;
#63723 = LINE ( 'NONE', #55241, #38842 ) ;
#63724 = CARTESIAN_POINT ( 'NONE',  ( -3.094860106618432471, 121.5949999999999847, -9.525000000000000355 ) ) ;
#63725 = ORIENTED_EDGE ( 'NONE', *, *, #20310, .T. ) ;
#63726 = FACE_OUTER_BOUND ( 'NONE', #33689, .T. ) ;
#63727 = CARTESIAN_POINT ( 'NONE',  ( -9.058813317711338797, 123.4549999999999841, 2.943386871421373563 ) ) ;
#63728 = CARTESIAN_POINT ( 'NONE',  ( -65.60499999999998977, 6.826472737025113702, -4.959722759717902107 ) ) ;
#63729 = FACE_OUTER_BOUND ( 'NONE', #63279, .T. ) ;
#63730 = ORIENTED_EDGE ( 'NONE', *, *, #33286, .F. ) ;
#63731 = CARTESIAN_POINT ( 'NONE',  ( 5.598654528085805993, 151.3549999999999898, 7.705886871421374629 ) ) ;
#63732 = UNCERTAINTY_MEASURE_WITH_UNIT (LENGTH_MEASURE( 1.000000000000000082E-05 ), #15304, 'distance_accuracy_value', 'NONE');
#63733 = AXIS2_PLACEMENT_3D ( 'NONE', #47043, #58592, #52979 ) ;
#63734 = DIRECTION ( 'NONE',  ( 0.000000000000000000, 0.000000000000000000, 1.000000000000000000 ) ) ;
#63735 = CIRCLE ( 'NONE', #17713, 4.999999999999990230 ) ;
#63736 = CARTESIAN_POINT ( 'NONE',  ( 4.683753779217428637, 2.005109422339667269, -5.887500484252663036 ) ) ;
#63737 = DIRECTION ( 'NONE',  ( -0.000000000000000000, -0.000000000000000000, 1.000000000000000000 ) ) ;
#63738 = ORIENTED_EDGE ( 'NONE', *, *, #53993, .T. ) ;
#63739 = CARTESIAN_POINT ( 'NONE',  ( -35.25000000000000000, 4.336808689942018722E-16, 0.000000000000000000 ) ) ;
#63740 = CARTESIAN_POINT ( 'NONE',  ( -46.55707362346617373, -1.166476076187852838E-15, -9.524999999999991473 ) ) ;
#63741 = CARTESIAN_POINT ( 'NONE',  ( -115.5570736234661808, -1.166476076187852838E-15, -9.524999999999991473 ) ) ;
#63742 = CARTESIAN_POINT ( 'NONE',  ( -184.4049999999999727, -2.607480562269069768, 8.024999999999991473 ) ) ;
#63743 = ORIENTED_EDGE ( 'NONE', *, *, #49727, .T. ) ;
#63744 = CARTESIAN_POINT ( 'NONE',  ( 4.134715136431655225, 111.0353213183942529, 8.000580966448456621 ) ) ;
#63745 = DIRECTION ( 'NONE',  ( 0.000000000000000000, 0.000000000000000000, -1.000000000000000000 ) ) ;
#63746 = FILL_AREA_STYLE_COLOUR ( '', #1467 ) ;
#63747 = EDGE_LOOP ( 'NONE', ( #57443, #65735, #25498, #13292 ) ) ;
#63748 = CARTESIAN_POINT ( 'NONE',  ( -5.196152422706634688, 9.000000000000008882, 7.500000000000000000 ) ) ;
#63749 = CARTESIAN_POINT ( 'NONE',  ( -48.44292637653380496, -1.166476076187852838E-15, -9.524999999999991473 ) ) ;
#63750 = ORIENTED_EDGE ( 'NONE', *, *, #11771, .T. ) ;
#63751 = CARTESIAN_POINT ( 'NONE',  ( -127.8570736234661780, -5.598654528085803328, -7.705886871421366635 ) ) ;
#63752 = CARTESIAN_POINT ( 'NONE',  ( -97.85499999999998977, 4.716976649647094177, 6.492361379858945902 ) ) ;
#63753 = ORIENTED_EDGE ( 'NONE', *, *, #10742, .T. ) ;
#63754 = CARTESIAN_POINT ( 'NONE',  ( 12.25000000000000355, 30.74999999999998579, 3.750000000000000000 ) ) ;
#63755 = ADVANCED_FACE ( 'NONE', ( #17604 ), #18627, .T. ) ;
#63756 =( LENGTH_UNIT ( ) NAMED_UNIT ( * ) SI_UNIT ( .MILLI., .METRE. ) );
#63757 = CARTESIAN_POINT ( 'NONE',  ( -134.0070736234661695, -8.102448949553172852, -5.886773742842741797 ) ) ;
#63758 =( BOUNDED_SURFACE ( )  B_SPLINE_SURFACE ( 3, 2, ( 
 ( #21045, #59029, #47852 ),
 ( #15791, #4863, #4141 ),
 ( #31589, #42544, #63611 ),
 ( #5528, #30897, #63943 ),
 ( #42221, #64296, #31231 ),
 ( #37275, #53419, #31941 ),
 ( #25611, #58673, #68909 ),
 ( #36590, #48513, #10503 ),
 ( #10156, #210, #32283 ),
 ( #26641, #48166, #10841 ),
 ( #21739, #15454, #43251 ),
 ( #69574, #21380, #42903 ) ),
 .UNSPECIFIED., .F., .F., .F. ) 
 B_SPLINE_SURFACE_WITH_KNOTS ( ( 4, 2, 2, 2, 2, 4 ),
 ( 3, 3 ),
 ( -6.326733460093544372E-06, 0.0004675000763919686308, 0.0009413268862440307781, 0.001415153696096092817, 0.001652067101022123945, 0.001888980505948155073 ),
 ( 0.000000000000000000, 1.000000000000000000 ),
 .UNSPECIFIED. ) 
 GEOMETRIC_REPRESENTATION_ITEM ( )  RATIONAL_B_SPLINE_SURFACE ( (
 ( 1.000000000000000000, 1.000000000000000000, 1.000000000000000000),
 ( 1.000000000000000000, 0.9999603998840329577, 1.000000000000000000),
 ( 1.000000000000000000, 0.9905097737965633531, 1.000000000000000000),
 ( 1.000000000000000000, 0.9539269352976011973, 1.000000000000000000),
 ( 1.000000000000000000, 0.9259356461951893102, 1.000000000000000000),
 ( 1.000000000000000000, 0.8584222786211590517, 1.000000000000000000),
 ( 1.000000000000000000, 0.8173629853940447276, 1.000000000000000000),
 ( 1.000000000000000000, 0.7644081322687370506, 1.000000000000000000),
 ( 1.000000000000000000, 0.7482903728718443004, 1.000000000000000000),
 ( 1.000000000000000000, 0.7257247660741658057, 1.000000000000000000),
 ( 1.000000000000000000, 0.7190551827508514515, 1.000000000000000000),
 ( 1.000000000000000000, 0.7191949522280786100, 1.000000000000000000) ) ) 
 REPRESENTATION_ITEM ( '' )  SURFACE ( )  );
#63759 = DIRECTION ( 'NONE',  ( 0.000000000000000000, 0.000000000000000000, 1.000000000000000000 ) ) ;
#63760 = CARTESIAN_POINT ( 'NONE',  ( -5.598654528085806881, 151.7450000000000045, -7.705886871421374629 ) ) ;
#63761 = CARTESIAN_POINT ( 'NONE',  ( -63.95707362346617231, 9.058813317711329915, -2.943386871421373119 ) ) ;
#63762 = AXIS2_PLACEMENT_3D ( 'NONE', #3701, #62810, #56503 ) ;
#63763 = CARTESIAN_POINT ( 'NONE',  ( -80.84292637653379643, 9.058813317711329915, -2.943386871421373119 ) ) ;
#63764 = ORIENTED_EDGE ( 'NONE', *, *, #33674, .F. ) ;
#63765 = DIRECTION ( 'NONE',  ( 0.000000000000000000, 0.000000000000000000, 1.000000000000000000 ) ) ;
#63766 =( NAMED_UNIT ( * ) PLANE_ANGLE_UNIT ( ) SI_UNIT ( $, .RADIAN. ) );
#63767 = VECTOR ( 'NONE', #58556, 1000.000000000000000 ) ;
#63769 = SURFACE_SIDE_STYLE ('',( #69409 ) ) ;
#63768 = DIRECTION ( 'NONE',  ( -0.000000000000000000, 0.6691306063588581265, 0.7431448254773944662 ) ) ;
#63770 = AXIS2_PLACEMENT_3D ( 'NONE', #31306, #47569, #68625 ) ;
#63771 = CARTESIAN_POINT ( 'NONE',  ( -110.1549999999999869, 7.632228543268600340, 2.479861379858949277 ) ) ;
#63772 = EDGE_CURVE ( 'NONE', #31646, #8395, #37675, .T. ) ;
#63773 = CARTESIAN_POINT ( 'NONE',  ( -9.058813317711337021, 119.0449999999999875, -2.943386871421374895 ) ) ;
#63774 = CARTESIAN_POINT ( 'NONE',  ( -124.6449999999999960, 4.716976649647091513, -6.492361379858946790 ) ) ;
#63775 = PRESENTATION_LAYER_ASSIGNMENT (  '', '', ( #15511 ) ) ;
#63776 = EDGE_CURVE ( 'NONE', #36200, #2398, #49996, .T. ) ;
#63777 =( NAMED_UNIT ( * ) PLANE_ANGLE_UNIT ( ) SI_UNIT ( $, .RADIAN. ) );
#63778 = CARTESIAN_POINT ( 'NONE',  ( -118.1929263765337907, -10.01517768586948698, 6.132527647946031529E-16 ) ) ;
#63779 = AXIS2_PLACEMENT_3D ( 'NONE', #66600, #55342, #41206 ) ;
#63780 = EDGE_CURVE ( 'NONE', #849, #26112, #51322, .T. ) ;
#63781 = ORIENTED_EDGE ( 'NONE', *, *, #47327, .F. ) ;
#63782 = CARTESIAN_POINT ( 'NONE',  ( -163.7929263765337851, -3.094860106618429807, 9.524999999999991473 ) ) ;
#63783 =( NAMED_UNIT ( * ) PLANE_ANGLE_UNIT ( ) SI_UNIT ( $, .RADIAN. ) );
#63784 = CARTESIAN_POINT ( 'NONE',  ( 10.39230484541327115, -3.482307324624967703E-15, 1.392304845413258718 ) ) ;
#63786 = EDGE_CURVE ( 'NONE', #17866, #15233, #6137, .T. ) ;
#63785 = VECTOR ( 'NONE', #36085, 1000.000000000000000 ) ;
#63787 = CARTESIAN_POINT ( 'NONE',  ( -2.607480562269116842, 149.4070736234661751, 8.024999999999970157 ) ) ;
#63788 = CARTESIAN_POINT ( 'NONE',  ( -20.77895614775982125, 115.1380991538496801, -10.00000000000000000 ) ) ;
#63789 = DIRECTION ( 'NONE',  ( 1.000000000000000000, -0.000000000000000000, -1.300977106640434891E-16 ) ) ;
#63790 = ORIENTED_EDGE ( 'NONE', *, *, #33058, .F. ) ;
#63791 = CARTESIAN_POINT ( 'NONE',  ( -77.54292637653379927, 9.058813317711329915, 2.943386871421369566 ) ) ;
#63792 = ITEM_DEFINED_TRANSFORMATION ( 'NONE', 'NONE', #65231,  #42840 ) ;
#63793 = FACE_BOUND ( 'NONE', #30323, .T. ) ;
#63794 = CARTESIAN_POINT ( 'NONE',  ( -165.5929263765340238, -3.094860106622363993, -9.524999999997135092 ) ) ;
#63795 = CARTESIAN_POINT ( 'NONE',  ( 7.632228543268607446, 147.1570736234661751, 2.479861379858954606 ) ) ;
#63796 = CARTESIAN_POINT ( 'NONE',  ( 57.00000000000000000, 13.00000000000000178, -79.00402776293826435 ) ) ;
#63797 = CARTESIAN_POINT ( 'NONE',  ( -176.6049999999999898, 6.826472737025113702, -4.959722759717902107 ) ) ;
#63798 = ORIENTED_EDGE ( 'NONE', *, *, #38969, .T. ) ;
#63799 = SURFACE_STYLE_FILL_AREA ( #47700 ) ;
#63800 = FILL_AREA_STYLE_COLOUR ( '', #54443 ) ;
#63801 = CARTESIAN_POINT ( 'NONE',  ( -74.60707362346617799, -8.102448949553174629, 5.886773742842742685 ) ) ;
#63802 = CYLINDRICAL_SURFACE ( 'NONE', #49892, 8.025000000000000355 ) ;
#63803 =( NAMED_UNIT ( * ) PLANE_ANGLE_UNIT ( ) SI_UNIT ( $, .RADIAN. ) );
#63804 = CARTESIAN_POINT ( 'NONE',  ( -2.607480562269073765, 142.2070736234661297, -8.025000000000000355 ) ) ;
#63805 = EDGE_LOOP ( 'NONE', ( #60167, #23922, #46658, #35088 ) ) ;
#63806 = DIRECTION ( 'NONE',  ( -0.000000000000000000, -0.000000000000000000, -1.000000000000000000 ) ) ;
#63807 = CARTESIAN_POINT ( 'NONE',  ( -88.55499999999999261, 0.000000000000000000, 8.024999999999991473 ) ) ;
#63808 = UNCERTAINTY_MEASURE_WITH_UNIT (LENGTH_MEASURE( 1.000000000000000082E-05 ), #59382, 'distance_accuracy_value', 'NONE');
#63809 = CARTESIAN_POINT ( 'NONE',  ( 2.607480562269113733, 131.7070736234662149, 8.024999999999973710 ) ) ;
#63810 = AXIS2_PLACEMENT_3D ( 'NONE', #24039, #18427, #3579 ) ;
#63811 = ORIENTED_EDGE ( 'NONE', *, *, #24437, .F. ) ;
#63812 = AXIS2_PLACEMENT_3D ( 'NONE', #20603, #57544, #31835 ) ;
#63813 = DIRECTION ( 'NONE',  ( 0.000000000000000000, 0.000000000000000000, 1.000000000000000000 ) ) ;
#63814 = LINE ( 'NONE', #54298, #29910 ) ;
#63815 = DIRECTION ( 'NONE',  ( 0.000000000000000000, -1.000000000000000000, 0.000000000000000000 ) ) ;
#63816 = ORIENTED_EDGE ( 'NONE', *, *, #67769, .F. ) ;
#63817 = COLOUR_RGB ( '', 0.08235294, 0.09019608, 0.10196078) ;
#63818 = CARTESIAN_POINT ( 'NONE',  ( 57.49999999999999289, 28.24999999999998934, 4.000000000000000000 ) ) ;
#63819 = CARTESIAN_POINT ( 'NONE',  ( -70.79499999999998749, 2.607480562269068880, -8.024999999999993250 ) ) ;
#63820 = ORIENTED_EDGE ( 'NONE', *, *, #26668, .T. ) ;
#63821 = DIRECTION ( 'NONE',  ( -0.7833176619561783571, 0.6216216216216310375, -0.000000000000000000 ) ) ;
#63822 = CARTESIAN_POINT ( 'NONE',  ( 8.373843646579334887, 5.621768377696955810, -11.90713709031378897 ) ) ;
#63823 = ORIENTED_EDGE ( 'NONE', *, *, #51478, .T. ) ;
#63824 = DIRECTION ( 'NONE',  ( 1.000000000000000000, 0.000000000000000000, -0.000000000000000000 ) ) ;
#63825 = FACE_OUTER_BOUND ( 'NONE', #55858, .T. ) ;
#63826 = VECTOR ( 'NONE', #29957, 1000.000000000000000 ) ;
#63827 = DIRECTION ( 'NONE',  ( 1.000000000000000000, 0.000000000000000000, 0.000000000000000000 ) ) ;
#63828 = VERTEX_POINT ( 'NONE', #30890 ) ;
#63829 = CARTESIAN_POINT ( 'NONE',  ( 57.00000000000000000, 16.00000000000000000, -72.50402776293826435 ) ) ;
#63831 = VERTEX_POINT ( 'NONE', #25603 ) ;
#63830 = EDGE_CURVE ( 'NONE', #20856, #13735, #3904, .T. ) ;
#63832 = FILL_AREA_STYLE ('',( #42441 ) ) ;
#63833 = SURFACE_STYLE_USAGE ( .BOTH. , #17074 ) ;
#63834 = CARTESIAN_POINT ( 'NONE',  ( -159.8070736234662093, 10.01517768586948698, -1.839758294383808571E-15 ) ) ;
#63835 = CARTESIAN_POINT ( 'NONE',  ( -3.094860106618432471, 121.5949999999999847, -9.525000000000000355 ) ) ;
#63836 = EDGE_CURVE ( 'NONE', #11552, #4457, #2727, .T. ) ;
#63837 = CARTESIAN_POINT ( 'NONE',  ( -103.4070736234661751, 3.094860106618428031, -9.524999999999993250 ) ) ;
#63838 = EDGE_CURVE ( 'NONE', #26540, #2804, #42144, .T. ) ;
#63839 = AXIS2_PLACEMENT_3D ( 'NONE', #18709, #22950, #66548 ) ;
#63840 = DIRECTION ( 'NONE',  ( 0.000000000000000000, -1.000000000000000000, 0.000000000000000000 ) ) ;
#63841 = ORIENTED_EDGE ( 'NONE', *, *, #48281, .F. ) ;
#63842 = CARTESIAN_POINT ( 'NONE',  ( -15.48999599679679662, 117.9999999999999716, 7.500000000000000000 ) ) ;
#63843 = ADVANCED_FACE ( 'NONE', ( #41146 ), #42813, .F. ) ;
#63844 = FACE_OUTER_BOUND ( 'NONE', #19513, .T. ) ;
#63845 = CIRCLE ( 'NONE', #33526, 5.000000000000004441 ) ;
#63846 = CARTESIAN_POINT ( 'NONE',  ( -142.8550000000000182, 4.716976649647094177, 6.492361379858945902 ) ) ;
#63847 = EDGE_CURVE ( 'NONE', #11851, #7249, #46664, .T. ) ;
#63848 = FILL_AREA_STYLE_COLOUR ( '', #57764 ) ;
#63849 = CARTESIAN_POINT ( 'NONE',  ( 0.000000000000000000, 42.00000000000000711, 44.99999999999999289 ) ) ;
#63850 = CARTESIAN_POINT ( 'NONE',  ( -153.5949999999999989, 2.607480562269073321, 8.024999999999991473 ) ) ;
#63851 = ADVANCED_FACE ( 'NONE', ( #14737 ), #38768, .T. ) ;
#63852 =( GEOMETRIC_REPRESENTATION_CONTEXT ( 3 ) GLOBAL_UNCERTAINTY_ASSIGNED_CONTEXT ( ( #57358 ) ) GLOBAL_UNIT_ASSIGNED_CONTEXT ( ( #58122, #21503, #43021 ) ) REPRESENTATION_CONTEXT ( 'NONE', 'WORKASPACE' ) );
#63853 = CARTESIAN_POINT ( 'NONE',  ( -133.7949999999999875, 2.607480562269069324, -8.024999999999993250 ) ) ;
#63854 = EDGE_CURVE ( 'NONE', #38669, #3572, #59435, .T. ) ;
#63855 = ORIENTED_EDGE ( 'NONE', *, *, #49187, .T. ) ;
#63856 =( BOUNDED_CURVE ( )  B_SPLINE_CURVE ( 2, ( #10609, #25390, #53183, #69013, #26074, #53517, #47954, #63711, #68315, #20094, #58445 ),
 .UNSPECIFIED., .F., .F. ) 
 B_SPLINE_CURVE_WITH_KNOTS ( ( 3, 2, 2, 2, 2, 3 ),
 ( 0.1176470588235295212, 0.1235294117647059986, 0.1294117647058824760, 0.1352941176470589257, 0.1411764705882354032, 0.1470588235294118806 ),
 .UNSPECIFIED. ) 
 CURVE ( )  GEOMETRIC_REPRESENTATION_ITEM ( )  RATIONAL_B_SPLINE_CURVE ( ( 0.9999999999999991118, 0.9510565162951544194, 1.000000000000000000, 0.9510565162951535312, 1.000000000000000000, 0.9510565162951535312, 1.000000000000000000, 0.9510565162951535312, 1.000000000000000000, 0.9510565162951526430, 1.000000000000000888 ) ) 
 REPRESENTATION_ITEM ( '' )  );
#63857 = DIRECTION ( 'NONE',  ( 1.000000000000000000, -0.000000000000000000, 0.000000000000000000 ) ) ;
#63858 = DIRECTION ( 'NONE',  ( 0.000000000000000000, 1.000000000000000000, 0.000000000000000000 ) ) ;
#63859 = ADVANCED_FACE ( 'NONE', ( #48421 ), #51671, .F. ) ;
#63860 = CYLINDRICAL_SURFACE ( 'NONE', #53007, 13.99999999999999822 ) ;
#63861 = CARTESIAN_POINT ( 'NONE',  ( -51.20499999999996277, -2.607480562269071545, -8.024999999999991473 ) ) ;
#63862 = CARTESIAN_POINT ( 'NONE',  ( 34.99999999999992895, 110.4999999999999858, -9.500000000000000000 ) ) ;
#63863 = COLOUR_RGB ( '', 0.72549020, 0.75294118, 0.79215686) ;
#63864 = AXIS2_PLACEMENT_3D ( 'NONE', #31754, #63768, #36021 ) ;
#63865 = CARTESIAN_POINT ( 'NONE',  ( -138.7429263765338021, -5.598654528085803328, -7.705886871421366635 ) ) ;
#63866 = CARTESIAN_POINT ( 'NONE',  ( 4.000000000000029310, 34.36176364315826248, 80.00402776293826435 ) ) ;
#63867 = AXIS2_PLACEMENT_3D ( 'NONE', #20604, #30432, #20246 ) ;
#63868 = CARTESIAN_POINT ( 'NONE',  ( -4.299999999999977618, 26.00000000000000355, 23.99999999999999289 ) ) ;
#63869 = AXIS2_PLACEMENT_3D ( 'NONE', #10122, #26274, #60020 ) ;
#63870 = SURFACE_SIDE_STYLE ('',( #3720 ) ) ;
#63871 = STYLED_ITEM ( 'NONE', ( #37703 ), #68068 ) ;
#63872 = DIRECTION ( 'NONE',  ( 0.000000000000000000, 0.000000000000000000, -1.000000000000000000 ) ) ;
#63873 = FACE_OUTER_BOUND ( 'NONE', #6229, .T. ) ;
#63874 = DIRECTION ( 'NONE',  ( 0.000000000000000000, 0.000000000000000000, 1.000000000000000000 ) ) ;
#63875 = CARTESIAN_POINT ( 'NONE',  ( 27.99999999999999645, 5.000000000000000000, 24.00402776293821816 ) ) ;
#63876 = ORIENTED_EDGE ( 'NONE', *, *, #25404, .F. ) ;
#63877 = CARTESIAN_POINT ( 'NONE',  ( 2.607480562269076430, 117.9070736234661467, -8.025000000000000355 ) ) ;
#63878 = ADVANCED_FACE ( 'NONE', ( #33580 ), #17770, .T. ) ;
#63879 = AXIS2_PLACEMENT_3D ( 'NONE', #11170, #21039, #52720 ) ;
#63880 = CARTESIAN_POINT ( 'NONE',  ( -20.26251832593580104, 115.0246525964671207, 10.00000000000000178 ) ) ;
#63881 = FACE_OUTER_BOUND ( 'NONE', #58377, .T. ) ;
#63882 = ORIENTED_EDGE ( 'NONE', *, *, #63967, .T. ) ;
#63884 = ORIENTED_EDGE ( 'NONE', *, *, #14553, .T. ) ;
#63883 = TOROIDAL_SURFACE ( 'NONE', #16776, 8.499999999999998224, 0.5000000000000000000 ) ;
#63885 = CARTESIAN_POINT ( 'NONE',  ( 48.25000000000000000, 22.24999999999998579, -4.000000000000000000 ) ) ;
#63886 = CARTESIAN_POINT ( 'NONE',  ( 3.000000000000002665, 34.36176364315826248, -80.00402776293826435 ) ) ;
#63887 = VERTEX_POINT ( 'NONE', #55017 ) ;
#63888 = CARTESIAN_POINT ( 'NONE',  ( -10.01517768586949231, 123.3049999999999926, -6.132527647946036459E-16 ) ) ;
#63889 = CARTESIAN_POINT ( 'NONE',  ( -15.48999599679679662, 117.9999999999999716, 7.000000000000000000 ) ) ;
#63890 = VECTOR ( 'NONE', #69243, 1000.000000000000000 ) ;
#63891 = AXIS2_PLACEMENT_3D ( 'NONE', #28046, #49553, #6973 ) ;
#63892 = CARTESIAN_POINT ( 'NONE',  ( -18.25000000000000711, 33.99999999999999289, 4.000000000000000000 ) ) ;
#63893 = CARTESIAN_POINT ( 'NONE',  ( -103.1950000000000074, 8.437984349512085203, -1.550032578732815448E-15 ) ) ;
#63894 = ORIENTED_EDGE ( 'NONE', *, *, #57762, .T. ) ;
#63895 = FACE_OUTER_BOUND ( 'NONE', #48219, .T. ) ;
#63896 = DIRECTION ( 'NONE',  ( 0.000000000000000000, 0.000000000000000000, 1.000000000000000000 ) ) ;
#63897 = DIRECTION ( 'NONE',  ( 0.000000000000000000, -0.000000000000000000, 1.000000000000000000 ) ) ;
#63898 = ORIENTED_EDGE ( 'NONE', *, *, #59944, .T. ) ;
#63899 = CARTESIAN_POINT ( 'NONE',  ( 4.716976649647096842, 154.7429263765338021, 6.492361379858953896 ) ) ;
#63900 = FILL_AREA_STYLE ('',( #42504 ) ) ;
#63901 = AXIS2_PLACEMENT_3D ( 'NONE', #33259, #1167, #4610 ) ;
#63902 = MECHANICAL_DESIGN_GEOMETRIC_PRESENTATION_REPRESENTATION (  '', ( #24582 ), #907 ) ;
#63903 = CARTESIAN_POINT ( 'NONE',  ( 0.000000000000000000, 0.000000000000000000, 0.2499999999999941436 ) ) ;
#63904 = DIRECTION ( 'NONE',  ( -1.000000000000000000, 0.000000000000000000, -0.000000000000000000 ) ) ;
#63905 = EDGE_CURVE ( 'NONE', #59935, #27359, #14077, .T. ) ;
#63906 = CARTESIAN_POINT ( 'NONE',  ( -62.45707362346617231, -9.058813317711329915, 2.943386871421371787 ) ) ;
#63907 = VERTEX_POINT ( 'NONE', #54681 ) ;
#63908 = CYLINDRICAL_SURFACE ( 'NONE', #51843, 1.000000000000000000 ) ;
#63909 = CARTESIAN_POINT ( 'NONE',  ( 23.21231517720798010, 113.4999999999999858, -10.00000000000000000 ) ) ;
#63910 = CARTESIAN_POINT ( 'NONE',  ( 0.000000000000000000, 2.500000000000000000, 5.500000000000001776 ) ) ;
#63912 = CIRCLE ( 'NONE', #42634, 0.2500000000000002220 ) ;
#63911 = CARTESIAN_POINT ( 'NONE',  ( -34.93094464088179052, -9.512283121613265280, 4.966208934664647856 ) ) ;
#63913 = CARTESIAN_POINT ( 'NONE',  ( 3.249999999999998668, 36.74999999999999289, -4.000000000000000000 ) ) ;
#63914 = VECTOR ( 'NONE', #48331, 1000.000000000000000 ) ;
#63915 = EDGE_CURVE ( 'NONE', #34757, #32368, #48771, .T. ) ;
#63916 = CARTESIAN_POINT ( 'NONE',  ( -125.9929263765338021, 8.102448949553172852, -5.886773742842744461 ) ) ;
#63917 = LINE ( 'NONE', #64271, #30500 ) ;
#63918 = CARTESIAN_POINT ( 'NONE',  ( -4.716976649647098618, 121.1429263765338220, 6.492361379858953008 ) ) ;
#63919 = DIRECTION ( 'NONE',  ( 0.000000000000000000, 0.000000000000000000, 1.000000000000000000 ) ) ;
#63920 = ORIENTED_EDGE ( 'NONE', *, *, #21882, .F. ) ;
#63921 = AXIS2_PLACEMENT_3D ( 'NONE', #26631, #68898, #27319 ) ;
#63922 = ORIENTED_EDGE ( 'NONE', *, *, #10096, .F. ) ;
#63923 = FILL_AREA_STYLE_COLOUR ( '', #17151 ) ;
#63924 = DIRECTION ( 'NONE',  ( 0.000000000000000000, -0.000000000000000000, 1.000000000000000000 ) ) ;
#63925 = DIRECTION ( 'NONE',  ( 0.000000000000000000, 0.000000000000000000, 1.000000000000000000 ) ) ;
#63926 = SURFACE_SIDE_STYLE ('',( #49509 ) ) ;
#63927 = VERTEX_POINT ( 'NONE', #5789 ) ;
#63928 = CARTESIAN_POINT ( 'NONE',  ( -169.7050000000000125, 2.607480562269073321, 8.024999999999991473 ) ) ;
#63929 = CARTESIAN_POINT ( 'NONE',  ( 0.000000000000000000, 0.000000000000000000, 1.000000000000000000 ) ) ;
#63930 = DIRECTION ( 'NONE',  ( 0.000000000000000000, 1.000000000000000000, -0.000000000000000000 ) ) ;
#63931 = CARTESIAN_POINT ( 'NONE',  ( -49.85707362346617089, -5.598654528085803328, -7.705886871421366635 ) ) ;
#63932 = EDGE_CURVE ( 'NONE', #62258, #25953, #33850, .T. ) ;
#63933 = CARTESIAN_POINT ( 'NONE',  ( -166.4950000000000045, 6.826472737025113702, -4.959722759717902107 ) ) ;
#63934 = ORIENTED_EDGE ( 'NONE', *, *, #5307, .T. ) ;
#63935 = SURFACE_STYLE_USAGE ( .BOTH. , #16142 ) ;
#63937 = FACE_BOUND ( 'NONE', #41542, .T. ) ;
#63936 = MECHANICAL_DESIGN_GEOMETRIC_PRESENTATION_REPRESENTATION (  '', ( #52774 ), #5521 ) ;
#63938 = ADVANCED_FACE ( 'NONE', ( #50129 ), #56764, .T. ) ;
#63939 = CARTESIAN_POINT ( 'NONE',  ( -12.76923511868948502, 11.13042849027246817, 4.486927442365898244 ) ) ;
#63940 = CARTESIAN_POINT ( 'NONE',  ( -85.40499999999998693, -2.607480562269069768, 8.024999999999991473 ) ) ;
#63941 = CYLINDRICAL_SURFACE ( 'NONE', #9575, 9.524999999999991473 ) ;
#63942 = CARTESIAN_POINT ( 'NONE',  ( 66.74999999999998579, 37.00000000000000000, -3.750000000000000000 ) ) ;
#63943 = CARTESIAN_POINT ( 'NONE',  ( -74.71853681387480606, 36.06263896201981112, -9.953338452735643216 ) ) ;
#63944 = MECHANICAL_DESIGN_GEOMETRIC_PRESENTATION_REPRESENTATION (  '', ( #50501 ), #59460 ) ;
#63945 = CARTESIAN_POINT ( 'NONE',  ( -83.99499999999999034, -6.826472737025113702, 4.959722759717902107 ) ) ;
#63946 = CARTESIAN_POINT ( 'NONE',  ( 0.000000000000000000, 128.5549999999999784, -9.525000000000000355 ) ) ;
#63947 = CARTESIAN_POINT ( 'NONE',  ( 20.20529291564252716, 114.9650358309326492, -10.39743153126989128 ) ) ;
#63948 = VECTOR ( 'NONE', #51169, 1000.000000000000000 ) ;
#63949 =( GEOMETRIC_REPRESENTATION_CONTEXT ( 3 ) GLOBAL_UNCERTAINTY_ASSIGNED_CONTEXT ( ( #60888 ) ) GLOBAL_UNIT_ASSIGNED_CONTEXT ( ( #23417, #39636, #62087 ) ) REPRESENTATION_CONTEXT ( 'NONE', 'WORKASPACE' ) );
#63950 = CARTESIAN_POINT ( 'NONE',  ( -171.5070736234661695, 8.102448949553176405, 5.886773742842740909 ) ) ;
#63951 = DIRECTION ( 'NONE',  ( 0.7071067811865451302, 8.659560562354903276E-17, -0.7071067811865500152 ) ) ;
#63952 = AXIS2_PLACEMENT_3D ( 'NONE', #6434, #32836, #10693 ) ;
#63953 = VECTOR ( 'NONE', #38888, 1000.000000000000000 ) ;
#63954 = FILL_AREA_STYLE_COLOUR ( '', #64072 ) ;
#63955 = AXIS2_PLACEMENT_3D ( 'NONE', #43101, #32842, #16355 ) ;
#63956 = EDGE_LOOP ( 'NONE', ( #54865, #13014, #27725, #62538 ) ) ;
#63957 = DIRECTION ( 'NONE',  ( 0.000000000000000000, 1.000000000000000000, 0.000000000000000000 ) ) ;
#63958 = AXIS2_PLACEMENT_3D ( 'NONE', #26737, #6341, #33094 ) ;
#63959 = DIRECTION ( 'NONE',  ( 0.000000000000000000, -1.000000000000000000, 0.000000000000000000 ) ) ;
#63961 = DIRECTION ( 'NONE',  ( -1.000000000000000000, -0.000000000000000000, -0.000000000000000000 ) ) ;
#63960 = CARTESIAN_POINT ( 'NONE',  ( 66.24999999999998579, 33.99999999999999289, 3.750000000000000000 ) ) ;
#63962 = DIRECTION ( 'NONE',  ( 1.000000000000000000, 0.000000000000000000, 0.000000000000000000 ) ) ;
#63963 = ORIENTED_EDGE ( 'NONE', *, *, #6195, .T. ) ;
#63964 = VERTEX_POINT ( 'NONE', #18101 ) ;
#63965 = CARTESIAN_POINT ( 'NONE',  ( -45.86897471612435595, 9.253287829606158255, -6.241231906388602368 ) ) ;
#63966 = CARTESIAN_POINT ( 'NONE',  ( 2.607480562269093305, 130.5929263765337964, 8.024999999999986144 ) ) ;
#63967 = EDGE_CURVE ( 'NONE', #29123, #29357, #18785, .T. ) ;
#63968 = PRESENTATION_STYLE_ASSIGNMENT (( #16176 ) ) ;
#63969 = VECTOR ( 'NONE', #31142, 1000.000000000000000 ) ;
#63970 = SURFACE_SIDE_STYLE ('',( #25639 ) ) ;
#63971 = CARTESIAN_POINT ( 'NONE',  ( 60.00000000000000000, 1.797044900979284448E-15, 11.50000000000000000 ) ) ;
#63972 = ORIENTED_EDGE ( 'NONE', *, *, #67492, .T. ) ;
#63973 = CARTESIAN_POINT ( 'NONE',  ( -122.1549999999999869, 7.632228543268600340, 2.479861379858949277 ) ) ;
#63974 = EDGE_LOOP ( 'NONE', ( #35441, #36387, #26543 ) ) ;
#63975 = DIRECTION ( 'NONE',  ( -1.000000000000000000, 0.000000000000000000, 0.000000000000000000 ) ) ;
#63976 = CARTESIAN_POINT ( 'NONE',  ( 20.86757785789463071, 115.0275815560950718, -10.00000000000000000 ) ) ;
#63977 = ORIENTED_EDGE ( 'NONE', *, *, #9307, .T. ) ;
#63978 = DIRECTION ( 'NONE',  ( -1.156482317317866302E-16, -1.000000000000000000, -2.430666987508116652E-16 ) ) ;
#63979 = DIRECTION ( 'NONE',  ( -1.000000000000000000, 0.000000000000000000, 0.000000000000000000 ) ) ;
#63980 = VERTEX_POINT ( 'NONE', #28970 ) ;
#63981 = PRESENTATION_LAYER_ASSIGNMENT (  '', '', ( #59452 ) ) ;
#63983 =( NAMED_UNIT ( * ) PLANE_ANGLE_UNIT ( ) SI_UNIT ( $, .RADIAN. ) );
#63982 = STYLED_ITEM ( 'NONE', ( #27981 ), #58704 ) ;
#63984 = CARTESIAN_POINT ( 'NONE',  ( -3.094860106618432471, 154.5949999999999704, -9.525000000000000355 ) ) ;
#63985 = B_SPLINE_CURVE_WITH_KNOTS ( 'NONE', 3,
 ( #20553, #52592, #36443, #30748, #41007, #26166, #3643, #46992 ),
 .UNSPECIFIED., .F., .F.,
 ( 4, 2, 2, 4 ),
 ( 2.544313220888523934E-07, 0.002693395767724531854, 0.004039966435925753697, 0.005386537104126975541 ),
 .UNSPECIFIED. ) ;
#63986 = LINE ( 'NONE', #58048, #16080 ) ;
#63987 = ORIENTED_EDGE ( 'NONE', *, *, #3614, .F. ) ;
#63988 = CARTESIAN_POINT ( 'NONE',  ( 9.058813317711338797, 145.9550000000000125, -2.943386871421372675 ) ) ;
#63989 = FILL_AREA_STYLE_COLOUR ( '', #49672 ) ;
#63990 = VECTOR ( 'NONE', #18715, 1000.000000000000000 ) ;
#63991 = CARTESIAN_POINT ( 'NONE',  ( -130.4929263765338021, -8.102448949553174629, 5.886773742842742685 ) ) ;
#63992 = ORIENTED_EDGE ( 'NONE', *, *, #64809, .T. ) ;
#63993 = CARTESIAN_POINT ( 'NONE',  ( 0.000000000000000000, 122.9429263765338192, -8.025000000000000355 ) ) ;
#63994 = DIRECTION ( 'NONE',  ( -1.000000000000000000, 0.000000000000000000, 0.000000000000000000 ) ) ;
#63995 = CARTESIAN_POINT ( 'NONE',  ( -75.25488889474493703, 36.12129367854308981, -9.832813668515733241 ) ) ;
#63996 = ADVANCED_FACE ( 'NONE', ( #51858 ), #69416, .T. ) ;
#63997 = DIRECTION ( 'NONE',  ( 1.000000000000000000, 0.000000000000000000, 0.000000000000000000 ) ) ;
#63998 = DIRECTION ( 'NONE',  ( -0.000000000000000000, -0.000000000000000000, 1.000000000000000000 ) ) ;
#63999 = EDGE_CURVE ( 'NONE', #42883, #529, #10708, .T. ) ;
#64000 = ORIENTED_EDGE ( 'NONE', *, *, #16153, .T. ) ;
#64001 = MECHANICAL_DESIGN_GEOMETRIC_PRESENTATION_REPRESENTATION (  '', ( #11230 ), #44965 ) ;
#64002 = CARTESIAN_POINT ( 'NONE',  ( -41.84210526315788314, 107.2928455055531600, -4.000000000000000000 ) ) ;
#64003 = ORIENTED_EDGE ( 'NONE', *, *, #32174, .T. ) ;
#64004 = CARTESIAN_POINT ( 'NONE',  ( -62.09292637653379643, 3.094860106618433360, 9.524999999999991473 ) ) ;
#64005 = COLOUR_RGB ( '', 0.72549020, 0.75294118, 0.79215686) ;
#64006 = CARTESIAN_POINT ( 'NONE',  ( -6.418790567836333949, 2.882328613363593917, 0.02778322089669647138 ) ) ;
#64007 = CARTESIAN_POINT ( 'NONE',  ( -146.0050000000000239, 6.826472737025116366, 4.959722759717898555 ) ) ;
#64008 = CARTESIAN_POINT ( 'NONE',  ( 61.99999999999998579, 33.99999999999999289, 3.750000000000000000 ) ) ;
#64009 = CIRCLE ( 'NONE', #43866, 1.000000000000001998 ) ;
#64010 = CARTESIAN_POINT ( 'NONE',  ( 69.99999999999998579, 8.572527594031471415E-15, 3.000000000000000000 ) ) ;
#64011 = EDGE_CURVE ( 'NONE', #11115, #52209, #54003, .T. ) ;
#64012 = AXIS2_PLACEMENT_3D ( 'NONE', #46604, #8230, #40960 ) ;
#64013 = SURFACE_STYLE_FILL_AREA ( #26380 ) ;
#64014 = SURFACE_STYLE_FILL_AREA ( #23109 ) ;
#64015 = EDGE_LOOP ( 'NONE', ( #68239, #64849, #51364 ) ) ;
#64017 = EDGE_CURVE ( 'NONE', #66508, #67023, #17465, .T. ) ;
#64016 = ORIENTED_EDGE ( 'NONE', *, *, #28088, .T. ) ;
#64018 = CARTESIAN_POINT ( 'NONE',  ( -22.25000000000000711, 34.24999999999999289, 4.000000000000000000 ) ) ;
#64019 = CARTESIAN_POINT ( 'NONE',  ( -67.55499999999999261, 0.000000000000000000, 8.024999999999991473 ) ) ;
#64020 = VERTEX_POINT ( 'NONE', #11090 ) ;
#64021 = CARTESIAN_POINT ( 'NONE',  ( 27.00000000000001776, 15.00000000000000000, -34.49999999999999289 ) ) ;
#64022 = SURFACE_SIDE_STYLE ('',( #42616 ) ) ;
#64023 = CYLINDRICAL_SURFACE ( 'NONE', #295, 0.2500000000000002220 ) ;
#64024 =( LENGTH_UNIT ( ) NAMED_UNIT ( * ) SI_UNIT ( .MILLI., .METRE. ) );
#64025 = ADVANCED_FACE ( 'NONE', ( #38222 ), #64211, .F. ) ;
#64026 = PRESENTATION_LAYER_ASSIGNMENT (  '', '', ( #67388 ) ) ;
#64027 =( LENGTH_UNIT ( ) NAMED_UNIT ( * ) SI_UNIT ( .MILLI., .METRE. ) );
#64028 = CARTESIAN_POINT ( 'NONE',  ( 13.75000000000000533, 30.74999999999999289, -3.750000000000000000 ) ) ;
#64029 = EDGE_LOOP ( 'NONE', ( #23481, #31974, #44219, #14702 ) ) ;
#64030 = CARTESIAN_POINT ( 'NONE',  ( 5.196152422706631135, -1.107695154586740394, 9.000000000000001776 ) ) ;
#64031 = EDGE_CURVE ( 'NONE', #50251, #4472, #36602, .T. ) ;
#64032 = CARTESIAN_POINT ( 'NONE',  ( 31.00000000000000000, 14.00000000000000000, -80.00402776293826435 ) ) ;
#64033 =( NAMED_UNIT ( * ) SI_UNIT ( $, .STERADIAN. ) SOLID_ANGLE_UNIT ( ) );
#64034 = COLOUR_RGB ( '', 0.09019608, 0.27058824, 0.51372549) ;
#64035 = CARTESIAN_POINT ( 'NONE',  ( 6.826472737025119919, 126.0070736234661695, 4.959722759717908325 ) ) ;
#64036 = CARTESIAN_POINT ( 'NONE',  ( -113.0949999999999847, -2.607480562269071545, -8.024999999999991473 ) ) ;
#64037 = CARTESIAN_POINT ( 'NONE',  ( -3.094860106618434248, 152.7949999999999591, 9.525000000000000355 ) ) ;
#64038 = CARTESIAN_POINT ( 'NONE',  ( -92.09499999999998465, -2.607480562269071545, -8.024999999999991473 ) ) ;
#64039 =( NAMED_UNIT ( * ) SI_UNIT ( $, .STERADIAN. ) SOLID_ANGLE_UNIT ( ) );
#64040 = SURFACE_SIDE_STYLE ('',( #48953 ) ) ;
#64041 = MECHANICAL_DESIGN_GEOMETRIC_PRESENTATION_REPRESENTATION (  '', ( #23564 ), #29171 ) ;
#64042 = CARTESIAN_POINT ( 'NONE',  ( 15.48999599679679662, 147.4999999999999716, -10.00000000000000000 ) ) ;
#64044 = VERTEX_POINT ( 'NONE', #16424 ) ;
#64043 = VECTOR ( 'NONE', #37631, 1000.000000000000000 ) ;
#64045 = CARTESIAN_POINT ( 'NONE',  ( -130.7929263765338135, -3.094860106618429807, 9.524999999999991473 ) ) ;
#64046 = CYLINDRICAL_SURFACE ( 'NONE', #30987, 9.524999999999991473 ) ;
#64047 = CARTESIAN_POINT ( 'NONE',  ( -146.9950000000000045, -6.826472737025115478, 4.959722759717900331 ) ) ;
#64048 = CARTESIAN_POINT ( 'NONE',  ( 25.00000000000000355, 37.00000000000000000, 3.750000000000000000 ) ) ;
#64049 = CARTESIAN_POINT ( 'NONE',  ( -46.64499999999998892, 4.716976649647091513, -6.492361379858946790 ) ) ;
#64050 = STYLED_ITEM ( 'NONE', ( #636 ), #11205 ) ;
#64051 = DIRECTION ( 'NONE',  ( 1.000000000000000000, 0.000000000000000000, 0.000000000000000000 ) ) ;
#64052 = ORIENTED_EDGE ( 'NONE', *, *, #42237, .F. ) ;
#64053 = EDGE_LOOP ( 'NONE', ( #58566, #10524, #65807 ) ) ;
#64054 = DIRECTION ( 'NONE',  ( 1.000000000000000000, 0.000000000000000000, 0.000000000000000000 ) ) ;
#64055 = PRESENTATION_LAYER_ASSIGNMENT (  '', '', ( #29196 ) ) ;
#64056 = CARTESIAN_POINT ( 'NONE',  ( 10.50000000000000178, 8.000000000000000000, 4.000000000000000000 ) ) ;
#64057 = CARTESIAN_POINT ( 'NONE',  ( -45.00000000000000000, 9.118333594695746669, 6.737587966311194165 ) ) ;
#64058 = DIRECTION ( 'NONE',  ( -0.000000000000000000, -0.000000000000000000, 1.000000000000000000 ) ) ;
#64059 = VECTOR ( 'NONE', #32220, 1000.000000000000227 ) ;
#64060 =( NAMED_UNIT ( * ) PLANE_ANGLE_UNIT ( ) SI_UNIT ( $, .RADIAN. ) );
#64061 = ORIENTED_EDGE ( 'NONE', *, *, #60170, .T. ) ;
#64062 = CARTESIAN_POINT ( 'NONE',  ( -153.9550000000000125, -7.632228543268599452, 2.479861379858951054 ) ) ;
#64063 = ORIENTED_EDGE ( 'NONE', *, *, #48343, .T. ) ;
#64064 = CARTESIAN_POINT ( 'NONE',  ( -9.000000000000003553, 25.24999999999998934, -4.000000000000000000 ) ) ;
#64065 = CARTESIAN_POINT ( 'NONE',  ( 45.00000000000000000, -1.469576158976824618E-14, 9.500000000000000000 ) ) ;
#64066 = VERTEX_POINT ( 'NONE', #59979 ) ;
#64067 = VECTOR ( 'NONE', #33080, 1000.000000000000000 ) ;
#64068 = CARTESIAN_POINT ( 'NONE',  ( 1.000000000000000000, 42.00000000000000000, 0.000000000000000000 ) ) ;
#64069 = DIRECTION ( 'NONE',  ( 0.000000000000000000, 0.000000000000000000, 1.000000000000000000 ) ) ;
#64070 = CARTESIAN_POINT ( 'NONE',  ( -8.102448949553181734, 116.4949999999999761, 5.886773742842747126 ) ) ;
#64071 =( LENGTH_UNIT ( ) NAMED_UNIT ( * ) SI_UNIT ( .MILLI., .METRE. ) );
#64072 = COLOUR_RGB ( '', 0.08235294, 0.09019608, 0.10196078) ;
#64073 = ORIENTED_EDGE ( 'NONE', *, *, #26385, .F. ) ;
#64074 = EDGE_CURVE ( 'NONE', #45200, #61112, #42466, .T. ) ;
#64075 = PLANE ( 'NONE',  #2611 ) ;
#64076 = CARTESIAN_POINT ( 'NONE',  ( -5.598654528085808657, 123.7549999999999955, 7.705886871421373741 ) ) ;
#64077 = CARTESIAN_POINT ( 'NONE',  ( -62.00499999999998835, 6.826472737025115478, 4.959722759717899443 ) ) ;
#64078 = CARTESIAN_POINT ( 'NONE',  ( -123.8949999999999676, 6.826472737025116366, 4.959722759717898555 ) ) ;
#64079 = DIRECTION ( 'NONE',  ( -1.156482317317873451E-16, -1.000000000000000000, 0.000000000000000000 ) ) ;
#64080 = ORIENTED_EDGE ( 'NONE', *, *, #18960, .T. ) ;
#64081 = CARTESIAN_POINT ( 'NONE',  ( 9.058813317711337021, 151.6549999999999727, 2.943386871421375783 ) ) ;
#64082 =( GEOMETRIC_REPRESENTATION_CONTEXT ( 3 ) GLOBAL_UNCERTAINTY_ASSIGNED_CONTEXT ( ( #47405 ) ) GLOBAL_UNIT_ASSIGNED_CONTEXT ( ( #61763, #24479, #40716 ) ) REPRESENTATION_CONTEXT ( 'NONE', 'WORKASPACE' ) );
#64083 = ADVANCED_FACE ( 'NONE', ( #5806 ), #11442, .F. ) ;
#64084 = DIRECTION ( 'NONE',  ( 0.000000000000000000, 0.000000000000000000, -1.000000000000000000 ) ) ;
#64085 = EDGE_CURVE ( 'NONE', #1577, #69035, #60107, .T. ) ;
#64086 = CARTESIAN_POINT ( 'NONE',  ( 4.357963766315029019, 1.733608113333017897, -6.451785339198144342 ) ) ;
#64087 = EDGE_CURVE ( 'NONE', #57077, #47284, #54351, .T. ) ;
#64088 = DIRECTION ( 'NONE',  ( 0.000000000000000000, 0.000000000000000000, -1.000000000000000000 ) ) ;
#64089 = ORIENTED_EDGE ( 'NONE', *, *, #27142, .T. ) ;
#64090 = DIRECTION ( 'NONE',  ( -0.000000000000000000, -0.000000000000000000, -1.000000000000000000 ) ) ;
#64091 = FACE_OUTER_BOUND ( 'NONE', #50366, .T. ) ;
#64092 = CARTESIAN_POINT ( 'NONE',  ( -181.5550000000000068, 0.000000000000000000, 8.024999999999991473 ) ) ;
#64093 = ORIENTED_EDGE ( 'NONE', *, *, #12568, .T. ) ;
#64094 = CARTESIAN_POINT ( 'NONE',  ( 10.39230484541326582, 2.500000000000000000, 0.000000000000000000 ) ) ;
#64095 = DIRECTION ( 'NONE',  ( 0.000000000000000000, -0.000000000000000000, 1.000000000000000000 ) ) ;
#64096 = AXIS2_PLACEMENT_3D ( 'NONE', #55240, #22554, #16950 ) ;
#64097 = VECTOR ( 'NONE', #50044, 1000.000000000000000 ) ;
#64098 = CARTESIAN_POINT ( 'NONE',  ( 15.98999599679679839, 118.4999999999999716, 7.500000000000000000 ) ) ;
#64099 = FILL_AREA_STYLE_COLOUR ( '', #45594 ) ;
#64100 = DIRECTION ( 'NONE',  ( -1.000000000000000000, -0.000000000000000000, -0.000000000000000000 ) ) ;
#64101 = EDGE_LOOP ( 'NONE', ( #40751, #10950, #24522, #24596 ) ) ;
#64102 = EDGE_CURVE ( 'NONE', #42981, #11929, #46544, .T. ) ;
#64103 = CARTESIAN_POINT ( 'NONE',  ( -10.39230484541326938, -1.107695154586735509, -1.661048719643172847E-15 ) ) ;
#64104 = CARTESIAN_POINT ( 'NONE',  ( -95.75499999999999545, 4.716976649647091513, -6.492361379858946790 ) ) ;
#64105 = ORIENTED_EDGE ( 'NONE', *, *, #53677, .T. ) ;
#64106 = CIRCLE ( 'NONE', #61815, 0.5000000000000004441 ) ;
#64107 = DIRECTION ( 'NONE',  ( -0.000000000000000000, -0.000000000000000000, -1.000000000000000000 ) ) ;
#64108 = CARTESIAN_POINT ( 'NONE',  ( -134.9070736234661183, -3.094860106618429807, 9.524999999999991473 ) ) ;
#64109 = MECHANICAL_DESIGN_GEOMETRIC_PRESENTATION_REPRESENTATION (  '', ( #59628 ), #30387 ) ;
#64110 =( LENGTH_UNIT ( ) NAMED_UNIT ( * ) SI_UNIT ( .MILLI., .METRE. ) );
#64111 = CARTESIAN_POINT ( 'NONE',  ( 0.000000000000000000, 0.000000000000000000, 0.000000000000000000 ) ) ;
#64112 = CARTESIAN_POINT ( 'NONE',  ( -68.90707362346616094, -3.094860106618429807, 9.524999999999991473 ) ) ;
#64113 = MECHANICAL_DESIGN_GEOMETRIC_PRESENTATION_REPRESENTATION (  '', ( #7975 ), #55107 ) ;
#64114 = CARTESIAN_POINT ( 'NONE',  ( -80.39292637653379359, 8.102448949553176405, 5.886773742842740909 ) ) ;
#64115 = EDGE_LOOP ( 'NONE', ( #52802, #55514, #38549, #12353 ) ) ;
#64116 = CARTESIAN_POINT ( 'NONE',  ( -195.0000000000000000, 0.000000000000000000, 9.524999999999991473 ) ) ;
#64117 = DIRECTION ( 'NONE',  ( -1.000000000000000000, 0.000000000000000000, 0.000000000000000000 ) ) ;
#64119 = DIRECTION ( 'NONE',  ( 0.000000000000000000, 1.000000000000000000, 0.000000000000000000 ) ) ;
#64118 = DIRECTION ( 'NONE',  ( -0.000000000000000000, -1.000000000000000000, -0.000000000000000000 ) ) ;
#64120 = CARTESIAN_POINT ( 'NONE',  ( -114.6549999999999869, -7.632228543268600340, -2.479861379858950166 ) ) ;
#64121 = EDGE_CURVE ( 'NONE', #67711, #15394, #67602, .T. ) ;
#64122 = CARTESIAN_POINT ( 'NONE',  ( 0.000000000000000000, 121.4449999999999790, -9.525000000000000355 ) ) ;
#64123 = CARTESIAN_POINT ( 'NONE',  ( -120.8949999999999960, 6.826472737025116366, 4.959722759717898555 ) ) ;
#64124 = AXIS2_PLACEMENT_3D ( 'NONE', #66447, #23879, #33732 ) ;
#64125 = ADVANCED_FACE ( 'NONE', ( #17780 ), #13008, .F. ) ;
#64126 = B_SPLINE_CURVE_WITH_KNOTS ( 'NONE', 3,
 ( #49163, #28344, #38285, #861, #17506, #49850, #1588, #38979, #5864, #23113, #55088, #37942 ),
 .UNSPECIFIED., .F., .F.,
 ( 4, 2, 2, 2, 2, 4 ),
 ( 0.007986462481733982294, 0.009333070490708115369, 0.01067967849968225018, 0.01202628650865638499, 0.01269959051314345153, 0.01337289451763051980 ),
 .UNSPECIFIED. ) ;
#64127 = VECTOR ( 'NONE', #62824, 1000.000000000000000 ) ;
#64128 = CARTESIAN_POINT ( 'NONE',  ( -55.79276673654523933, -8.274029027338688280, -1.902897798319236777 ) ) ;
#64130 = CARTESIAN_POINT ( 'NONE',  ( -87.50000000000000000, -6.499999999999990230, 3.000000000000000000 ) ) ;
#64129 = DIRECTION ( 'NONE',  ( -0.000000000000000000, -1.000000000000000000, -0.000000000000000000 ) ) ;
#64131 = VERTEX_POINT ( 'NONE', #60653 ) ;
#64132 = CARTESIAN_POINT ( 'NONE',  ( -161.8429263765337964, 9.058813317711329915, -2.943386871421373119 ) ) ;
#64133 = CARTESIAN_POINT ( 'NONE',  ( -173.6949999999999648, -8.437984349512085203, 5.166775262442717831E-16 ) ) ;
#64134 = CARTESIAN_POINT ( 'NONE',  ( -6.826472737025120807, 149.1070736234661354, 4.959722759717906548 ) ) ;
#64135 = CARTESIAN_POINT ( 'NONE',  ( -25.00000000000000000, 1.000000000000000000, -3.000000000000000000 ) ) ;
#64136 = FACE_OUTER_BOUND ( 'NONE', #17581, .T. ) ;
#64137 = ORIENTED_EDGE ( 'NONE', *, *, #49981, .T. ) ;
#64138 = CARTESIAN_POINT ( 'NONE',  ( -75.74292637653380211, -5.598654528085803328, -7.705886871421366635 ) ) ;
#64139 = CARTESIAN_POINT ( 'NONE',  ( -45.91547277936962956, 9.430195807687216103, 6.000000000000000888 ) ) ;
#64140 = CARTESIAN_POINT ( 'NONE',  ( 4.716976649647099507, 152.6429263765338078, -6.492361379858953008 ) ) ;
#64141 =( BOUNDED_SURFACE ( )  B_SPLINE_SURFACE ( 3, 2, ( 
 ( #49799, #44895, #7230 ),
 ( #28659, #66303, #66666 ),
 ( #23742, #60331, #50156 ),
 ( #2931, #61367, #12135 ),
 ( #7909, #61022, #29720 ),
 ( #12840, #13526, #34305 ),
 ( #55761, #24421, #29353 ),
 ( #23068, #7567, #33603 ) ),
 .UNSPECIFIED., .F., .F., .F. ) 
 B_SPLINE_SURFACE_WITH_KNOTS ( ( 4, 2, 2, 4 ),
 ( 3, 3 ),
 ( 0.0006464147718099833234, 0.001546301970866990460, 0.001996245570395494082, 0.002446189169923997705 ),
 ( 0.000000000000000000, 1.000000000000000000 ),
 .UNSPECIFIED. ) 
 GEOMETRIC_REPRESENTATION_ITEM ( )  RATIONAL_B_SPLINE_SURFACE ( (
 ( 1.000000000000000000, 0.7071067811865475727, 1.000000000000000000),
 ( 1.000000000000000000, 0.7604340084995849791, 1.000000000000000000),
 ( 1.000000000000000000, 0.8048286378025968357, 1.000000000000000000),
 ( 1.000000000000000000, 0.8534265415373917252, 1.000000000000000000),
 ( 1.000000000000000000, 0.8663147087826937875, 1.000000000000000000),
 ( 1.000000000000000000, 0.8838688826995332315, 1.000000000000000000),
 ( 1.000000000000000000, 0.8885266032449491425, 1.000000000000000000),
 ( 1.000000000000000000, 0.8885233166386380388, 1.000000000000000000) ) ) 
 REPRESENTATION_ITEM ( '' )  SURFACE ( )  );
#64142 = DIRECTION ( 'NONE',  ( -1.000000000000000000, 0.000000000000000000, 0.000000000000000000 ) ) ;
#64143 = AXIS2_PLACEMENT_3D ( 'NONE', #22790, #18195, #54088 ) ;
#64144 = CARTESIAN_POINT ( 'NONE',  ( -183.3549999999999898, -4.716976649647093289, -6.492361379858945902 ) ) ;
#64145 = B_SPLINE_CURVE_WITH_KNOTS ( 'NONE', 3,
 ( #46221, #26099, #35640, #63047, #13827, #14889, #25754, #47633, #67641, #57075 ),
 .UNSPECIFIED., .F., .F.,
 ( 4, 2, 2, 2, 4 ),
 ( 0.000000000000000000, 0.0002942714429691386125, 0.0005885428859382772250, 0.0008828143289074158375, 0.001177085771876554450 ),
 .UNSPECIFIED. ) ;
#64146 = ORIENTED_EDGE ( 'NONE', *, *, #40528, .T. ) ;
#64147 = DIRECTION ( 'NONE',  ( 0.000000000000000000, -1.000000000000000000, 0.000000000000000000 ) ) ;
#64148 = EDGE_CURVE ( 'NONE', #23924, #62845, #593, .T. ) ;
#64149 = MECHANICAL_DESIGN_GEOMETRIC_PRESENTATION_REPRESENTATION (  '', ( #13582 ), #3446 ) ;
#64150 = FILL_AREA_STYLE_COLOUR ( '', #58926 ) ;
#64151 = VECTOR ( 'NONE', #16773, 1000.000000000000000 ) ;
#64152 = CARTESIAN_POINT ( 'NONE',  ( -13.74999999999998757, -7.950815931560351124E-15, 4.000000000000000000 ) ) ;
#64153 = CARTESIAN_POINT ( 'NONE',  ( 6.826472737025121695, 138.6070736234661638, -4.959722759717905660 ) ) ;
#64154 = ORIENTED_EDGE ( 'NONE', *, *, #61589, .F. ) ;
#64155 = EDGE_CURVE ( 'NONE', #14824, #21109, #62322, .T. ) ;
#64156 = CARTESIAN_POINT ( 'NONE',  ( -32.58426884830655013, -9.007081295888278660, -1.826937090823335108 ) ) ;
#64157 = CARTESIAN_POINT ( 'NONE',  ( -92.90499999999997272, 2.607480562269069324, -8.024999999999993250 ) ) ;
#64158 = AXIS2_PLACEMENT_3D ( 'NONE', #14859, #37389, #57766 ) ;
#64159 =( NAMED_UNIT ( * ) PLANE_ANGLE_UNIT ( ) SI_UNIT ( $, .RADIAN. ) );
#64160 = VERTEX_POINT ( 'NONE', #1528 ) ;
#64161 =( LENGTH_UNIT ( ) NAMED_UNIT ( * ) SI_UNIT ( .MILLI., .METRE. ) );
#64162 = EDGE_CURVE ( 'NONE', #4344, #43339, #67970, .T. ) ;
#64163 =( NAMED_UNIT ( * ) PLANE_ANGLE_UNIT ( ) SI_UNIT ( $, .RADIAN. ) );
#64164 = DIRECTION ( 'NONE',  ( -8.673617379884015751E-17, 0.000000000000000000, -1.000000000000000000 ) ) ;
#64165 = SURFACE_STYLE_FILL_AREA ( #51989 ) ;
#64166 = VERTEX_POINT ( 'NONE', #23055 ) ;
#64167 = FILL_AREA_STYLE ('',( #30768 ) ) ;
#64168 = CARTESIAN_POINT ( 'NONE',  ( -70.19499999999995055, 8.437984349512085203, -1.550032578732815448E-15 ) ) ;
#64169 = ORIENTED_EDGE ( 'NONE', *, *, #39903, .T. ) ;
#64170 =( BOUNDED_CURVE ( )  B_SPLINE_CURVE ( 3, ( #62767, #58549, #52265, #3657 ),
 .UNSPECIFIED., .F., .F. ) 
 B_SPLINE_CURVE_WITH_KNOTS ( ( 4, 4 ),
 ( -7.105427357601001859E-15, 1.570796326794896558 ),
 .UNSPECIFIED. ) 
 CURVE ( )  GEOMETRIC_REPRESENTATION_ITEM ( )  RATIONAL_B_SPLINE_CURVE ( ( 1.000000000000000000, 0.8047378541243632721, 0.8047378541243632721, 1.000000000000000000 ) ) 
 REPRESENTATION_ITEM ( '' )  );
#64171 = TOROIDAL_SURFACE ( 'NONE', #23752, 18.50000000000000355, 0.5000000000000000000 ) ;
#64172 = CARTESIAN_POINT ( 'NONE',  ( 7.000000000000017764, 17.78868675966041835, -9.106839746483067901E-16 ) ) ;
#64173 = CARTESIAN_POINT ( 'NONE',  ( 2.000000000000015543, 26.00000000000000355, 23.99999999999999645 ) ) ;
#64174 = ORIENTED_EDGE ( 'NONE', *, *, #54223, .F. ) ;
#64175 = CARTESIAN_POINT ( 'NONE',  ( 13.25000000000000355, 28.24999999999998934, -3.750000000000000000 ) ) ;
#64176 = CARTESIAN_POINT ( 'NONE',  ( -13.50000000000000533, 30.74999999999999289, 4.000000000000000000 ) ) ;
#64177 =( GEOMETRIC_REPRESENTATION_CONTEXT ( 3 ) GLOBAL_UNCERTAINTY_ASSIGNED_CONTEXT ( ( #20624 ) ) GLOBAL_UNIT_ASSIGNED_CONTEXT ( ( #24748, #63448, #31413 ) ) REPRESENTATION_CONTEXT ( 'NONE', 'WORKASPACE' ) );
#64178 = EDGE_CURVE ( 'NONE', #46991, #3091, #46181, .T. ) ;
#64179 = PLANE ( 'NONE',  #11164 ) ;
#64180 = LINE ( 'NONE', #26542, #49195 ) ;
#64181 = VERTEX_POINT ( 'NONE', #1872 ) ;
#64182 = PRESENTATION_STYLE_ASSIGNMENT (( #62784 ) ) ;
#64183 = ORIENTED_EDGE ( 'NONE', *, *, #46144, .F. ) ;
#64184 = CARTESIAN_POINT ( 'NONE',  ( -62.28939201416945082, 0.000000000000000000, -5.000000000000000000 ) ) ;
#64185 =( NAMED_UNIT ( * ) PLANE_ANGLE_UNIT ( ) SI_UNIT ( $, .RADIAN. ) );
#64186 = CARTESIAN_POINT ( 'NONE',  ( -156.9570736234661581, 9.058813317711329915, -2.943386871421373119 ) ) ;
#64187 = CIRCLE ( 'NONE', #33847, 0.2500000000000002220 ) ;
#64188 = CARTESIAN_POINT ( 'NONE',  ( -10.01517768586949408, 125.1950000000000074, -6.132527647946036459E-16 ) ) ;
#64189 = CARTESIAN_POINT ( 'NONE',  ( -89.75707362346616947, -5.598654528085801552, 7.705886871421367523 ) ) ;
#64190 = STYLED_ITEM ( 'NONE', ( #48379 ), #45798 ) ;
#64191 = DIRECTION ( 'NONE',  ( 0.000000000000000000, -0.000000000000000000, 1.000000000000000000 ) ) ;
#64192 = ORIENTED_EDGE ( 'NONE', *, *, #16638, .T. ) ;
#64195 = VECTOR ( 'NONE', #40257, 1000.000000000000000 ) ;
#64194 = FILL_AREA_STYLE ('',( #64559 ) ) ;
#64193 = CARTESIAN_POINT ( 'NONE',  ( -195.0000000000000000, 0.000000000000000000, 0.000000000000000000 ) ) ;
#64196 = DIRECTION ( 'NONE',  ( 0.000000000000000000, -1.000000000000000000, 0.000000000000000000 ) ) ;
#64197 = CARTESIAN_POINT ( 'NONE',  ( -142.1049999999999613, -6.826472737025115478, 4.959722759717900331 ) ) ;
#64198 =( LENGTH_UNIT ( ) NAMED_UNIT ( * ) SI_UNIT ( .MILLI., .METRE. ) );
#64199 = CYLINDRICAL_SURFACE ( 'NONE', #58354, 0.2500000000000002220 ) ;
#64200 = DIRECTION ( 'NONE',  ( 0.000000000000000000, 0.000000000000000000, 1.000000000000000000 ) ) ;
#64201 = STYLED_ITEM ( 'NONE', ( #22809 ), #22077 ) ;
#64202 = CARTESIAN_POINT ( 'NONE',  ( -148.6450000000000102, 4.716976649647091513, -6.492361379858946790 ) ) ;
#64203 = CARTESIAN_POINT ( 'NONE',  ( -137.0949999999999989, -2.607480562269071545, -8.024999999999991473 ) ) ;
#64204 = STYLED_ITEM ( 'NONE', ( #44328 ), #35438 ) ;
#64205 = EDGE_LOOP ( 'NONE', ( #66125, #53140 ) ) ;
#64206 = CARTESIAN_POINT ( 'NONE',  ( 45.61109309484434249, 10.20369769828143092, -3.650011426053815011 ) ) ;
#64207 = DIRECTION ( 'NONE',  ( -0.000000000000000000, -0.000000000000000000, -1.000000000000000000 ) ) ;
#64208 = UNCERTAINTY_MEASURE_WITH_UNIT (LENGTH_MEASURE( 1.000000000000000082E-05 ), #68007, 'distance_accuracy_value', 'NONE');
#64209 = CARTESIAN_POINT ( 'NONE',  ( -55.10499999999998266, -6.826472737025115478, 4.959722759717900331 ) ) ;
#64210 = STYLED_ITEM ( 'NONE', ( #56926 ), #28413 ) ;
#64211 = CYLINDRICAL_SURFACE ( 'NONE', #41066, 8.025000000000000355 ) ;
#64212 = SURFACE_STYLE_USAGE ( .BOTH. , #4780 ) ;
#64213 = FACE_OUTER_BOUND ( 'NONE', #3295, .T. ) ;
#64214 = VECTOR ( 'NONE', #46946, 1000.000000000000000 ) ;
#64215 = CARTESIAN_POINT ( 'NONE',  ( 74.50000000000000000, -2.220952357103124925E-14, -6.999999999999999112 ) ) ;
#64216 = PRODUCT_DEFINITION_CONTEXT ( 'detailed design', #39716, 'design' ) ;
#64217 = CARTESIAN_POINT ( 'NONE',  ( 35.50000000000010658, 49.99999999999985079, -59.99999999999958789 ) ) ;
#64218 = CARTESIAN_POINT ( 'NONE',  ( -152.8429263765337964, 9.058813317711329915, -2.943386871421373119 ) ) ;
#64219 = AXIS2_PLACEMENT_3D ( 'NONE', #31655, #16557, #42961 ) ;
#64220 = CARTESIAN_POINT ( 'NONE',  ( -75.05707362346616662, 0.000000000000000000, 9.524999999999991473 ) ) ;
#64221 = CARTESIAN_POINT ( 'NONE',  ( -100.4070736234672125, 3.094860106601488248, -9.525000000012305179 ) ) ;
#64222 = MECHANICAL_DESIGN_GEOMETRIC_PRESENTATION_REPRESENTATION (  '', ( #19270 ), #14849 ) ;
#64223 = DIRECTION ( 'NONE',  ( -1.239088197126290324E-16, 0.000000000000000000, -1.000000000000000000 ) ) ;
#64224 = EDGE_CURVE ( 'NONE', #62949, #65192, #52795, .T. ) ;
#64225 = CARTESIAN_POINT ( 'NONE',  ( 6.999798566743336004, 53.02677333163759243, -6.907879333238362562 ) ) ;
#64226 = ORIENTED_EDGE ( 'NONE', *, *, #41149, .T. ) ;
#64227 = SURFACE_STYLE_USAGE ( .BOTH. , #63548 ) ;
#64228 = CARTESIAN_POINT ( 'NONE',  ( -4.716976649647097730, 112.3570736234661496, -6.492361379858953896 ) ) ;
#64229 = CIRCLE ( 'NONE', #24918, 0.5000000000000004441 ) ;
#64230 = AXIS2_PLACEMENT_3D ( 'NONE', #33252, #60318, #54686 ) ;
#64231 = CARTESIAN_POINT ( 'NONE',  ( -19.89974874213240241, 114.9999999999999574, 10.49999999999999822 ) ) ;
#64232 = CYLINDRICAL_SURFACE ( 'NONE', #66522, 0.5000000000000004441 ) ;
#64233 = AXIS2_PLACEMENT_3D ( 'NONE', #21692, #6204, #7254 ) ;
#64234 = ADVANCED_FACE ( 'NONE', ( #27935 ), #55695, .T. ) ;
#64235 = VERTEX_POINT ( 'NONE', #39607 ) ;
#64236 = ORIENTED_EDGE ( 'NONE', *, *, #55682, .F. ) ;
#64237 = CARTESIAN_POINT ( 'NONE',  ( -15.75000000000000000, -0.9999999999999995559, 24.00000000000000000 ) ) ;
#64238 = CARTESIAN_POINT ( 'NONE',  ( -195.0000000000000000, 0.000000000000000000, 0.000000000000000000 ) ) ;
#64239 = EDGE_CURVE ( 'NONE', #20590, #51912, #19063, .T. ) ;
#64240 = CARTESIAN_POINT ( 'NONE',  ( 6.000000000000017764, -60.04052944165106709, -35.50000000000000000 ) ) ;
#64241 = ORIENTED_EDGE ( 'NONE', *, *, #5007, .T. ) ;
#64242 = CARTESIAN_POINT ( 'NONE',  ( 9.058813317711338797, 118.9549999999999983, -2.943386871421372675 ) ) ;
#64243 = FACE_OUTER_BOUND ( 'NONE', #30839, .T. ) ;
#64244 = CYLINDRICAL_SURFACE ( 'NONE', #50211, 0.5000000000000004441 ) ;
#64245 = STYLED_ITEM ( 'NONE', ( #41983 ), #22481 ) ;
#64246 = EDGE_CURVE ( 'NONE', #35469, #835, #41956, .T. ) ;
#64247 = EDGE_CURVE ( 'NONE', #37997, #67791, #49013, .T. ) ;
#64248 = CARTESIAN_POINT ( 'NONE',  ( -105.4449999999999790, 0.000000000000000000, 8.024999999999991473 ) ) ;
#64249 = ORIENTED_EDGE ( 'NONE', *, *, #10517, .F. ) ;
#64250 = PRESENTATION_LAYER_ASSIGNMENT (  '', '', ( #16047 ) ) ;
#64251 = CARTESIAN_POINT ( 'NONE',  ( 71.62068965517238439, 63.58603185604027885, 9.500000000000000000 ) ) ;
#64252 = EDGE_CURVE ( 'NONE', #49213, #52470, #20811, .T. ) ;
#64253 = DIRECTION ( 'NONE',  ( 0.000000000000000000, 0.000000000000000000, -1.000000000000000000 ) ) ;
#64254 = ORIENTED_EDGE ( 'NONE', *, *, #14455, .F. ) ;
#64255 = CARTESIAN_POINT ( 'NONE',  ( -2.607480562269075097, 151.2929263765338135, 8.025000000000000355 ) ) ;
#64256 = PRESENTATION_LAYER_ASSIGNMENT (  '', '', ( #13702 ) ) ;
#64257 = AXIS2_PLACEMENT_3D ( 'NONE', #62386, #31746, #63759 ) ;
#64258 = DIRECTION ( 'NONE',  ( 1.000000000000000000, 0.000000000000000000, 4.516179008354028246E-16 ) ) ;
#64259 = AXIS2_PLACEMENT_3D ( 'NONE', #33399, #21814, #65042 ) ;
#64260 = CARTESIAN_POINT ( 'NONE',  ( 20.42980746818723503, 114.8194254430358399, -10.32394991351191571 ) ) ;
#64261 = ORIENTED_EDGE ( 'NONE', *, *, #48879, .F. ) ;
#64262 = PRESENTATION_STYLE_ASSIGNMENT (( #17154 ) ) ;
#64263 = DIRECTION ( 'NONE',  ( 0.3162277660168358873, -0.9486832980505145452, 0.000000000000000000 ) ) ;
#64264 = FILL_AREA_STYLE ('',( #54733 ) ) ;
#64265 = SURFACE_STYLE_FILL_AREA ( #14713 ) ;
#64266 =( LENGTH_UNIT ( ) NAMED_UNIT ( * ) SI_UNIT ( .MILLI., .METRE. ) );
#64267 = LINE ( 'NONE', #16122, #19532 ) ;
#64268 =( BOUNDED_CURVE ( )  B_SPLINE_CURVE ( 2, ( #11039, #32485, #16705, #49733, #60952, #23331, #1820, #438, #34241, #60597, #54972 ),
 .UNSPECIFIED., .F., .F. ) 
 B_SPLINE_CURVE_WITH_KNOTS ( ( 3, 2, 2, 2, 2, 3 ),
 ( 0.4130434782608596311, 0.4152173913043378239, 0.4173913043478160723, 0.4195652173912943206, 0.4217391304347725689, 0.4239130434782507617 ),
 .UNSPECIFIED. ) 
 CURVE ( )  GEOMETRIC_REPRESENTATION_ITEM ( )  RATIONAL_B_SPLINE_CURVE ( ( 1.000000000000223821, 0.9510565162949298212, 1.000000000000000000, 0.9510565162951535312, 1.000000000000000000, 0.9510565162951535312, 1.000000000000000000, 0.9510565162951535312, 1.000000000000000000, 0.9510565162953810159, 0.9999999999997725153 ) ) 
 REPRESENTATION_ITEM ( '' )  );
#64269 = AXIS2_PLACEMENT_3D ( 'NONE', #30695, #35657, #68026 ) ;
#64270 = DIRECTION ( 'NONE',  ( -1.000000000000000000, -0.000000000000000000, -0.000000000000000000 ) ) ;
#64271 = CARTESIAN_POINT ( 'NONE',  ( -87.50000000000000000, -6.499999999999990230, 21.00000000000000000 ) ) ;
#64272 = CARTESIAN_POINT ( 'NONE',  ( -2.607480562269116842, 121.2929263765337993, 8.024999999999970157 ) ) ;
#64273 = LINE ( 'NONE', #49503, #31305 ) ;
#64274 = VERTEX_POINT ( 'NONE', #58104 ) ;
#64275 = AXIS2_PLACEMENT_3D ( 'NONE', #27892, #60962, #1481 ) ;
#64276 = EDGE_LOOP ( 'NONE', ( #54877, #36778, #21938, #47688 ) ) ;
#64277 = DIRECTION ( 'NONE',  ( 0.000000000000000000, 0.000000000000000000, -1.000000000000000000 ) ) ;
#64278 = DIRECTION ( 'NONE',  ( 0.000000000000000000, 1.000000000000000000, -0.000000000000000000 ) ) ;
#64279 = CARTESIAN_POINT ( 'NONE',  ( -170.7570736234661695, -5.598654528085801552, 7.705886871421367523 ) ) ;
#64280 = CARTESIAN_POINT ( 'NONE',  ( 12.25000000000000355, 30.99999999999998579, -3.750000000000000000 ) ) ;
#64281 = ORIENTED_EDGE ( 'NONE', *, *, #62958, .F. ) ;
#64282 = CARTESIAN_POINT ( 'NONE',  ( 4.000000000000029310, 43.00000000000000000, 90.00000000000000000 ) ) ;
#64283 = CARTESIAN_POINT ( 'NONE',  ( -171.9549999999999841, -7.632228543268599452, 2.479861379858951054 ) ) ;
#64284 = CARTESIAN_POINT ( 'NONE',  ( 62.59999999999998721, 11.99999999999999822, -4.000000000000000000 ) ) ;
#64285 = LINE ( 'NONE', #37261, #57144 ) ;
#64286 = CARTESIAN_POINT ( 'NONE',  ( -48.50707362346617657, 8.102448949553176405, 5.886773742842740909 ) ) ;
#64287 = CARTESIAN_POINT ( 'NONE',  ( -169.9449999999999932, -9.827790563157499189E-16, -8.024999999999991473 ) ) ;
#64288 = ORIENTED_EDGE ( 'NONE', *, *, #20335, .F. ) ;
#64289 = CARTESIAN_POINT ( 'NONE',  ( 7.794228634059952476, 4.500000000000003553, 0.000000000000000000 ) ) ;
#64290 = AXIS2_PLACEMENT_3D ( 'NONE', #613, #28059, #21798 ) ;
#64291 = CARTESIAN_POINT ( 'NONE',  ( -0.9109038252169192607, -2.456844516558473135, 9.000000000000001776 ) ) ;
#64292 = CARTESIAN_POINT ( 'NONE',  ( -11.69351122144522215, 11.39671261894639187, -3.764684334147166300 ) ) ;
#64293 = CARTESIAN_POINT ( 'NONE',  ( -79.10499999999998977, -6.826472737025115478, 4.959722759717900331 ) ) ;
#64294 = CARTESIAN_POINT ( 'NONE',  ( 1.000000000000000000, 36.74999999999999289, 3.000000000000000000 ) ) ;
#64295 = CARTESIAN_POINT ( 'NONE',  ( 24.16127419156986278, 27.24068003726083376, 27.27382999534755115 ) ) ;
#64296 = CARTESIAN_POINT ( 'NONE',  ( -74.89071377870236290, 36.10880737351290293, -9.849303885975091433 ) ) ;
#64297 = CARTESIAN_POINT ( 'NONE',  ( -83.09499999999998465, -2.607480562269071545, -8.024999999999991473 ) ) ;
#64298 = CARTESIAN_POINT ( 'NONE',  ( 8.102448949553183510, 137.1049999999999898, -5.886773742842746238 ) ) ;
#64299 = VECTOR ( 'NONE', #22917, 1000.000000000000000 ) ;
#64300 = FACE_BOUND ( 'NONE', #18885, .T. ) ;
#64301 = CARTESIAN_POINT ( 'NONE',  ( -171.9570736234661865, 9.058813317711329915, -2.943386871421373119 ) ) ;
#64302 = AXIS2_PLACEMENT_3D ( 'NONE', #3573, #19081, #29296 ) ;
#64303 = CYLINDRICAL_SURFACE ( 'NONE', #24820, 0.2500000000000002220 ) ;
#64304 = UNCERTAINTY_MEASURE_WITH_UNIT (LENGTH_MEASURE( 1.000000000000000082E-05 ), #68400, 'distance_accuracy_value', 'NONE');
#64305 = SURFACE_SIDE_STYLE ('',( #21391 ) ) ;
#64306 = VERTEX_POINT ( 'NONE', #26411 ) ;
#64307 = PRESENTATION_LAYER_ASSIGNMENT (  '', '', ( #37412 ) ) ;
#64308 = CARTESIAN_POINT ( 'NONE',  ( -55.00000000000000000, -1.962809905030629631E-14, 6.999999999999995559 ) ) ;
#64309 = VECTOR ( 'NONE', #27749, 1000.000000000000000 ) ;
#64310 = FILL_AREA_STYLE_COLOUR ( '', #31678 ) ;
#64311 = DIRECTION ( 'NONE',  ( -0.000000000000000000, -0.000000000000000000, -1.000000000000000000 ) ) ;
#64312 = EDGE_CURVE ( 'NONE', #33379, #30008, #4607, .T. ) ;
#64313 = CARTESIAN_POINT ( 'NONE',  ( -71.50000000000000000, 14.49137674618942562, 7.500000000000000000 ) ) ;
#64314 =( NAMED_UNIT ( * ) SI_UNIT ( $, .STERADIAN. ) SOLID_ANGLE_UNIT ( ) );
#64315 = ORIENTED_EDGE ( 'NONE', *, *, #37480, .T. ) ;
#64316 = EDGE_LOOP ( 'NONE', ( #12966, #18699, #57168, #6359 ) ) ;
#64317 = DIRECTION ( 'NONE',  ( -0.7071067811865543451, 0.000000000000000000, -0.7071067811865408004 ) ) ;
#64318 = UNCERTAINTY_MEASURE_WITH_UNIT (LENGTH_MEASURE( 1.000000000000000082E-05 ), #35349, 'distance_accuracy_value', 'NONE');
#64319 = EDGE_CURVE ( 'NONE', #26721, #19782, #15218, .T. ) ;
#64320 = MECHANICAL_DESIGN_GEOMETRIC_PRESENTATION_REPRESENTATION (  '', ( #9316 ), #32913 ) ;
#64321 = SURFACE_STYLE_FILL_AREA ( #36941 ) ;
#64322 = FILL_AREA_STYLE_COLOUR ( '', #15782 ) ;
#64323 =( GEOMETRIC_REPRESENTATION_CONTEXT ( 3 ) GLOBAL_UNCERTAINTY_ASSIGNED_CONTEXT ( ( #18059 ) ) GLOBAL_UNIT_ASSIGNED_CONTEXT ( ( #40868, #46504, #14810 ) ) REPRESENTATION_CONTEXT ( 'NONE', 'WORKASPACE' ) );
#64324 = CARTESIAN_POINT ( 'NONE',  ( 1.999798566743339334, 49.09558629977726696, 2.000000000000000000 ) ) ;
#64325 = CARTESIAN_POINT ( 'NONE',  ( -9.827790563157511022E-16, 139.4429263765338192, 8.025000000000000355 ) ) ;
#64326 = ORIENTED_EDGE ( 'NONE', *, *, #14798, .F. ) ;
#64327 = CARTESIAN_POINT ( 'NONE',  ( -119.1550000000000011, 7.632228543268600340, 2.479861379858949277 ) ) ;
#64328 = EDGE_LOOP ( 'NONE', ( #7761, #42563, #65040, #10418 ) ) ;
#64329 = CARTESIAN_POINT ( 'NONE',  ( 179.4361977533518484, 5.000000000000000000, 103.7004518695275550 ) ) ;
#64330 = CARTESIAN_POINT ( 'NONE',  ( 20.56536453975222756, 115.3173173917729173, -10.00000000000000000 ) ) ;
#64331 = ORIENTED_EDGE ( 'NONE', *, *, #42127, .T. ) ;
#64332 = PRESENTATION_STYLE_ASSIGNMENT (( #58363 ) ) ;
#64333 = DIRECTION ( 'NONE',  ( 1.000000000000000000, 0.000000000000000000, 0.000000000000000000 ) ) ;
#64334 = ORIENTED_EDGE ( 'NONE', *, *, #16706, .T. ) ;
#64335 = ADVANCED_FACE ( 'NONE', ( #9914 ), #64046, .T. ) ;
#64336 = AXIS2_PLACEMENT_3D ( 'NONE', #34427, #67130, #35479 ) ;
#64337 =( GEOMETRIC_REPRESENTATION_CONTEXT ( 3 ) GLOBAL_UNCERTAINTY_ASSIGNED_CONTEXT ( ( #1619 ) ) GLOBAL_UNIT_ASSIGNED_CONTEXT ( ( #22366, #140, #37568 ) ) REPRESENTATION_CONTEXT ( 'NONE', 'WORKASPACE' ) );
#64338 =( NAMED_UNIT ( * ) SI_UNIT ( $, .STERADIAN. ) SOLID_ANGLE_UNIT ( ) );
#64339 = CARTESIAN_POINT ( 'NONE',  ( 5.598654528085805993, 147.2449999999999761, 7.705886871421374629 ) ) ;
#64340 = DIRECTION ( 'NONE',  ( 0.000000000000000000, -1.000000000000000000, 0.000000000000000000 ) ) ;
#64341 = ORIENTED_EDGE ( 'NONE', *, *, #12721, .T. ) ;
#64342 = AXIS2_PLACEMENT_3D ( 'NONE', #15755, #53033, #20673 ) ;
#64343 = SURFACE_SIDE_STYLE ('',( #32322 ) ) ;
#64344 = SURFACE_STYLE_FILL_AREA ( #54473 ) ;
#64345 = SURFACE_STYLE_FILL_AREA ( #68597 ) ;
#64346 = EDGE_CURVE ( 'NONE', #29086, #51850, #58782, .T. ) ;
#64347 = CARTESIAN_POINT ( 'NONE',  ( -130.6429263765338078, -5.598654528085801552, 7.705886871421367523 ) ) ;
#64348 = VERTEX_POINT ( 'NONE', #69004 ) ;
#64349 = CARTESIAN_POINT ( 'NONE',  ( 2.607480562269071989, 130.5929263765337964, 8.025000000000002132 ) ) ;
#64350 = SPHERICAL_SURFACE ( 'NONE', #69381, 0.2500000000000000000 ) ;
#64351 = MECHANICAL_DESIGN_GEOMETRIC_PRESENTATION_REPRESENTATION (  '', ( #41903 ), #29497 ) ;
#64352 = CARTESIAN_POINT ( 'NONE',  ( 6.826472737025121695, 125.4929263765338021, -4.959722759717905660 ) ) ;
#64354 = AXIS2_PLACEMENT_3D ( 'NONE', #14514, #35990, #68344 ) ;
#64353 = FACE_OUTER_BOUND ( 'NONE', #38024, .T. ) ;
#64355 = ORIENTED_EDGE ( 'NONE', *, *, #29563, .T. ) ;
#64356 = CARTESIAN_POINT ( 'NONE',  ( 179.4361977533490631, 5.000000000000000000, -103.7004518695262192 ) ) ;
#64357 = ORIENTED_EDGE ( 'NONE', *, *, #58232, .T. ) ;
#64358 = CARTESIAN_POINT ( 'NONE',  ( 4.000000000000030198, 43.00000000000000000, 89.00000000000000000 ) ) ;
#64359 = FILL_AREA_STYLE_COLOUR ( '', #44700 ) ;
#64360 = CARTESIAN_POINT ( 'NONE',  ( -13.75000000000000533, 30.74999999999999289, 3.750000000000000000 ) ) ;
#64361 = CARTESIAN_POINT ( 'NONE',  ( -141.9549999999999841, -7.632228543268599452, 2.479861379858951054 ) ) ;
#64362 = CIRCLE ( 'NONE', #44221, 0.5000000000000004441 ) ;
#64363 = CARTESIAN_POINT ( 'NONE',  ( -19.89974874213240597, 115.4999999999999574, -10.50000000000000000 ) ) ;
#64364 = FILL_AREA_STYLE_COLOUR ( '', #45188 ) ;
#64365 = UNCERTAINTY_MEASURE_WITH_UNIT (LENGTH_MEASURE( 1.000000000000000082E-05 ), #6172, 'distance_accuracy_value', 'NONE');
#64366 = DIRECTION ( 'NONE',  ( -1.000000000000000000, -0.000000000000000000, -0.000000000000000000 ) ) ;
#64367 = DIRECTION ( 'NONE',  ( 1.000000000000000000, 0.000000000000000000, 0.000000000000000000 ) ) ;
#64368 = CARTESIAN_POINT ( 'NONE',  ( 41.00000002860134884, 108.0041655605199367, 3.103651540213804516 ) ) ;
#64369 = CARTESIAN_POINT ( 'NONE',  ( 23.71231517720798010, 118.4999999999999716, -7.500000000000000000 ) ) ;
#64370 = ORIENTED_EDGE ( 'NONE', *, *, #25502, .T. ) ;
#64371 = ORIENTED_EDGE ( 'NONE', *, *, #47319, .F. ) ;
#64372 = CARTESIAN_POINT ( 'NONE',  ( -35.65778776279520912, -9.947368421052624754, 4.481646853389230856 ) ) ;
#64373 = PRESENTATION_LAYER_ASSIGNMENT (  '', '', ( #46440 ) ) ;
#64374 = CARTESIAN_POINT ( 'NONE',  ( -4.683753779217433078, 2.005109422339666825, 5.887500484252660371 ) ) ;
#64375 = STYLED_ITEM ( 'NONE', ( #63685 ), #29078 ) ;
#64376 = CARTESIAN_POINT ( 'NONE',  ( -60.20499999999998408, -2.607480562269071545, -8.024999999999991473 ) ) ;
#64377 = ORIENTED_EDGE ( 'NONE', *, *, #62711, .T. ) ;
#64378 = SPHERICAL_SURFACE ( 'NONE', #45020, 1.000000000000000000 ) ;
#64379 = DIRECTION ( 'NONE',  ( 0.000000000000000000, 0.000000000000000000, -1.000000000000000000 ) ) ;
#64380 = AXIS2_PLACEMENT_3D ( 'NONE', #51931, #24816, #15363 ) ;
#64381 = CARTESIAN_POINT ( 'NONE',  ( 41.49999999999998579, 108.0000000000000000, -3.500000000000000000 ) ) ;
#64382 = CARTESIAN_POINT ( 'NONE',  ( -24.00000000000000355, 37.00000000000000000, -3.000000000000000000 ) ) ;
#64383 = FACE_OUTER_BOUND ( 'NONE', #22107, .T. ) ;
#64384 = ORIENTED_EDGE ( 'NONE', *, *, #30550, .T. ) ;
#64385 = EDGE_CURVE ( 'NONE', #8740, #40876, #58432, .T. ) ;
#64386 = AXIS2_PLACEMENT_3D ( 'NONE', #57373, #3151, #14124 ) ;
#64387 = DIRECTION ( 'NONE',  ( -0.000000000000000000, -0.000000000000000000, 1.000000000000000000 ) ) ;
#64388 = FACE_OUTER_BOUND ( 'NONE', #23505, .T. ) ;
#64389 = SURFACE_SIDE_STYLE ('',( #16582 ) ) ;
#64390 = CARTESIAN_POINT ( 'NONE',  ( -107.2449999999999903, -4.716976649647093289, -6.492361379858945902 ) ) ;
#64391 = CARTESIAN_POINT ( 'NONE',  ( -5.598654528085808657, 155.6449999999999818, 7.705886871421373741 ) ) ;
#64392 = CARTESIAN_POINT ( 'NONE',  ( -90.29499999999997328, -2.607480562269069768, 8.024999999999991473 ) ) ;
#64393 = CARTESIAN_POINT ( 'NONE',  ( 22.00000000000001066, 43.00000000000000000, -45.61250543006184444 ) ) ;
#64394 = VECTOR ( 'NONE', #64317, 1000.000000000000114 ) ;
#64395 = VECTOR ( 'NONE', #32149, 1000.000000000000000 ) ;
#64396 = DIRECTION ( 'NONE',  ( 1.000000000000000000, 0.000000000000000000, 0.000000000000000000 ) ) ;
#64397 = DIRECTION ( 'NONE',  ( 1.000000000000000000, 0.000000000000000000, 0.000000000000000000 ) ) ;
#64398 = UNCERTAINTY_MEASURE_WITH_UNIT (LENGTH_MEASURE( 1.000000000000000082E-05 ), #15169, 'distance_accuracy_value', 'NONE');
#64399 = CARTESIAN_POINT ( 'NONE',  ( 23.21231517720797655, 117.4999999999999716, -9.500000000000000000 ) ) ;
#64400 = PRESENTATION_LAYER_ASSIGNMENT (  '', '', ( #311 ) ) ;
#64401 = ORIENTED_EDGE ( 'NONE', *, *, #31477, .F. ) ;
#64402 = CARTESIAN_POINT ( 'NONE',  ( -135.7429263765338021, -5.598654528085803328, -7.705886871421366635 ) ) ;
#64403 = CARTESIAN_POINT ( 'NONE',  ( -148.6450000000000102, 4.716976649647091513, -6.492361379858946790 ) ) ;
#64404 = LINE ( 'NONE', #21487, #54954 ) ;
#64405 = ADVANCED_FACE ( 'NONE', ( #52495 ), #37375, .T. ) ;
#64406 =( GEOMETRIC_REPRESENTATION_CONTEXT ( 3 ) GLOBAL_UNCERTAINTY_ASSIGNED_CONTEXT ( ( #44758 ) ) GLOBAL_UNIT_ASSIGNED_CONTEXT ( ( #30737, #14233, #9673 ) ) REPRESENTATION_CONTEXT ( 'NONE', 'WORKASPACE' ) );
#64407 = EDGE_CURVE ( 'NONE', #28358, #39909, #25709, .T. ) ;
#64408 = FACE_OUTER_BOUND ( 'NONE', #35646, .T. ) ;
#64409 = DIRECTION ( 'NONE',  ( 0.000000000000000000, 0.000000000000000000, -1.000000000000000000 ) ) ;
#64410 = VERTEX_POINT ( 'NONE', #46055 ) ;
#64411 = ORIENTED_EDGE ( 'NONE', *, *, #40160, .F. ) ;
#64412 = AXIS2_PLACEMENT_3D ( 'NONE', #11235, #937, #6999 ) ;
#64413 = FACE_OUTER_BOUND ( 'NONE', #19774, .T. ) ;
#64414 = EDGE_CURVE ( 'NONE', #2776, #49636, #30166, .T. ) ;
#64415 = VECTOR ( 'NONE', #15553, 1000.000000000000000 ) ;
#64416 = DIRECTION ( 'NONE',  ( -1.000000000000000000, 0.000000000000000000, 0.000000000000000000 ) ) ;
#64417 = CARTESIAN_POINT ( 'NONE',  ( -59.69292637653380496, 10.01517768586948698, -1.839758294383808966E-15 ) ) ;
#64418 =( NAMED_UNIT ( * ) PLANE_ANGLE_UNIT ( ) SI_UNIT ( $, .RADIAN. ) );
#64419 = AXIS2_PLACEMENT_3D ( 'NONE', #52521, #47264, #9255 ) ;
#64420 = DIRECTION ( 'NONE',  ( -1.000000000000000000, -0.000000000000000000, -0.000000000000000000 ) ) ;
#64421 = ORIENTED_EDGE ( 'NONE', *, *, #45481, .F. ) ;
#64422 = CARTESIAN_POINT ( 'NONE',  ( -147.0549999999999784, -9.827790563157499189E-16, -8.024999999999991473 ) ) ;
#64423 = AXIS2_PLACEMENT_3D ( 'NONE', #17293, #11279, #22535 ) ;
#64424 = ORIENTED_EDGE ( 'NONE', *, *, #51797, .F. ) ;
#64425 = SURFACE_STYLE_FILL_AREA ( #53193 ) ;
#64426 = ORIENTED_EDGE ( 'NONE', *, *, #22968, .T. ) ;
#64427 = ADVANCED_FACE ( 'NONE', ( #45375 ), #54588, .F. ) ;
#64428 = LINE ( 'NONE', #10954, #16976 ) ;
#64429 = DIRECTION ( 'NONE',  ( 6.938893903907222067E-15, 0.000000000000000000, -1.000000000000000000 ) ) ;
#64430 = CARTESIAN_POINT ( 'NONE',  ( -5.598654528085806881, 124.7449999999999903, -7.705886871421374629 ) ) ;
#64431 = CARTESIAN_POINT ( 'NONE',  ( -2.012550282676216817E-15, 42.24279663153547659, -74.85430519625602130 ) ) ;
#64432 = CONICAL_SURFACE ( 'NONE', #28444, 5.500000000000005329, 0.7853981633974482790 ) ;
#64433 = ORIENTED_EDGE ( 'NONE', *, *, #44225, .F. ) ;
#64434 = AXIS2_PLACEMENT_3D ( 'NONE', #12141, #55408, #50160 ) ;
#64435 = PRESENTATION_STYLE_ASSIGNMENT (( #43709 ) ) ;
#64436 = CARTESIAN_POINT ( 'NONE',  ( -10.01517768586949408, 132.3049999999999784, -6.132527647946036459E-16 ) ) ;
#64437 = CARTESIAN_POINT ( 'NONE',  ( -65.00499999999998124, 6.826472737025115478, 4.959722759717899443 ) ) ;
#64438 = CARTESIAN_POINT ( 'NONE',  ( -121.0449999999999875, 7.632228543268600340, 2.479861379858949277 ) ) ;
#64439 = ADVANCED_FACE ( 'NONE', ( #19265 ), #57261, .F. ) ;
#64440 = DIRECTION ( 'NONE',  ( 0.000000000000000000, 0.000000000000000000, -1.000000000000000000 ) ) ;
#64441 = ORIENTED_EDGE ( 'NONE', *, *, #29946, .F. ) ;
#64442 = CARTESIAN_POINT ( 'NONE',  ( -5.598654528085806881, 149.8549999999999898, -7.705886871421374629 ) ) ;
#64443 = UNCERTAINTY_MEASURE_WITH_UNIT (LENGTH_MEASURE( 1.000000000000000082E-05 ), #46756, 'distance_accuracy_value', 'NONE');
#64444 = AXIS2_PLACEMENT_3D ( 'NONE', #7722, #18296, #44720 ) ;
#64445 = CARTESIAN_POINT ( 'NONE',  ( 59.00000000000000000, 11.99999999999999822, -4.000000000000000000 ) ) ;
#64446 = DIRECTION ( 'NONE',  ( 1.000000000000000000, 0.000000000000000000, -0.000000000000000000 ) ) ;
#64447 = LINE ( 'NONE', #42688, #31766 ) ;
#64448 = ORIENTED_EDGE ( 'NONE', *, *, #9563, .T. ) ;
#64449 = CIRCLE ( 'NONE', #7150, 0.5000000000000004441 ) ;
#64450 = AXIS2_PLACEMENT_3D ( 'NONE', #62585, #67894, #62929 ) ;
#64451 = FACE_OUTER_BOUND ( 'NONE', #20655, .T. ) ;
#64452 = SURFACE_SIDE_STYLE ('',( #32092 ) ) ;
#64453 = CARTESIAN_POINT ( 'NONE',  ( -168.6550000000000011, -7.632228543268600340, -2.479861379858950166 ) ) ;
#64454 = VERTEX_POINT ( 'NONE', #3403 ) ;
#64455 = UNCERTAINTY_MEASURE_WITH_UNIT (LENGTH_MEASURE( 1.000000000000000082E-05 ), #35889, 'distance_accuracy_value', 'NONE');
#64456 = AXIS2_PLACEMENT_3D ( 'NONE', #62692, #35650, #19089 ) ;
#64457 = PRESENTATION_STYLE_ASSIGNMENT (( #17341 ) ) ;
#64458 =( NAMED_UNIT ( * ) PLANE_ANGLE_UNIT ( ) SI_UNIT ( $, .RADIAN. ) );
#64459 = ORIENTED_EDGE ( 'NONE', *, *, #27225, .F. ) ;
#64460 = CARTESIAN_POINT ( 'NONE',  ( 57.00000000000000000, 0.000000000000000000, 77.00402776293825013 ) ) ;
#64461 = SURFACE_STYLE_USAGE ( .BOTH. , #43057 ) ;
#64462 = CARTESIAN_POINT ( 'NONE',  ( -86.00499999999999545, 6.826472737025116366, 4.959722759717898555 ) ) ;
#64464 = ORIENTED_EDGE ( 'NONE', *, *, #51714, .F. ) ;
#64463 = AXIS2_PLACEMENT_3D ( 'NONE', #63374, #53516, #26747 ) ;
#64465 = DIRECTION ( 'NONE',  ( 0.000000000000000000, 0.000000000000000000, 1.000000000000000000 ) ) ;
#64466 = SURFACE_STYLE_USAGE ( .BOTH. , #68717 ) ;
#64467 = AXIS2_PLACEMENT_3D ( 'NONE', #60370, #17156, #27987 ) ;
#64468 = FACE_OUTER_BOUND ( 'NONE', #61346, .T. ) ;
#64469 = CARTESIAN_POINT ( 'NONE',  ( -4.041451884327378785, -1.417096231345241542, 7.000000000000000000 ) ) ;
#64470 = CARTESIAN_POINT ( 'NONE',  ( -66.80707362346618083, 10.01517768586948698, -1.839758294383808571E-15 ) ) ;
#64471 = AXIS2_PLACEMENT_3D ( 'NONE', #50184, #12516, #6218 ) ;
#64472 = EDGE_CURVE ( 'NONE', #34731, #37678, #51305, .T. ) ;
#64473 = CARTESIAN_POINT ( 'NONE',  ( -57.11974195712093660, -8.499999999999992895, 8.000000000000000000 ) ) ;
#64474 = AXIS2_PLACEMENT_3D ( 'NONE', #14841, #58097, #47590 ) ;
#64475 = VERTEX_POINT ( 'NONE', #9095 ) ;
#64476 = CARTESIAN_POINT ( 'NONE',  ( -71.50000000000000000, 14.49137674618942562, -7.500000000000000000 ) ) ;
#64478 =( NAMED_UNIT ( * ) SI_UNIT ( $, .STERADIAN. ) SOLID_ANGLE_UNIT ( ) );
#64477 = SURFACE_STYLE_USAGE ( .BOTH. , #44455 ) ;
#64479 = VECTOR ( 'NONE', #51698, 1000.000000000000000 ) ;
#64480 = CARTESIAN_POINT ( 'NONE',  ( -114.3549999999999898, -4.716976649647093289, -6.492361379858945902 ) ) ;
#64481 = CARTESIAN_POINT ( 'NONE',  ( 9.058813317711338797, 129.8449999999999989, -2.943386871421372675 ) ) ;
#64482 = CARTESIAN_POINT ( 'NONE',  ( -117.4449999999999932, 0.000000000000000000, 8.024999999999991473 ) ) ;
#64483 = CIRCLE ( 'NONE', #52154, 0.5000000000000004441 ) ;
#64484 = CARTESIAN_POINT ( 'NONE',  ( 22.50000000000000711, 34.24999999999999289, 3.750000000000000000 ) ) ;
#64485 = AXIS2_PLACEMENT_3D ( 'NONE', #39660, #12539, #2268 ) ;
#64487 = FACE_OUTER_BOUND ( 'NONE', #18937, .T. ) ;
#64486 = DIRECTION ( 'NONE',  ( 1.000000000000000000, 0.000000000000000000, 0.000000000000000000 ) ) ;
#64488 =( GEOMETRIC_REPRESENTATION_CONTEXT ( 3 ) GLOBAL_UNCERTAINTY_ASSIGNED_CONTEXT ( ( #55268 ) ) GLOBAL_UNIT_ASSIGNED_CONTEXT ( ( #16031, #32175, #42431 ) ) REPRESENTATION_CONTEXT ( 'NONE', 'WORKASPACE' ) );
#64489 = ADVANCED_FACE ( 'NONE', ( #3046 ), #18920, .F. ) ;
#64490 = CARTESIAN_POINT ( 'NONE',  ( -157.9429263765338192, 0.000000000000000000, 9.524999999999991473 ) ) ;
#64491 = CARTESIAN_POINT ( 'NONE',  ( -173.8449999999999989, -7.632228543268599452, 2.479861379858951054 ) ) ;
#64492 = ADVANCED_FACE ( 'NONE', ( #34758 ), #40416, .F. ) ;
#64493 = VECTOR ( 'NONE', #1584, 1000.000000000000227 ) ;
#64494 = ADVANCED_FACE ( 'NONE', ( #54136 ), #59401, .T. ) ;
#64495 = VECTOR ( 'NONE', #53674, 1000.000000000000000 ) ;
#64496 = CARTESIAN_POINT ( 'NONE',  ( -40.66238049145326272, -13.67042966192550502, 0.8504759240107299112 ) ) ;
#64497 = CARTESIAN_POINT ( 'NONE',  ( 74.99999999999998579, 50.00000000000000000, 7.500000000000000000 ) ) ;
#64498 = ORIENTED_EDGE ( 'NONE', *, *, #14145, .T. ) ;
#64499 = CARTESIAN_POINT ( 'NONE',  ( -78.89292637653380780, -8.102448949553172852, -5.886773742842741797 ) ) ;
#64500 = CONTEXT_DEPENDENT_SHAPE_REPRESENTATION ( #9204, #55370 ) ;
#64501 = DIRECTION ( 'NONE',  ( 1.000000000000000000, 0.000000000000000000, 0.000000000000000000 ) ) ;
#64502 = ADVANCED_FACE ( 'NONE', ( #28069 ), #22845, .T. ) ;
#64503 =( NAMED_UNIT ( * ) PLANE_ANGLE_UNIT ( ) SI_UNIT ( $, .RADIAN. ) );
#64504 = DIRECTION ( 'NONE',  ( -0.000000000000000000, -0.000000000000000000, -1.000000000000000000 ) ) ;
#64505 = EDGE_CURVE ( 'NONE', #31668, #65582, #29825, .T. ) ;
#64506 = CARTESIAN_POINT ( 'NONE',  ( -179.6049999999999898, 6.826472737025113702, -4.959722759717902107 ) ) ;
#64507 = AXIS2_PLACEMENT_3D ( 'NONE', #11636, #54540, #33101 ) ;
#64508 = ORIENTED_EDGE ( 'NONE', *, *, #35286, .T. ) ;
#64509 = SURFACE_SIDE_STYLE ('',( #10366 ) ) ;
#64510 = CARTESIAN_POINT ( 'NONE',  ( -74.45707362346617231, -9.058813317711329915, 2.943386871421371787 ) ) ;
#64511 = AXIS2_PLACEMENT_3D ( 'NONE', #49159, #48136, #181 ) ;
#64512 = DIRECTION ( 'NONE',  ( 0.000000000000000000, 0.000000000000000000, -1.000000000000000000 ) ) ;
#64513 = CARTESIAN_POINT ( 'NONE',  ( 7.632228543268607446, 141.1570736234661751, 2.479861379858954606 ) ) ;
#64514 = CIRCLE ( 'NONE', #18426, 6.999999999999997335 ) ;
#64515 = AXIS2_PLACEMENT_3D ( 'NONE', #50172, #18825, #44914 ) ;
#64516 = ORIENTED_EDGE ( 'NONE', *, *, #21368, .F. ) ;
#64517 = CARTESIAN_POINT ( 'NONE',  ( 57.24999999999999289, 27.99999999999998934, -4.000000000000000000 ) ) ;
#64518 = CARTESIAN_POINT ( 'NONE',  ( -91.55499999999997840, 0.000000000000000000, 8.024999999999991473 ) ) ;
#64519 = PRESENTATION_LAYER_ASSIGNMENT (  '', '', ( #35351 ) ) ;
#64520 = UNCERTAINTY_MEASURE_WITH_UNIT (LENGTH_MEASURE( 1.000000000000000082E-05 ), #33249, 'distance_accuracy_value', 'NONE');
#64521 = CARTESIAN_POINT ( 'NONE',  ( 10.00000000000000711, 50.00000000000000000, -59.99999999999999289 ) ) ;
#64522 = ORIENTED_EDGE ( 'NONE', *, *, #30569, .T. ) ;
#64523 = DIRECTION ( 'NONE',  ( 0.000000000000000000, 0.000000000000000000, -1.000000000000000000 ) ) ;
#64524 = VECTOR ( 'NONE', #62493, 1000.000000000000000 ) ;
#64525 = DIRECTION ( 'NONE',  ( -0.000000000000000000, -0.000000000000000000, 1.000000000000000000 ) ) ;
#64526 = EDGE_CURVE ( 'NONE', #2848, #60303, #17512, .T. ) ;
#64527 = DIRECTION ( 'NONE',  ( 0.000000000000000000, 0.000000000000000000, -1.000000000000000000 ) ) ;
#64528 = CARTESIAN_POINT ( 'NONE',  ( 4.000000000000001776, 43.00000000000000000, -90.00000000000000000 ) ) ;
#64529 =( LENGTH_UNIT ( ) NAMED_UNIT ( * ) SI_UNIT ( .MILLI., .METRE. ) );
#64530 = ORIENTED_EDGE ( 'NONE', *, *, #48565, .F. ) ;
#64531 = CARTESIAN_POINT ( 'NONE',  ( 21.00000000000001776, 15.00000000000000000, 29.68999999999999417 ) ) ;
#64532 = EDGE_CURVE ( 'NONE', #36018, #16885, #11934, .T. ) ;
#64533 = CARTESIAN_POINT ( 'NONE',  ( -66.44499999999999318, 0.000000000000000000, 8.024999999999991473 ) ) ;
#64534 = ORIENTED_EDGE ( 'NONE', *, *, #50669, .F. ) ;
#64535 =( NAMED_UNIT ( * ) PLANE_ANGLE_UNIT ( ) SI_UNIT ( $, .RADIAN. ) );
#64536 = AXIS2_PLACEMENT_3D ( 'NONE', #6658, #27417, #16235 ) ;
#64537 = STYLED_ITEM ( 'NONE', ( #18249 ), #7774 ) ;
#64538 = CARTESIAN_POINT ( 'NONE',  ( 6.000000000000017764, 16.44305403005404287, -2.635024667321593109E-15 ) ) ;
#64539 = ORIENTED_EDGE ( 'NONE', *, *, #15369, .F. ) ;
#64540 = PRESENTATION_STYLE_ASSIGNMENT (( #21980 ) ) ;
#64541 = ORIENTED_EDGE ( 'NONE', *, *, #12057, .F. ) ;
#64543 = FACE_OUTER_BOUND ( 'NONE', #8373, .T. ) ;
#64542 =( GEOMETRIC_REPRESENTATION_CONTEXT ( 3 ) GLOBAL_UNCERTAINTY_ASSIGNED_CONTEXT ( ( #9484 ) ) GLOBAL_UNIT_ASSIGNED_CONTEXT ( ( #29945, #50369, #40181 ) ) REPRESENTATION_CONTEXT ( 'NONE', 'WORKASPACE' ) );
#64544 = CARTESIAN_POINT ( 'NONE',  ( 53.25000000000000000, 25.24999999999998579, -3.750000000000000000 ) ) ;
#64545 = CARTESIAN_POINT ( 'NONE',  ( -126.8050000000000068, -8.437984349512085203, 5.166775262442717831E-16 ) ) ;
#64546 = ORIENTED_EDGE ( 'NONE', *, *, #50357, .T. ) ;
#64547 = CARTESIAN_POINT ( 'NONE',  ( -73.49292637653380211, -8.102448949553174629, 5.886773742842742685 ) ) ;
#64548 = ORIENTED_EDGE ( 'NONE', *, *, #12454, .F. ) ;
#64549 =( NAMED_UNIT ( * ) PLANE_ANGLE_UNIT ( ) SI_UNIT ( $, .RADIAN. ) );
#64550 = DIRECTION ( 'NONE',  ( 1.000000000000000000, 0.000000000000000000, 0.000000000000000000 ) ) ;
#64551 = VECTOR ( 'NONE', #12495, 1000.000000000000000 ) ;
#64552 = CARTESIAN_POINT ( 'NONE',  ( -162.3570736234661922, 5.598654528085804216, 7.705886871421366635 ) ) ;
#64553 = CARTESIAN_POINT ( 'NONE',  ( -10.01517768586949408, 128.1949999999999932, -6.132527647946036459E-16 ) ) ;
#64554 = CARTESIAN_POINT ( 'NONE',  ( -93.95707362346617231, 9.058813317711329915, -2.943386871421373119 ) ) ;
#64555 =( NAMED_UNIT ( * ) PLANE_ANGLE_UNIT ( ) SI_UNIT ( $, .RADIAN. ) );
#64556 = ORIENTED_EDGE ( 'NONE', *, *, #15309, .F. ) ;
#64557 = CIRCLE ( 'NONE', #8432, 0.5000000000000000000 ) ;
#64559 = FILL_AREA_STYLE_COLOUR ( '', #13351 ) ;
#64558 = FACE_OUTER_BOUND ( 'NONE', #34436, .T. ) ;
#64560 = DIRECTION ( 'NONE',  ( 1.000000000000000000, 0.000000000000000000, -1.300977106640434644E-16 ) ) ;
#64561 = PRESENTATION_LAYER_ASSIGNMENT (  '', '', ( #50016 ) ) ;
#64562 = CARTESIAN_POINT ( 'NONE',  ( -136.1049999999999898, -6.826472737025115478, 4.959722759717900331 ) ) ;
#64563 = SURFACE_STYLE_FILL_AREA ( #37536 ) ;
#64564 = EDGE_CURVE ( 'NONE', #59291, #52539, #65401, .T. ) ;
#64565 = CARTESIAN_POINT ( 'NONE',  ( -146.3950000000000102, -6.826472737025115478, -4.959722759717899443 ) ) ;
#64566 = AXIS2_PLACEMENT_3D ( 'NONE', #55368, #7192, #45203 ) ;
#64567 = CARTESIAN_POINT ( 'NONE',  ( -141.2949999999999875, -2.607480562269069768, 8.024999999999991473 ) ) ;
#64568 = B_SPLINE_CURVE_WITH_KNOTS ( 'NONE', 3,
 ( #12574, #33692, #55845, #39016, #66754, #7644, #28388, #50576 ),
 .UNSPECIFIED., .F., .F.,
 ( 4, 2, 2, 4 ),
 ( 0.01462827986756859780, 0.01731435831274189333, 0.01865739753532854109, 0.02000043675791518885 ),
 .UNSPECIFIED. ) ;
#64569 = VERTEX_POINT ( 'NONE', #28785 ) ;
#64570 = AXIS2_PLACEMENT_3D ( 'NONE', #49377, #42757, #21593 ) ;
#64571 = CARTESIAN_POINT ( 'NONE',  ( 44.88867800444037925, 10.61949827965496063, -3.673511479703639449 ) ) ;
#64572 = FACE_OUTER_BOUND ( 'NONE', #47884, .T. ) ;
#64573 = ADVANCED_FACE ( 'NONE', ( #623 ), #65030, .F. ) ;
#64574 = CARTESIAN_POINT ( 'NONE',  ( -8.750000000000001776, 24.74999999999998579, 4.000000000000000000 ) ) ;
#64575 = AXIS2_PLACEMENT_3D ( 'NONE', #11876, #566, #22091 ) ;
#64576 = CARTESIAN_POINT ( 'NONE',  ( -58.25499999999997414, -4.716976649647092401, 6.492361379858946790 ) ) ;
#64577 =( BOUNDED_CURVE ( )  B_SPLINE_CURVE ( 2, ( #68745, #68054, #8609, #24411, #46634, #41334, #62735, #14569, #9667, #36038, #41685 ),
 .UNSPECIFIED., .F., .F. ) 
 B_SPLINE_CURVE_WITH_KNOTS ( ( 3, 2, 2, 2, 2, 3 ),
 ( 0.2941176470588235392, 0.2999999999999999889, 0.3058823529411764941, 0.3117647058823529438, 0.3176470588235293935, 0.3235294117647058987 ),
 .UNSPECIFIED. ) 
 CURVE ( )  GEOMETRIC_REPRESENTATION_ITEM ( )  RATIONAL_B_SPLINE_CURVE ( ( 1.000000000000000000, 0.9510565162951535312, 1.000000000000000000, 0.9510565162951535312, 1.000000000000000000, 0.9510565162951535312, 1.000000000000000000, 0.9510565162951535312, 1.000000000000000000, 0.9510565162951535312, 1.000000000000000000 ) ) 
 REPRESENTATION_ITEM ( '' )  );
#64578 = CYLINDRICAL_SURFACE ( 'NONE', #61860, 0.5000000000000004441 ) ;
#64579 = CARTESIAN_POINT ( 'NONE',  ( -62.99499999999996902, -6.826472737025115478, 4.959722759717900331 ) ) ;
#64580 = B_SPLINE_CURVE_WITH_KNOTS ( 'NONE', 3,
 ( #54514, #17273, #6323, #7381, #66099, #22518, #55197, #43667 ),
 .UNSPECIFIED., .F., .F.,
 ( 4, 2, 2, 4 ),
 ( 2.544313220903533887E-07, 0.002693395767724532288, 0.004039966435925753697, 0.005386537104126974673 ),
 .UNSPECIFIED. ) ;
#64581 = EDGE_CURVE ( 'NONE', #3932, #9272, #37824, .T. ) ;
#64582 = DIRECTION ( 'NONE',  ( -1.000000000000000000, -0.000000000000000000, -0.000000000000000000 ) ) ;
#64583 = DIRECTION ( 'NONE',  ( -0.000000000000000000, -0.000000000000000000, -1.000000000000000000 ) ) ;
#64584 = CARTESIAN_POINT ( 'NONE',  ( -55.47019710162637551, -8.775703220318050057, -1.286986433361734461 ) ) ;
#64585 = CARTESIAN_POINT ( 'NONE',  ( -107.3929263765338078, 8.102448949553176405, 5.886773742842740909 ) ) ;
#64586 = DIRECTION ( 'NONE',  ( -1.249000902703301108E-16, 0.8519903597659395089, 0.5235574723618271475 ) ) ;
#64587 = CIRCLE ( 'NONE', #16315, 13.50000000000000533 ) ;
#64588 = CARTESIAN_POINT ( 'NONE',  ( -71.49999999999998579, 64.07124727947029896, 7.500000000000000000 ) ) ;
#64589 = AXIS2_PLACEMENT_3D ( 'NONE', #47316, #58514, #52905 ) ;
#64590 = FACE_OUTER_BOUND ( 'NONE', #34155, .T. ) ;
#64591 = CARTESIAN_POINT ( 'NONE',  ( 16.75000000000000711, 27.99999999999998224, -3.750000000000000000 ) ) ;
#64592 = EDGE_CURVE ( 'NONE', #21751, #28960, #16554, .T. ) ;
#64593 = LINE ( 'NONE', #69177, #56320 ) ;
#64594 = CARTESIAN_POINT ( 'NONE',  ( -7.632228543268607446, 138.5429263765338135, -2.479861379858953718 ) ) ;
#64595 = FILL_AREA_STYLE_COLOUR ( '', #57617 ) ;
#64597 = ORIENTED_EDGE ( 'NONE', *, *, #10422, .T. ) ;
#64596 = CIRCLE ( 'NONE', #35428, 12.50000000000000178 ) ;
#64598 = CIRCLE ( 'NONE', #44413, 13.00000000000000533 ) ;
#64599 =( BOUNDED_CURVE ( )  B_SPLINE_CURVE ( 2, ( #32885, #5419, #59235, #5097, #27575, #69470, #32184, #43815, #11060, #21258, #21623 ),
 .UNSPECIFIED., .F., .F. ) 
 B_SPLINE_CURVE_WITH_KNOTS ( ( 3, 2, 2, 2, 2, 3 ),
 ( 0.1739130434782566736, 0.1760869565217348942, 0.1782608695652131148, 0.1804347826086913353, 0.1826086956521695559, 0.1847826086956477487 ),
 .UNSPECIFIED. ) 
 CURVE ( )  GEOMETRIC_REPRESENTATION_ITEM ( )  RATIONAL_B_SPLINE_CURVE ( ( 1.000000000000094147, 0.9510565162950590512, 1.000000000000000000, 0.9510565162951535312, 1.000000000000000000, 0.9510565162951535312, 1.000000000000000000, 0.9510565162951535312, 1.000000000000000000, 0.9510565162952528961, 0.9999999999999006350 ) ) 
 REPRESENTATION_ITEM ( '' )  );
#64600 = CARTESIAN_POINT ( 'NONE',  ( 7.632228543268607446, 117.1570736234661609, 2.479861379858954606 ) ) ;
#64601 = CARTESIAN_POINT ( 'NONE',  ( 74.62643842725373133, 19.76989462323605906, -6.307273367294813582 ) ) ;
#64602 = ORIENTED_EDGE ( 'NONE', *, *, #45796, .F. ) ;
#64603 = ORIENTED_EDGE ( 'NONE', *, *, #20735, .T. ) ;
#64604 = CARTESIAN_POINT ( 'NONE',  ( -4.682380833558966060, -2.003239292658526516, -5.889878495889164789 ) ) ;
#64605 = DIRECTION ( 'NONE',  ( -1.000000000000000000, -0.000000000000000000, -0.000000000000000000 ) ) ;
#64606 = COLOUR_RGB ( '', 0.31764706, 0.68627451, 0.89019608) ;
#64607 = PRESENTATION_STYLE_ASSIGNMENT (( #42846 ) ) ;
#64608 = ORIENTED_EDGE ( 'NONE', *, *, #26518, .T. ) ;
#64609 = CARTESIAN_POINT ( 'NONE',  ( 0.000000000000000000, 131.5549999999999784, -9.525000000000000355 ) ) ;
#64610 = DIRECTION ( 'NONE',  ( -0.000000000000000000, 0.000000000000000000, -1.000000000000000000 ) ) ;
#64611 =( NAMED_UNIT ( * ) PLANE_ANGLE_UNIT ( ) SI_UNIT ( $, .RADIAN. ) );
#64612 = DIRECTION ( 'NONE',  ( 1.000000000000000000, 0.000000000000000000, 0.000000000000000000 ) ) ;
#64613 = EDGE_CURVE ( 'NONE', #60581, #55705, #17555, .T. ) ;
#64614 = CARTESIAN_POINT ( 'NONE',  ( -100.1949999999999790, 8.437984349512085203, -1.550032578732815448E-15 ) ) ;
#64615 = ORIENTED_EDGE ( 'NONE', *, *, #46555, .F. ) ;
#64616 = AXIS2_PLACEMENT_3D ( 'NONE', #16952, #48282, #38439 ) ;
#64617 = DIRECTION ( 'NONE',  ( 0.000000000000000000, 0.000000000000000000, 1.000000000000000000 ) ) ;
#64618 = COLOUR_RGB ( '', 0.40784314, 0.44705882, 0.49803922) ;
#64619 = VERTEX_POINT ( 'NONE', #27730 ) ;
#64620 =( LENGTH_UNIT ( ) NAMED_UNIT ( * ) SI_UNIT ( .MILLI., .METRE. ) );
#64621 = DIRECTION ( 'NONE',  ( -1.000000000000000000, -0.000000000000000000, -0.000000000000000000 ) ) ;
#64622 = ORIENTED_EDGE ( 'NONE', *, *, #43407, .F. ) ;
#64623 = DIRECTION ( 'NONE',  ( 0.5000000000000001110, 0.8660254037844385966, 0.000000000000000000 ) ) ;
#64624 = ORIENTED_EDGE ( 'NONE', *, *, #65289, .F. ) ;
#64625 = CARTESIAN_POINT ( 'NONE',  ( -165.0570736234661524, 0.000000000000000000, 9.524999999999991473 ) ) ;
#64626 = CARTESIAN_POINT ( 'NONE',  ( 68.99999999999998579, 1.000000000000008438, -3.000000000000000000 ) ) ;
#64627 = CARTESIAN_POINT ( 'NONE',  ( -4.041451884327378785, 2.500000000000000000, 7.000000000000000000 ) ) ;
#64628 = FACE_OUTER_BOUND ( 'NONE', #43457, .T. ) ;
#64629 =( LENGTH_UNIT ( ) NAMED_UNIT ( * ) SI_UNIT ( .MILLI., .METRE. ) );
#64630 = MECHANICAL_DESIGN_GEOMETRIC_PRESENTATION_REPRESENTATION (  '', ( #32043 ), #47873 ) ;
#64631 = CARTESIAN_POINT ( 'NONE',  ( -60.05707362346616662, 0.000000000000000000, 9.524999999999991473 ) ) ;
#64632 = LINE ( 'NONE', #36893, #9116 ) ;
#64633 = CARTESIAN_POINT ( 'NONE',  ( -10.11618306975752368, 54.14354156754873060, 2.000000000000000000 ) ) ;
#64634 = ORIENTED_EDGE ( 'NONE', *, *, #5778, .T. ) ;
#64635 = ORIENTED_EDGE ( 'NONE', *, *, #50645, .F. ) ;
#64636 = CARTESIAN_POINT ( 'NONE',  ( -48.35707362346617089, 5.598654528085804216, 7.705886871421366635 ) ) ;
#64637 = DIRECTION ( 'NONE',  ( 2.312964634635740689E-15, -1.000000000000000000, 0.000000000000000000 ) ) ;
#64638 = FACE_OUTER_BOUND ( 'NONE', #64690, .T. ) ;
#64640 = DIRECTION ( 'NONE',  ( 0.6216216216216191581, -0.7833176619561879050, 0.000000000000000000 ) ) ;
#64639 = VECTOR ( 'NONE', #43518, 1000.000000000000000 ) ;
#64641 = EDGE_LOOP ( 'NONE', ( #3226, #51112, #6016, #28443, #57878, #30046 ) ) ;
#64642 = CARTESIAN_POINT ( 'NONE',  ( -171.2049999999999841, -2.607480562269071545, -8.024999999999991473 ) ) ;
#64643 = DIRECTION ( 'NONE',  ( 0.000000000000000000, 0.000000000000000000, -1.000000000000000000 ) ) ;
#64644 = DIRECTION ( 'NONE',  ( 0.000000000000000000, 0.000000000000000000, -1.000000000000000000 ) ) ;
#64645 = EDGE_CURVE ( 'NONE', #55705, #51980, #17903, .T. ) ;
#64646 = CARTESIAN_POINT ( 'NONE',  ( -174.2949999999999591, -2.607480562269069768, 8.024999999999991473 ) ) ;
#64647 = CIRCLE ( 'NONE', #44501, 1.000000000000000888 ) ;
#64648 = AXIS2_PLACEMENT_3D ( 'NONE', #47109, #58316, #69230 ) ;
#64649 = CARTESIAN_POINT ( 'NONE',  ( -162.7450000000000045, 4.716976649647094177, 6.492361379858945902 ) ) ;
#64650 = ORIENTED_EDGE ( 'NONE', *, *, #31106, .T. ) ;
#64651 = DIRECTION ( 'NONE',  ( 1.000000000000000000, 0.000000000000000000, 0.000000000000000000 ) ) ;
#64652 = CARTESIAN_POINT ( 'NONE',  ( 45.00000000000000000, -1.469576158976824618E-14, 10.00000000000000000 ) ) ;
#64653 = CARTESIAN_POINT ( 'NONE',  ( -79.40500000000000114, -2.607480562269069768, 8.024999999999991473 ) ) ;
#64654 = DIRECTION ( 'NONE',  ( 0.000000000000000000, 0.000000000000000000, -1.000000000000000000 ) ) ;
#64655 = SURFACE_STYLE_FILL_AREA ( #43250 ) ;
#64656 = CARTESIAN_POINT ( 'NONE',  ( 0.000000000000000000, 149.9999999999999716, 0.000000000000000000 ) ) ;
#64657 = VECTOR ( 'NONE', #33785, 1000.000000000000000 ) ;
#64658 = EDGE_CURVE ( 'NONE', #59896, #57410, #67150, .T. ) ;
#64659 = CARTESIAN_POINT ( 'NONE',  ( -76.49499999999999034, 6.826472737025113702, -4.959722759717902107 ) ) ;
#64660 = CARTESIAN_POINT ( 'NONE',  ( 5.598654528085809545, 137.2549999999999955, -7.705886871421373741 ) ) ;
#64661 = FACE_OUTER_BOUND ( 'NONE', #36547, .T. ) ;
#64662 = AXIS2_PLACEMENT_3D ( 'NONE', #30951, #35202, #8486 ) ;
#64663 = CARTESIAN_POINT ( 'NONE',  ( -170.3929263765337794, 8.102448949553176405, 5.886773742842740909 ) ) ;
#64664 = ADVANCED_FACE ( 'NONE', ( #46404 ), #62184, .T. ) ;
#64665 = DIRECTION ( 'NONE',  ( 0.000000000000000000, 0.000000000000000000, -1.000000000000000000 ) ) ;
#64666 = STYLED_ITEM ( 'NONE', ( #20387 ), #56958 ) ;
#64667 = CARTESIAN_POINT ( 'NONE',  ( -73.94292637653379074, 0.000000000000000000, 9.524999999999991473 ) ) ;
#64668 = CYLINDRICAL_SURFACE ( 'NONE', #62922, 0.2500000000000002220 ) ;
#64669 = EDGE_LOOP ( 'NONE', ( #2810, #58456, #11583, #22910 ) ) ;
#64670 = ADVANCED_FACE ( 'NONE', ( #40411 ), #66429, .F. ) ;
#64671 = CARTESIAN_POINT ( 'NONE',  ( 6.418790567836325955, -2.472216779103306283, -2.882328613363592584 ) ) ;
#64672 = CARTESIAN_POINT ( 'NONE',  ( -50.09292637653378222, 3.094860106618433360, 9.524999999999991473 ) ) ;
#64673 = EDGE_CURVE ( 'NONE', #58485, #30209, #51233, .T. ) ;
#64674 = LINE ( 'NONE', #22445, #34941 ) ;
#64676 = DIRECTION ( 'NONE',  ( -0.000000000000000000, -0.000000000000000000, -1.000000000000000000 ) ) ;
#64675 = CARTESIAN_POINT ( 'NONE',  ( -78.05707362346616662, 0.000000000000000000, 9.524999999999991473 ) ) ;
#64677 = CARTESIAN_POINT ( 'NONE',  ( -4.716976649647097730, 136.3570736234661638, -6.492361379858953896 ) ) ;
#64678 = VERTEX_POINT ( 'NONE', #13295 ) ;
#64679 = ORIENTED_EDGE ( 'NONE', *, *, #38955, .T. ) ;
#64680 = CARTESIAN_POINT ( 'NONE',  ( -15.98999599679679839, 118.4999999999999716, 7.500000000000000000 ) ) ;
#64681 = DIRECTION ( 'NONE',  ( 0.000000000000000000, 0.000000000000000000, -1.000000000000000000 ) ) ;
#64682 = CARTESIAN_POINT ( 'NONE',  ( -71.50000000000000000, 14.49137674618942562, 9.500000000000000000 ) ) ;
#64683 = CARTESIAN_POINT ( 'NONE',  ( 2.607480562269155921, 139.5929263765337964, 8.024999999999941735 ) ) ;
#64684 = ORIENTED_EDGE ( 'NONE', *, *, #9944, .F. ) ;
#64685 = CARTESIAN_POINT ( 'NONE',  ( -108.2049999999999983, -2.607480562269071545, -8.024999999999991473 ) ) ;
#64686 = ORIENTED_EDGE ( 'NONE', *, *, #51397, .T. ) ;
#64687 = COLOUR_RGB ( '', 0.08235294, 0.09019608, 0.10196078) ;
#64688 = CARTESIAN_POINT ( 'NONE',  ( 0.000000000000000000, -2.500000000000000000, 0.000000000000000000 ) ) ;
#64689 = CYLINDRICAL_SURFACE ( 'NONE', #61311, 11.99999999999999645 ) ;
#64690 = EDGE_LOOP ( 'NONE', ( #14689, #37857, #56731, #28767 ) ) ;
#64691 = DIRECTION ( 'NONE',  ( 0.000000000000000000, 1.000000000000000000, -0.000000000000000000 ) ) ;
#64692 = ORIENTED_EDGE ( 'NONE', *, *, #45805, .T. ) ;
#64693 = MECHANICAL_DESIGN_GEOMETRIC_PRESENTATION_REPRESENTATION (  '', ( #10810 ), #65854 ) ;
#64694 = PRESENTATION_LAYER_ASSIGNMENT (  '', '', ( #6281 ) ) ;
#64695 = AXIS2_PLACEMENT_3D ( 'NONE', #912, #38338, #39703 ) ;
#64696 = CARTESIAN_POINT ( 'NONE',  ( 0.000000000000000000, 119.9429263765338050, -8.025000000000000355 ) ) ;
#64697 = SURFACE_STYLE_FILL_AREA ( #11559 ) ;
#64698 = CARTESIAN_POINT ( 'NONE',  ( 30.50000000000001066, 15.99999999999997691, 4.000000000000000000 ) ) ;
#64699 =( BOUNDED_CURVE ( )  B_SPLINE_CURVE ( 3, ( #23260, #6376, #27804, #18339 ),
 .UNSPECIFIED., .F., .F. ) 
 B_SPLINE_CURVE_WITH_KNOTS ( ( 4, 4 ),
 ( 3.043785426622117374, 4.712388980384689674 ),
 .UNSPECIFIED. ) 
 CURVE ( )  GEOMETRIC_REPRESENTATION_ITEM ( )  RATIONAL_B_SPLINE_CURVE ( ( 1.000000000000000000, 0.7811300729168891843, 0.7811300729168891843, 1.000000000000000000 ) ) 
 REPRESENTATION_ITEM ( '' )  );
#64700 = ORIENTED_EDGE ( 'NONE', *, *, #44364, .F. ) ;
#64701 = SURFACE_STYLE_USAGE ( .BOTH. , #64343 ) ;
#64702 = CARTESIAN_POINT ( 'NONE',  ( -15.00000000000000000, -10.90871211463571200, 5.000000000000000000 ) ) ;
#64703 = DIRECTION ( 'NONE',  ( -1.000000000000000000, 0.000000000000000000, 0.000000000000000000 ) ) ;
#64704 = ORIENTED_EDGE ( 'NONE', *, *, #41004, .F. ) ;
#64705 = CARTESIAN_POINT ( 'NONE',  ( -7.632228543268608334, 123.8429263765338249, 2.479861379858952830 ) ) ;
#64706 =( NAMED_UNIT ( * ) SI_UNIT ( $, .STERADIAN. ) SOLID_ANGLE_UNIT ( ) );
#64707 =( NAMED_UNIT ( * ) SI_UNIT ( $, .STERADIAN. ) SOLID_ANGLE_UNIT ( ) );
#64708 = SURFACE_SIDE_STYLE ('',( #262 ) ) ;
#64709 = CIRCLE ( 'NONE', #36688, 3.100000000000005418 ) ;
#64710 = EDGE_LOOP ( 'NONE', ( #49316, #65797, #51930, #30229 ) ) ;
#64711 = FACE_OUTER_BOUND ( 'NONE', #56280, .T. ) ;
#64712 = ORIENTED_EDGE ( 'NONE', *, *, #33378, .F. ) ;
#64713 = CARTESIAN_POINT ( 'NONE',  ( -53.09292637653378932, 3.094860106618433360, 9.524999999999991473 ) ) ;
#64714 = CARTESIAN_POINT ( 'NONE',  ( -147.2050000000000125, -2.607480562269071545, -8.024999999999991473 ) ) ;
#64715 = CARTESIAN_POINT ( 'NONE',  ( -60.00000000000000000, -2.024042244987997205E-14, 7.000000000000000000 ) ) ;
#64716 = CARTESIAN_POINT ( 'NONE',  ( -24.21231517720798010, 112.4999999999999858, 10.00000000000000000 ) ) ;
#64717 = VECTOR ( 'NONE', #18227, 1000.000000000000000 ) ;
#64718 = CARTESIAN_POINT ( 'NONE',  ( -44.54421273840488738, -13.99257275267859413, 0.7732724246005804325 ) ) ;
#64719 = PRESENTATION_STYLE_ASSIGNMENT (( #16898 ) ) ;
#64720 = ORIENTED_EDGE ( 'NONE', *, *, #67595, .T. ) ;
#64721 = ORIENTED_EDGE ( 'NONE', *, *, #11826, .F. ) ;
#64722 = CARTESIAN_POINT ( 'NONE',  ( 44.99999999999977973, 147.4999999999999716, 10.00000000000000000 ) ) ;
#64723 = CARTESIAN_POINT ( 'NONE',  ( -54.35499999999998977, -4.716976649647093289, -6.492361379858945902 ) ) ;
#64724 = VERTEX_POINT ( 'NONE', #35474 ) ;
#64725 = CYLINDRICAL_SURFACE ( 'NONE', #60673, 1.000000000000000888 ) ;
#64726 = LINE ( 'NONE', #27055, #60687 ) ;
#64727 = DIRECTION ( 'NONE',  ( 0.000000000000000000, -1.000000000000000000, 0.000000000000000000 ) ) ;
#64728 =( NAMED_UNIT ( * ) PLANE_ANGLE_UNIT ( ) SI_UNIT ( $, .RADIAN. ) );
#64729 = EDGE_CURVE ( 'NONE', #8613, #27375, #9896, .T. ) ;
#64730 = CARTESIAN_POINT ( 'NONE',  ( -97.49292637653380211, -8.102448949553174629, 5.886773742842742685 ) ) ;
#64732 = EDGE_CURVE ( 'NONE', #3817, #6686, #62467, .T. ) ;
#64731 = ORIENTED_EDGE ( 'NONE', *, *, #39826, .T. ) ;
#64733 =( GEOMETRIC_REPRESENTATION_CONTEXT ( 3 ) GLOBAL_UNCERTAINTY_ASSIGNED_CONTEXT ( ( #7451 ) ) GLOBAL_UNIT_ASSIGNED_CONTEXT ( ( #28264, #19388, #65935 ) ) REPRESENTATION_CONTEXT ( 'NONE', 'WORKASPACE' ) );
#64734 = EDGE_CURVE ( 'NONE', #57704, #23416, #57728, .T. ) ;
#64735 = DIRECTION ( 'NONE',  ( -0.000000000000000000, -0.000000000000000000, -1.000000000000000000 ) ) ;
#64736 = FACE_OUTER_BOUND ( 'NONE', #40732, .T. ) ;
#64737 = FACE_OUTER_BOUND ( 'NONE', #58626, .T. ) ;
#64738 = CARTESIAN_POINT ( 'NONE',  ( 23.50000000000001776, -3.148064030671221758, 29.68999999999999417 ) ) ;
#64739 = ADVANCED_FACE ( 'NONE', ( #19626 ), #35813, .F. ) ;
#64740 = EDGE_CURVE ( 'NONE', #66764, #28375, #18701, .T. ) ;
#64741 = CARTESIAN_POINT ( 'NONE',  ( -109.1949999999999790, 8.437984349512086979, -1.550032578732815448E-15 ) ) ;
#64742 = CARTESIAN_POINT ( 'NONE',  ( 9.058813317711337021, 112.6549999999999869, 2.943386871421375783 ) ) ;
#64743 = AXIS2_PLACEMENT_3D ( 'NONE', #6208, #53374, #49147 ) ;
#64744 = CARTESIAN_POINT ( 'NONE',  ( -87.44499999999999318, 0.000000000000000000, 8.024999999999991473 ) ) ;
#64745 = ADVANCED_FACE ( 'NONE', ( #18606 ), #61473, .T. ) ;
#64746 = DIRECTION ( 'NONE',  ( 0.000000000000000000, 0.7071067811865451302, 0.7071067811865500152 ) ) ;
#64747 = DIRECTION ( 'NONE',  ( 1.000000000000000000, 0.000000000000000000, 0.000000000000000000 ) ) ;
#64748 = CARTESIAN_POINT ( 'NONE',  ( -4.358330484967981810, 1.733974831985838794, -6.451150163859153963 ) ) ;
#64749 = DIRECTION ( 'NONE',  ( -1.000000000000000000, 0.000000000000000000, 0.000000000000000000 ) ) ;
#64750 = ORIENTED_EDGE ( 'NONE', *, *, #8533, .F. ) ;
#64751 = EDGE_CURVE ( 'NONE', #40236, #7265, #67125, .T. ) ;
#64752 = CARTESIAN_POINT ( 'NONE',  ( -123.1429263765338078, 5.598654528085800663, -7.705886871421367523 ) ) ;
#64753 = CARTESIAN_POINT ( 'NONE',  ( -145.3449999999999989, 7.632228543268599452, -2.479861379858951942 ) ) ;
#64754 = DIRECTION ( 'NONE',  ( 0.000000000000000000, 1.000000000000000000, 0.000000000000000000 ) ) ;
#64755 = AXIS2_PLACEMENT_3D ( 'NONE', #55063, #54032, #1204 ) ;
#64756 = CYLINDRICAL_SURFACE ( 'NONE', #64423, 0.2500000000000002220 ) ;
#64757 = FILL_AREA_STYLE_COLOUR ( '', #12554 ) ;
#64758 = ORIENTED_EDGE ( 'NONE', *, *, #39911, .T. ) ;
#64759 = ORIENTED_EDGE ( 'NONE', *, *, #38614, .F. ) ;
#64760 = CARTESIAN_POINT ( 'NONE',  ( 60.00000000000000000, 1.797044900979284448E-15, -12.00000000000000000 ) ) ;
#64761 = CARTESIAN_POINT ( 'NONE',  ( 3.249999999999998668, 36.74999999999999289, -3.750000000000000000 ) ) ;
#64762 = CARTESIAN_POINT ( 'NONE',  ( -11.74999999999999645, -4.000000000000000000, 19.00000000000000000 ) ) ;
#64763 = CARTESIAN_POINT ( 'NONE',  ( -45.00000000000000000, 8.588294701370031703, 5.575869277511095845 ) ) ;
#64764 = CARTESIAN_POINT ( 'NONE',  ( 22.99999999999996447, 5.000000000000000000, -29.00402776293825369 ) ) ;
#64765 = CARTESIAN_POINT ( 'NONE',  ( -116.3929263765338078, 8.102448949553176405, 5.886773742842740909 ) ) ;
#64766 = ORIENTED_EDGE ( 'NONE', *, *, #39521, .T. ) ;
#64767 = CARTESIAN_POINT ( 'NONE',  ( -138.8050000000000068, -8.437984349512086979, 5.166775262442717831E-16 ) ) ;
#64768 = ORIENTED_EDGE ( 'NONE', *, *, #67909, .F. ) ;
#64769 = ORIENTED_EDGE ( 'NONE', *, *, #56534, .T. ) ;
#64770 =( LENGTH_UNIT ( ) NAMED_UNIT ( * ) SI_UNIT ( .MILLI., .METRE. ) );
#64771 = CARTESIAN_POINT ( 'NONE',  ( 14.98999599679679662, 117.9999999999999716, 9.500000000000000000 ) ) ;
#64772 = ORIENTED_EDGE ( 'NONE', *, *, #36584, .T. ) ;
#64773 = CARTESIAN_POINT ( 'NONE',  ( -56.67071223451711859, -8.499999999999992895, -0.2282353707497825623 ) ) ;
#64774 = SURFACE_STYLE_FILL_AREA ( #43383 ) ;
#64775 = CARTESIAN_POINT ( 'NONE',  ( -9.058813317711337021, 134.0449999999999875, -2.943386871421374895 ) ) ;
#64776 = CARTESIAN_POINT ( 'NONE',  ( 74.99999999999998579, 50.00000000000000000, -7.000000000000000000 ) ) ;
#64777 = ADVANCED_FACE ( 'NONE', ( #8398 ), #43456, .T. ) ;
#64778 = ORIENTED_EDGE ( 'NONE', *, *, #59817, .F. ) ;
#64779 = LINE ( 'NONE', #17319, #6022 ) ;
#64780 = CARTESIAN_POINT ( 'NONE',  ( -9.058813317711338797, 126.4549999999999841, 2.943386871421373563 ) ) ;
#64781 = CARTESIAN_POINT ( 'NONE',  ( -64.10499999999997556, -6.826472737025113702, 4.959722759717902107 ) ) ;
#64782 = CARTESIAN_POINT ( 'NONE',  ( -120.7449999999999903, 4.716976649647094177, 6.492361379858945902 ) ) ;
#64783 = CARTESIAN_POINT ( 'NONE',  ( 2.000000000000008438, 50.00000000000000000, -65.00000000000000000 ) ) ;
#64784 = PRODUCT ( '10. Bolt M10x25', '10. Bolt M10x25', '', ( #34630 ) ) ;
#64785 = ORIENTED_EDGE ( 'NONE', *, *, #66902, .F. ) ;
#64786 = CARTESIAN_POINT ( 'NONE',  ( -3.094860106618432471, 146.7049999999999841, -9.525000000000000355 ) ) ;
#64787 = COLOUR_RGB ( '', 0.66274510, 0.83137255, 0.94901961) ;
#64788 = LINE ( 'NONE', #21172, #46686 ) ;
#64789 = DIRECTION ( 'NONE',  ( 1.000000000000000000, 0.000000000000000000, 0.000000000000000000 ) ) ;
#64790 = CIRCLE ( 'NONE', #28865, 0.2500000000000002220 ) ;
#64791 = ORIENTED_EDGE ( 'NONE', *, *, #29221, .T. ) ;
#64792 = FACE_OUTER_BOUND ( 'NONE', #56716, .T. ) ;
#64793 = SURFACE_SIDE_STYLE ('',( #33809 ) ) ;
#64794 = CARTESIAN_POINT ( 'NONE',  ( -170.1550000000000011, 7.632228543268600340, 2.479861379858949277 ) ) ;
#64795 = ORIENTED_EDGE ( 'NONE', *, *, #381, .T. ) ;
#64796 = SURFACE_SIDE_STYLE ('',( #367 ) ) ;
#64797 = CARTESIAN_POINT ( 'NONE',  ( -16.75000000000000000, -0.9999999999999995559, 20.00000000000000000 ) ) ;
#64798 = FILL_AREA_STYLE ('',( #64099 ) ) ;
#64799 = CARTESIAN_POINT ( 'NONE',  ( -74.50000000000000000, -1.856352308976905642E-14, 6.500000000000000000 ) ) ;
#64800 = ORIENTED_EDGE ( 'NONE', *, *, #53382, .T. ) ;
#64801 = FILL_AREA_STYLE ('',( #43414 ) ) ;
#64802 = CARTESIAN_POINT ( 'NONE',  ( -86.30499999999997840, 8.437984349512085203, -1.550032578732815448E-15 ) ) ;
#64803 = ORIENTED_EDGE ( 'NONE', *, *, #6006, .F. ) ;
#64804 = ADVANCED_FACE ( 'NONE', ( #35115 ), #9731, .F. ) ;
#64805 = DIRECTION ( 'NONE',  ( -1.000000000000000000, 0.000000000000000000, -0.000000000000000000 ) ) ;
#64806 = DIRECTION ( 'NONE',  ( 1.000000000000000000, 0.000000000000000000, 0.000000000000000000 ) ) ;
#64807 =( NAMED_UNIT ( * ) SI_UNIT ( $, .STERADIAN. ) SOLID_ANGLE_UNIT ( ) );
#64808 = CARTESIAN_POINT ( 'NONE',  ( -61.40707362346618226, 3.094860106618428031, -9.524999999999993250 ) ) ;
#64809 = EDGE_CURVE ( 'NONE', #38944, #11547, #67003, .T. ) ;
#64810 =( GEOMETRIC_REPRESENTATION_CONTEXT ( 3 ) GLOBAL_UNCERTAINTY_ASSIGNED_CONTEXT ( ( #6530 ) ) GLOBAL_UNIT_ASSIGNED_CONTEXT ( ( #156, #64611, #11475 ) ) REPRESENTATION_CONTEXT ( 'NONE', 'WORKASPACE' ) );
#64811 = FACE_OUTER_BOUND ( 'NONE', #43886, .T. ) ;
#64812 = VERTEX_POINT ( 'NONE', #42189 ) ;
#64813 = CARTESIAN_POINT ( 'NONE',  ( 0.000000000000000000, 114.4999999999999574, 0.000000000000000000 ) ) ;
#64815 = DIRECTION ( 'NONE',  ( -0.000000000000000000, -0.000000000000000000, 1.000000000000000000 ) ) ;
#64814 = FILL_AREA_STYLE ('',( #60233 ) ) ;
#64816 = CARTESIAN_POINT ( 'NONE',  ( -105.5049999999999812, -6.826472737025115478, -4.959722759717899443 ) ) ;
#64817 = CARTESIAN_POINT ( 'NONE',  ( -9.058813317711337021, 131.0449999999999875, -2.943386871421374895 ) ) ;
#64818 = CARTESIAN_POINT ( 'NONE',  ( -114.5949999999999704, 2.607480562269073321, 8.024999999999991473 ) ) ;
#64819 = EDGE_CURVE ( 'NONE', #4261, #2790, #69220, .T. ) ;
#64820 = DIRECTION ( 'NONE',  ( 0.000000000000000000, -0.000000000000000000, 1.000000000000000000 ) ) ;
#64821 = DIRECTION ( 'NONE',  ( 0.000000000000000000, -1.000000000000000000, 0.000000000000000000 ) ) ;
#64822 = ADVANCED_FACE ( 'NONE', ( #25931 ), #31906, .T. ) ;
#64823 = CARTESIAN_POINT ( 'NONE',  ( -161.0929263765338249, 3.094860106618433360, 9.524999999999991473 ) ) ;
#64824 =( NAMED_UNIT ( * ) SI_UNIT ( $, .STERADIAN. ) SOLID_ANGLE_UNIT ( ) );
#64825 = CARTESIAN_POINT ( 'NONE',  ( -176.5450000000000159, -7.632228543268600340, -2.479861379858950166 ) ) ;
#64826 = MECHANICAL_DESIGN_GEOMETRIC_PRESENTATION_REPRESENTATION (  '', ( #37971 ), #22203 ) ;
#64827 = CARTESIAN_POINT ( 'NONE',  ( -4.716976649647098618, 149.2570736234661695, 6.492361379858953008 ) ) ;
#64828 = CARTESIAN_POINT ( 'NONE',  ( 6.887213563469345878, 6.070996185493600095, 0.1702817813269535685 ) ) ;
#64829 = ORIENTED_EDGE ( 'NONE', *, *, #42787, .T. ) ;
#64830 = DIRECTION ( 'NONE',  ( 1.000000000000000000, -0.000000000000000000, 0.000000000000000000 ) ) ;
#64831 = SPHERICAL_SURFACE ( 'NONE', #40695, 1.000000000000000000 ) ;
#64832 = ORIENTED_EDGE ( 'NONE', *, *, #32331, .F. ) ;
#64833 = CARTESIAN_POINT ( 'NONE',  ( -78.14292637653380780, 5.598654528085800663, -7.705886871421367523 ) ) ;
#64834 = ITEM_DEFINED_TRANSFORMATION ( 'NONE', 'NONE', #5662,  #42840 ) ;
#64835 = DIRECTION ( 'NONE',  ( 0.000000000000000000, 0.000000000000000000, 1.000000000000000000 ) ) ;
#64836 = DIRECTION ( 'NONE',  ( 0.000000000000000000, 0.000000000000000000, 1.000000000000000000 ) ) ;
#64837 = CARTESIAN_POINT ( 'NONE',  ( 67.50000000000000000, 1.797044900979284448E-15, 11.50000000000000000 ) ) ;
#64838 = AXIS2_PLACEMENT_3D ( 'NONE', #33802, #28145, #11661 ) ;
#64839 = ORIENTED_EDGE ( 'NONE', *, *, #21496, .F. ) ;
#64840 = CARTESIAN_POINT ( 'NONE',  ( -176.4550000000000125, 7.632228543268599452, -2.479861379858951942 ) ) ;
#64841 = EDGE_LOOP ( 'NONE', ( #3675, #39877, #25149, #27034 ) ) ;
#64842 =( NAMED_UNIT ( * ) SI_UNIT ( $, .STERADIAN. ) SOLID_ANGLE_UNIT ( ) );
#64843 = SURFACE_STYLE_USAGE ( .BOTH. , #59559 ) ;
#64844 = DIRECTION ( 'NONE',  ( -5.782411586589351722E-16, 1.000000000000000000, 0.000000000000000000 ) ) ;
#64845 = CARTESIAN_POINT ( 'NONE',  ( -183.0000000000000284, -1.154738647139537111, 9.454745033939424559 ) ) ;
#64846 = CARTESIAN_POINT ( 'NONE',  ( -4.716976649647098618, 140.2570736234661410, 6.492361379858953008 ) ) ;
#64847 = ADVANCED_FACE ( 'NONE', ( #53705 ), #5493, .T. ) ;
#64848 =( REPRESENTATION_RELATIONSHIP ('NONE','NONE', #5102, #14155 ) REPRESENTATION_RELATIONSHIP_WITH_TRANSFORMATION ( #35346 )SHAPE_REPRESENTATION_RELATIONSHIP( ) );
#64849 = ORIENTED_EDGE ( 'NONE', *, *, #26453, .T. ) ;
#64850 = FACE_BOUND ( 'NONE', #32515, .T. ) ;
#64851 = CARTESIAN_POINT ( 'NONE',  ( -89.45499999999999829, 7.632228543268599452, -2.479861379858951942 ) ) ;
#64852 = CARTESIAN_POINT ( 'NONE',  ( 54.99999999999999289, 2.409368300552961372E-15, -12.00000000000000000 ) ) ;
#64853 = ORIENTED_EDGE ( 'NONE', *, *, #16037, .F. ) ;
#64854 = DIRECTION ( 'NONE',  ( 0.000000000000000000, 1.000000000000000000, 0.000000000000000000 ) ) ;
#64855 = SURFACE_STYLE_USAGE ( .BOTH. , #43473 ) ;
#64856 = DIRECTION ( 'NONE',  ( -1.000000000000000000, 0.000000000000000000, 0.000000000000000000 ) ) ;
#64857 = ORIENTED_EDGE ( 'NONE', *, *, #65799, .F. ) ;
#64858 = CARTESIAN_POINT ( 'NONE',  ( -64.19499999999999318, 8.437984349512085203, -1.550032578732815448E-15 ) ) ;
#64859 = EDGE_LOOP ( 'NONE', ( #8507, #52671, #5295, #41584 ) ) ;
#64860 = PRODUCT_DEFINITION ( 'UNKNOWN', '', #15801, #19135 ) ;
#64861 = ADVANCED_FACE ( 'NONE', ( #36190 ), #53388, .T. ) ;
#64862 = SURFACE_SIDE_STYLE ('',( #7175 ) ) ;
#64863 = CARTESIAN_POINT ( 'NONE',  ( -138.3570736234661638, 5.598654528085804216, 7.705886871421366635 ) ) ;
#64864 = EDGE_LOOP ( 'NONE', ( #64924, #69614, #22495, #17746 ) ) ;
#64865 = CARTESIAN_POINT ( 'NONE',  ( 31.00000000000002132, 42.00000000000000000, 80.00402776293826435 ) ) ;
#64866 = ORIENTED_EDGE ( 'NONE', *, *, #55680, .F. ) ;
#64867 = MECHANICAL_DESIGN_GEOMETRIC_PRESENTATION_REPRESENTATION (  '', ( #62605 ), #34539 ) ;
#64868 = AXIS2_PLACEMENT_3D ( 'NONE', #16486, #4127, #37951 ) ;
#64869 = ADVANCED_FACE ( 'NONE', ( #57616 ), #4686, .T. ) ;
#64870 = CARTESIAN_POINT ( 'NONE',  ( -111.9549999999999841, -7.632228543268599452, 2.479861379858951054 ) ) ;
#64871 = EDGE_LOOP ( 'NONE', ( #50425, #18771 ) ) ;
#64872 = EDGE_CURVE ( 'NONE', #51146, #63065, #42687, .T. ) ;
#64873 = DIRECTION ( 'NONE',  ( 1.000000000000000000, 0.000000000000000000, 0.000000000000000000 ) ) ;
#64874 = DIRECTION ( 'NONE',  ( 0.000000000000000000, 0.000000000000000000, 1.000000000000000000 ) ) ;
#64875 = SURFACE_STYLE_USAGE ( .BOTH. , #457 ) ;
#64876 = CARTESIAN_POINT ( 'NONE',  ( -15.00000000000000000, 10.90871211463577239, 5.000000000000000888 ) ) ;
#64877 = CARTESIAN_POINT ( 'NONE',  ( -162.9570736234661865, 9.058813317711329915, -2.943386871421373119 ) ) ;
#64878 = CARTESIAN_POINT ( 'NONE',  ( -8.102448949553179958, 134.4949999999999477, 5.886773742842747126 ) ) ;
#64879 =( BOUNDED_CURVE ( )  B_SPLINE_CURVE ( 2, ( #35173, #55933, #45763, #17038, #56634, #7739, #8461, #35536, #27540, #51356, #12667 ),
 .UNSPECIFIED., .F., .F. ) 
 B_SPLINE_CURVE_WITH_KNOTS ( ( 3, 2, 2, 2, 2, 3 ),
 ( 0.4021739130434687226, 0.4043478260869469154, 0.4065217391304251082, 0.4086956521739034121, 0.4108695652173816049, 0.4130434782608597977 ),
 .UNSPECIFIED. ) 
 CURVE ( )  GEOMETRIC_REPRESENTATION_ITEM ( )  RATIONAL_B_SPLINE_CURVE ( ( 1.000000000000214939, 0.9510565162949385920, 1.000000000000000000, 0.9510565162951535312, 1.000000000000000000, 0.9510565162951535312, 1.000000000000000000, 0.9510565162951535312, 1.000000000000000000, 0.9510565162953734664, 0.9999999999997800648 ) ) 
 REPRESENTATION_ITEM ( '' )  );
#64880 = CARTESIAN_POINT ( 'NONE',  ( -91.55707362346616662, -1.166476076187852838E-15, -9.524999999999991473 ) ) ;
#64881 = ADVANCED_FACE ( 'NONE', ( #65657 ), #38627, .F. ) ;
#64882 = CARTESIAN_POINT ( 'NONE',  ( 0.000000000000000000, 114.4999999999999574, 23.00000000000000000 ) ) ;
#64883 = ORIENTED_EDGE ( 'NONE', *, *, #32756, .F. ) ;
#64884 = DIRECTION ( 'NONE',  ( -0.000000000000000000, -0.000000000000000000, -1.000000000000000000 ) ) ;
#64885 = VECTOR ( 'NONE', #48086, 1000.000000000000000 ) ;
#64886 = ADVANCED_FACE ( 'NONE', ( #64628 ), #60371, .T. ) ;
#64887 = FILL_AREA_STYLE_COLOUR ( '', #32431 ) ;
#64888 = DIRECTION ( 'NONE',  ( 0.000000000000000000, 1.000000000000000000, 0.000000000000000000 ) ) ;
#64889 = CIRCLE ( 'NONE', #41331, 14.49999999999999822 ) ;
#64890 = CARTESIAN_POINT ( 'NONE',  ( -134.7549999999999955, 4.716976649647091513, -6.492361379858946790 ) ) ;
#64891 = DIRECTION ( 'NONE',  ( 1.000000000000000000, 0.000000000000000000, 0.000000000000000000 ) ) ;
#64892 = CARTESIAN_POINT ( 'NONE',  ( -55.94292637653380496, 0.000000000000000000, 9.524999999999991473 ) ) ;
#64893 = CARTESIAN_POINT ( 'NONE',  ( -145.9449999999999932, -9.827790563157499189E-16, -8.024999999999991473 ) ) ;
#64894 = EDGE_CURVE ( 'NONE', #67044, #52223, #37879, .T. ) ;
#64895 = CARTESIAN_POINT ( 'NONE',  ( -136.0449999999999875, 7.632228543268600340, 2.479861379858949277 ) ) ;
#64896 = ORIENTED_EDGE ( 'NONE', *, *, #15074, .T. ) ;
#64897 = CARTESIAN_POINT ( 'NONE',  ( 44.75458990717763896, 9.918196635725919919, -3.527112199763385192 ) ) ;
#64898 =( NAMED_UNIT ( * ) SI_UNIT ( $, .STERADIAN. ) SOLID_ANGLE_UNIT ( ) );
#64899 =( NAMED_UNIT ( * ) PLANE_ANGLE_UNIT ( ) SI_UNIT ( $, .RADIAN. ) );
#64900 = UNCERTAINTY_MEASURE_WITH_UNIT (LENGTH_MEASURE( 1.000000000000000082E-05 ), #9615, 'distance_accuracy_value', 'NONE');
#64901 = EDGE_CURVE ( 'NONE', #67841, #10695, #2959, .T. ) ;
#64902 = CARTESIAN_POINT ( 'NONE',  ( -50.30499999999999261, 8.437984349512085203, -1.550032578732815448E-15 ) ) ;
#64903 = CARTESIAN_POINT ( 'NONE',  ( -59.24499999999999034, -4.716976649647093289, -6.492361379858945902 ) ) ;
#64904 = DIRECTION ( 'NONE',  ( 0.000000000000000000, 0.000000000000000000, -1.000000000000000000 ) ) ;
#64905 = SURFACE_STYLE_USAGE ( .BOTH. , #43520 ) ;
#64906 = FACE_OUTER_BOUND ( 'NONE', #42324, .T. ) ;
#64907 = CARTESIAN_POINT ( 'NONE',  ( -103.9429263765338050, 0.000000000000000000, 9.524999999999991473 ) ) ;
#64908 = DIRECTION ( 'NONE',  ( 1.132643588934172738E-16, -1.000000000000000000, -1.473213661637684397E-17 ) ) ;
#64909 = COLOUR_RGB ( '', 0.72549020, 0.75294118, 0.79215686) ;
#64910 = DIRECTION ( 'NONE',  ( -1.000000000000000000, 0.000000000000000000, 0.000000000000000000 ) ) ;
#64911 = COLOUR_RGB ( '', 0.66274510, 0.83137255, 0.94901961) ;
#64912 = TOROIDAL_SURFACE ( 'NONE', #61531, 0.5000000000000000000, 0.2500000000000000000 ) ;
#64913 =( NAMED_UNIT ( * ) SI_UNIT ( $, .STERADIAN. ) SOLID_ANGLE_UNIT ( ) );
#64914 = ORIENTED_EDGE ( 'NONE', *, *, #4513, .T. ) ;
#64915 = DIRECTION ( 'NONE',  ( 0.000000000000000000, -0.000000000000000000, 1.000000000000000000 ) ) ;
#64916 = SURFACE_STYLE_USAGE ( .BOTH. , #43531 ) ;
#64917 = ORIENTED_EDGE ( 'NONE', *, *, #63480, .F. ) ;
#64918 = DIRECTION ( 'NONE',  ( 0.000000000000000000, 0.000000000000000000, -1.000000000000000000 ) ) ;
#64919 = MECHANICAL_DESIGN_GEOMETRIC_PRESENTATION_REPRESENTATION (  '', ( #49233 ), #58171 ) ;
#64920 = CARTESIAN_POINT ( 'NONE',  ( -6.826472737025120807, 113.1070736234661638, 4.959722759717906548 ) ) ;
#64921 = CARTESIAN_POINT ( 'NONE',  ( 30.25000000000001066, 16.24999999999997513, -4.000000000000000000 ) ) ;
#64922 = FACE_BOUND ( 'NONE', #36567, .T. ) ;
#64923 = DIRECTION ( 'NONE',  ( 0.000000000000000000, -0.000000000000000000, 1.000000000000000000 ) ) ;
#64924 = ORIENTED_EDGE ( 'NONE', *, *, #50796, .T. ) ;
#64925 = ORIENTED_EDGE ( 'NONE', *, *, #11757, .T. ) ;
#64926 =( NAMED_UNIT ( * ) PLANE_ANGLE_UNIT ( ) SI_UNIT ( $, .RADIAN. ) );
#64927 = STYLED_ITEM ( 'NONE', ( #15350 ), #41399 ) ;
#64928 = FACE_OUTER_BOUND ( 'NONE', #26351, .T. ) ;
#64929 = CARTESIAN_POINT ( 'NONE',  ( -101.0929263765348622, 3.094860106636045938, 9.524999999987192822 ) ) ;
#64930 = ORIENTED_EDGE ( 'NONE', *, *, #31696, .T. ) ;
#64931 = CARTESIAN_POINT ( 'NONE',  ( 29.00000000000000000, 42.00000000000000000, -80.00402776293826435 ) ) ;
#64932 = DIRECTION ( 'NONE',  ( 0.000000000000000000, 0.000000000000000000, -1.000000000000000000 ) ) ;
#64933 = CARTESIAN_POINT ( 'NONE',  ( 0.000000000000000000, 149.9999999999999716, 0.000000000000000000 ) ) ;
#64934 = CARTESIAN_POINT ( 'NONE',  ( -93.59499999999997044, 2.607480562269073321, 8.024999999999991473 ) ) ;
#64935 = ORIENTED_EDGE ( 'NONE', *, *, #38499, .T. ) ;
#64936 = CARTESIAN_POINT ( 'NONE',  ( 8.035289517290014061, 153.2535762506718413, 2.032298507828633749 ) ) ;
#64937 = EDGE_CURVE ( 'NONE', #52223, #1044, #28339, .T. ) ;
#64938 = SURFACE_STYLE_USAGE ( .BOTH. , #44584 ) ;
#64939 = SURFACE_STYLE_FILL_AREA ( #5160 ) ;
#64940 = EDGE_LOOP ( 'NONE', ( #57469, #54131, #31103, #18829 ) ) ;
#64941 = CARTESIAN_POINT ( 'NONE',  ( 0.000000000000000000, 2.500000000000000000, 0.000000000000000000 ) ) ;
#64942 = CARTESIAN_POINT ( 'NONE',  ( 16.00000000000001776, 15.00000000000000000, -29.68999999999999417 ) ) ;
#64943 = ADVANCED_FACE ( 'NONE', ( #16475 ), #27651, .T. ) ;
#64944 = CARTESIAN_POINT ( 'NONE',  ( 57.00000000000000000, 14.00000000000000000, 60.00402776293825724 ) ) ;
#64945 = B_SPLINE_CURVE_WITH_KNOTS ( 'NONE', 3,
 ( #46774, #14013, #3762, #56921, #4462, #9092, #24537, #14715, #30870, #62532, #25932, #25581, #47098, #67833 ),
 .UNSPECIFIED., .F., .F.,
 ( 4, 2, 2, 2, 2, 2, 4 ),
 ( 0.000000000000000000, 0.002322248283345770738, 0.003483372425018657192, 0.004644496566691544079, 0.006966744850037316986, 0.008127868991710203439, 0.009288993133383091627 ),
 .UNSPECIFIED. ) ;
#64946 = ADVANCED_FACE ( 'NONE', ( #37939 ), #8607, .T. ) ;
#64947 = CARTESIAN_POINT ( 'NONE',  ( -10.11618306975752368, 54.14354156754873060, -6.790106699912857202 ) ) ;
#64948 = ORIENTED_EDGE ( 'NONE', *, *, #58829, .F. ) ;
#64949 = ORIENTED_EDGE ( 'NONE', *, *, #65212, .T. ) ;
#64950 = DIRECTION ( 'NONE',  ( -1.000000000000000000, 1.224646799147349509E-16, 0.000000000000000000 ) ) ;
#64951 = CARTESIAN_POINT ( 'NONE',  ( -184.0000000000000000, 0.000000000000000000, 5.499999999999985789 ) ) ;
#64952 = FILL_AREA_STYLE ('',( #59313 ) ) ;
#64953 = CARTESIAN_POINT ( 'NONE',  ( -195.0000000000000000, 0.000000000000000000, 9.524999999999991473 ) ) ;
#64954 = LINE ( 'NONE', #28700, #56603 ) ;
#64955 = AXIS2_PLACEMENT_3D ( 'NONE', #36188, #8730, #51642 ) ;
#64956 = CARTESIAN_POINT ( 'NONE',  ( -68.69292637653380496, 10.01517768586948698, -1.839758294383808966E-15 ) ) ;
#64957 = CARTESIAN_POINT ( 'NONE',  ( -6.240333192270997920, 153.8516573869858632, 6.318785644388177580 ) ) ;
#64958 = ORIENTED_EDGE ( 'NONE', *, *, #26144, .T. ) ;
#64959 = PRESENTATION_LAYER_ASSIGNMENT (  '', '', ( #3097 ) ) ;
#64960 = CARTESIAN_POINT ( 'NONE',  ( -161.3929263765338078, 8.102448949553176405, 5.886773742842740909 ) ) ;
#64961 = PRESENTATION_LAYER_ASSIGNMENT (  '', '', ( #39200 ) ) ;
#64962 = CARTESIAN_POINT ( 'NONE',  ( 44.00000000000000000, 18.99999999999998224, 4.000000000000000000 ) ) ;
#64963 = EDGE_CURVE ( 'NONE', #37864, #46687, #48839, .T. ) ;
#64964 = CARTESIAN_POINT ( 'NONE',  ( -149.6070736234661638, -8.102448949553174629, 5.886773742842742685 ) ) ;
#64965 = ORIENTED_EDGE ( 'NONE', *, *, #871, .F. ) ;
#64966 = SURFACE_SIDE_STYLE ('',( #43573 ) ) ;
#64967 = CARTESIAN_POINT ( 'NONE',  ( -172.8550000000000182, 4.716976649647094177, 6.492361379858945902 ) ) ;
#64968 = CARTESIAN_POINT ( 'NONE',  ( 17.00000000000000711, 27.99999999999998224, 3.750000000000000000 ) ) ;
#64969 = CARTESIAN_POINT ( 'NONE',  ( -171.5949999999999704, 2.607480562269073321, 8.024999999999991473 ) ) ;
#64970 = VECTOR ( 'NONE', #36039, 1000.000000000000000 ) ;
#64971 = CARTESIAN_POINT ( 'NONE',  ( -167.0949999999999704, -2.607480562269071545, -8.024999999999991473 ) ) ;
#64972 = VERTEX_POINT ( 'NONE', #28697 ) ;
#64973 = DIRECTION ( 'NONE',  ( -0.000000000000000000, 1.000000000000000000, -0.000000000000000000 ) ) ;
#64974 = DIRECTION ( 'NONE',  ( 0.000000000000000000, -0.000000000000000000, 1.000000000000000000 ) ) ;
#64975 = CARTESIAN_POINT ( 'NONE',  ( 51.99999999999998579, 1.797044900979284448E-15, 12.00000000000000000 ) ) ;
#64976 = CARTESIAN_POINT ( 'NONE',  ( -78.35499999999997556, -4.716976649647093289, -6.492361379858945902 ) ) ;
#64977 =( NAMED_UNIT ( * ) PLANE_ANGLE_UNIT ( ) SI_UNIT ( $, .RADIAN. ) );
#64978 = DIRECTION ( 'NONE',  ( 0.000000000000000000, 0.000000000000000000, 1.000000000000000000 ) ) ;
#64979 = CARTESIAN_POINT ( 'NONE',  ( -78.89499999999999602, 6.826472737025115478, 4.959722759717899443 ) ) ;
#64980 = CARTESIAN_POINT ( 'NONE',  ( -1.166476076187854022E-15, 133.0549999999999784, 9.525000000000000355 ) ) ;
#64981 = EDGE_CURVE ( 'NONE', #43795, #46607, #40685, .T. ) ;
#64982 = CARTESIAN_POINT ( 'NONE',  ( -10.39230484541327293, 3.469446951953614189E-15, 7.500000000000000000 ) ) ;
#64983 = DIRECTION ( 'NONE',  ( -0.7071067811865483499, 0.000000000000000000, -0.7071067811865466846 ) ) ;
#64984 = EDGE_CURVE ( 'NONE', #27282, #43138, #29937, .T. ) ;
#64985 = UNCERTAINTY_MEASURE_WITH_UNIT (LENGTH_MEASURE( 1.000000000000000082E-05 ), #6481, 'distance_accuracy_value', 'NONE');
#64986 = DIRECTION ( 'NONE',  ( 0.000000000000000000, 0.000000000000000000, 1.000000000000000000 ) ) ;
#64987 = ORIENTED_EDGE ( 'NONE', *, *, #33357, .F. ) ;
#64988 = AXIS2_PLACEMENT_3D ( 'NONE', #2011, #18276, #12277 ) ;
#64989 = CARTESIAN_POINT ( 'NONE',  ( -7.632228543268608334, 132.8429263765338249, 2.479861379858952830 ) ) ;
#64990 = DIRECTION ( 'NONE',  ( 0.000000000000000000, 0.000000000000000000, -1.000000000000000000 ) ) ;
#64991 = PRESENTATION_LAYER_ASSIGNMENT (  '', '', ( #54895 ) ) ;
#64992 = FILL_AREA_STYLE_COLOUR ( '', #68957 ) ;
#64993 = VERTEX_POINT ( 'NONE', #1912 ) ;
#64994 = CIRCLE ( 'NONE', #25688, 0.2500000000000002220 ) ;
#64995 = ORIENTED_EDGE ( 'NONE', *, *, #21273, .T. ) ;
#64996 = CARTESIAN_POINT ( 'NONE',  ( -8.437984349512095861, 135.6929263765338192, -5.166775262442723748E-16 ) ) ;
#64997 = CIRCLE ( 'NONE', #32457, 0.5000000000000004441 ) ;
#64998 = DIRECTION ( 'NONE',  ( 0.000000000000000000, -0.000000000000000000, -1.000000000000000000 ) ) ;
#64999 = AXIS2_PLACEMENT_3D ( 'NONE', #47048, #4407, #20974 ) ;
#65000 = FILL_AREA_STYLE ('',( #60083 ) ) ;
#65001 = STYLED_ITEM ( 'NONE', ( #16320 ), #66717 ) ;
#65002 = VERTEX_POINT ( 'NONE', #62099 ) ;
#65003 = CARTESIAN_POINT ( 'NONE',  ( -113.9049999999999727, 2.607480562269069324, -8.024999999999993250 ) ) ;
#65004 = ORIENTED_EDGE ( 'NONE', *, *, #69432, .F. ) ;
#65005 = DIRECTION ( 'NONE',  ( 0.000000000000000000, 0.000000000000000000, 1.000000000000000000 ) ) ;
#65006 = CARTESIAN_POINT ( 'NONE',  ( -71.49999999999998579, 64.07124727947029896, 10.00000000000000000 ) ) ;
#65007 = ORIENTED_EDGE ( 'NONE', *, *, #44296, .F. ) ;
#65008 = CARTESIAN_POINT ( 'NONE',  ( 54.50000000000002132, 1.797044900979284448E-15, -12.00000000000000000 ) ) ;
#65009 = CARTESIAN_POINT ( 'NONE',  ( -8.082903768654761123, -1.417096231345241097, -1.759977097422839922E-15 ) ) ;
#65010 = ORIENTED_EDGE ( 'NONE', *, *, #19167, .F. ) ;
#65011 = EDGE_CURVE ( 'NONE', #14417, #67683, #20957, .T. ) ;
#65012 = PRESENTATION_LAYER_ASSIGNMENT (  '', '', ( #11092 ) ) ;
#65013 = DIRECTION ( 'NONE',  ( 0.000000000000000000, 0.000000000000000000, 1.000000000000000000 ) ) ;
#65014 = CARTESIAN_POINT ( 'NONE',  ( 5.598654528085805993, 156.2450000000000045, 7.705886871421374629 ) ) ;
#65015 = CARTESIAN_POINT ( 'NONE',  ( 0.000000000000000000, 42.00000000000000000, -79.00402776293826435 ) ) ;
#65016 = ORIENTED_EDGE ( 'NONE', *, *, #33593, .T. ) ;
#65017 = VECTOR ( 'NONE', #28628, 1000.000000000000227 ) ;
#65018 = ORIENTED_EDGE ( 'NONE', *, *, #58221, .T. ) ;
#65019 = CARTESIAN_POINT ( 'NONE',  ( -118.2570736234661695, 5.598654528085800663, -7.705886871421367523 ) ) ;
#65020 = SURFACE_STYLE_FILL_AREA ( #39035 ) ;
#65021 = CARTESIAN_POINT ( 'NONE',  ( -181.0429263765338135, -9.058813317711329915, -2.943386871421370898 ) ) ;
#65022 = ORIENTED_EDGE ( 'NONE', *, *, #20724, .T. ) ;
#65023 = CARTESIAN_POINT ( 'NONE',  ( 0.000000000000000000, 131.9429263765338192, -8.025000000000000355 ) ) ;
#65024 = CARTESIAN_POINT ( 'NONE',  ( -54.73909730288738018, -9.103122581846379902, -2.000000000000000000 ) ) ;
#65025 = EDGE_CURVE ( 'NONE', #6283, #25093, #39298, .T. ) ;
#65026 = ORIENTED_EDGE ( 'NONE', *, *, #25095, .F. ) ;
#65027 = VERTEX_POINT ( 'NONE', #34344 ) ;
#65028 = SURFACE_STYLE_USAGE ( .BOTH. , #49578 ) ;
#65029 = CARTESIAN_POINT ( 'NONE',  ( -74.75000000000000000, -3.000000000000000000, 0.000000000000000000 ) ) ;
#65030 = CYLINDRICAL_SURFACE ( 'NONE', #8561, 26.99999999999999645 ) ;
#65031 = CARTESIAN_POINT ( 'NONE',  ( -139.4050000000000296, -2.607480562269069768, 8.024999999999991473 ) ) ;
#65032 = SURFACE_STYLE_USAGE ( .BOTH. , #43642 ) ;
#65033 = FILL_AREA_STYLE ('',( #64364 ) ) ;
#65034 = UNCERTAINTY_MEASURE_WITH_UNIT (LENGTH_MEASURE( 1.000000000000000082E-05 ), #58517, 'distance_accuracy_value', 'NONE');
#65035 = VERTEX_POINT ( 'NONE', #55793 ) ;
#65036 = AXIS2_PLACEMENT_3D ( 'NONE', #40439, #40109, #35142 ) ;
#65037 = DIRECTION ( 'NONE',  ( 1.982541115402069054E-16, 0.000000000000000000, 1.000000000000000000 ) ) ;
#65038 = PRESENTATION_STYLE_ASSIGNMENT (( #16560 ) ) ;
#65039 = CARTESIAN_POINT ( 'NONE',  ( 41.27334858134414475, 107.3315027881082528, 3.464507624621605331 ) ) ;
#65040 = ORIENTED_EDGE ( 'NONE', *, *, #26897, .F. ) ;
#65041 = ORIENTED_EDGE ( 'NONE', *, *, #26089, .T. ) ;
#65042 = DIRECTION ( 'NONE',  ( -1.000000000000000000, 0.000000000000000000, 0.000000000000000000 ) ) ;
#65043 = VECTOR ( 'NONE', #67062, 1000.000000000000000 ) ;
#65044 = EDGE_CURVE ( 'NONE', #61571, #4261, #67046, .T. ) ;
#65045 = LINE ( 'NONE', #1326, #33442 ) ;
#65046 = CARTESIAN_POINT ( 'NONE',  ( -57.80499999999998550, -8.437984349512085203, 5.166775262442717831E-16 ) ) ;
#65047 = ORIENTED_EDGE ( 'NONE', *, *, #63070, .F. ) ;
#65048 =( NAMED_UNIT ( * ) PLANE_ANGLE_UNIT ( ) SI_UNIT ( $, .RADIAN. ) );
#65049 = CARTESIAN_POINT ( 'NONE',  ( 45.00000000000000000, 10.69371294336137801, 10.00000000000000000 ) ) ;
#65050 = STYLED_ITEM ( 'NONE', ( #57115 ), #20646 ) ;
#65051 = VECTOR ( 'NONE', #20584, 1000.000000000000000 ) ;
#65052 = DIRECTION ( 'NONE',  ( 0.000000000000000000, 0.000000000000000000, -1.000000000000000000 ) ) ;
#65053 = CIRCLE ( 'NONE', #34716, 22.50000000000000000 ) ;
#65054 = LINE ( 'NONE', #48238, #8412 ) ;
#65055 = AXIS2_PLACEMENT_3D ( 'NONE', #45558, #50792, #60297 ) ;
#65056 = VERTEX_POINT ( 'NONE', #34671 ) ;
#65057 = DIRECTION ( 'NONE',  ( 1.000000000000000000, 0.000000000000000000, 0.000000000000000000 ) ) ;
#65058 = FACE_OUTER_BOUND ( 'NONE', #55884, .T. ) ;
#65059 =( NAMED_UNIT ( * ) PLANE_ANGLE_UNIT ( ) SI_UNIT ( $, .RADIAN. ) );
#65060 = CARTESIAN_POINT ( 'NONE',  ( 48.81081081081080697, 14.09971791521133255, 7.000000000000000000 ) ) ;
#65061 = VECTOR ( 'NONE', #21137, 1000.000000000000000 ) ;
#65062 = PLANE ( 'NONE',  #23606 ) ;
#65063 = CARTESIAN_POINT ( 'NONE',  ( -106.0449999999999875, 7.632228543268600340, 2.479861379858949277 ) ) ;
#65064 = CARTESIAN_POINT ( 'NONE',  ( 5.598654528085809545, 157.1449999999999818, -7.705886871421373741 ) ) ;
#65065 = CARTESIAN_POINT ( 'NONE',  ( -86.39499999999999602, -6.826472737025115478, -4.959722759717899443 ) ) ;
#65066 = VECTOR ( 'NONE', #13858, 1000.000000000000000 ) ;
#65067 = DIRECTION ( 'NONE',  ( 0.000000000000000000, 1.000000000000000000, 0.000000000000000000 ) ) ;
#65068 = CARTESIAN_POINT ( 'NONE',  ( 22.25000000000000711, 34.24999999999999289, 3.750000000000000000 ) ) ;
#65069 = UNCERTAINTY_MEASURE_WITH_UNIT (LENGTH_MEASURE( 1.000000000000000082E-05 ), #67715, 'distance_accuracy_value', 'NONE');
#65070 = AXIS2_PLACEMENT_3D ( 'NONE', #4229, #67600, #46894 ) ;
#65071 = ORIENTED_EDGE ( 'NONE', *, *, #28088, .F. ) ;
#65072 = CARTESIAN_POINT ( 'NONE',  ( -120.4429263765338050, -1.166476076187852838E-15, -9.524999999999991473 ) ) ;
#65073 = CARTESIAN_POINT ( 'NONE',  ( -143.2449999999999761, -4.716976649647093289, -6.492361379858945902 ) ) ;
#65074 = CARTESIAN_POINT ( 'NONE',  ( -7.511572993685801073E-16, 7.000000000000000888, 0.000000000000000000 ) ) ;
#65075 = AXIS2_PLACEMENT_3D ( 'NONE', #65940, #17769, #40977 ) ;
#65076 = SURFACE_STYLE_USAGE ( .BOTH. , #22188 ) ;
#65077 = SURFACE_SIDE_STYLE ('',( #11281 ) ) ;
#65078 = ORIENTED_EDGE ( 'NONE', *, *, #3034, .T. ) ;
#65079 = EDGE_LOOP ( 'NONE', ( #9192, #38691, #68799, #62696 ) ) ;
#65080 = DIRECTION ( 'NONE',  ( -0.000000000000000000, -0.000000000000000000, -1.000000000000000000 ) ) ;
#65081 = FACE_OUTER_BOUND ( 'NONE', #15439, .T. ) ;
#65082 = UNCERTAINTY_MEASURE_WITH_UNIT (LENGTH_MEASURE( 1.000000000000000082E-05 ), #3328, 'distance_accuracy_value', 'NONE');
#65083 = DIRECTION ( 'NONE',  ( 0.000000000000000000, 1.000000000000000000, 0.000000000000000000 ) ) ;
#65084 = SURFACE_SIDE_STYLE ('',( #59123 ) ) ;
#65085 = VECTOR ( 'NONE', #4676, 1000.000000000000000 ) ;
#65086 = DIRECTION ( 'NONE',  ( -0.000000000000000000, -1.000000000000000000, -0.000000000000000000 ) ) ;
#65087 = EDGE_LOOP ( 'NONE', ( #38483, #55363, #14083, #9256 ) ) ;
#65088 = CARTESIAN_POINT ( 'NONE',  ( -145.1049999999999898, -6.826472737025113702, 4.959722759717902107 ) ) ;
#65089 = ORIENTED_EDGE ( 'NONE', *, *, #21781, .F. ) ;
#65090 = ORIENTED_EDGE ( 'NONE', *, *, #36813, .T. ) ;
#65091 = CARTESIAN_POINT ( 'NONE',  ( 71.50000000000000000, 99.99999999999998579, -7.000000000000000000 ) ) ;
#65092 = CARTESIAN_POINT ( 'NONE',  ( 10.39230484541327115, -4.119968255444916849E-15, 7.500000000000000000 ) ) ;
#65093 = VERTEX_POINT ( 'NONE', #50532 ) ;
#65094 = EDGE_CURVE ( 'NONE', #28053, #14756, #2253, .T. ) ;
#65095 = AXIS2_PLACEMENT_3D ( 'NONE', #49985, #1723, #44041 ) ;
#65096 = FACE_BOUND ( 'NONE', #61536, .T. ) ;
#65097 = CARTESIAN_POINT ( 'NONE',  ( 3.000000000000030198, 38.70020753820971748, 90.00000000000000000 ) ) ;
#65098 = MECHANICAL_DESIGN_GEOMETRIC_PRESENTATION_REPRESENTATION (  '', ( #29077 ), #15681 ) ;
#65099 = CARTESIAN_POINT ( 'NONE',  ( -9.058813317711338797, 134.3449999999999989, 2.943386871421373563 ) ) ;
#65100 = STYLED_ITEM ( 'NONE', ( #37442 ), #4948 ) ;
#65101 = ADVANCED_FACE ( 'NONE', ( #66702 ), #18518, .F. ) ;
#65102 = ORIENTED_EDGE ( 'NONE', *, *, #7549, .F. ) ;
#65103 = EDGE_CURVE ( 'NONE', #408, #40021, #36810, .T. ) ;
#65104 = CARTESIAN_POINT ( 'NONE',  ( -95.60707362346614957, -8.102448949553174629, 5.886773742842742685 ) ) ;
#65105 = CARTESIAN_POINT ( 'NONE',  ( -8.102448949553179958, 132.6049999999999898, 5.886773742842747126 ) ) ;
#65106 = CARTESIAN_POINT ( 'NONE',  ( -57.05499999999999261, -9.827790563157499189E-16, -8.024999999999991473 ) ) ;
#65107 = CARTESIAN_POINT ( 'NONE',  ( -119.2449999999999903, -4.716976649647093289, -6.492361379858945902 ) ) ;
#65108 = CARTESIAN_POINT ( 'NONE',  ( -40.95866658621363854, 108.0312444614857128, -3.562488397568094989 ) ) ;
#65109 = ORIENTED_EDGE ( 'NONE', *, *, #22435, .T. ) ;
#65110 = CARTESIAN_POINT ( 'NONE',  ( 0.000000000000000000, 155.5550000000000068, -9.525000000000000355 ) ) ;
#65111 = DIRECTION ( 'NONE',  ( 0.000000000000000000, 0.000000000000000000, -1.000000000000000000 ) ) ;
#65112 = UNCERTAINTY_MEASURE_WITH_UNIT (LENGTH_MEASURE( 1.000000000000000082E-05 ), #59386, 'distance_accuracy_value', 'NONE');
#65113 = CIRCLE ( 'NONE', #48299, 17.50000000000000000 ) ;
#65114 = DIRECTION ( 'NONE',  ( 0.000000000000000000, 0.000000000000000000, -1.000000000000000000 ) ) ;
#65115 = ADVANCED_FACE ( 'NONE', ( #25173 ), #31127, .T. ) ;
#65116 = FACE_OUTER_BOUND ( 'NONE', #30612, .T. ) ;
#65117 = EDGE_CURVE ( 'NONE', #52614, #37693, #6378, .T. ) ;
#65118 = SURFACE_STYLE_FILL_AREA ( #54896 ) ;
#65119 = EDGE_LOOP ( 'NONE', ( #63898, #34352, #9294 ) ) ;
#65120 = AXIS2_PLACEMENT_3D ( 'NONE', #8514, #19742, #34879 ) ;
#65121 = SURFACE_STYLE_USAGE ( .BOTH. , #27127 ) ;
#65122 = DIRECTION ( 'NONE',  ( -0.000000000000000000, -0.000000000000000000, -1.000000000000000000 ) ) ;
#65123 = CARTESIAN_POINT ( 'NONE',  ( -174.9550000000000125, -7.632228543268599452, 2.479861379858951054 ) ) ;
#65125 = ORIENTED_EDGE ( 'NONE', *, *, #26488, .F. ) ;
#65124 = EDGE_CURVE ( 'NONE', #36781, #23235, #40115, .T. ) ;
#65126 =( LENGTH_UNIT ( ) NAMED_UNIT ( * ) SI_UNIT ( .MILLI., .METRE. ) );
#65127 = UNCERTAINTY_MEASURE_WITH_UNIT (LENGTH_MEASURE( 1.000000000000000082E-05 ), #45550, 'distance_accuracy_value', 'NONE');
#65128 = CIRCLE ( 'NONE', #68563, 0.2500000000000002220 ) ;
#65129 = SURFACE_STYLE_FILL_AREA ( #370 ) ;
#65130 = EDGE_CURVE ( 'NONE', #32643, #61826, #23322, .T. ) ;
#65131 = CARTESIAN_POINT ( 'NONE',  ( -65.00000000000000000, -1.962809905030629631E-14, -7.000000000000024869 ) ) ;
#65132 = SURFACE_STYLE_FILL_AREA ( #22234 ) ;
#65133 = CARTESIAN_POINT ( 'NONE',  ( -34.99999999999999289, 99.99999999999998579, -10.00000000000000000 ) ) ;
#65134 = ORIENTED_EDGE ( 'NONE', *, *, #50273, .F. ) ;
#65135 = COLOUR_RGB ( '', 0.31764706, 0.68627451, 0.89019608) ;
#65136 = CARTESIAN_POINT ( 'NONE',  ( -45.90208536020663388, 9.410173053538171573, -3.203892945547820226 ) ) ;
#65137 = CARTESIAN_POINT ( 'NONE',  ( -195.0000000000000000, 0.000000000000000000, 0.000000000000000000 ) ) ;
#65138 = CARTESIAN_POINT ( 'NONE',  ( -89.75499999999998124, 4.716976649647091513, -6.492361379858946790 ) ) ;
#65139 = VERTEX_POINT ( 'NONE', #9360 ) ;
#65140 = FILL_AREA_STYLE ('',( #49686 ) ) ;
#65141 = CARTESIAN_POINT ( 'NONE',  ( 4.683753779217428637, -2.005109422339667269, -5.887500484252663036 ) ) ;
#65142 = CIRCLE ( 'NONE', #12359, 4.999999999999997335 ) ;
#65143 = DIRECTION ( 'NONE',  ( -0.000000000000000000, -0.000000000000000000, -1.000000000000000000 ) ) ;
#65144 = DIRECTION ( 'NONE',  ( 0.000000000000000000, 0.000000000000000000, 1.000000000000000000 ) ) ;
#65145 = CARTESIAN_POINT ( 'NONE',  ( -66.50707362346615525, 8.102448949553176405, 5.886773742842740909 ) ) ;
#65146 = AXIS2_PLACEMENT_3D ( 'NONE', #65511, #29608, #34202 ) ;
#65147 = DIRECTION ( 'NONE',  ( -1.000000000000000000, 0.000000000000000000, 1.300977106640434891E-16 ) ) ;
#65148 = ORIENTED_EDGE ( 'NONE', *, *, #7402, .F. ) ;
#65149 = CARTESIAN_POINT ( 'NONE',  ( 0.7098900097155618205, 7.000000000000007105, -1.987393404142764886E-14 ) ) ;
#65150 = FACE_OUTER_BOUND ( 'NONE', #13307, .T. ) ;
#65151 = CARTESIAN_POINT ( 'NONE',  ( -99.65499999999998693, -7.632228543268600340, -2.479861379858950166 ) ) ;
#65152 = CARTESIAN_POINT ( 'NONE',  ( 0.000000000000000000, 133.4449999999999932, -9.525000000000000355 ) ) ;
#65153 = CARTESIAN_POINT ( 'NONE',  ( -118.9449999999999932, -9.827790563157499189E-16, -8.024999999999991473 ) ) ;
#65154 = AXIS2_PLACEMENT_3D ( 'NONE', #50155, #44894, #49798 ) ;
#65155 = AXIS2_PLACEMENT_3D ( 'NONE', #44357, #27410, #39067 ) ;
#65156 = CARTESIAN_POINT ( 'NONE',  ( 31.00000000000000355, 43.00000000000000000, -45.61250543006184444 ) ) ;
#65157 = CIRCLE ( 'NONE', #24671, 0.5000000000000004441 ) ;
#65159 = DIRECTION ( 'NONE',  ( 1.000000000000000000, 0.000000000000000000, -0.000000000000000000 ) ) ;
#65158 = CARTESIAN_POINT ( 'NONE',  ( 7.750000000000000000, 33.74999999999998579, -4.000000000000000000 ) ) ;
#65160 = PRESENTATION_LAYER_ASSIGNMENT (  '', '', ( #37148 ) ) ;
#65161 = CARTESIAN_POINT ( 'NONE',  ( -151.7929263765338135, -3.094860106618429807, 9.524999999999991473 ) ) ;
#65162 = CARTESIAN_POINT ( 'NONE',  ( -177.5950000000000273, 2.607480562269073321, 8.024999999999991473 ) ) ;
#65163 = STYLED_ITEM ( 'NONE', ( #38233 ), #52134 ) ;
#65164 = CARTESIAN_POINT ( 'NONE',  ( 0.000000000000000000, 148.0570736234661524, -8.025000000000000355 ) ) ;
#65165 =( GEOMETRIC_REPRESENTATION_CONTEXT ( 3 ) GLOBAL_UNCERTAINTY_ASSIGNED_CONTEXT ( ( #26330 ) ) GLOBAL_UNIT_ASSIGNED_CONTEXT ( ( #32350, #32020, #42297 ) ) REPRESENTATION_CONTEXT ( 'NONE', 'WORKASPACE' ) );
#65166 = VECTOR ( 'NONE', #54517, 1000.000000000000000 ) ;
#65167 = CARTESIAN_POINT ( 'NONE',  ( -46.35633800517990011, -13.76932876361770752, 2.685086742506573199 ) ) ;
#65168 = VERTEX_POINT ( 'NONE', #5099 ) ;
#65169 = DIRECTION ( 'NONE',  ( 1.000000000000000000, 0.000000000000000000, 0.000000000000000000 ) ) ;
#65170 = EDGE_LOOP ( 'NONE', ( #56934, #35785, #28259, #15238 ) ) ;
#65171 = CARTESIAN_POINT ( 'NONE',  ( -71.24292637653380211, 5.598654528085804216, 7.705886871421366635 ) ) ;
#65172 = COLOUR_RGB ( '', 0.66274510, 0.83137255, 0.94901961) ;
#65173 = CARTESIAN_POINT ( 'NONE',  ( -195.0000000000000000, 1.166476076187852838E-15, -9.524999999999991473 ) ) ;
#65174 = CARTESIAN_POINT ( 'NONE',  ( 44.25000000000000000, 21.74999999999998579, 3.750000000000000000 ) ) ;
#65175 = COLOUR_RGB ( '', 0.40784314, 0.44705882, 0.49803922) ;
#65176 = CARTESIAN_POINT ( 'NONE',  ( 35.99999999999999289, 5.000000000000000000, 32.00402776293825724 ) ) ;
#65177 = CARTESIAN_POINT ( 'NONE',  ( -142.7929263765343251, -3.094860106609758077, 9.525000000006292211 ) ) ;
#65178 = DIRECTION ( 'NONE',  ( 0.000000000000000000, -1.000000000000000000, 0.000000000000000000 ) ) ;
#65179 = MECHANICAL_DESIGN_GEOMETRIC_PRESENTATION_REPRESENTATION (  '', ( #15805 ), #64082 ) ;
#65180 = FILL_AREA_STYLE_COLOUR ( '', #55525 ) ;
#65181 = EDGE_LOOP ( 'NONE', ( #22036, #16537 ) ) ;
#65182 = CARTESIAN_POINT ( 'NONE',  ( -172.4050000000000011, -2.607480562269069768, 8.024999999999991473 ) ) ;
#65183 = EDGE_CURVE ( 'NONE', #17330, #23656, #31825, .T. ) ;
#65184 = EDGE_LOOP ( 'NONE', ( #57057, #68431, #28164 ) ) ;
#65185 = CARTESIAN_POINT ( 'NONE',  ( 8.250000000000001776, 30.99999999999998579, -3.750000000000000000 ) ) ;
#65186 = EDGE_CURVE ( 'NONE', #69284, #57165, #26204, .T. ) ;
#65187 = VECTOR ( 'NONE', #10132, 1000.000000000000000 ) ;
#65188 =( BOUNDED_CURVE ( )  B_SPLINE_CURVE ( 2, ( #30503, #31556, #15083, #69215, #53037, #47817, #52360, #21016, #62181, #56916, #8729 ),
 .UNSPECIFIED., .F., .F. ) 
 B_SPLINE_CURVE_WITH_KNOTS ( ( 3, 2, 2, 2, 2, 3 ),
 ( 0.3235294117647058987, 0.3294117647058823484, 0.3352941176470587981, 0.3411764705882353033, 0.3470588235294117530, 0.3529411764705882582 ),
 .UNSPECIFIED. ) 
 CURVE ( )  GEOMETRIC_REPRESENTATION_ITEM ( )  RATIONAL_B_SPLINE_CURVE ( ( 1.000000000000000000, 0.9510565162951535312, 1.000000000000000000, 0.9510565162951535312, 1.000000000000000000, 0.9510565162951535312, 1.000000000000000000, 0.9510565162951535312, 1.000000000000000000, 0.9510565162951535312, 1.000000000000000000 ) ) 
 REPRESENTATION_ITEM ( '' )  );
#65189 = CARTESIAN_POINT ( 'NONE',  ( -182.7570736234661979, -5.598654528085801552, 7.705886871421367523 ) ) ;
#65190 = CARTESIAN_POINT ( 'NONE',  ( -2.607480562269073765, 148.2070736234661581, -8.025000000000000355 ) ) ;
#65191 = EDGE_CURVE ( 'NONE', #3129, #2414, #21259, .T. ) ;
#65192 = VERTEX_POINT ( 'NONE', #57171 ) ;
#65193 = AXIS2_PLACEMENT_3D ( 'NONE', #6334, #66834, #40121 ) ;
#65194 =( LENGTH_UNIT ( ) NAMED_UNIT ( * ) SI_UNIT ( .MILLI., .METRE. ) );
#65195 = CIRCLE ( 'NONE', #31665, 0.2500000000000002220 ) ;
#65196 = CARTESIAN_POINT ( 'NONE',  ( -80.60499999999996135, 6.826472737025113702, -4.959722759717902107 ) ) ;
#65197 = UNCERTAINTY_MEASURE_WITH_UNIT (LENGTH_MEASURE( 1.000000000000000082E-05 ), #40667, 'distance_accuracy_value', 'NONE');
#65198 = CARTESIAN_POINT ( 'NONE',  ( 0.000000000000000000, 2.500000000000000000, 0.000000000000000000 ) ) ;
#65199 = FILL_AREA_STYLE_COLOUR ( '', #33261 ) ;
#65200 = CYLINDRICAL_SURFACE ( 'NONE', #26222, 0.5000000000000004441 ) ;
#65201 = AXIS2_PLACEMENT_3D ( 'NONE', #38511, #60254, #12748 ) ;
#65202 = EDGE_CURVE ( 'NONE', #18309, #11647, #5208, .T. ) ;
#65203 = MECHANICAL_DESIGN_GEOMETRIC_PRESENTATION_REPRESENTATION (  '', ( #36010 ), #40542 ) ;
#65204 = VERTEX_POINT ( 'NONE', #10401 ) ;
#65205 = FILL_AREA_STYLE ('',( #5751 ) ) ;
#65206 = CARTESIAN_POINT ( 'NONE',  ( -64.04499999999998749, 7.632228543268600340, 2.479861379858949277 ) ) ;
#65208 = ORIENTED_EDGE ( 'NONE', *, *, #33292, .T. ) ;
#65207 = MECHANICAL_DESIGN_GEOMETRIC_PRESENTATION_REPRESENTATION (  '', ( #61824 ), #57328 ) ;
#65209 = CARTESIAN_POINT ( 'NONE',  ( 9.250000000000003553, 0.000000000000000000, 4.000000000000000000 ) ) ;
#65210 = LINE ( 'NONE', #33886, #50322 ) ;
#65211 = CARTESIAN_POINT ( 'NONE',  ( -45.00000000000000000, 9.115532208874116193, -6.738970650128846884 ) ) ;
#65212 = EDGE_CURVE ( 'NONE', #65703, #50928, #53313, .T. ) ;
#65213 = ORIENTED_EDGE ( 'NONE', *, *, #3610, .F. ) ;
#65214 = DIRECTION ( 'NONE',  ( 0.000000000000000000, 0.000000000000000000, 1.000000000000000000 ) ) ;
#65215 = FILL_AREA_STYLE_COLOUR ( '', #11214 ) ;
#65216 =( GEOMETRIC_REPRESENTATION_CONTEXT ( 3 ) GLOBAL_UNCERTAINTY_ASSIGNED_CONTEXT ( ( #14467 ) ) GLOBAL_UNIT_ASSIGNED_CONTEXT ( ( #11371, #66209, #22272 ) ) REPRESENTATION_CONTEXT ( 'NONE', 'WORKASPACE' ) );
#65217 = ORIENTED_EDGE ( 'NONE', *, *, #6203, .F. ) ;
#65218 = CARTESIAN_POINT ( 'NONE',  ( 48.74999999999999289, 24.74999999999998579, -4.000000000000000000 ) ) ;
#65219 = DIRECTION ( 'NONE',  ( 0.000000000000000000, 0.000000000000000000, 1.000000000000000000 ) ) ;
#65220 = CARTESIAN_POINT ( 'NONE',  ( -118.2549999999999812, -4.716976649647092401, 6.492361379858946790 ) ) ;
#65221 = ORIENTED_EDGE ( 'NONE', *, *, #32139, .F. ) ;
#65222 = CARTESIAN_POINT ( 'NONE',  ( 0.000000000000000000, 149.9999999999999716, 0.000000000000000000 ) ) ;
#65223 = FACE_OUTER_BOUND ( 'NONE', #7856, .T. ) ;
#65224 =( GEOMETRIC_REPRESENTATION_CONTEXT ( 3 ) GLOBAL_UNCERTAINTY_ASSIGNED_CONTEXT ( ( #32057 ) ) GLOBAL_UNIT_ASSIGNED_CONTEXT ( ( #49599, #65419, #45389 ) ) REPRESENTATION_CONTEXT ( 'NONE', 'WORKASPACE' ) );
#65225 = DIRECTION ( 'NONE',  ( -0.000000000000000000, 1.000000000000000000, 0.000000000000000000 ) ) ;
#65226 = DIRECTION ( 'NONE',  ( 1.000000000000000000, 0.000000000000000000, 0.000000000000000000 ) ) ;
#65227 = PRESENTATION_STYLE_ASSIGNMENT (( #6826 ) ) ;
#65228 = CARTESIAN_POINT ( 'NONE',  ( -150.2070736234661581, 3.094860106618433360, 9.524999999999991473 ) ) ;
#65229 = CARTESIAN_POINT ( 'NONE',  ( -1.166476076187854022E-15, 134.9449999999999932, 9.525000000000000355 ) ) ;
#65230 = CARTESIAN_POINT ( 'NONE',  ( -94.40707362346618936, 3.094860106618428031, -9.524999999999993250 ) ) ;
#65231 = AXIS2_PLACEMENT_3D ( 'NONE', #42471, #37192, #32216 ) ;
#65232 = ORIENTED_EDGE ( 'NONE', *, *, #21342, .T. ) ;
#65233 = MECHANICAL_DESIGN_GEOMETRIC_PRESENTATION_REPRESENTATION (  '', ( #11315 ), #33803 ) ;
#65234 = SURFACE_SIDE_STYLE ('',( #6152 ) ) ;
#65235 = CARTESIAN_POINT ( 'NONE',  ( 68.99999999999998579, 36.75000000000000000, -3.000000000000000000 ) ) ;
#65236 = DIRECTION ( 'NONE',  ( 0.000000000000000000, 0.000000000000000000, -1.000000000000000000 ) ) ;
#65237 = CARTESIAN_POINT ( 'NONE',  ( -126.6549999999999869, -7.632228543268600340, -2.479861379858950166 ) ) ;
#65238 = CARTESIAN_POINT ( 'NONE',  ( -7.249999999999999112, 0.000000000000000000, 0.7500000000000000000 ) ) ;
#65239 = CARTESIAN_POINT ( 'NONE',  ( -146.8429263765338249, 9.058813317711329915, -2.943386871421373119 ) ) ;
#65240 = CARTESIAN_POINT ( 'NONE',  ( -55.64292637653381490, -5.598654528085801552, 7.705886871421367523 ) ) ;
#65241 = CARTESIAN_POINT ( 'NONE',  ( -146.5449999999999875, -7.632228543268600340, -2.479861379858950166 ) ) ;
#65242 = CARTESIAN_POINT ( 'NONE',  ( -129.5949999999999989, 2.607480562269072433, 8.024999999999991473 ) ) ;
#65243 =( GEOMETRIC_REPRESENTATION_CONTEXT ( 3 ) GLOBAL_UNCERTAINTY_ASSIGNED_CONTEXT ( ( #43352 ) ) GLOBAL_UNIT_ASSIGNED_CONTEXT ( ( #53743, #5899, #27342 ) ) REPRESENTATION_CONTEXT ( 'NONE', 'WORKASPACE' ) );
#65244 = ORIENTED_EDGE ( 'NONE', *, *, #14084, .F. ) ;
#65245 = DIRECTION ( 'NONE',  ( 0.000000000000000000, -1.000000000000000000, 0.000000000000000000 ) ) ;
#65246 = ADVANCED_FACE ( 'NONE', ( #59947 ), #32185, .F. ) ;
#65247 = CARTESIAN_POINT ( 'NONE',  ( 44.97648960591794776, 10.67803934730668658, -3.825005713026913057 ) ) ;
#65248 = FILL_AREA_STYLE ('',( #43840 ) ) ;
#65250 = CIRCLE ( 'NONE', #39483, 0.2500000000000002220 ) ;
#65249 =( NAMED_UNIT ( * ) SI_UNIT ( $, .STERADIAN. ) SOLID_ANGLE_UNIT ( ) );
#65251 = CARTESIAN_POINT ( 'NONE',  ( -184.4929263765337737, -8.102448949553172852, 5.886773742842742685 ) ) ;
#65252 = CARTESIAN_POINT ( 'NONE',  ( -56.99499999999999034, -6.826472737025115478, 4.959722759717900331 ) ) ;
#65253 = PRESENTATION_LAYER_ASSIGNMENT (  '', '', ( #7966 ) ) ;
#65254 = CARTESIAN_POINT ( 'NONE',  ( 6.999798566743344885, 8.428680263886673385E-16, 12.50000000000000000 ) ) ;
#65255 = DIRECTION ( 'NONE',  ( -1.000000000000000000, 0.000000000000000000, 0.000000000000000000 ) ) ;
#65256 = VECTOR ( 'NONE', #15230, 1000.000000000000000 ) ;
#65257 =( NAMED_UNIT ( * ) PLANE_ANGLE_UNIT ( ) SI_UNIT ( $, .RADIAN. ) );
#65258 = AXIS2_PLACEMENT_3D ( 'NONE', #38601, #38245, #44224 ) ;
#65259 = CARTESIAN_POINT ( 'NONE',  ( -107.2429263765338021, 5.598654528085804216, 7.705886871421366635 ) ) ;
#65260 = CARTESIAN_POINT ( 'NONE',  ( -0.7999999999998980149, 49.99999999999984368, -59.99999999999958789 ) ) ;
#65261 = DIRECTION ( 'NONE',  ( -0.000000000000000000, 1.000000000000000000, -0.000000000000000000 ) ) ;
#65262 = CARTESIAN_POINT ( 'NONE',  ( 60.00000000000000000, 1.797044900979284448E-15, -12.00000000000000000 ) ) ;
#65263 = CIRCLE ( 'NONE', #37194, 3.499999999999996003 ) ;
#65264 = CARTESIAN_POINT ( 'NONE',  ( 60.00000000000000000, 1.797044900979284448E-15, -10.49999999999999822 ) ) ;
#65265 = VECTOR ( 'NONE', #61785, 1000.000000000000000 ) ;
#65266 = EDGE_CURVE ( 'NONE', #10058, #28793, #53636, .T. ) ;
#65267 =( NAMED_UNIT ( * ) SI_UNIT ( $, .STERADIAN. ) SOLID_ANGLE_UNIT ( ) );
#65268 = EDGE_CURVE ( 'NONE', #19277, #23284, #16392, .T. ) ;
#65269 = ORIENTED_EDGE ( 'NONE', *, *, #40366, .F. ) ;
#65270 = COLOUR_RGB ( '', 0.66274510, 0.83137255, 0.94901961) ;
#65271 = LINE ( 'NONE', #66308, #56452 ) ;
#65272 = ORIENTED_EDGE ( 'NONE', *, *, #59722, .T. ) ;
#65273 = CARTESIAN_POINT ( 'NONE',  ( -20.71231517720798010, 149.9999999999999716, 10.00000000000000000 ) ) ;
#65274 = CIRCLE ( 'NONE', #36076, 0.5000000000000004441 ) ;
#65275 = CARTESIAN_POINT ( 'NONE',  ( 2.607480562269076430, 126.9070736234661467, -8.025000000000000355 ) ) ;
#65276 = CIRCLE ( 'NONE', #24740, 0.5000000000000004441 ) ;
#65277 = EDGE_CURVE ( 'NONE', #9929, #13814, #38192, .T. ) ;
#65278 = PLANE ( 'NONE',  #24827 ) ;
#65279 = COLOUR_RGB ( '', 0.31764706, 0.68627451, 0.89019608) ;
#65280 = DIRECTION ( 'NONE',  ( -1.000000000000000000, 0.000000000000000000, 0.000000000000000000 ) ) ;
#65281 = EDGE_CURVE ( 'NONE', #13722, #52924, #52506, .T. ) ;
#65282 = ORIENTED_EDGE ( 'NONE', *, *, #43574, .T. ) ;
#65283 = ORIENTED_EDGE ( 'NONE', *, *, #68232, .T. ) ;
#65284 = DIRECTION ( 'NONE',  ( -1.000000000000000000, 0.000000000000000000, 0.000000000000000000 ) ) ;
#65285 = SURFACE_STYLE_FILL_AREA ( #33287 ) ;
#65286 = EDGE_LOOP ( 'NONE', ( #59858, #17882, #44238, #44764, #52530, #43020 ) ) ;
#65287 = SURFACE_STYLE_USAGE ( .BOTH. , #21687 ) ;
#65288 = LINE ( 'NONE', #17805, #4117 ) ;
#65289 = EDGE_CURVE ( 'NONE', #41931, #42883, #60305, .T. ) ;
#65290 = AXIS2_PLACEMENT_3D ( 'NONE', #62652, #14852, #69348 ) ;
#65291 = CARTESIAN_POINT ( 'NONE',  ( 8.437984349512095861, 134.1929263765338192, 1.550032578732816828E-15 ) ) ;
#65292 = CARTESIAN_POINT ( 'NONE',  ( -89.99499999999999034, -6.826472737025115478, 4.959722759717900331 ) ) ;
#65293 = ORIENTED_EDGE ( 'NONE', *, *, #16562, .T. ) ;
#65294 =( BOUNDED_CURVE ( )  B_SPLINE_CURVE ( 2, ( #59331, #59017, #15444, #32982, #53057, #48502, #54417, #201, #54070, #25948, #42209 ),
 .UNSPECIFIED., .F., .F. ) 
 B_SPLINE_CURVE_WITH_KNOTS ( ( 3, 2, 2, 2, 2, 3 ),
 ( 0.2499999999999941158, 0.2521739130434723086, 0.2543478260869505014, 0.2565217391304288053, 0.2586956521739069981, 0.2608695652173851909 ),
 .UNSPECIFIED. ) 
 CURVE ( )  GEOMETRIC_REPRESENTATION_ITEM ( )  RATIONAL_B_SPLINE_CURVE ( ( 1.000000000000132561, 0.9510565162950210816, 1.000000000000000000, 0.9510565162951535312, 1.000000000000000000, 0.9510565162951535312, 1.000000000000000000, 0.9510565162951535312, 1.000000000000000000, 0.9510565162952909768, 0.9999999999998625544 ) ) 
 REPRESENTATION_ITEM ( '' )  );
#65295 = CARTESIAN_POINT ( 'NONE',  ( -20.20444455447386645, 114.9652390998742533, -10.39771284005833252 ) ) ;
#65296 = COLOUR_RGB ( '', 0.40784314, 0.44705882, 0.49803922) ;
#65297 = CARTESIAN_POINT ( 'NONE',  ( -23.71231517720798010, 117.9999999999999716, 7.500000000000000000 ) ) ;
#65298 = STYLED_ITEM ( 'NONE', ( #39670 ), #12629 ) ;
#65299 = DIRECTION ( 'NONE',  ( -1.224646799147353207E-16, 1.000000000000000000, 0.000000000000000000 ) ) ;
#65300 = ADVANCED_FACE ( 'NONE', ( #48758 ), #59595, .T. ) ;
#65301 = ORIENTED_EDGE ( 'NONE', *, *, #51669, .T. ) ;
#65302 = DIRECTION ( 'NONE',  ( -0.000000000000000000, -1.000000000000000000, -0.000000000000000000 ) ) ;
#65303 = CARTESIAN_POINT ( 'NONE',  ( 11.00000000000000000, 8.000000000000000000, 4.000000000000000000 ) ) ;
#65304 = VECTOR ( 'NONE', #30348, 1000.000000000000000 ) ;
#65305 = ORIENTED_EDGE ( 'NONE', *, *, #58138, .F. ) ;
#65306 =( GEOMETRIC_REPRESENTATION_CONTEXT ( 3 ) GLOBAL_UNCERTAINTY_ASSIGNED_CONTEXT ( ( #47712 ) ) GLOBAL_UNIT_ASSIGNED_CONTEXT ( ( #1639, #22111, #60081 ) ) REPRESENTATION_CONTEXT ( 'NONE', 'WORKASPACE' ) );
#65307 = PLANE ( 'NONE',  #12731 ) ;
#65308 = ORIENTED_EDGE ( 'NONE', *, *, #29870, .T. ) ;
#65309 = CARTESIAN_POINT ( 'NONE',  ( 17.75000000000000711, 30.74999999999999289, -4.000000000000000000 ) ) ;
#65310 = DIRECTION ( 'NONE',  ( 0.000000000000000000, -1.000000000000000000, 0.000000000000000000 ) ) ;
#65311 = CARTESIAN_POINT ( 'NONE',  ( 27.00000000000001776, 15.00000000000000000, -34.49999999999999289 ) ) ;
#65312 = DIRECTION ( 'NONE',  ( -1.000000000000000000, 0.000000000000000000, 0.000000000000000000 ) ) ;
#65313 = CARTESIAN_POINT ( 'NONE',  ( -176.3070736234661808, -10.01517768586948698, 6.132527647946031529E-16 ) ) ;
#65314 = CIRCLE ( 'NONE', #42874, 0.2500000000000002220 ) ;
#65315 = PRESENTATION_STYLE_ASSIGNMENT (( #66002 ) ) ;
#65316 = AXIS2_PLACEMENT_3D ( 'NONE', #56097, #55405, #18131 ) ;
#65317 = CARTESIAN_POINT ( 'NONE',  ( -4.559337023122181698, 153.1785496352698601, -6.825287955804306250 ) ) ;
#65318 = ORIENTED_EDGE ( 'NONE', *, *, #56539, .F. ) ;
#65319 = VECTOR ( 'NONE', #41336, 1000.000000000000000 ) ;
#65320 = CARTESIAN_POINT ( 'NONE',  ( -162.1429263765338362, 5.598654528085800663, -7.705886871421367523 ) ) ;
#65321 = CARTESIAN_POINT ( 'NONE',  ( 39.24999999999999289, 15.99999999999997691, -4.000000000000000000 ) ) ;
#65322 = PRESENTATION_STYLE_ASSIGNMENT (( #23118 ) ) ;
#65323 = FILL_AREA_STYLE_COLOUR ( '', #37725 ) ;
#65324 = ORIENTED_EDGE ( 'NONE', *, *, #45101, .T. ) ;
#65325 = DIRECTION ( 'NONE',  ( 0.000000000000000000, 0.000000000000000000, -1.000000000000000000 ) ) ;
#65326 = CARTESIAN_POINT ( 'NONE',  ( -158.1550000000000011, 7.632228543268600340, 2.479861379858949277 ) ) ;
#65327 = CARTESIAN_POINT ( 'NONE',  ( -183.4034255575450914, -1.261462791345238532, -9.055628821941482443 ) ) ;
#65328 = AXIS2_PLACEMENT_3D ( 'NONE', #23964, #40880, #67945 ) ;
#65329 = CARTESIAN_POINT ( 'NONE',  ( -172.0450000000000159, 7.632228543268600340, 2.479861379858949277 ) ) ;
#65330 = CARTESIAN_POINT ( 'NONE',  ( -161.2450000000000045, -4.716976649647093289, -6.492361379858945902 ) ) ;
#65331 = COLOUR_RGB ( '', 0.40784314, 0.44705882, 0.49803922) ;
#65332 = ORIENTED_EDGE ( 'NONE', *, *, #23406, .T. ) ;
#65333 = ADVANCED_FACE ( 'NONE', ( #54322 ), #65575, .T. ) ;
#65334 = CARTESIAN_POINT ( 'NONE',  ( -89.84292637653381064, 9.058813317711329915, -2.943386871421373119 ) ) ;
#65335 = AXIS2_PLACEMENT_3D ( 'NONE', #30165, #35816, #30871 ) ;
#65336 = LINE ( 'NONE', #35418, #68298 ) ;
#65337 = CARTESIAN_POINT ( 'NONE',  ( -69.35499999999998977, -4.716976649647093289, -6.492361379858945902 ) ) ;
#65338 = CARTESIAN_POINT ( 'NONE',  ( 24.29522375537286649, 27.12549504607582662, 27.31719062346842364 ) ) ;
#65339 = CARTESIAN_POINT ( 'NONE',  ( -85.64499999999998181, 4.716976649647091513, -6.492361379858946790 ) ) ;
#65340 = CARTESIAN_POINT ( 'NONE',  ( 0.000000000000000000, 140.5549999999999784, -9.525000000000000355 ) ) ;
#65341 = CARTESIAN_POINT ( 'NONE',  ( 30.25000000000001066, 16.24999999999997513, -4.000000000000000000 ) ) ;
#65342 = CIRCLE ( 'NONE', #29373, 0.5000000000000004441 ) ;
#65343 = CARTESIAN_POINT ( 'NONE',  ( 5.512442546757785777, 154.3838412429289804, 7.633710229762624699 ) ) ;
#65344 = DIRECTION ( 'NONE',  ( 1.000000000000000000, 0.000000000000000000, 0.000000000000000000 ) ) ;
#65345 = LINE ( 'NONE', #29433, #27059 ) ;
#65347 = ORIENTED_EDGE ( 'NONE', *, *, #354, .T. ) ;
#65346 = MECHANICAL_DESIGN_GEOMETRIC_PRESENTATION_REPRESENTATION (  '', ( #12505 ), #46265 ) ;
#65348 = EDGE_CURVE ( 'NONE', #33237, #18309, #19731, .T. ) ;
#65349 = VECTOR ( 'NONE', #34288, 1000.000000000000000 ) ;
#65350 = DIRECTION ( 'NONE',  ( -0.000000000000000000, -0.000000000000000000, -1.000000000000000000 ) ) ;
#65351 = CARTESIAN_POINT ( 'NONE',  ( -50.84292637653378932, 9.058813317711329915, -2.943386871421373119 ) ) ;
#65352 = VECTOR ( 'NONE', #41442, 1000.000000000000000 ) ;
#65353 = STYLED_ITEM ( 'NONE', ( #1060 ), #11966 ) ;
#65354 = ADVANCED_FACE ( 'NONE', ( #67946 ), #5264, .F. ) ;
#65355 = CYLINDRICAL_SURFACE ( 'NONE', #14718, 0.5000000000000004441 ) ;
#65356 = EDGE_CURVE ( 'NONE', #18512, #56203, #17661, .T. ) ;
#65357 = CARTESIAN_POINT ( 'NONE',  ( 45.00000000000000000, 9.639620389971918613, -6.999999999999999112 ) ) ;
#65358 = SURFACE_STYLE_FILL_AREA ( #48881 ) ;
#65359 = EDGE_LOOP ( 'NONE', ( #63545, #64546 ) ) ;
#65360 = ORIENTED_EDGE ( 'NONE', *, *, #6287, .F. ) ;
#65361 = DIRECTION ( 'NONE',  ( 1.000000000000000000, 0.000000000000000000, 0.000000000000000000 ) ) ;
#65362 = TOROIDAL_SURFACE ( 'NONE', #44082, 1.000000000000000000, 0.5000000000000000000 ) ;
#65363 = AXIS2_PLACEMENT_3D ( 'NONE', #68251, #34494, #16192 ) ;
#65364 =( REPRESENTATION_RELATIONSHIP ('NONE','NONE', #5102, #60355 ) REPRESENTATION_RELATIONSHIP_WITH_TRANSFORMATION ( #26154 )SHAPE_REPRESENTATION_RELATIONSHIP( ) );
#65365 = EDGE_CURVE ( 'NONE', #9536, #56195, #13148, .T. ) ;
#65366 = CARTESIAN_POINT ( 'NONE',  ( 71.50000000000000000, 14.49137674618942562, -9.500000000000000000 ) ) ;
#65367 = FILL_AREA_STYLE_COLOUR ( '', #40543 ) ;
#65368 = CIRCLE ( 'NONE', #40545, 10.99999999999995381 ) ;
#65369 = CARTESIAN_POINT ( 'NONE',  ( -69.65707362346616094, 9.058813317711329915, 2.943386871421369566 ) ) ;
#65370 = EDGE_CURVE ( 'NONE', #11547, #69397, #3148, .T. ) ;
#65371 = EDGE_LOOP ( 'NONE', ( #51805, #27912, #12322 ) ) ;
#65372 = CARTESIAN_POINT ( 'NONE',  ( -111.2049999999999841, -2.607480562269071545, -8.024999999999991473 ) ) ;
#65373 = ORIENTED_EDGE ( 'NONE', *, *, #30032, .T. ) ;
#65374 = CYLINDRICAL_SURFACE ( 'NONE', #50052, 0.5000000000000000000 ) ;
#65375 = AXIS2_PLACEMENT_3D ( 'NONE', #50797, #24726, #12442 ) ;
#65376 = ORIENTED_EDGE ( 'NONE', *, *, #34252, .T. ) ;
#65377 = CARTESIAN_POINT ( 'NONE',  ( -68.00707362346616947, -8.102448949553174629, -5.886773742842741797 ) ) ;
#65378 = ORIENTED_EDGE ( 'NONE', *, *, #47865, .F. ) ;
#65379 = DIRECTION ( 'NONE',  ( 0.000000000000000000, -0.000000000000000000, -1.000000000000000000 ) ) ;
#65380 = CARTESIAN_POINT ( 'NONE',  ( 3.094860106618431583, 156.0949999999999989, 9.525000000000000355 ) ) ;
#65381 = LINE ( 'NONE', #55513, #41959 ) ;
#65382 = EDGE_LOOP ( 'NONE', ( #51359, #61290, #35356, #68614 ) ) ;
#65383 = ORIENTED_EDGE ( 'NONE', *, *, #59182, .F. ) ;
#65384 =( GEOMETRIC_REPRESENTATION_CONTEXT ( 3 ) GLOBAL_UNCERTAINTY_ASSIGNED_CONTEXT ( ( #32853 ) ) GLOBAL_UNIT_ASSIGNED_CONTEXT ( ( #15428, #5767, #43489 ) ) REPRESENTATION_CONTEXT ( 'NONE', 'WORKASPACE' ) );
#65385 = DIRECTION ( 'NONE',  ( 0.000000000000000000, 0.000000000000000000, 1.000000000000000000 ) ) ;
#65386 = DIRECTION ( 'NONE',  ( 0.000000000000000000, 0.000000000000000000, 1.000000000000000000 ) ) ;
#65387 = SURFACE_SIDE_STYLE ('',( #22830 ) ) ;
#65388 = CARTESIAN_POINT ( 'NONE',  ( -67.99999999999998579, -2.024042244987997205E-14, -10.49999999999999822 ) ) ;
#65389 = ORIENTED_EDGE ( 'NONE', *, *, #40209, .F. ) ;
#65390 = CARTESIAN_POINT ( 'NONE',  ( 6.826472737025121695, 137.4929263765338305, -4.959722759717905660 ) ) ;
#65391 = DIRECTION ( 'NONE',  ( 0.000000000000000000, 0.000000000000000000, -1.000000000000000000 ) ) ;
#65392 =( GEOMETRIC_REPRESENTATION_CONTEXT ( 3 ) GLOBAL_UNCERTAINTY_ASSIGNED_CONTEXT ( ( #11737 ) ) GLOBAL_UNIT_ASSIGNED_CONTEXT ( ( #10034, #4734, #41718 ) ) REPRESENTATION_CONTEXT ( 'NONE', 'WORKASPACE' ) );
#65393 = CARTESIAN_POINT ( 'NONE',  ( -57.05707362346618083, 0.000000000000000000, 9.524999999999991473 ) ) ;
#65394 = ADVANCED_FACE ( 'NONE', ( #41562 ), #19014, .F. ) ;
#65395 = VERTEX_POINT ( 'NONE', #13764 ) ;
#65396 = FACE_OUTER_BOUND ( 'NONE', #52500, .T. ) ;
#65397 = EDGE_LOOP ( 'NONE', ( #52359, #22483, #34073, #65208 ) ) ;
#65398 = CARTESIAN_POINT ( 'NONE',  ( -51.14292637653380780, 5.598654528085800663, -7.705886871421367523 ) ) ;
#65399 = FACE_OUTER_BOUND ( 'NONE', #2852, .T. ) ;
#65400 = DIRECTION ( 'NONE',  ( -0.000000000000000000, 1.000000000000000000, 0.000000000000000000 ) ) ;
#65401 = LINE ( 'NONE', #7357, #6327 ) ;
#65402 = CARTESIAN_POINT ( 'NONE',  ( -144.5049999999999670, -6.826472737025115478, -4.959722759717899443 ) ) ;
#65403 = EDGE_CURVE ( 'NONE', #67895, #51506, #29013, .T. ) ;
#65404 = FACE_OUTER_BOUND ( 'NONE', #37143, .T. ) ;
#65405 = ORIENTED_EDGE ( 'NONE', *, *, #61128, .T. ) ;
#65406 = AXIS2_PLACEMENT_3D ( 'NONE', #60520, #17328, #10973 ) ;
#65407 = AXIS2_PLACEMENT_3D ( 'NONE', #7719, #38408, #7033 ) ;
#65408 = CARTESIAN_POINT ( 'NONE',  ( -106.3429263765338106, -9.058813317711329915, 2.943386871421371787 ) ) ;
#65409 = CARTESIAN_POINT ( 'NONE',  ( -107.0070736234661695, -8.102448949553174629, -5.886773742842741797 ) ) ;
#65410 = FACE_OUTER_BOUND ( 'NONE', #28706, .T. ) ;
#65411 = VERTEX_POINT ( 'NONE', #48232 ) ;
#65412 = CIRCLE ( 'NONE', #46364, 0.5000000000000004441 ) ;
#65413 = ORIENTED_EDGE ( 'NONE', *, *, #267, .T. ) ;
#65414 = CARTESIAN_POINT ( 'NONE',  ( -45.91046261216711599, 9.422709103004114795, 3.407326739365095225 ) ) ;
#65415 = CARTESIAN_POINT ( 'NONE',  ( -109.6429263765338078, -5.598654528085801552, 7.705886871421367523 ) ) ;
#65416 = CARTESIAN_POINT ( 'NONE',  ( -52.25499999999999545, -4.716976649647092401, 6.492361379858946790 ) ) ;
#65417 = VERTEX_POINT ( 'NONE', #63337 ) ;
#65418 = LINE ( 'NONE', #48938, #3349 ) ;
#65419 =( NAMED_UNIT ( * ) PLANE_ANGLE_UNIT ( ) SI_UNIT ( $, .RADIAN. ) );
#65420 = CARTESIAN_POINT ( 'NONE',  ( -29.82215890055010377, -8.499999999999996447, 0.3549037236123264716 ) ) ;
#65421 =( GEOMETRIC_REPRESENTATION_CONTEXT ( 3 ) GLOBAL_UNCERTAINTY_ASSIGNED_CONTEXT ( ( #20922 ) ) GLOBAL_UNIT_ASSIGNED_CONTEXT ( ( #37755, #4633, #43028 ) ) REPRESENTATION_CONTEXT ( 'NONE', 'WORKASPACE' ) );
#65422 = FACE_OUTER_BOUND ( 'NONE', #62515, .T. ) ;
#65423 = DIRECTION ( 'NONE',  ( -1.000000000000000000, 0.000000000000000000, 0.000000000000000000 ) ) ;
#65424 = ORIENTED_EDGE ( 'NONE', *, *, #42098, .F. ) ;
#65425 = CIRCLE ( 'NONE', #4753, 0.2500000000000002220 ) ;
#65426 = PRESENTATION_STYLE_ASSIGNMENT (( #27752 ) ) ;
#65427 = CARTESIAN_POINT ( 'NONE',  ( 1.000000000000000000, -60.04052944165106709, 35.50000000000000000 ) ) ;
#65428 = FACE_OUTER_BOUND ( 'NONE', #40407, .T. ) ;
#65429 = DIRECTION ( 'NONE',  ( 0.000000000000000000, -1.000000000000000000, 0.000000000000000000 ) ) ;
#65430 = CARTESIAN_POINT ( 'NONE',  ( -105.1449999999999818, -4.716976649647092401, 6.492361379858946790 ) ) ;
#65431 = CARTESIAN_POINT ( 'NONE',  ( 10.01517768586949231, 153.6949999999999932, 1.839758294383810543E-15 ) ) ;
#65432 = CARTESIAN_POINT ( 'NONE',  ( -80.69499999999999318, -8.437984349512085203, 5.166775262442717831E-16 ) ) ;
#65433 = VECTOR ( 'NONE', #19188, 1000.000000000000000 ) ;
#65434 = EDGE_CURVE ( 'NONE', #5399, #21155, #53584, .T. ) ;
#65435 = PRESENTATION_STYLE_ASSIGNMENT (( #44380 ) ) ;
#65436 = DIRECTION ( 'NONE',  ( -1.000000000000000000, 0.000000000000000000, 0.000000000000000000 ) ) ;
#65437 = CARTESIAN_POINT ( 'NONE',  ( 9.827790563157511022E-16, 87.30187232391182306, -8.025000000000000355 ) ) ;
#65438 = EDGE_LOOP ( 'NONE', ( #30661, #52464, #11409, #48561 ) ) ;
#65439 = EDGE_CURVE ( 'NONE', #18810, #39701, #32233, .T. ) ;
#65440 = CARTESIAN_POINT ( 'NONE',  ( -125.0929263765337964, 3.094860106618433360, 9.524999999999991473 ) ) ;
#65441 = PRESENTATION_STYLE_ASSIGNMENT (( #43360 ) ) ;
#65442 = CARTESIAN_POINT ( 'NONE',  ( -144.5950000000000273, 2.607480562269073321, 8.024999999999991473 ) ) ;
#65443 = PRESENTATION_STYLE_ASSIGNMENT (( #39785 ) ) ;
#65444 = AXIS2_PLACEMENT_3D ( 'NONE', #32419, #53883, #54580 ) ;
#65445 = EDGE_CURVE ( 'NONE', #57229, #54767, #4577, .T. ) ;
#65446 = CARTESIAN_POINT ( 'NONE',  ( -47.39499999999998892, -6.826472737025113702, -4.959722759717900331 ) ) ;
#65447 = PRESENTATION_STYLE_ASSIGNMENT (( #16259 ) ) ;
#65448 = VERTEX_POINT ( 'NONE', #42971 ) ;
#65449 = ORIENTED_EDGE ( 'NONE', *, *, #16490, .F. ) ;
#65450 = CIRCLE ( 'NONE', #248, 3.599999999999992095 ) ;
#65451 = DIRECTION ( 'NONE',  ( 0.000000000000000000, -1.000000000000000000, 0.000000000000000000 ) ) ;
#65452 = AXIS2_PLACEMENT_3D ( 'NONE', #31284, #58734, #53461 ) ;
#65453 = PLANE ( 'NONE',  #38404 ) ;
#65454 = TOROIDAL_SURFACE ( 'NONE', #50846, 2.000000000000000000, 1.000000000000000000 ) ;
#65455 = CARTESIAN_POINT ( 'NONE',  ( -49.55707362346617373, -1.166476076187852838E-15, -9.524999999999991473 ) ) ;
#65456 = EDGE_CURVE ( 'NONE', #28382, #47284, #36804, .T. ) ;
#65457 = ORIENTED_EDGE ( 'NONE', *, *, #63462, .F. ) ;
#65458 = CARTESIAN_POINT ( 'NONE',  ( -143.6049999999999613, 6.826472737025113702, -4.959722759717902107 ) ) ;
#65459 = VERTEX_POINT ( 'NONE', #15866 ) ;
#65460 = ORIENTED_EDGE ( 'NONE', *, *, #46976, .T. ) ;
#65461 = CARTESIAN_POINT ( 'NONE',  ( 55.39999999999999147, 11.99999999999999822, 4.000000000000000000 ) ) ;
#65462 = ORIENTED_EDGE ( 'NONE', *, *, #34317, .T. ) ;
#65463 = PRODUCT_DEFINITION_SHAPE ( 'NONE', 'NONE',  #69712 ) ;
#65464 = CARTESIAN_POINT ( 'NONE',  ( -55.95931559381303089, -8.622190103400207306, -1.508108381079090510 ) ) ;
#65465 = CARTESIAN_POINT ( 'NONE',  ( 5.598654528085805993, 126.2449999999999903, 7.705886871421374629 ) ) ;
#65466 = AXIS2_PLACEMENT_3D ( 'NONE', #37769, #10299, #5675 ) ;
#65467 = VERTEX_POINT ( 'NONE', #16222 ) ;
#65468 = FACE_OUTER_BOUND ( 'NONE', #19855, .T. ) ;
#65469 = CARTESIAN_POINT ( 'NONE',  ( -8.102448949553179958, 135.0050000000000239, -5.886773742842749790 ) ) ;
#65470 = CARTESIAN_POINT ( 'NONE',  ( -50.30499999999998550, 8.437984349512086979, -1.550032578732815448E-15 ) ) ;
#65471 = CARTESIAN_POINT ( 'NONE',  ( 40.95793942982998459, 108.0317815798972418, -3.561444987364487780 ) ) ;
#65472 = ORIENTED_EDGE ( 'NONE', *, *, #50537, .T. ) ;
#65473 = CARTESIAN_POINT ( 'NONE',  ( -9.058813317711338797, 156.4549999999999841, 2.943386871421373563 ) ) ;
#65474 = DIRECTION ( 'NONE',  ( 1.000000000000000000, 0.000000000000000000, 0.000000000000000000 ) ) ;
#65475 = SURFACE_STYLE_FILL_AREA ( #44072 ) ;
#65476 =( GEOMETRIC_REPRESENTATION_CONTEXT ( 3 ) GLOBAL_UNCERTAINTY_ASSIGNED_CONTEXT ( ( #31296 ) ) GLOBAL_UNIT_ASSIGNED_CONTEXT ( ( #54723, #55072, #11483 ) ) REPRESENTATION_CONTEXT ( 'NONE', 'WORKASPACE' ) );
#65477 = TOROIDAL_SURFACE ( 'NONE', #26147, 7.249999999999999112, 0.2500000000000000000 ) ;
#65478 = VECTOR ( 'NONE', #31485, 1000.000000000000000 ) ;
#65479 = ORIENTED_EDGE ( 'NONE', *, *, #7402, .T. ) ;
#65480 = CARTESIAN_POINT ( 'NONE',  ( -15.00000000000000000, -12.00000000000000000, 0.000000000000000000 ) ) ;
#65481 = EDGE_LOOP ( 'NONE', ( #29498, #2038, #12149, #10209 ) ) ;
#65482 = CARTESIAN_POINT ( 'NONE',  ( -10.74999999999999645, -0.9999999999999995559, 7.000000000000001776 ) ) ;
#65483 = CARTESIAN_POINT ( 'NONE',  ( -167.4549999999999841, 7.632228543268599452, -2.479861379858951942 ) ) ;
#65484 = VERTEX_POINT ( 'NONE', #15192 ) ;
#65485 = CARTESIAN_POINT ( 'NONE',  ( 22.99999999999998224, 5.000000000000000000, 72.00402776293825013 ) ) ;
#65486 =( GEOMETRIC_REPRESENTATION_CONTEXT ( 3 ) GLOBAL_UNCERTAINTY_ASSIGNED_CONTEXT ( ( #66596 ) ) GLOBAL_UNIT_ASSIGNED_CONTEXT ( ( #28087, #12266, #29506 ) ) REPRESENTATION_CONTEXT ( 'NONE', 'WORKASPACE' ) );
#65487 =( LENGTH_UNIT ( ) NAMED_UNIT ( * ) SI_UNIT ( .MILLI., .METRE. ) );
#65488 = FACE_OUTER_BOUND ( 'NONE', #31352, .T. ) ;
#65489 = DIRECTION ( 'NONE',  ( 0.000000000000000000, 0.000000000000000000, -1.000000000000000000 ) ) ;
#65490 = VERTEX_POINT ( 'NONE', #53484 ) ;
#65491 = SURFACE_STYLE_FILL_AREA ( #64801 ) ;
#65492 = DIRECTION ( 'NONE',  ( -0.000000000000000000, -0.000000000000000000, -1.000000000000000000 ) ) ;
#65493 = CARTESIAN_POINT ( 'NONE',  ( -83.75499999999998124, 4.716976649647091513, -6.492361379858946790 ) ) ;
#65494 = ORIENTED_EDGE ( 'NONE', *, *, #44390, .T. ) ;
#65495 = CARTESIAN_POINT ( 'NONE',  ( 1.000000000000000000, 1.000000000000000222, -3.000000000000000000 ) ) ;
#65496 = AXIS2_PLACEMENT_3D ( 'NONE', #9796, #41827, #58650 ) ;
#65497 = CIRCLE ( 'NONE', #35168, 1.000000000000000000 ) ;
#65498 = CARTESIAN_POINT ( 'NONE',  ( 0.000000000000000000, 145.0570736234661524, -8.025000000000000355 ) ) ;
#65499 = DIRECTION ( 'NONE',  ( 0.000000000000000000, 1.000000000000000000, 0.000000000000000000 ) ) ;
#65500 = CARTESIAN_POINT ( 'NONE',  ( -53.00707362346619078, -8.102448949553172852, -5.886773742842741797 ) ) ;
#65501 =( GEOMETRIC_REPRESENTATION_CONTEXT ( 3 ) GLOBAL_UNCERTAINTY_ASSIGNED_CONTEXT ( ( #32533 ) ) GLOBAL_UNIT_ASSIGNED_CONTEXT ( ( #2335, #66067, #44673 ) ) REPRESENTATION_CONTEXT ( 'NONE', 'WORKASPACE' ) );
#65502 = CARTESIAN_POINT ( 'NONE',  ( -75.00000000000000000, 7.952411872162292283, -6.456960098911577184 ) ) ;
#65503 = VERTEX_POINT ( 'NONE', #54150 ) ;
#65504 = CARTESIAN_POINT ( 'NONE',  ( 3.728548500389067488, 7.000000000000006217, 0.9264520766856050304 ) ) ;
#65505 = DIRECTION ( 'NONE',  ( 0.000000000000000000, 1.000000000000000000, 0.000000000000000000 ) ) ;
#65506 = CARTESIAN_POINT ( 'NONE',  ( -3.094860106618434248, 128.7949999999999875, 9.525000000000000355 ) ) ;
#65507 = MECHANICAL_DESIGN_GEOMETRIC_PRESENTATION_REPRESENTATION (  '', ( #55365 ), #58738 ) ;
#65508 = CARTESIAN_POINT ( 'NONE',  ( -119.2449999999999903, -4.716976649647093289, -6.492361379858945902 ) ) ;
#65509 = ADVANCED_FACE ( 'NONE', ( #10911 ), #27407, .T. ) ;
#65510 = AXIS2_PLACEMENT_3D ( 'NONE', #53791, #48923, #622 ) ;
#65511 = CARTESIAN_POINT ( 'NONE',  ( 34.99999999999992895, 112.4999999999999858, 9.500000000000000000 ) ) ;
#65512 = MECHANICAL_DESIGN_GEOMETRIC_PRESENTATION_REPRESENTATION (  '', ( #22850 ), #2549 ) ;
#65514 = CARTESIAN_POINT ( 'NONE',  ( -17.22054250019079902, 11.13153480011775365, -4.482835375932292976 ) ) ;
#65513 = LINE ( 'NONE', #28188, #59282 ) ;
#65515 = CARTESIAN_POINT ( 'NONE',  ( -150.8929263765337794, -8.102448949553172852, -5.886773742842741797 ) ) ;
#65516 = TOROIDAL_SURFACE ( 'NONE', #4859, 1.000000000000000000, 0.5000000000000000000 ) ;
#65517 = SHAPE_REPRESENTATION_RELATIONSHIP ( 'NONE' , 'NONE' ,  #31597, #53933 ) ;
#65518 = CARTESIAN_POINT ( 'NONE',  ( -176.0949999999999704, -2.607480562269071545, -8.024999999999991473 ) ) ;
#65519 = COLOUR_RGB ( '', 0.72549020, 0.75294118, 0.79215686) ;
#65520 = MECHANICAL_DESIGN_GEOMETRIC_PRESENTATION_REPRESENTATION (  '', ( #5965 ), #16148 ) ;
#65521 = EDGE_CURVE ( 'NONE', #26743, #60935, #16565, .T. ) ;
#65522 = CARTESIAN_POINT ( 'NONE',  ( 0.000000000000000000, 149.9999999999999716, 0.000000000000000000 ) ) ;
#65523 = ADVANCED_FACE ( 'NONE', ( #59414 ), #37347, .T. ) ;
#65524 = CARTESIAN_POINT ( 'NONE',  ( -40.19857555756881595, -13.54303449714841889, 2.705192303963717126 ) ) ;
#65525 = VERTEX_POINT ( 'NONE', #36992 ) ;
#65526 = SURFACE_SIDE_STYLE ('',( #32827 ) ) ;
#65527 = VERTEX_POINT ( 'NONE', #20785 ) ;
#65528 = EDGE_CURVE ( 'NONE', #3314, #4855, #52559, .T. ) ;
#65529 = CARTESIAN_POINT ( 'NONE',  ( -69.44292637653380496, -1.166476076187852838E-15, -9.524999999999991473 ) ) ;
#65530 = CARTESIAN_POINT ( 'NONE',  ( 22.25000000000000711, 33.74999999999999289, 4.000000000000000000 ) ) ;
#65531 = STYLED_ITEM ( 'NONE', ( #35490 ), #26459 ) ;
#65532 = EDGE_CURVE ( 'NONE', #22472, #18963, #68258, .T. ) ;
#65533 = DIRECTION ( 'NONE',  ( 0.000000000000000000, 1.000000000000000000, 0.000000000000000000 ) ) ;
#65534 = DIRECTION ( 'NONE',  ( 0.000000000000000000, 0.000000000000000000, 1.000000000000000000 ) ) ;
#65535 = DIRECTION ( 'NONE',  ( 0.000000000000000000, 0.000000000000000000, 1.000000000000000000 ) ) ;
#65536 = EDGE_CURVE ( 'NONE', #19085, #59074, #55432, .T. ) ;
#65537 = EDGE_LOOP ( 'NONE', ( #36627, #13761, #39496, #12435 ) ) ;
#65538 = CARTESIAN_POINT ( 'NONE',  ( -165.9549999999999841, -7.632228543268599452, 2.479861379858951054 ) ) ;
#65539 = ORIENTED_EDGE ( 'NONE', *, *, #57703, .F. ) ;
#65540 = CARTESIAN_POINT ( 'NONE',  ( -112.4929263765338021, -8.102448949553174629, 5.886773742842742685 ) ) ;
#65541 = CARTESIAN_POINT ( 'NONE',  ( -3.000000000000000444, 0.000000000000000000, 52.50000000000000000 ) ) ;
#65542 = FACE_OUTER_BOUND ( 'NONE', #10043, .T. ) ;
#65543 = AXIS2_PLACEMENT_3D ( 'NONE', #26949, #11848, #185 ) ;
#65545 = VECTOR ( 'NONE', #60954, 1000.000000000000000 ) ;
#65544 = VECTOR ( 'NONE', #46467, 1000.000000000000000 ) ;
#65546 = CARTESIAN_POINT ( 'NONE',  ( 0.000000000000000000, 148.0570736234661524, -8.025000000000000355 ) ) ;
#65547 = CIRCLE ( 'NONE', #34114, 0.5000000000000004441 ) ;
#65548 = ORIENTED_EDGE ( 'NONE', *, *, #24553, .F. ) ;
#65549 = PRESENTATION_STYLE_ASSIGNMENT (( #50084 ) ) ;
#65550 = CARTESIAN_POINT ( 'NONE',  ( -86.90499999999998693, 2.607480562269069324, -8.024999999999993250 ) ) ;
#65551 = CARTESIAN_POINT ( 'NONE',  ( -44.99999999999977973, 146.4999999999999716, 7.500000000000000000 ) ) ;
#65552 = FILL_AREA_STYLE_COLOUR ( '', #51864 ) ;
#65553 = DIRECTION ( 'NONE',  ( 0.000000000000000000, 0.000000000000000000, -1.000000000000000000 ) ) ;
#65554 = DIRECTION ( 'NONE',  ( 1.000000000000000000, -0.000000000000000000, -0.000000000000000000 ) ) ;
#65555 = ORIENTED_EDGE ( 'NONE', *, *, #52420, .F. ) ;
#65556 = TOROIDAL_SURFACE ( 'NONE', #17296, 16.44999999999999574, 0.5000000000000000000 ) ;
#65557 = FACE_OUTER_BOUND ( 'NONE', #5224, .T. ) ;
#65558 = CARTESIAN_POINT ( 'NONE',  ( -64.34499999999998465, 7.632228543268599452, -2.479861379858951942 ) ) ;
#65559 = VERTEX_POINT ( 'NONE', #28081 ) ;
#65560 = COLOUR_RGB ( '', 0.08235294, 0.09019608, 0.10196078) ;
#65561 = DIRECTION ( 'NONE',  ( -1.156482317317873451E-16, -1.000000000000000000, 0.000000000000000000 ) ) ;
#65562 = CARTESIAN_POINT ( 'NONE',  ( -45.87390969075753588, 9.272074904602295220, -6.224541297626196013 ) ) ;
#65563 = EDGE_LOOP ( 'NONE', ( #62727, #60490, #50778, #48151 ) ) ;
#65564 = DIRECTION ( 'NONE',  ( 1.000000000000000000, 0.000000000000000000, 0.000000000000000000 ) ) ;
#65565 = ORIENTED_EDGE ( 'NONE', *, *, #49656, .T. ) ;
#65566 = VECTOR ( 'NONE', #47083, 1000.000000000000114 ) ;
#65567 = MECHANICAL_DESIGN_GEOMETRIC_PRESENTATION_REPRESENTATION (  '', ( #16200 ), #4911 ) ;
#65568 = DIRECTION ( 'NONE',  ( 0.000000000000000000, 0.000000000000000000, 1.000000000000000000 ) ) ;
#65569 = CARTESIAN_POINT ( 'NONE',  ( -117.5049999999999670, -6.826472737025115478, -4.959722759717899443 ) ) ;
#65570 = ORIENTED_EDGE ( 'NONE', *, *, #23989, .T. ) ;
#65571 = DIRECTION ( 'NONE',  ( 1.000000000000000000, 0.000000000000000000, -1.300977106640435137E-16 ) ) ;
#65572 = CARTESIAN_POINT ( 'NONE',  ( 0.000000000000000000, 0.000000000000000000, 0.000000000000000000 ) ) ;
#65573 = DIRECTION ( 'NONE',  ( 0.000000000000000000, 0.000000000000000000, -1.000000000000000000 ) ) ;
#65574 = FACE_OUTER_BOUND ( 'NONE', #53800, .T. ) ;
#65575 = CYLINDRICAL_SURFACE ( 'NONE', #10909, 1.000000000000000888 ) ;
#65576 = CARTESIAN_POINT ( 'NONE',  ( -154.8570736234661922, -5.598654528085803328, -7.705886871421366635 ) ) ;
#65577 = CIRCLE ( 'NONE', #40911, 13.00000000000000533 ) ;
#65578 = CARTESIAN_POINT ( 'NONE',  ( -5.598654528085806881, 133.7450000000000045, -7.705886871421374629 ) ) ;
#65579 = CARTESIAN_POINT ( 'NONE',  ( -95.30707362346615241, -10.01517768586948698, 6.132527647946031529E-16 ) ) ;
#65580 = VECTOR ( 'NONE', #17515, 1000.000000000000000 ) ;
#65581 = COLOUR_RGB ( '', 0.08235294, 0.09019608, 0.10196078) ;
#65582 = VERTEX_POINT ( 'NONE', #23201 ) ;
#65583 = FACE_OUTER_BOUND ( 'NONE', #38676, .T. ) ;
#65584 = DIRECTION ( 'NONE',  ( 0.000000000000000000, -1.000000000000000000, 0.000000000000000000 ) ) ;
#65585 = DIRECTION ( 'NONE',  ( 0.000000000000000000, 0.000000000000000000, -1.000000000000000000 ) ) ;
#65586 = STYLED_ITEM ( 'NONE', ( #46953 ), #62992 ) ;
#65587 = CARTESIAN_POINT ( 'NONE',  ( -133.8549999999999898, 4.716976649647094177, 6.492361379858945902 ) ) ;
#65588 = CARTESIAN_POINT ( 'NONE',  ( 62.24999999999998579, 33.99999999999999289, 4.000000000000000000 ) ) ;
#65589 = SURFACE_STYLE_USAGE ( .BOTH. , #44191 ) ;
#65590 = CARTESIAN_POINT ( 'NONE',  ( -145.6450000000000102, 4.716976649647091513, -6.492361379858946790 ) ) ;
#65591 = EDGE_CURVE ( 'NONE', #42583, #45809, #65045, .T. ) ;
#65592 = VECTOR ( 'NONE', #33011, 1000.000000000000000 ) ;
#65593 = CARTESIAN_POINT ( 'NONE',  ( -132.4449999999999932, 0.000000000000000000, 8.024999999999991473 ) ) ;
#65594 = ORIENTED_EDGE ( 'NONE', *, *, #20580, .T. ) ;
#65595 = SURFACE_STYLE_USAGE ( .BOTH. , #38573 ) ;
#65596 = ADVANCED_FACE ( 'NONE', ( #11945 ), #7368, .T. ) ;
#65597 = FACE_OUTER_BOUND ( 'NONE', #67377, .T. ) ;
#65598 = COLOUR_RGB ( '', 0.31764706, 0.68627451, 0.89019608) ;
#65599 = SURFACE_STYLE_FILL_AREA ( #65248 ) ;
#65600 = UNCERTAINTY_MEASURE_WITH_UNIT (LENGTH_MEASURE( 1.000000000000000082E-05 ), #69195, 'distance_accuracy_value', 'NONE');
#65601 = CARTESIAN_POINT ( 'NONE',  ( -184.1929263765337623, -10.01517768586948698, 6.132527647946031529E-16 ) ) ;
#65602 = CARTESIAN_POINT ( 'NONE',  ( -60.89499999999999602, 6.826472737025116366, 4.959722759717898555 ) ) ;
#65603 = EDGE_CURVE ( 'NONE', #41177, #9969, #67136, .T. ) ;
#65604 = AXIS2_PLACEMENT_3D ( 'NONE', #33517, #45152, #32832 ) ;
#65605 =( LENGTH_UNIT ( ) NAMED_UNIT ( * ) SI_UNIT ( .MILLI., .METRE. ) );
#65606 = PLANE ( 'NONE',  #12926 ) ;
#65607 = EDGE_CURVE ( 'NONE', #11349, #60715, #36846, .T. ) ;
#65608 = COLOUR_RGB ( '', 0.66274510, 0.83137255, 0.94901961) ;
#65609 = CARTESIAN_POINT ( 'NONE',  ( 57.75000000000005684, 1.335737076502141715E-13, 4.000000000000000000 ) ) ;
#65610 = DIRECTION ( 'NONE',  ( -0.000000000000000000, -1.000000000000000000, 0.000000000000000000 ) ) ;
#65611 = UNCERTAINTY_MEASURE_WITH_UNIT (LENGTH_MEASURE( 1.000000000000000082E-05 ), #57208, 'distance_accuracy_value', 'NONE');
#65613 =( BOUNDED_CURVE ( )  B_SPLINE_CURVE ( 2, ( #60592, #60946, #12765, #51122, #34237, #56021, #2868, #55691, #12410, #67283, #33870 ),
 .UNSPECIFIED., .F., .F. ) 
 B_SPLINE_CURVE_WITH_KNOTS ( ( 3, 2, 2, 2, 2, 3 ),
 ( 0.2352941176470587370, 0.2411764705882352144, 0.2470588235294116919, 0.2529411764705881693, 0.2588235294117646745, 0.2647058823529411242 ),
 .UNSPECIFIED. ) 
 CURVE ( )  GEOMETRIC_REPRESENTATION_ITEM ( )  RATIONAL_B_SPLINE_CURVE ( ( 1.000000000000000666, 0.9510565162951529761, 1.000000000000000000, 0.9510565162951535312, 1.000000000000000000, 0.9510565162951535312, 1.000000000000000000, 0.9510565162951535312, 1.000000000000000000, 0.9510565162951539753, 0.9999999999999995559 ) ) 
 REPRESENTATION_ITEM ( '' )  );
#65612 = CARTESIAN_POINT ( 'NONE',  ( -94.79292637653378506, -3.094860106618429807, 9.524999999999991473 ) ) ;
#65614 = B_SPLINE_CURVE_WITH_KNOTS ( 'NONE', 3,
 ( #47715, #14971, #47002, #16018, #9335, #31447, #63132, #25150, #52261, #47346, #15657, #69451 ),
 .UNSPECIFIED., .F., .F.,
 ( 4, 2, 2, 2, 2, 4 ),
 ( 4.336808689942017255E-19, 0.001855247662732223239, 0.002782871494098332690, 0.003710495325464443009, 0.005565742988196644564, 0.007420990650928846986 ),
 .UNSPECIFIED. ) ;
#65615 = DIRECTION ( 'NONE',  ( 0.000000000000000000, 0.000000000000000000, -1.000000000000000000 ) ) ;
#65616 = LINE ( 'NONE', #38590, #43933 ) ;
#65617 = EDGE_CURVE ( 'NONE', #40833, #25339, #50514, .T. ) ;
#65618 = PRESENTATION_LAYER_ASSIGNMENT (  '', '', ( #13951 ) ) ;
#65619 = DIRECTION ( 'NONE',  ( -1.000000000000000000, 0.000000000000000000, 0.000000000000000000 ) ) ;
#65620 = AXIS2_PLACEMENT_3D ( 'NONE', #53186, #30655, #52505 ) ;
#65621 =( LENGTH_UNIT ( ) NAMED_UNIT ( * ) SI_UNIT ( .MILLI., .METRE. ) );
#65622 = ORIENTED_EDGE ( 'NONE', *, *, #2328, .T. ) ;
#65623 = FILL_AREA_STYLE ('',( #1546 ) ) ;
#65624 = CARTESIAN_POINT ( 'NONE',  ( -47.50000000000000000, 99.99999999999992895, 9.500000000000000000 ) ) ;
#65625 = ORIENTED_EDGE ( 'NONE', *, *, #5464, .F. ) ;
#65626 = STYLED_ITEM ( 'NONE', ( #52518 ), #2568 ) ;
#65627 = CARTESIAN_POINT ( 'NONE',  ( 2.607480562269076430, 123.9070736234661467, -8.025000000000000355 ) ) ;
#65628 = AXIS2_PLACEMENT_3D ( 'NONE', #49106, #7538, #44189 ) ;
#65629 = CARTESIAN_POINT ( 'NONE',  ( 3.499999999999998668, 36.74999999999999289, 3.750000000000000000 ) ) ;
#65630 = CARTESIAN_POINT ( 'NONE',  ( 75.00000000000000000, 19.70845863561317657, -6.466567654931034248 ) ) ;
#65631 = CARTESIAN_POINT ( 'NONE',  ( 22.99999999999996447, 5.000000000000000000, 29.00402776293825369 ) ) ;
#65632 = ORIENTED_EDGE ( 'NONE', *, *, #57841, .T. ) ;
#65633 = CARTESIAN_POINT ( 'NONE',  ( -6.062177826491070398, -2.500000000000000000, -3.499999999999998224 ) ) ;
#65634 = AXIS2_PLACEMENT_3D ( 'NONE', #65857, #5697, #38121 ) ;
#65635 = ORIENTED_EDGE ( 'NONE', *, *, #45318, .F. ) ;
#65636 = DIRECTION ( 'NONE',  ( 0.000000000000000000, -0.000000000000000000, 1.000000000000000000 ) ) ;
#65637 = CARTESIAN_POINT ( 'NONE',  ( -94.25707362346618368, 5.598654528085800663, -7.705886871421367523 ) ) ;
#65638 = AXIS2_PLACEMENT_3D ( 'NONE', #23751, #8625, #67024 ) ;
#65639 = STYLED_ITEM ( 'NONE', ( #31102 ), #62157 ) ;
#65640 = CARTESIAN_POINT ( 'NONE',  ( 7.632228543268607446, 149.0429263765338135, 2.479861379858954606 ) ) ;
#65641 = CARTESIAN_POINT ( 'NONE',  ( -95.54499999999998749, -7.632228543268600340, -2.479861379858950166 ) ) ;
#65642 = ORIENTED_EDGE ( 'NONE', *, *, #3623, .F. ) ;
#65643 = ADVANCED_FACE ( 'NONE', ( #7691 ), #48934, .F. ) ;
#65644 = SURFACE_SIDE_STYLE ('',( #12866 ) ) ;
#65645 = DIRECTION ( 'NONE',  ( -1.000000000000000000, -0.000000000000000000, -0.000000000000000000 ) ) ;
#65646 = UNCERTAINTY_MEASURE_WITH_UNIT (LENGTH_MEASURE( 1.000000000000000082E-05 ), #64620, 'distance_accuracy_value', 'NONE');
#65647 = ORIENTED_EDGE ( 'NONE', *, *, #57916, .F. ) ;
#65648 = LINE ( 'NONE', #12162, #41493 ) ;
#65649 = FILL_AREA_STYLE_COLOUR ( '', #54870 ) ;
#65650 = CARTESIAN_POINT ( 'NONE',  ( 13.50000000000000533, 30.74999999999999289, 3.750000000000000000 ) ) ;
#65651 = ORIENTED_EDGE ( 'NONE', *, *, #18753, .F. ) ;
#65652 = B_SPLINE_CURVE_WITH_KNOTS ( 'NONE', 3,
 ( #53418, #26640, #48165, #64295, #65338, #43926, #561, #22086, #43586, #16832, #11520, #32993, #54426, #27673, #883, #17183, #60057, #17849, #49870, #50215 ),
 .UNSPECIFIED., .F., .F.,
 ( 4, 2, 2, 2, 2, 2, 2, 2, 2, 4 ),
 ( 0.004227980867416260453, 0.004756478475843291601, 0.005284976084270322748, 0.005813473692697353895, 0.006341971301124385042, 0.006870468909551416190, 0.007398966517978447337, 0.007663215322191966813, 0.007927464126405487158, 0.008455961734832519172 ),
 .UNSPECIFIED. ) ;
#65653 = FILL_AREA_STYLE_COLOUR ( '', #35240 ) ;
#65654 = ORIENTED_EDGE ( 'NONE', *, *, #55426, .F. ) ;
#65655 = LINE ( 'NONE', #44598, #15592 ) ;
#65656 = SURFACE_STYLE_USAGE ( .BOTH. , #16117 ) ;
#65657 = FACE_OUTER_BOUND ( 'NONE', #8790, .T. ) ;
#65658 = CARTESIAN_POINT ( 'NONE',  ( -180.8070736234661524, 10.01517768586948698, -1.839758294383808571E-15 ) ) ;
#65659 = DIRECTION ( 'NONE',  ( 1.000000000000000000, 0.000000000000000000, 0.000000000000000000 ) ) ;
#65660 =( GEOMETRIC_REPRESENTATION_CONTEXT ( 3 ) GLOBAL_UNCERTAINTY_ASSIGNED_CONTEXT ( ( #57429 ) ) GLOBAL_UNIT_ASSIGNED_CONTEXT ( ( #66831, #39424, #67503 ) ) REPRESENTATION_CONTEXT ( 'NONE', 'WORKASPACE' ) );
#65661 = CARTESIAN_POINT ( 'NONE',  ( -0.9728900412908211282, 153.0000000000000000, -7.965808808122195828 ) ) ;
#65662 = ORIENTED_EDGE ( 'NONE', *, *, #68224, .T. ) ;
#65663 = CARTESIAN_POINT ( 'NONE',  ( 21.25000000000000711, 22.24999999999998224, -3.750000000000000000 ) ) ;
#65664 = ADVANCED_FACE ( 'NONE', ( #2357 ), #8411, .T. ) ;
#65665 = TOROIDAL_SURFACE ( 'NONE', #48846, 12.50000000000000000, 0.5000000000000000000 ) ;
#65666 = VERTEX_POINT ( 'NONE', #3413 ) ;
#65667 = CARTESIAN_POINT ( 'NONE',  ( -161.7549999999999955, 4.716976649647091513, -6.492361379858946790 ) ) ;
#65668 = EDGE_CURVE ( 'NONE', #25571, #19536, #51312, .T. ) ;
#65669 = LINE ( 'NONE', #66355, #65580 ) ;
#65670 = SURFACE_STYLE_USAGE ( .BOTH. , #49513 ) ;
#65671 = CARTESIAN_POINT ( 'NONE',  ( -173.5450000000000159, -7.632228543268600340, -2.479861379858950166 ) ) ;
#65672 = CARTESIAN_POINT ( 'NONE',  ( -155.2450000000000045, -4.716976649647093289, -6.492361379858945902 ) ) ;
#65673 = ORIENTED_EDGE ( 'NONE', *, *, #52226, .T. ) ;
#65674 = EDGE_CURVE ( 'NONE', #49290, #24428, #18933, .T. ) ;
#65675 = AXIS2_PLACEMENT_3D ( 'NONE', #28449, #45739, #24565 ) ;
#65676 = SURFACE_STYLE_USAGE ( .BOTH. , #33330 ) ;
#65677 = AXIS2_PLACEMENT_3D ( 'NONE', #64363, #10901, #55168 ) ;
#65678 = CARTESIAN_POINT ( 'NONE',  ( 44.32257855570070149, 10.24209864716889307, 3.524404701559999520 ) ) ;
#65679 = CARTESIAN_POINT ( 'NONE',  ( -74.30499999999996419, 8.437984349512085203, -1.550032578732815448E-15 ) ) ;
#65680 = CARTESIAN_POINT ( 'NONE',  ( 27.00000000000001776, 14.00000000000000000, 34.49999999999998579 ) ) ;
#65681 = SURFACE_STYLE_USAGE ( .BOTH. , #34016 ) ;
#65682 = AXIS2_PLACEMENT_3D ( 'NONE', #16909, #6650, #49252 ) ;
#65683 = CARTESIAN_POINT ( 'NONE',  ( -75.29499999999998749, -2.607480562269069768, 8.024999999999991473 ) ) ;
#65684 = CARTESIAN_POINT ( 'NONE',  ( 3.094860106618431583, 151.2049999999999841, 9.525000000000000355 ) ) ;
#65685 = LINE ( 'NONE', #34375, #53377 ) ;
#65686 = EDGE_CURVE ( 'NONE', #62934, #19236, #16604, .T. ) ;
#65687 = VECTOR ( 'NONE', #59053, 1000.000000000000000 ) ;
#65688 = STYLED_ITEM ( 'NONE', ( #46218 ), #62491 ) ;
#65689 = CARTESIAN_POINT ( 'NONE',  ( 5.812336001418906051, 154.3979462032312995, 7.425621158966782431 ) ) ;
#65690 = UNCERTAINTY_MEASURE_WITH_UNIT (LENGTH_MEASURE( 1.000000000000000082E-05 ), #7244, 'distance_accuracy_value', 'NONE');
#65691 =( NAMED_UNIT ( * ) SI_UNIT ( $, .STERADIAN. ) SOLID_ANGLE_UNIT ( ) );
#65692 = CARTESIAN_POINT ( 'NONE',  ( 0.000000000000000000, -2.500000000000000000, 0.000000000000000000 ) ) ;
#65693 = ORIENTED_EDGE ( 'NONE', *, *, #5795, .T. ) ;
#65694 = ADVANCED_FACE ( 'NONE', ( #62200 ), #62541, .T. ) ;
#65695 = DIRECTION ( 'NONE',  ( 1.000000000000000000, 0.000000000000000000, 0.000000000000000000 ) ) ;
#65696 = CARTESIAN_POINT ( 'NONE',  ( -23.21231517720798010, 1.797044900979284448E-15, -9.500000000000000000 ) ) ;
#65697 = CIRCLE ( 'NONE', #7263, 5.000000000000004441 ) ;
#65698 = PRESENTATION_LAYER_ASSIGNMENT (  '', '', ( #26388 ) ) ;
#65699 = SPHERICAL_SURFACE ( 'NONE', #11338, 1.000000000000000000 ) ;
#65700 = VECTOR ( 'NONE', #5748, 1000.000000000000000 ) ;
#65701 = CARTESIAN_POINT ( 'NONE',  ( 24.21231517720798010, 113.4999999999999858, -9.500000000000000000 ) ) ;
#65702 = CARTESIAN_POINT ( 'NONE',  ( 71.49999999999998579, 64.07124727947029896, -7.000000000000000000 ) ) ;
#65703 = VERTEX_POINT ( 'NONE', #61839 ) ;
#65704 = VERTEX_POINT ( 'NONE', #24906 ) ;
#65705 = MECHANICAL_DESIGN_GEOMETRIC_PRESENTATION_REPRESENTATION (  '', ( #8441 ), #35399 ) ;
#65706 =( BOUNDED_CURVE ( )  B_SPLINE_CURVE ( 2, ( #11917, #39372, #49918, #33377, #6612, #23176, #39036, #60432, #43624, #12240, #11219 ),
 .UNSPECIFIED., .F., .F. ) 
 B_SPLINE_CURVE_WITH_KNOTS ( ( 3, 2, 2, 2, 2, 3 ),
 ( 0.2173913043478209739, 0.2195652173912991945, 0.2217391304347773873, 0.2239130434782556356, 0.2260869565217338284, 0.2282608695652120212 ),
 .UNSPECIFIED. ) 
 CURVE ( )  GEOMETRIC_REPRESENTATION_ITEM ( )  RATIONAL_B_SPLINE_CURVE ( ( 1.000000000000115019, 0.9510565162950385121, 1.000000000000000000, 0.9510565162951535312, 1.000000000000000000, 0.9510565162951535312, 1.000000000000000000, 0.9510565162951535312, 1.000000000000000000, 0.9510565162952741014, 0.9999999999998794298 ) ) 
 REPRESENTATION_ITEM ( '' )  );
#65707 = PRESENTATION_LAYER_ASSIGNMENT (  '', '', ( #27488 ) ) ;
#65708 = CARTESIAN_POINT ( 'NONE',  ( -13.50000000000000355, 27.74999999999998934, -3.750000000000000000 ) ) ;
#65709 = SURFACE_STYLE_USAGE ( .BOTH. , #23477 ) ;
#65710 = CYLINDRICAL_SURFACE ( 'NONE', #17300, 9.524999999999991473 ) ;
#65711 = FILL_AREA_STYLE ('',( #27358 ) ) ;
#65712 = EDGE_LOOP ( 'NONE', ( #58646, #57954, #48919, #32563 ) ) ;
#65713 = CARTESIAN_POINT ( 'NONE',  ( -116.9050000000000011, 2.607480562269069324, -8.024999999999993250 ) ) ;
#65714 = EDGE_LOOP ( 'NONE', ( #6271, #59389 ) ) ;
#65715 = PRESENTATION_STYLE_ASSIGNMENT (( #16863 ) ) ;
#65716 = EDGE_LOOP ( 'NONE', ( #9270, #52738, #15249, #2249 ) ) ;
#65717 = FILL_AREA_STYLE ('',( #44318 ) ) ;
#65718 = CARTESIAN_POINT ( 'NONE',  ( -69.05707362346618083, 0.000000000000000000, 9.524999999999991473 ) ) ;
#65719 = ORIENTED_EDGE ( 'NONE', *, *, #29118, .T. ) ;
#65720 = DIRECTION ( 'NONE',  ( 0.000000000000000000, 0.000000000000000000, -1.000000000000000000 ) ) ;
#65721 = CARTESIAN_POINT ( 'NONE',  ( -8.102448949553181734, 157.8950000000000102, -5.886773742842749790 ) ) ;
#65722 = DIRECTION ( 'NONE',  ( 0.000000000000000000, 0.000000000000000000, -1.000000000000000000 ) ) ;
#65723 = ORIENTED_EDGE ( 'NONE', *, *, #8813, .T. ) ;
#65724 = EDGE_CURVE ( 'NONE', #23416, #35108, #9103, .T. ) ;
#65725 = ORIENTED_EDGE ( 'NONE', *, *, #40277, .T. ) ;
#65726 = CARTESIAN_POINT ( 'NONE',  ( -74.20344633242609689, 8.974374905500289046, -6.364158535394771832 ) ) ;
#65727 = CARTESIAN_POINT ( 'NONE',  ( -40.49999999999998579, 107.7459666924148394, -3.000000000000000444 ) ) ;
#65728 = ORIENTED_EDGE ( 'NONE', *, *, #8105, .F. ) ;
#65729 = CARTESIAN_POINT ( 'NONE',  ( -8.437984349512095861, 138.6929263765338192, -5.166775262442723748E-16 ) ) ;
#65730 = CARTESIAN_POINT ( 'NONE',  ( -22.75000000000000711, 34.24999999999999289, 3.750000000000000000 ) ) ;
#65731 =( LENGTH_UNIT ( ) NAMED_UNIT ( * ) SI_UNIT ( .MILLI., .METRE. ) );
#65732 =( GEOMETRIC_REPRESENTATION_CONTEXT ( 3 ) GLOBAL_UNCERTAINTY_ASSIGNED_CONTEXT ( ( #10162 ) ) GLOBAL_UNIT_ASSIGNED_CONTEXT ( ( #41249, #14472, #17453 ) ) REPRESENTATION_CONTEXT ( 'NONE', 'WORKASPACE' ) );
#65733 = DIRECTION ( 'NONE',  ( -0.000000000000000000, 1.000000000000000000, -0.000000000000000000 ) ) ;
#65734 = LINE ( 'NONE', #34070, #37803 ) ;
#65735 = ORIENTED_EDGE ( 'NONE', *, *, #34857, .F. ) ;
#65736 =( LENGTH_UNIT ( ) NAMED_UNIT ( * ) SI_UNIT ( .MILLI., .METRE. ) );
#65737 = VERTEX_POINT ( 'NONE', #41470 ) ;
#65738 = SURFACE_STYLE_FILL_AREA ( #11930 ) ;
#65739 = VECTOR ( 'NONE', #60419, 1000.000000000000000 ) ;
#65740 = DIRECTION ( 'NONE',  ( -1.000000000000000000, 0.000000000000000000, 0.000000000000000000 ) ) ;
#65741 = DIRECTION ( 'NONE',  ( 1.156482317317873451E-16, -1.000000000000000000, -0.000000000000000000 ) ) ;
#65742 = DIRECTION ( 'NONE',  ( 0.9994052928406508274, 0.03448275862069643399, -0.000000000000000000 ) ) ;
#65743 =( GEOMETRIC_REPRESENTATION_CONTEXT ( 3 ) GLOBAL_UNCERTAINTY_ASSIGNED_CONTEXT ( ( #41031 ) ) GLOBAL_UNIT_ASSIGNED_CONTEXT ( ( #4126, #3412, #53050 ) ) REPRESENTATION_CONTEXT ( 'NONE', 'WORKASPACE' ) );
#65744 = CARTESIAN_POINT ( 'NONE',  ( -131.9050000000000011, 2.607480562269068880, -8.024999999999993250 ) ) ;
#65745 = DIRECTION ( 'NONE',  ( 0.000000000000000000, 0.000000000000000000, 1.000000000000000000 ) ) ;
#65746 = FACE_OUTER_BOUND ( 'NONE', #28519, .T. ) ;
#65747 = ORIENTED_EDGE ( 'NONE', *, *, #35521, .F. ) ;
#65748 = PRODUCT_RELATED_PRODUCT_CATEGORY ( 'part', '', ( #10291 ) ) ;
#65749 = EDGE_CURVE ( 'NONE', #47479, #46287, #17702, .T. ) ;
#65750 = CARTESIAN_POINT ( 'NONE',  ( -24.00000000000000000, 1.000000000000000000, -3.000000000000000000 ) ) ;
#65751 = EDGE_CURVE ( 'NONE', #4180, #57518, #40096, .T. ) ;
#65752 = CARTESIAN_POINT ( 'NONE',  ( -157.0429263765338135, -9.058813317711329915, -2.943386871421370898 ) ) ;
#65753 = CARTESIAN_POINT ( 'NONE',  ( -7.511572993685798115E-16, -2.500000000000000000, 6.999999999999997335 ) ) ;
#65754 = VERTEX_POINT ( 'NONE', #56223 ) ;
#65755 = EDGE_LOOP ( 'NONE', ( #54778, #11836, #16442, #50354 ) ) ;
#65756 = CARTESIAN_POINT ( 'NONE',  ( -45.89905495969589566, 9.405628579224391217, 3.101891717392576187 ) ) ;
#65757 = FILL_AREA_STYLE_COLOUR ( '', #58165 ) ;
#65758 = EDGE_CURVE ( 'NONE', #46687, #47709, #46419, .T. ) ;
#65759 = CARTESIAN_POINT ( 'NONE',  ( -54.50499999999998835, -6.826472737025115478, -4.959722759717899443 ) ) ;
#65761 = VERTEX_POINT ( 'NONE', #45725 ) ;
#65760 = CIRCLE ( 'NONE', #66878, 23.00000000000000000 ) ;
#65762 = CYLINDRICAL_SURFACE ( 'NONE', #65155, 0.2500000000000002220 ) ;
#65763 = FACE_OUTER_BOUND ( 'NONE', #24425, .T. ) ;
#65764 = EDGE_CURVE ( 'NONE', #5489, #62632, #8746, .T. ) ;
#65765 = DIRECTION ( 'NONE',  ( 0.000000000000000000, 0.000000000000000000, -1.000000000000000000 ) ) ;
#65766 = DIRECTION ( 'NONE',  ( -0.000000000000000000, -0.000000000000000000, -1.000000000000000000 ) ) ;
#65767 =( GEOMETRIC_REPRESENTATION_CONTEXT ( 3 ) GLOBAL_UNCERTAINTY_ASSIGNED_CONTEXT ( ( #39087 ) ) GLOBAL_UNIT_ASSIGNED_CONTEXT ( ( #68008, #9616, #9948 ) ) REPRESENTATION_CONTEXT ( 'NONE', 'WORKASPACE' ) );
#65768 = CARTESIAN_POINT ( 'NONE',  ( -195.0000000000000000, 0.000000000000000000, 0.000000000000000000 ) ) ;
#65769 = LINE ( 'NONE', #2737, #18549 ) ;
#65770 = VERTEX_POINT ( 'NONE', #25264 ) ;
#65771 = DIRECTION ( 'NONE',  ( 0.000000000000000000, 0.6691306063588591257, 0.7431448254773933559 ) ) ;
#65772 = EDGE_CURVE ( 'NONE', #68774, #34213, #18927, .T. ) ;
#65773 = MECHANICAL_DESIGN_GEOMETRIC_PRESENTATION_REPRESENTATION (  '', ( #8499 ), #36606 ) ;
#65774 = DIRECTION ( 'NONE',  ( -1.000000000000000000, 0.000000000000000000, 1.300977106640434891E-16 ) ) ;
#65775 = CARTESIAN_POINT ( 'NONE',  ( 2.999999999999998668, 5.000000000000000000, 72.00402776293822171 ) ) ;
#65776 = CARTESIAN_POINT ( 'NONE',  ( 71.50000000000000000, 35.92875272052971525, -7.500000000000000000 ) ) ;
#65777 = ADVANCED_FACE ( 'NONE', ( #37255 ), #58657, .F. ) ;
#65778 = CARTESIAN_POINT ( 'NONE',  ( -104.0949999999999989, -2.607480562269071545, -8.024999999999991473 ) ) ;
#65779 = CARTESIAN_POINT ( 'NONE',  ( 3.094860106618435136, 154.2949999999999875, -9.525000000000000355 ) ) ;
#65780 = CARTESIAN_POINT ( 'NONE',  ( -78.59499999999999886, 2.607480562269073321, 8.024999999999991473 ) ) ;
#65781 = PRESENTATION_STYLE_ASSIGNMENT (( #54176 ) ) ;
#65782 = CARTESIAN_POINT ( 'NONE',  ( -6.826472737025120807, 141.3929263765338078, -4.959722759717907437 ) ) ;
#65783 = FACE_OUTER_BOUND ( 'NONE', #2540, .T. ) ;
#65784 = UNCERTAINTY_MEASURE_WITH_UNIT (LENGTH_MEASURE( 1.000000000000000082E-05 ), #43026, 'distance_accuracy_value', 'NONE');
#65786 = FILL_AREA_STYLE_COLOUR ( '', #5612 ) ;
#65785 = APPLICATION_CONTEXT ( 'automotive_design' ) ;
#65787 = MECHANICAL_DESIGN_GEOMETRIC_PRESENTATION_REPRESENTATION (  '', ( #2825 ), #5156 ) ;
#65788 = FILL_AREA_STYLE_COLOUR ( '', #62326 ) ;
#65789 = ORIENTED_EDGE ( 'NONE', *, *, #4593, .T. ) ;
#65790 = CARTESIAN_POINT ( 'NONE',  ( -123.7429263765338021, -5.598654528085803328, -7.705886871421366635 ) ) ;
#65791 = CARTESIAN_POINT ( 'NONE',  ( -134.9950000000000045, -6.826472737025115478, 4.959722759717900331 ) ) ;
#65792 = VECTOR ( 'NONE', #65952, 1000.000000000000000 ) ;
#65793 = DIRECTION ( 'NONE',  ( -0.000000000000000000, -1.000000000000000000, 0.000000000000000000 ) ) ;
#65794 = CIRCLE ( 'NONE', #39970, 5.000000000000000000 ) ;
#65795 = DIRECTION ( 'NONE',  ( -1.000000000000000000, 0.000000000000000000, 0.000000000000000000 ) ) ;
#65796 = ORIENTED_EDGE ( 'NONE', *, *, #177, .F. ) ;
#65797 = ORIENTED_EDGE ( 'NONE', *, *, #15467, .T. ) ;
#65798 = MECHANICAL_DESIGN_GEOMETRIC_PRESENTATION_REPRESENTATION (  '', ( #57929 ), #63582 ) ;
#65799 = EDGE_CURVE ( 'NONE', #32643, #30766, #58317, .T. ) ;
#65800 = LINE ( 'NONE', #39100, #51720 ) ;
#65801 = SPHERICAL_SURFACE ( 'NONE', #11683, 0.5000000000000000000 ) ;
#65802 = DIRECTION ( 'NONE',  ( 0.000000000000000000, 0.000000000000000000, 1.000000000000000000 ) ) ;
#65803 = CARTESIAN_POINT ( 'NONE',  ( -131.4570736234661865, -9.058813317711329915, 2.943386871421371787 ) ) ;
#65804 = LINE ( 'NONE', #17303, #26190 ) ;
#65805 = VERTEX_POINT ( 'NONE', #10486 ) ;
#65806 = CARTESIAN_POINT ( 'NONE',  ( -144.9550000000000125, -7.632228543268599452, 2.479861379858951054 ) ) ;
#65807 = ORIENTED_EDGE ( 'NONE', *, *, #54384, .T. ) ;
#65808 = VECTOR ( 'NONE', #6020, 1000.000000000000000 ) ;
#65809 = VERTEX_POINT ( 'NONE', #21719 ) ;
#65810 = DIRECTION ( 'NONE',  ( 0.000000000000000000, -0.9984713486292863260, 0.05527174654752588928 ) ) ;
#65811 = FACE_OUTER_BOUND ( 'NONE', #33780, .T. ) ;
#65812 = ORIENTED_EDGE ( 'NONE', *, *, #10579, .F. ) ;
#65813 = AXIS2_PLACEMENT_3D ( 'NONE', #24289, #41907, #41538 ) ;
#65814 = VECTOR ( 'NONE', #5013, 1000.000000000000000 ) ;
#65815 = CARTESIAN_POINT ( 'NONE',  ( -54.91578578071454331, -9.007051595042142367, -1.826885762205050501 ) ) ;
#65816 = CARTESIAN_POINT ( 'NONE',  ( 68.99999999999998579, 36.75000000000000000, 3.000000000000000000 ) ) ;
#65817 = CARTESIAN_POINT ( 'NONE',  ( 0.000000000000000000, 130.4449999999999648, -9.525000000000000355 ) ) ;
#65818 =( GEOMETRIC_REPRESENTATION_CONTEXT ( 3 ) GLOBAL_UNCERTAINTY_ASSIGNED_CONTEXT ( ( #49616 ) ) GLOBAL_UNIT_ASSIGNED_CONTEXT ( ( #37311, #16186, #64338 ) ) REPRESENTATION_CONTEXT ( 'NONE', 'WORKASPACE' ) );
#65819 = EDGE_LOOP ( 'NONE', ( #44363, #1803, #19062, #55709 ) ) ;
#65820 = CARTESIAN_POINT ( 'NONE',  ( -195.0000000000000000, 0.000000000000000000, 0.000000000000000000 ) ) ;
#65821 = CARTESIAN_POINT ( 'NONE',  ( 9.058813317711337021, 127.6549999999999869, 2.943386871421375783 ) ) ;
#65822 = CARTESIAN_POINT ( 'NONE',  ( -50.60499999999996845, 6.826472737025113702, -4.959722759717902107 ) ) ;
#65823 = COLOUR_RGB ( '', 0.31764706, 0.68627451, 0.89019608) ;
#65824 = CARTESIAN_POINT ( 'NONE',  ( 41.21596654039887397, 107.8367875949926429, -3.443506282739404512 ) ) ;
#65825 = ORIENTED_EDGE ( 'NONE', *, *, #4023, .T. ) ;
#65826 = CARTESIAN_POINT ( 'NONE',  ( 5.598654528085809545, 158.2549999999999670, -7.705886871421373741 ) ) ;
#65827 = DIRECTION ( 'NONE',  ( 0.000000000000000000, -1.000000000000000000, 0.000000000000000000 ) ) ;
#65828 = UNCERTAINTY_MEASURE_WITH_UNIT (LENGTH_MEASURE( 1.000000000000000082E-05 ), #41809, 'distance_accuracy_value', 'NONE');
#65829 = FACE_OUTER_BOUND ( 'NONE', #12336, .T. ) ;
#65830 = FILL_AREA_STYLE ('',( #44428 ) ) ;
#65831 = LINE ( 'NONE', #13049, #41078 ) ;
#65832 = ORIENTED_EDGE ( 'NONE', *, *, #47973, .T. ) ;
#65833 = CARTESIAN_POINT ( 'NONE',  ( 18.00000000000000711, 33.74999999999999289, -3.750000000000000000 ) ) ;
#65834 = ORIENTED_EDGE ( 'NONE', *, *, #28886, .T. ) ;
#65835 = CARTESIAN_POINT ( 'NONE',  ( 2.000000000000015987, 26.00000000000000355, 27.49999999999999645 ) ) ;
#65836 =( NAMED_UNIT ( * ) PLANE_ANGLE_UNIT ( ) SI_UNIT ( $, .RADIAN. ) );
#65837 = CARTESIAN_POINT ( 'NONE',  ( -173.3049999999999500, 8.437984349512085203, -1.550032578732815448E-15 ) ) ;
#65838 = ORIENTED_EDGE ( 'NONE', *, *, #34615, .T. ) ;
#65839 = UNCERTAINTY_MEASURE_WITH_UNIT (LENGTH_MEASURE( 1.000000000000000082E-05 ), #55583, 'distance_accuracy_value', 'NONE');
#65840 = COLOUR_RGB ( '', 0.31764706, 0.68627451, 0.89019608) ;
#65841 = ADVANCED_FACE ( 'NONE', ( #64638 ), #32268, .T. ) ;
#65842 =( NAMED_UNIT ( * ) SI_UNIT ( $, .STERADIAN. ) SOLID_ANGLE_UNIT ( ) );
#65843 = CARTESIAN_POINT ( 'NONE',  ( 44.99999999999977973, 146.9999999999999716, 7.000000000000000000 ) ) ;
#65844 = CARTESIAN_POINT ( 'NONE',  ( -77.99292637653378790, 8.102448949553172852, -5.886773742842744461 ) ) ;
#65845 = EDGE_LOOP ( 'NONE', ( #32054, #26971, #12776 ) ) ;
#65846 = ORIENTED_EDGE ( 'NONE', *, *, #69500, .F. ) ;
#65847 = DIRECTION ( 'NONE',  ( 0.000000000000000000, 0.000000000000000000, -1.000000000000000000 ) ) ;
#65848 =( GEOMETRIC_REPRESENTATION_CONTEXT ( 3 ) GLOBAL_UNCERTAINTY_ASSIGNED_CONTEXT ( ( #54435 ) ) GLOBAL_UNIT_ASSIGNED_CONTEXT ( ( #33642, #11843, #38974 ) ) REPRESENTATION_CONTEXT ( 'NONE', 'WORKASPACE' ) );
#65850 = EDGE_CURVE ( 'NONE', #55407, #22006, #31922, .T. ) ;
#65849 = DIRECTION ( 'NONE',  ( -1.000000000000000000, 0.000000000000000000, 0.000000000000000000 ) ) ;
#65851 = CARTESIAN_POINT ( 'NONE',  ( -87.20499999999999829, -2.607480562269071545, -8.024999999999991473 ) ) ;
#65852 = ORIENTED_EDGE ( 'NONE', *, *, #13167, .F. ) ;
#65853 = CARTESIAN_POINT ( 'NONE',  ( 30.75000000000001066, 15.99999999999997691, 3.750000000000000000 ) ) ;
#65854 =( GEOMETRIC_REPRESENTATION_CONTEXT ( 3 ) GLOBAL_UNCERTAINTY_ASSIGNED_CONTEXT ( ( #20805 ) ) GLOBAL_UNIT_ASSIGNED_CONTEXT ( ( #34571, #62360, #51126 ) ) REPRESENTATION_CONTEXT ( 'NONE', 'WORKASPACE' ) );
#65855 = AXIS2_PLACEMENT_3D ( 'NONE', #44334, #55523, #7347 ) ;
#65856 =( GEOMETRIC_REPRESENTATION_CONTEXT ( 3 ) GLOBAL_UNCERTAINTY_ASSIGNED_CONTEXT ( ( #34659 ) ) GLOBAL_UNIT_ASSIGNED_CONTEXT ( ( #17556, #17878, #62151 ) ) REPRESENTATION_CONTEXT ( 'NONE', 'WORKASPACE' ) );
#65857 = CARTESIAN_POINT ( 'NONE',  ( 22.25000000000000711, 34.24999999999999289, -3.750000000000000000 ) ) ;
#65858 = VERTEX_POINT ( 'NONE', #53402 ) ;
#65859 = CARTESIAN_POINT ( 'NONE',  ( 0.000000000000000000, 142.0570736234661524, -8.025000000000000355 ) ) ;
#65860 = CARTESIAN_POINT ( 'NONE',  ( 21.02379604162863913, 109.9999999999999858, 10.50000000000000000 ) ) ;
#65861 = EDGE_CURVE ( 'NONE', #63927, #66633, #11881, .T. ) ;
#65862 = AXIS2_PLACEMENT_3D ( 'NONE', #29460, #51277, #51982 ) ;
#65863 = CARTESIAN_POINT ( 'NONE',  ( 9.058813317711337021, 132.5449999999999875, 2.943386871421375783 ) ) ;
#65864 = CARTESIAN_POINT ( 'NONE',  ( -106.7949999999999733, 2.607480562269068880, -8.024999999999993250 ) ) ;
#65865 = PRESENTATION_LAYER_ASSIGNMENT (  '', '', ( #17583 ) ) ;
#65866 = DIRECTION ( 'NONE',  ( 0.000000000000000000, 0.000000000000000000, 1.000000000000000000 ) ) ;
#65867 = CARTESIAN_POINT ( 'NONE',  ( -33.24469977103449736, -9.366146070812339630, -2.498496608837086796 ) ) ;
#65868 = CARTESIAN_POINT ( 'NONE',  ( -148.4929263765337737, -8.102448949553172852, 5.886773742842742685 ) ) ;
#65869 =( LENGTH_UNIT ( ) NAMED_UNIT ( * ) SI_UNIT ( .MILLI., .METRE. ) );
#65870 = CARTESIAN_POINT ( 'NONE',  ( -166.7950000000000159, 2.607480562269068880, -8.024999999999993250 ) ) ;
#65871 = ADVANCED_FACE ( 'NONE', ( #42202 ), #48496, .T. ) ;
#65872 = FACE_OUTER_BOUND ( 'NONE', #65993, .T. ) ;
#65873 = DIRECTION ( 'NONE',  ( -0.000000000000000000, -0.000000000000000000, -1.000000000000000000 ) ) ;
#65874 = ORIENTED_EDGE ( 'NONE', *, *, #31348, .T. ) ;
#65875 = DIRECTION ( 'NONE',  ( -0.000000000000000000, -0.000000000000000000, -1.000000000000000000 ) ) ;
#65876 = EDGE_LOOP ( 'NONE', ( #16091, #54020, #605, #18352 ) ) ;
#65877 = CARTESIAN_POINT ( 'NONE',  ( -68.54292637653379927, 9.058813317711329915, 2.943386871421369566 ) ) ;
#65878 = EDGE_CURVE ( 'NONE', #16768, #50360, #60343, .T. ) ;
#65879 = B_SPLINE_CURVE_WITH_KNOTS ( 'NONE', 3,
 ( #42950, #22835, #16884, #27032, #10890, #38707, #32332, #54130 ),
 .UNSPECIFIED., .F., .F.,
 ( 4, 2, 2, 4 ),
 ( 0.005429405001700385487, 0.006777257746060603126, 0.008125110490420819898, 0.01082081597914125344 ),
 .UNSPECIFIED. ) ;
#65880 = CARTESIAN_POINT ( 'NONE',  ( -45.86904680146955116, 9.253562910438322575, 6.241030289661793518 ) ) ;
#65881 = DIRECTION ( 'NONE',  ( -0.000000000000000000, -0.000000000000000000, -1.000000000000000000 ) ) ;
#65882 = DIRECTION ( 'NONE',  ( 1.669238443041287922E-16, -0.000000000000000000, 1.000000000000000000 ) ) ;
#65883 = CARTESIAN_POINT ( 'NONE',  ( -141.8929263765337794, -8.102448949553174629, -5.886773742842741797 ) ) ;
#65884 =( NAMED_UNIT ( * ) SI_UNIT ( $, .STERADIAN. ) SOLID_ANGLE_UNIT ( ) );
#65885 = CARTESIAN_POINT ( 'NONE',  ( -79.19292637653379074, -10.01517768586948698, 6.132527647946031529E-16 ) ) ;
#65886 = VERTEX_POINT ( 'NONE', #20331 ) ;
#65887 = CARTESIAN_POINT ( 'NONE',  ( -172.1050000000000182, -6.826472737025113702, 4.959722759717902107 ) ) ;
#65888 = CIRCLE ( 'NONE', #5210, 4.000000000000000000 ) ;
#65889 = ORIENTED_EDGE ( 'NONE', *, *, #27283, .T. ) ;
#65890 = DIRECTION ( 'NONE',  ( 1.000000000000000000, 0.000000000000000000, 0.000000000000000000 ) ) ;
#65891 = SURFACE_SIDE_STYLE ('',( #66587 ) ) ;
#65892 = VECTOR ( 'NONE', #42348, 1000.000000000000000 ) ;
#65893 = FILL_AREA_STYLE ('',( #52074 ) ) ;
#65894 =( NAMED_UNIT ( * ) SI_UNIT ( $, .STERADIAN. ) SOLID_ANGLE_UNIT ( ) );
#65895 = CARTESIAN_POINT ( 'NONE',  ( -2.607480562269075097, 149.4070736234661751, 8.025000000000000355 ) ) ;
#65896 = ORIENTED_EDGE ( 'NONE', *, *, #3633, .T. ) ;
#65897 = CARTESIAN_POINT ( 'NONE',  ( -83.00499999999998124, 6.826472737025115478, 4.959722759717899443 ) ) ;
#65898 = CARTESIAN_POINT ( 'NONE',  ( 9.058813317711337021, 127.6549999999999869, 2.943386871421375783 ) ) ;
#65899 = UNCERTAINTY_MEASURE_WITH_UNIT (LENGTH_MEASURE( 1.000000000000000082E-05 ), #45792, 'distance_accuracy_value', 'NONE');
#65900 = CIRCLE ( 'NONE', #69279, 5.499999999999976907 ) ;
#65901 = FILL_AREA_STYLE_COLOUR ( '', #28204 ) ;
#65902 = CARTESIAN_POINT ( 'NONE',  ( -113.6929263765337907, 10.01517768586948698, -1.839758294383808966E-15 ) ) ;
#65903 = CARTESIAN_POINT ( 'NONE',  ( -195.0000000000000000, 0.000000000000000000, 7.499999999999984901 ) ) ;
#65904 = EDGE_CURVE ( 'NONE', #63288, #30672, #14310, .T. ) ;
#65905 = SURFACE_STYLE_FILL_AREA ( #56027 ) ;
#65906 = VERTEX_POINT ( 'NONE', #20691 ) ;
#65907 = FACE_OUTER_BOUND ( 'NONE', #6438, .T. ) ;
#65908 = SURFACE_STYLE_FILL_AREA ( #65205 ) ;
#65909 = CARTESIAN_POINT ( 'NONE',  ( -63.44499999999998607, 0.000000000000000000, 8.024999999999991473 ) ) ;
#65910 = ORIENTED_EDGE ( 'NONE', *, *, #13363, .T. ) ;
#65911 = SURFACE_STYLE_USAGE ( .BOTH. , #13835 ) ;
#65912 = CARTESIAN_POINT ( 'NONE',  ( -48.74292637653379501, -5.598654528085803328, -7.705886871421366635 ) ) ;
#65913 = CARTESIAN_POINT ( 'NONE',  ( -45.00000000000000000, 8.421502636539827336, -6.236752812775022470 ) ) ;
#65914 = ORIENTED_EDGE ( 'NONE', *, *, #13743, .T. ) ;
#65915 = DIRECTION ( 'NONE',  ( -0.000000000000000000, 1.000000000000000000, 0.000000000000000000 ) ) ;
#65916 = CARTESIAN_POINT ( 'NONE',  ( -51.59499999999997755, 2.607480562269072433, 8.024999999999991473 ) ) ;
#65917 = DIRECTION ( 'NONE',  ( 1.000000000000000000, -0.000000000000000000, -0.000000000000000000 ) ) ;
#65918 = ORIENTED_EDGE ( 'NONE', *, *, #20545, .F. ) ;
#65920 = ADVANCED_FACE ( 'NONE', ( #21028 ), #34540, .T. ) ;
#65919 = PLANE ( 'NONE',  #59484 ) ;
#65921 = CARTESIAN_POINT ( 'NONE',  ( -109.8549999999999898, 4.716976649647094177, 6.492361379858945902 ) ) ;
#65922 = ORIENTED_EDGE ( 'NONE', *, *, #43895, .F. ) ;
#65923 = SURFACE_SIDE_STYLE ('',( #32881 ) ) ;
#65924 = SURFACE_SIDE_STYLE ('',( #49413 ) ) ;
#65925 = CARTESIAN_POINT ( 'NONE',  ( 26.00000000000001776, 42.00000000000000000, -34.49999999999999289 ) ) ;
#65926 = CARTESIAN_POINT ( 'NONE',  ( -145.8570736234661638, -5.598654528085803328, -7.705886871421366635 ) ) ;
#65927 = EDGE_CURVE ( 'NONE', #62912, #68888, #98, .T. ) ;
#65928 = CARTESIAN_POINT ( 'NONE',  ( -23.71231517720798010, 117.4999999999999716, 10.00000000000000000 ) ) ;
#65929 = CARTESIAN_POINT ( 'NONE',  ( -3.094860106618432471, 136.5949999999999989, -9.525000000000000355 ) ) ;
#65930 = CARTESIAN_POINT ( 'NONE',  ( -88.40707362346614673, 3.094860106618428031, -9.524999999999993250 ) ) ;
#65931 = EDGE_CURVE ( 'NONE', #47977, #26603, #23302, .T. ) ;
#65932 = DIRECTION ( 'NONE',  ( 1.000000000000000000, 0.000000000000000000, 0.000000000000000000 ) ) ;
#65933 = ORIENTED_EDGE ( 'NONE', *, *, #69514, .T. ) ;
#65934 =( NAMED_UNIT ( * ) PLANE_ANGLE_UNIT ( ) SI_UNIT ( $, .RADIAN. ) );
#65935 =( NAMED_UNIT ( * ) SI_UNIT ( $, .STERADIAN. ) SOLID_ANGLE_UNIT ( ) );
#65936 = EDGE_CURVE ( 'NONE', #9180, #33812, #24003, .T. ) ;
#65937 = CARTESIAN_POINT ( 'NONE',  ( -130.5549999999999784, 0.000000000000000000, 8.024999999999991473 ) ) ;
#65938 = DIRECTION ( 'NONE',  ( 0.000000000000000000, 0.000000000000000000, -1.000000000000000000 ) ) ;
#65939 = VECTOR ( 'NONE', #61723, 1000.000000000000114 ) ;
#65940 = CARTESIAN_POINT ( 'NONE',  ( 45.50000000000000000, 9.639620389971918613, -6.999999999999999112 ) ) ;
#65941 = FILL_AREA_STYLE_COLOUR ( '', #19690 ) ;
#65942 = CARTESIAN_POINT ( 'NONE',  ( -139.9449999999999932, -9.827790563157499189E-16, -8.024999999999991473 ) ) ;
#65943 = AXIS2_PLACEMENT_3D ( 'NONE', #36971, #46854, #30948 ) ;
#65944 = CARTESIAN_POINT ( 'NONE',  ( -129.1449999999999818, -4.716976649647092401, 6.492361379858946790 ) ) ;
#65945 = ORIENTED_EDGE ( 'NONE', *, *, #39762, .F. ) ;
#65946 = DIRECTION ( 'NONE',  ( 0.000000000000000000, 0.000000000000000000, 1.000000000000000000 ) ) ;
#65947 = CARTESIAN_POINT ( 'NONE',  ( 57.24999999999999289, 27.99999999999998934, 3.750000000000000000 ) ) ;
#65948 = CARTESIAN_POINT ( 'NONE',  ( -58.75000000000000000, -13.99999999999999822, 11.89999999999999858 ) ) ;
#65949 = CARTESIAN_POINT ( 'NONE',  ( -178.1929263765338192, -10.01517768586948698, 6.132527647946031529E-16 ) ) ;
#65950 = CARTESIAN_POINT ( 'NONE',  ( -58.19500000000000028, 8.437984349512085203, -1.550032578732815448E-15 ) ) ;
#65951 = AXIS2_PLACEMENT_3D ( 'NONE', #14602, #24794, #65111 ) ;
#65952 = DIRECTION ( 'NONE',  ( 1.000000000000000000, -0.000000000000000000, 0.000000000000000000 ) ) ;
#65953 = DIRECTION ( 'NONE',  ( -1.000000000000000000, -0.000000000000000000, -0.000000000000000000 ) ) ;
#65954 = CARTESIAN_POINT ( 'NONE',  ( -54.91569865845073650, -9.007098961898055478, -1.826967611413356396 ) ) ;
#65955 = CARTESIAN_POINT ( 'NONE',  ( -99.29292637653378506, 3.094860106618428031, -9.524999999999993250 ) ) ;
#65956 =( NAMED_UNIT ( * ) PLANE_ANGLE_UNIT ( ) SI_UNIT ( $, .RADIAN. ) );
#65957 = CYLINDRICAL_SURFACE ( 'NONE', #41375, 8.025000000000000355 ) ;
#65958 = DIRECTION ( 'NONE',  ( 1.000000000000000000, 7.709882115452468306E-16, -0.000000000000000000 ) ) ;
#65959 = CARTESIAN_POINT ( 'NONE',  ( -163.6429263765338078, -5.598654528085801552, 7.705886871421367523 ) ) ;
#65960 = LINE ( 'NONE', #45242, #54057 ) ;
#65961 = VERTEX_POINT ( 'NONE', #27313 ) ;
#65962 = PRESENTATION_STYLE_ASSIGNMENT (( #12488 ) ) ;
#65963 = CARTESIAN_POINT ( 'NONE',  ( 59.00000000000000000, 11.99999999999999822, -4.000000000000000000 ) ) ;
#65964 = ORIENTED_EDGE ( 'NONE', *, *, #50524, .T. ) ;
#65965 = DIRECTION ( 'NONE',  ( 1.000000000000000000, 0.000000000000000000, 0.000000000000000000 ) ) ;
#65966 = CARTESIAN_POINT ( 'NONE',  ( -7.632228543268608334, 124.9570736234661581, 2.479861379858952830 ) ) ;
#65967 = DIRECTION ( 'NONE',  ( 0.000000000000000000, 1.000000000000000000, -0.000000000000000000 ) ) ;
#65968 = PRESENTATION_STYLE_ASSIGNMENT (( #22370 ) ) ;
#65969 = SURFACE_SIDE_STYLE ('',( #33959 ) ) ;
#65970 = AXIS2_PLACEMENT_3D ( 'NONE', #18598, #49573, #54479 ) ;
#65971 = VERTEX_POINT ( 'NONE', #1593 ) ;
#65972 = AXIS2_PLACEMENT_3D ( 'NONE', #47470, #31570, #5180 ) ;
#65973 =( NAMED_UNIT ( * ) SI_UNIT ( $, .STERADIAN. ) SOLID_ANGLE_UNIT ( ) );
#65974 = FILL_AREA_STYLE ('',( #511 ) ) ;
#65975 = ORIENTED_EDGE ( 'NONE', *, *, #41671, .F. ) ;
#65976 = AXIS2_PLACEMENT_3D ( 'NONE', #48922, #5592, #59081 ) ;
#65977 = DIRECTION ( 'NONE',  ( 0.000000000000000000, 0.6449798928094538919, 0.7641995406119433953 ) ) ;
#65978 = EDGE_CURVE ( 'NONE', #30128, #11361, #32285, .T. ) ;
#65979 = CARTESIAN_POINT ( 'NONE',  ( 0.000000000000000000, 33.74999999999999289, 3.750000000000000000 ) ) ;
#65980 = CARTESIAN_POINT ( 'NONE',  ( -92.84499999999998465, -7.632228543268599452, 2.479861379858951054 ) ) ;
#65981 = ORIENTED_EDGE ( 'NONE', *, *, #14692, .F. ) ;
#65982 = EDGE_CURVE ( 'NONE', #34547, #4261, #60042, .T. ) ;
#65983 = SURFACE_STYLE_USAGE ( .BOTH. , #60014 ) ;
#65984 = ADVANCED_FACE ( 'NONE', ( #66010 ), #33653, .F. ) ;
#65985 = PRESENTATION_STYLE_ASSIGNMENT (( #64938 ) ) ;
#65986 = ORIENTED_EDGE ( 'NONE', *, *, #40775, .T. ) ;
#65987 = CARTESIAN_POINT ( 'NONE',  ( -9.827790563157511022E-16, 160.4429263765338192, 8.025000000000000355 ) ) ;
#65988 = DIRECTION ( 'NONE',  ( 0.000000000000000000, 0.000000000000000000, -1.000000000000000000 ) ) ;
#65989 = AXIS2_PLACEMENT_3D ( 'NONE', #66285, #44877, #53996 ) ;
#65990 = EDGE_CURVE ( 'NONE', #6607, #59022, #17747, .T. ) ;
#65991 = VECTOR ( 'NONE', #10550, 1000.000000000000000 ) ;
#65992 = ADVANCED_FACE ( 'NONE', ( #12533 ), #22409, .T. ) ;
#65993 = EDGE_LOOP ( 'NONE', ( #42996, #44721, #50861 ) ) ;
#65994 = CARTESIAN_POINT ( 'NONE',  ( 35.99999999999999289, 0.000000000000000000, 72.00402776293825013 ) ) ;
#65995 = EDGE_CURVE ( 'NONE', #14584, #7763, #41051, .T. ) ;
#65996 = VERTEX_POINT ( 'NONE', #9016 ) ;
#65997 = DIRECTION ( 'NONE',  ( 1.000000000000000000, 0.000000000000000000, 0.000000000000000000 ) ) ;
#65998 = FACE_OUTER_BOUND ( 'NONE', #10876, .T. ) ;
#65999 = CARTESIAN_POINT ( 'NONE',  ( -176.4570736234661865, -9.058813317711329915, 2.943386871421371787 ) ) ;
#66000 = ADVANCED_FACE ( 'NONE', ( #40699 ), #16662, .T. ) ;
#66001 = SURFACE_SIDE_STYLE ('',( #64014 ) ) ;
#66002 = SURFACE_STYLE_USAGE ( .BOTH. , #55452 ) ;
#66003 = CARTESIAN_POINT ( 'NONE',  ( -110.6070736234661780, -8.102448949553172852, 5.886773742842742685 ) ) ;
#66004 = DIRECTION ( 'NONE',  ( 1.000000000000000000, 0.000000000000000000, 0.000000000000000000 ) ) ;
#66005 = EDGE_CURVE ( 'NONE', #5374, #32655, #8744, .T. ) ;
#66006 = DIRECTION ( 'NONE',  ( -0.000000000000000000, 1.000000000000000000, -0.000000000000000000 ) ) ;
#66007 = ORIENTED_EDGE ( 'NONE', *, *, #57205, .F. ) ;
#66008 = CARTESIAN_POINT ( 'NONE',  ( 8.437984349512095861, 122.1929263765337907, 1.550032578732816828E-15 ) ) ;
#66009 = SURFACE_STYLE_FILL_AREA ( #2978 ) ;
#66010 = FACE_OUTER_BOUND ( 'NONE', #41560, .T. ) ;
#66011 = ORIENTED_EDGE ( 'NONE', *, *, #5371, .F. ) ;
#66012 = CARTESIAN_POINT ( 'NONE',  ( -156.2050000000000125, -2.607480562269071545, -8.024999999999991473 ) ) ;
#66013 = LINE ( 'NONE', #17840, #15654 ) ;
#66014 = CARTESIAN_POINT ( 'NONE',  ( -171.8949999999999534, 6.826472737025116366, 4.959722759717898555 ) ) ;
#66015 = CARTESIAN_POINT ( 'NONE',  ( -154.3449999999999704, 7.632228543268599452, -2.479861379858951942 ) ) ;
#66016 =( BOUNDED_CURVE ( )  B_SPLINE_CURVE ( 2, ( #51661, #51314, #28800, #7695, #19643, #45037, #3416, #18263, #67483, #34771, #18930 ),
 .UNSPECIFIED., .F., .F. ) 
 B_SPLINE_CURVE_WITH_KNOTS ( ( 3, 2, 2, 2, 2, 3 ),
 ( 0.4239130434782509282, 0.4260869565217291211, 0.4282608695652073694, 0.4304347826086855622, 0.4326086956521637550, 0.4347826086956419478 ),
 .UNSPECIFIED. ) 
 CURVE ( )  GEOMETRIC_REPRESENTATION_ITEM ( )  RATIONAL_B_SPLINE_CURVE ( ( 1.000000000000223821, 0.9510565162949298212, 1.000000000000000000, 0.9510565162951535312, 1.000000000000000000, 0.9510565162951535312, 1.000000000000000000, 0.9510565162951535312, 1.000000000000000000, 0.9510565162953834584, 0.9999999999997700728 ) ) 
 REPRESENTATION_ITEM ( '' )  );
#66017 = ORIENTED_EDGE ( 'NONE', *, *, #186, .F. ) ;
#66018 = CARTESIAN_POINT ( 'NONE',  ( -89.69292637653379074, 10.01517768586948698, -1.839758294383808966E-15 ) ) ;
#66019 = AXIS2_PLACEMENT_3D ( 'NONE', #18183, #64974, #881 ) ;
#66020 = PRESENTATION_STYLE_ASSIGNMENT (( #49868 ) ) ;
#66021 = CARTESIAN_POINT ( 'NONE',  ( -75.95499999999998408, -7.632228543268599452, 2.479861379858951054 ) ) ;
#66022 = CARTESIAN_POINT ( 'NONE',  ( -38.83454371628977242, -13.12359704688498141, 1.007153542399198409 ) ) ;
#66023 = PRESENTATION_LAYER_ASSIGNMENT (  '', '', ( #819 ) ) ;
#66024 = AXIS2_PLACEMENT_3D ( 'NONE', #7965, #56494, #30098 ) ;
#66025 = CARTESIAN_POINT ( 'NONE',  ( -71.09499999999998465, -2.607480562269071545, -8.024999999999991473 ) ) ;
#66026 = CARTESIAN_POINT ( 'NONE',  ( 8.102448949553181734, 151.5049999999999955, 5.886773742842750679 ) ) ;
#66027 = CARTESIAN_POINT ( 'NONE',  ( -3.414270897523325132, 1.730686724747263705, -7.000000000000004441 ) ) ;
#66028 = PRODUCT_DEFINITION_SHAPE ( 'NONE', 'NONE',  #69719 ) ;
#66029 = CARTESIAN_POINT ( 'NONE',  ( 2.128399401614408669E-13, 154.1464374838464266, 9.171437483846471395 ) ) ;
#66030 = ADVANCED_FACE ( 'NONE', ( #2641 ), #67066, .T. ) ;
#66031 = DIRECTION ( 'NONE',  ( 0.000000000000000000, 0.000000000000000000, -1.000000000000000000 ) ) ;
#66032 = DIRECTION ( 'NONE',  ( 1.000000000000000000, 0.000000000000000000, 0.000000000000000000 ) ) ;
#66033 = AXIS2_PLACEMENT_3D ( 'NONE', #2837, #29250, #7471 ) ;
#66034 = AXIS2_PLACEMENT_3D ( 'NONE', #25851, #24452, #20227 ) ;
#66035 = DIRECTION ( 'NONE',  ( -0.8946296187927070820, 0.000000000000000000, 0.4468085106382997385 ) ) ;
#66036 = DIRECTION ( 'NONE',  ( -1.000000000000000000, 0.000000000000000000, 0.000000000000000000 ) ) ;
#66037 = DIRECTION ( 'NONE',  ( 0.000000000000000000, 0.000000000000000000, 1.000000000000000000 ) ) ;
#66038 = ORIENTED_EDGE ( 'NONE', *, *, #12469, .T. ) ;
#66039 = VERTEX_POINT ( 'NONE', #61749 ) ;
#66040 = SURFACE_STYLE_FILL_AREA ( #59121 ) ;
#66041 = DIRECTION ( 'NONE',  ( 0.000000000000000000, 0.000000000000000000, -1.000000000000000000 ) ) ;
#66042 = CARTESIAN_POINT ( 'NONE',  ( 57.00000000000000000, 14.00000000000000000, 60.00402776293825724 ) ) ;
#66043 = CARTESIAN_POINT ( 'NONE',  ( 0.000000000000000000, 0.000000000000000000, 0.000000000000000000 ) ) ;
#66044 = EDGE_LOOP ( 'NONE', ( #37302, #58780, #60078, #65789 ) ) ;
#66045 = CARTESIAN_POINT ( 'NONE',  ( -109.8549999999999898, 4.716976649647094177, 6.492361379858945902 ) ) ;
#66046 = ORIENTED_EDGE ( 'NONE', *, *, #4109, .F. ) ;
#66047 = FILL_AREA_STYLE ('',( #33021 ) ) ;
#66048 = EDGE_CURVE ( 'NONE', #49280, #45911, #39160, .T. ) ;
#66049 = ORIENTED_EDGE ( 'NONE', *, *, #34227, .F. ) ;
#66050 = DIRECTION ( 'NONE',  ( 0.000000000000000000, 0.000000000000000000, 1.000000000000000000 ) ) ;
#66051 = VERTEX_POINT ( 'NONE', #35407 ) ;
#66052 = CARTESIAN_POINT ( 'NONE',  ( 24.00000000000000000, -2.250452076942884869E-15, 4.000000000000000000 ) ) ;
#66053 = DIRECTION ( 'NONE',  ( -1.000000000000000000, 0.000000000000000000, 0.000000000000000000 ) ) ;
#66054 = EDGE_LOOP ( 'NONE', ( #46394, #38758, #10947, #20044, #68530, #52347, #26935, #40601, #67531, #39220 ) ) ;
#66055 = EDGE_CURVE ( 'NONE', #25561, #11136, #9917, .T. ) ;
#66056 = ORIENTED_EDGE ( 'NONE', *, *, #25271, .T. ) ;
#66057 = FACE_OUTER_BOUND ( 'NONE', #26839, .T. ) ;
#66058 = CARTESIAN_POINT ( 'NONE',  ( -51.44292637653380496, -1.166476076187852838E-15, -9.524999999999991473 ) ) ;
#66059 = CARTESIAN_POINT ( 'NONE',  ( -75.75000000000000000, -0.9999999999999995559, 19.00000000000000000 ) ) ;
#66060 = DIRECTION ( 'NONE',  ( 0.000000000000000000, -0.000000000000000000, -1.000000000000000000 ) ) ;
#66061 = ORIENTED_EDGE ( 'NONE', *, *, #47807, .F. ) ;
#66062 = CARTESIAN_POINT ( 'NONE',  ( 4.716976649647096842, 139.7429263765338305, 6.492361379858953896 ) ) ;
#66063 = DIRECTION ( 'NONE',  ( 0.000000000000000000, 0.000000000000000000, 1.000000000000000000 ) ) ;
#66064 = PRESENTATION_STYLE_ASSIGNMENT (( #1977 ) ) ;
#66065 = VECTOR ( 'NONE', #69050, 1000.000000000000000 ) ;
#66066 = VECTOR ( 'NONE', #35670, 1000.000000000000000 ) ;
#66067 =( NAMED_UNIT ( * ) PLANE_ANGLE_UNIT ( ) SI_UNIT ( $, .RADIAN. ) );
#66068 = DIRECTION ( 'NONE',  ( 0.000000000000000000, 0.000000000000000000, 1.000000000000000000 ) ) ;
#66069 = VERTEX_POINT ( 'NONE', #8669 ) ;
#66070 =( NAMED_UNIT ( * ) PLANE_ANGLE_UNIT ( ) SI_UNIT ( $, .RADIAN. ) );
#66071 = ADVANCED_FACE ( 'NONE', ( #62465 ), #64912, .T. ) ;
#66072 = VERTEX_POINT ( 'NONE', #46701 ) ;
#66073 = CARTESIAN_POINT ( 'NONE',  ( 31.00000000000001421, 43.00000000000000000, 36.49999999999999289 ) ) ;
#66074 = DIRECTION ( 'NONE',  ( 0.000000000000000000, 0.000000000000000000, -1.000000000000000000 ) ) ;
#66076 = CIRCLE ( 'NONE', #14408, 1.000000000000000888 ) ;
#66075 = DIRECTION ( 'NONE',  ( 0.000000000000000000, -1.000000000000000000, 0.000000000000000000 ) ) ;
#66077 = CARTESIAN_POINT ( 'NONE',  ( -129.2049999999999841, -2.607480562269071545, -8.024999999999991473 ) ) ;
#66078 = CARTESIAN_POINT ( 'NONE',  ( 25.00000000000001421, 43.00000000000000000, -34.49999999999999289 ) ) ;
#66079 = EDGE_LOOP ( 'NONE', ( #59285, #31006, #39802, #39147, #13100, #66418 ) ) ;
#66080 =( GEOMETRIC_REPRESENTATION_CONTEXT ( 3 ) GLOBAL_UNCERTAINTY_ASSIGNED_CONTEXT ( ( #49484 ) ) GLOBAL_UNIT_ASSIGNED_CONTEXT ( ( #14337, #2333, #47811 ) ) REPRESENTATION_CONTEXT ( 'NONE', 'WORKASPACE' ) );
#66081 = LINE ( 'NONE', #49238, #66603 ) ;
#66082 = ADVANCED_FACE ( 'NONE', ( #12892 ), #14282, .T. ) ;
#66083 = DIRECTION ( 'NONE',  ( 0.000000000000000000, 0.000000000000000000, -1.000000000000000000 ) ) ;
#66084 = CARTESIAN_POINT ( 'NONE',  ( 31.00000000000001421, 43.00000000000000000, 36.50000000000000000 ) ) ;
#66085 = ORIENTED_EDGE ( 'NONE', *, *, #9003, .F. ) ;
#66086 = VECTOR ( 'NONE', #15529, 1000.000000000000000 ) ;
#66087 = ORIENTED_EDGE ( 'NONE', *, *, #30604, .T. ) ;
#66088 = CARTESIAN_POINT ( 'NONE',  ( -45.21668476461162811, 8.382617247524210669, 3.000000000000000444 ) ) ;
#66089 = DIRECTION ( 'NONE',  ( -1.000000000000000000, 0.000000000000000000, 0.000000000000000000 ) ) ;
#66090 = ORIENTED_EDGE ( 'NONE', *, *, #5314, .T. ) ;
#66091 = CARTESIAN_POINT ( 'NONE',  ( -12.72792206135785698, 149.9999999999999716, -10.00000000000000000 ) ) ;
#66092 = DIRECTION ( 'NONE',  ( 0.000000000000000000, 0.000000000000000000, 1.000000000000000000 ) ) ;
#66093 = DIRECTION ( 'NONE',  ( 1.000000000000000000, 0.000000000000000000, 0.000000000000000000 ) ) ;
#66094 = CARTESIAN_POINT ( 'NONE',  ( -182.8449999999999989, -7.632228543268599452, 2.479861379858951054 ) ) ;
#66095 = ORIENTED_EDGE ( 'NONE', *, *, #43481, .T. ) ;
#66096 = SURFACE_SIDE_STYLE ('',( #69406 ) ) ;
#66098 = MECHANICAL_DESIGN_GEOMETRIC_PRESENTATION_REPRESENTATION (  '', ( #14434 ), #24500 ) ;
#66097 = CARTESIAN_POINT ( 'NONE',  ( -144.9570736234661865, 9.058813317711329915, -2.943386871421373119 ) ) ;
#66099 = CARTESIAN_POINT ( 'NONE',  ( -6.887213563469350319, 2.329718218673038077, -6.070996185493596542 ) ) ;
#66100 = SURFACE_SIDE_STYLE ('',( #17611 ) ) ;
#66101 = DIRECTION ( 'NONE',  ( 0.000000000000000000, 0.000000000000000000, 1.000000000000000000 ) ) ;
#66102 = CARTESIAN_POINT ( 'NONE',  ( -95.39499999999999602, -6.826472737025113702, -4.959722759717900331 ) ) ;
#66103 = CARTESIAN_POINT ( 'NONE',  ( 8.102448949553183510, 119.1049999999999756, -5.886773742842746238 ) ) ;
#66104 = CARTESIAN_POINT ( 'NONE',  ( -82.49499999999997613, 6.826472737025113702, -4.959722759717902107 ) ) ;
#66105 = DIRECTION ( 'NONE',  ( -1.000000000000000000, 0.000000000000000000, 1.300977106640434891E-16 ) ) ;
#66106 = VECTOR ( 'NONE', #13808, 1000.000000000000000 ) ;
#66107 = DIRECTION ( 'NONE',  ( 0.000000000000000000, 0.000000000000000000, -1.000000000000000000 ) ) ;
#66108 = DIRECTION ( 'NONE',  ( 1.000000000000000000, 0.000000000000000000, 0.000000000000000000 ) ) ;
#66109 = CIRCLE ( 'NONE', #54853, 1.000000000000000888 ) ;
#66110 =( BOUNDED_SURFACE ( )  B_SPLINE_SURFACE ( 3, 2, ( 
 ( #57363, #8501, #56674 ),
 ( #29932, #67938, #20419 ),
 ( #41556, #41923, #30610 ),
 ( #9190, #15187, #57012 ),
 ( #58073, #3497, #36653 ),
 ( #52113, #26025, #68974 ),
 ( #25350, #51394, #3141 ),
 ( #24632, #67573, #40874 ),
 ( #62293, #8827, #25000 ),
 ( #30253, #51755, #46509 ) ),
 .UNSPECIFIED., .F., .F., .T. ) 
 B_SPLINE_SURFACE_WITH_KNOTS ( ( 4, 2, 2, 2, 4 ),
 ( 3, 3 ),
 ( 4.712388980384689674, 5.105088062083414258, 5.497787143782137953, 5.890486225480861648, 6.283185307179586232 ),
 ( 0.000000000000000000, 1.000000000000000000 ),
 .UNSPECIFIED. ) 
 GEOMETRIC_REPRESENTATION_ITEM ( )  RATIONAL_B_SPLINE_SURFACE ( (
 ( 1.000000000000000000, 0.7071067811865482389, 1.000000000000000000),
 ( 1.000000000000000000, 0.7217502572880009071, 1.000000000000000000),
 ( 1.000000000000000000, 0.7359001690391617778, 1.000000000000000000),
 ( 1.000000000000000000, 0.7614408922481175068, 1.000000000000000000),
 ( 1.000000000000000000, 0.7728233248393500121, 1.000000000000000000),
 ( 1.000000000000000000, 0.7915339219236553481, 1.000000000000000000),
 ( 1.000000000000000000, 0.7988629633398777186, 1.000000000000000000),
 ( 1.000000000000000000, 0.8087168080150187732, 1.000000000000000000),
 ( 1.000000000000000000, 0.8112499556556335145, 1.000000000000000000),
 ( 1.000000000000000000, 0.8112421851755602376, 1.000000000000000000) ) ) 
 REPRESENTATION_ITEM ( '' )  SURFACE ( )  );
#66111 = EDGE_CURVE ( 'NONE', #45247, #9929, #24818, .T. ) ;
#66112 = DIRECTION ( 'NONE',  ( -0.000000000000000000, 0.000000000000000000, 1.000000000000000000 ) ) ;
#66113 = DIRECTION ( 'NONE',  ( 0.000000000000000000, 1.000000000000000000, -0.000000000000000000 ) ) ;
#66114 = ORIENTED_EDGE ( 'NONE', *, *, #33297, .F. ) ;
#66115 = CARTESIAN_POINT ( 'NONE',  ( -125.6929263765338192, 10.01517768586948698, -1.839758294383808571E-15 ) ) ;
#66116 = CARTESIAN_POINT ( 'NONE',  ( -137.3950000000000102, -6.826472737025115478, -4.959722759717899443 ) ) ;
#66117 = ADVANCED_FACE ( 'NONE', ( #35748 ), #2264, .F. ) ;
#66118 = CARTESIAN_POINT ( 'NONE',  ( 23.50000000000001776, 42.00000000000000000, 29.68999999999999417 ) ) ;
#66119 = STYLED_ITEM ( 'NONE', ( #32213 ), #51092 ) ;
#66120 = EDGE_CURVE ( 'NONE', #9275, #64306, #40045, .T. ) ;
#66121 = DIRECTION ( 'NONE',  ( 1.000000000000000000, 0.000000000000000000, 0.000000000000000000 ) ) ;
#66122 = FACE_OUTER_BOUND ( 'NONE', #16023, .T. ) ;
#66123 = EDGE_LOOP ( 'NONE', ( #31110, #44317, #28219, #23153 ) ) ;
#66124 = CIRCLE ( 'NONE', #30162, 0.4999999999999994449 ) ;
#66125 = ORIENTED_EDGE ( 'NONE', *, *, #20001, .T. ) ;
#66126 = CARTESIAN_POINT ( 'NONE',  ( -18.25000000000000711, 0.000000000000000000, 3.750000000000000000 ) ) ;
#66127 = DIRECTION ( 'NONE',  ( 1.000000000000000000, -0.000000000000000000, -0.000000000000000000 ) ) ;
#66128 = DIRECTION ( 'NONE',  ( 1.000000000000000000, 0.000000000000000000, 0.000000000000000000 ) ) ;
#66129 = CIRCLE ( 'NONE', #37027, 3.100000000000005418 ) ;
#66130 = CARTESIAN_POINT ( 'NONE',  ( 23.50000000000001776, 15.00000000000000000, -29.68999999999999417 ) ) ;
#66131 = VERTEX_POINT ( 'NONE', #8330 ) ;
#66132 = CARTESIAN_POINT ( 'NONE',  ( -145.5549999999999784, 0.000000000000000000, 8.024999999999991473 ) ) ;
#66134 = EDGE_CURVE ( 'NONE', #29454, #28945, #820, .T. ) ;
#66133 = VERTEX_POINT ( 'NONE', #18532 ) ;
#66135 = EDGE_CURVE ( 'NONE', #62845, #35085, #29410, .T. ) ;
#66136 = EDGE_LOOP ( 'NONE', ( #47803, #60797, #48661 ) ) ;
#66137 = CARTESIAN_POINT ( 'NONE',  ( 0.000000000000000000, 152.9999999999999716, 0.000000000000000000 ) ) ;
#66138 = DIRECTION ( 'NONE',  ( -1.000000000000000000, 0.000000000000000000, 0.000000000000000000 ) ) ;
#66139 = EDGE_LOOP ( 'NONE', ( #45438, #36621, #13796, #36988 ) ) ;
#66140 = LINE ( 'NONE', #61541, #19228 ) ;
#66141 = FILL_AREA_STYLE ('',( #22555 ) ) ;
#66142 = CARTESIAN_POINT ( 'NONE',  ( 10.01517768586949231, 129.6949999999999648, 1.839758294383810543E-15 ) ) ;
#66143 = ORIENTED_EDGE ( 'NONE', *, *, #56790, .T. ) ;
#66144 = CARTESIAN_POINT ( 'NONE',  ( 21.25000000000000711, 22.24999999999998224, -4.000000000000000000 ) ) ;
#66146 = EDGE_CURVE ( 'NONE', #19166, #52175, #58203, .T. ) ;
#66145 = CARTESIAN_POINT ( 'NONE',  ( -3.094860106618434248, 141.9050000000000011, 9.525000000000000355 ) ) ;
#66147 = CARTESIAN_POINT ( 'NONE',  ( -53.00499999999999545, 6.826472737025115478, 4.959722759717899443 ) ) ;
#66148 = VECTOR ( 'NONE', #66821, 1000.000000000000000 ) ;
#66149 =( NAMED_UNIT ( * ) PLANE_ANGLE_UNIT ( ) SI_UNIT ( $, .RADIAN. ) );
#66150 = ORIENTED_EDGE ( 'NONE', *, *, #64239, .T. ) ;
#66151 = CARTESIAN_POINT ( 'NONE',  ( 10.01517768586949231, 157.8050000000000068, 1.839758294383810543E-15 ) ) ;
#66152 = DIRECTION ( 'NONE',  ( 0.000000000000000000, 0.000000000000000000, 1.000000000000000000 ) ) ;
#66153 = DIRECTION ( 'NONE',  ( 1.000000000000000000, -0.000000000000000000, -0.000000000000000000 ) ) ;
#66154 = ADVANCED_FACE ( 'NONE', ( #52298 ), #5107, .T. ) ;
#66155 = VECTOR ( 'NONE', #59602, 1000.000000000000000 ) ;
#66156 = DIRECTION ( 'NONE',  ( 1.000000000000000000, 0.000000000000000000, 0.000000000000000000 ) ) ;
#66157 = DIRECTION ( 'NONE',  ( -1.000000000000000000, -1.224646799147353454E-16, 0.000000000000000000 ) ) ;
#66158 = ORIENTED_EDGE ( 'NONE', *, *, #38697, .F. ) ;
#66159 = EDGE_CURVE ( 'NONE', #44595, #68002, #42450, .T. ) ;
#66160 = EDGE_LOOP ( 'NONE', ( #47526, #49651, #39906, #65018 ) ) ;
#66161 = FILL_AREA_STYLE ('',( #2076 ) ) ;
#66162 = VECTOR ( 'NONE', #69282, 1000.000000000000000 ) ;
#66163 = CARTESIAN_POINT ( 'NONE',  ( 20.05202421861157447, 114.9999999999999432, 10.44839000960907960 ) ) ;
#66164 = CARTESIAN_POINT ( 'NONE',  ( 15.98999599679679839, 118.4999999999999716, 9.500000000000000000 ) ) ;
#66165 = CARTESIAN_POINT ( 'NONE',  ( -163.7049999999999841, 2.607480562269073321, 8.024999999999991473 ) ) ;
#66166 = ORIENTED_EDGE ( 'NONE', *, *, #58070, .F. ) ;
#66167 = DIRECTION ( 'NONE',  ( 0.000000000000000000, -1.000000000000000000, 0.000000000000000000 ) ) ;
#66168 = FILL_AREA_STYLE ('',( #39143 ) ) ;
#66169 = ADVANCED_FACE ( 'NONE', ( #63844 ), #10061, .T. ) ;
#66170 = PRESENTATION_STYLE_ASSIGNMENT (( #55272 ) ) ;
#66171 = SURFACE_STYLE_FILL_AREA ( #2452 ) ;
#66172 = ORIENTED_EDGE ( 'NONE', *, *, #25967, .F. ) ;
#66173 = COLOUR_RGB ( '', 0.72549020, 0.75294118, 0.79215686) ;
#66174 = ORIENTED_EDGE ( 'NONE', *, *, #35110, .T. ) ;
#66175 = CARTESIAN_POINT ( 'NONE',  ( -44.99928706149596280, 9.682046777738220200, -3.525278482175732808 ) ) ;
#66176 = CARTESIAN_POINT ( 'NONE',  ( 27.00000000000001776, 15.00000000000000000, 29.68999999999999417 ) ) ;
#66177 = CARTESIAN_POINT ( 'NONE',  ( -74.30499999999996419, 8.437984349512085203, -1.550032578732815448E-15 ) ) ;
#66178 = ORIENTED_EDGE ( 'NONE', *, *, #23418, .T. ) ;
#66179 = CARTESIAN_POINT ( 'NONE',  ( -71.75000000000000000, -3.000000000000000000, 18.00000000000000000 ) ) ;
#66180 = CIRCLE ( 'NONE', #32474, 0.7499999999999997780 ) ;
#66181 = DIRECTION ( 'NONE',  ( -0.000000000000000000, -0.000000000000000000, 1.000000000000000000 ) ) ;
#66182 = DIRECTION ( 'NONE',  ( -1.000000000000000000, 0.000000000000000000, 0.000000000000000000 ) ) ;
#66183 = VECTOR ( 'NONE', #46958, 1000.000000000000000 ) ;
#66184 = DIRECTION ( 'NONE',  ( -1.000000000000000000, 0.000000000000000000, 0.000000000000000000 ) ) ;
#66185 = EDGE_LOOP ( 'NONE', ( #61648, #63816, #58162, #68219 ) ) ;
#66186 = PLANE ( 'NONE',  #49502 ) ;
#66187 = VECTOR ( 'NONE', #32904, 1000.000000000000000 ) ;
#66188 = CARTESIAN_POINT ( 'NONE',  ( -13.75000000000000533, 30.99999999999999289, 3.750000000000000000 ) ) ;
#66189 = CARTESIAN_POINT ( 'NONE',  ( -9.058813317711337021, 140.0449999999999875, -2.943386871421374895 ) ) ;
#66190 = CARTESIAN_POINT ( 'NONE',  ( -111.4449999999999932, 0.000000000000000000, 8.024999999999991473 ) ) ;
#66191 = FACE_OUTER_BOUND ( 'NONE', #16275, .T. ) ;
#66192 = EDGE_CURVE ( 'NONE', #7834, #14638, #20245, .T. ) ;
#66193 = CARTESIAN_POINT ( 'NONE',  ( -96.35707362346616378, 5.598654528085804216, 7.705886871421366635 ) ) ;
#66194 = AXIS2_PLACEMENT_3D ( 'NONE', #10672, #31, #21566 ) ;
#66195 = CARTESIAN_POINT ( 'NONE',  ( -149.3929263765338078, 8.102448949553176405, 5.886773742842740909 ) ) ;
#66196 = CARTESIAN_POINT ( 'NONE',  ( -170.2450000000000045, -4.716976649647093289, -6.492361379858945902 ) ) ;
#66197 = CIRCLE ( 'NONE', #3247, 1.000000000000000888 ) ;
#66198 = SURFACE_SIDE_STYLE ('',( #60922 ) ) ;
#66199 = CIRCLE ( 'NONE', #51599, 0.5000000000000004441 ) ;
#66200 = VECTOR ( 'NONE', #65302, 1000.000000000000000 ) ;
#66201 = CARTESIAN_POINT ( 'NONE',  ( -9.250000000000003553, 0.000000000000000000, 4.000000000000000000 ) ) ;
#66202 = ORIENTED_EDGE ( 'NONE', *, *, #51714, .T. ) ;
#66203 = ORIENTED_EDGE ( 'NONE', *, *, #25721, .T. ) ;
#66204 = CARTESIAN_POINT ( 'NONE',  ( -71.09292637653381064, 3.094860106618433360, 9.524999999999991473 ) ) ;
#66205 = CIRCLE ( 'NONE', #7815, 0.2500000000000002220 ) ;
#66206 = CIRCLE ( 'NONE', #50512, 0.2500000000000002220 ) ;
#66207 = DIRECTION ( 'NONE',  ( -0.000000000000000000, -1.000000000000000000, -0.000000000000000000 ) ) ;
#66208 = ADVANCED_FACE ( 'NONE', ( #37171 ), #57905, .T. ) ;
#66209 =( NAMED_UNIT ( * ) PLANE_ANGLE_UNIT ( ) SI_UNIT ( $, .RADIAN. ) );
#66210 = CARTESIAN_POINT ( 'NONE',  ( -141.7429263765338021, -5.598654528085803328, -7.705886871421366635 ) ) ;
#66211 = CARTESIAN_POINT ( 'NONE',  ( 3.250000000000003553, 4.698209414103854191E-16, 4.000000000000000000 ) ) ;
#66212 = AXIS2_PLACEMENT_3D ( 'NONE', #41420, #35069, #13604 ) ;
#66213 = EDGE_CURVE ( 'NONE', #373, #61874, #12137, .T. ) ;
#66214 = DIRECTION ( 'NONE',  ( 0.000000000000000000, 0.000000000000000000, 1.000000000000000000 ) ) ;
#66215 = ORIENTED_EDGE ( 'NONE', *, *, #33921, .T. ) ;
#66216 = CARTESIAN_POINT ( 'NONE',  ( -169.7049999999999841, 2.607480562269072433, 8.024999999999991473 ) ) ;
#66217 = EDGE_CURVE ( 'NONE', #16875, #63288, #53324, .T. ) ;
#66218 = EDGE_CURVE ( 'NONE', #9977, #58400, #37529, .T. ) ;
#66219 = ORIENTED_EDGE ( 'NONE', *, *, #32386, .T. ) ;
#66220 = ADVANCED_FACE ( 'NONE', ( #25519 ), #48076, .F. ) ;
#66221 = CARTESIAN_POINT ( 'NONE',  ( -112.9429263765338050, 0.000000000000000000, 9.524999999999991473 ) ) ;
#66222 = DIRECTION ( 'NONE',  ( 1.000000000000000000, 0.000000000000000000, -0.000000000000000000 ) ) ;
#66223 = CARTESIAN_POINT ( 'NONE',  ( 31.00000000000001421, 42.00000000000000000, 36.50000000000000000 ) ) ;
#66224 = STYLED_ITEM ( 'NONE', ( #5618 ), #15305 ) ;
#66225 = CARTESIAN_POINT ( 'NONE',  ( -7.632228543268608334, 148.9570736234661581, 2.479861379858952830 ) ) ;
#66226 = STYLED_ITEM ( 'NONE', ( #6079 ), #15907 ) ;
#66227 = EDGE_LOOP ( 'NONE', ( #22861, #49928, #66747, #39834 ) ) ;
#66228 = DIRECTION ( 'NONE',  ( 0.000000000000000000, 0.000000000000000000, -1.000000000000000000 ) ) ;
#66229 = CARTESIAN_POINT ( 'NONE',  ( 0.000000000000000000, 0.000000000000000000, 0.000000000000000000 ) ) ;
#66230 = CARTESIAN_POINT ( 'NONE',  ( -82.25499999999998124, -4.716976649647092401, 6.492361379858946790 ) ) ;
#66231 = CARTESIAN_POINT ( 'NONE',  ( -60.00000000000000000, -2.024042244987997205E-14, 9.500000000000000000 ) ) ;
#66232 = CARTESIAN_POINT ( 'NONE',  ( 3.094860106618435136, 131.4049999999999727, -9.525000000000000355 ) ) ;
#66233 =( GEOMETRIC_REPRESENTATION_CONTEXT ( 3 ) GLOBAL_UNCERTAINTY_ASSIGNED_CONTEXT ( ( #2286 ) ) GLOBAL_UNIT_ASSIGNED_CONTEXT ( ( #47305, #9651, #17275 ) ) REPRESENTATION_CONTEXT ( 'NONE', 'WORKASPACE' ) );
#66234 = DIRECTION ( 'NONE',  ( 0.000000000000000000, 1.000000000000000000, -0.000000000000000000 ) ) ;
#66235 = EDGE_CURVE ( 'NONE', #63288, #6972, #59271, .T. ) ;
#66236 = CARTESIAN_POINT ( 'NONE',  ( -73.40707362346617515, 3.094860106618428031, -9.524999999999993250 ) ) ;
#66237 =( NAMED_UNIT ( * ) PLANE_ANGLE_UNIT ( ) SI_UNIT ( $, .RADIAN. ) );
#66238 = CYLINDRICAL_SURFACE ( 'NONE', #32968, 0.2500000000000002220 ) ;
#66239 = FACE_OUTER_BOUND ( 'NONE', #3085, .T. ) ;
#66240 = ORIENTED_EDGE ( 'NONE', *, *, #4778, .T. ) ;
#66241 = CARTESIAN_POINT ( 'NONE',  ( 44.50000000000000000, -1.469576158976824618E-14, -4.000000000000000000 ) ) ;
#66242 =( GEOMETRIC_REPRESENTATION_CONTEXT ( 3 ) GLOBAL_UNCERTAINTY_ASSIGNED_CONTEXT ( ( #38958 ) ) GLOBAL_UNIT_ASSIGNED_CONTEXT ( ( #32581, #49487, #54392 ) ) REPRESENTATION_CONTEXT ( 'NONE', 'WORKASPACE' ) );
#66244 = CARTESIAN_POINT ( 'NONE',  ( -54.59499999999997044, 2.607480562269073321, 8.024999999999991473 ) ) ;
#66243 = VECTOR ( 'NONE', #46150, 1000.000000000000000 ) ;
#66245 = ORIENTED_EDGE ( 'NONE', *, *, #10360, .F. ) ;
#66246 = FILL_AREA_STYLE ('',( #12781 ) ) ;
#66247 = CARTESIAN_POINT ( 'NONE',  ( -44.99999999999999289, 8.547452476119513420, -5.556748833515239738 ) ) ;
#66248 = TOROIDAL_SURFACE ( 'NONE', #28010, 0.5000000000000000000, 0.2500000000000000000 ) ;
#66249 = ORIENTED_EDGE ( 'NONE', *, *, #33064, .T. ) ;
#66250 = CARTESIAN_POINT ( 'NONE',  ( -48.63607860962903828, -13.13395492442522539, 2.757111910427318513 ) ) ;
#66251 = CARTESIAN_POINT ( 'NONE',  ( -53.99499999999998323, -6.826472737025113702, 4.959722759717902107 ) ) ;
#66252 = ORIENTED_EDGE ( 'NONE', *, *, #49255, .F. ) ;
#66253 = CARTESIAN_POINT ( 'NONE',  ( -74.09161580380370538, 9.403326511829389389, 6.097699930223767772 ) ) ;
#66254 = CARTESIAN_POINT ( 'NONE',  ( -116.6049999999999756, 6.826472737025113702, -4.959722759717902107 ) ) ;
#66255 = VERTEX_POINT ( 'NONE', #21274 ) ;
#66256 = ADVANCED_FACE ( 'NONE', ( #42807 ), #41749, .T. ) ;
#66257 = CARTESIAN_POINT ( 'NONE',  ( 0.000000000000000000, 118.0570736234661524, -8.025000000000000355 ) ) ;
#66258 = VECTOR ( 'NONE', #30205, 1000.000000000000000 ) ;
#66259 = DIRECTION ( 'NONE',  ( 1.000000000000000000, 0.000000000000000000, 0.000000000000000000 ) ) ;
#66260 = VECTOR ( 'NONE', #54868, 1000.000000000000000 ) ;
#66261 = CARTESIAN_POINT ( 'NONE',  ( -151.5570736234661808, -1.166476076187852838E-15, -9.524999999999991473 ) ) ;
#66262 = EDGE_CURVE ( 'NONE', #49593, #11358, #30111, .T. ) ;
#66263 = VECTOR ( 'NONE', #16601, 1000.000000000000000 ) ;
#66264 = CARTESIAN_POINT ( 'NONE',  ( -58.70707362346615810, -3.094860106618431139, -9.524999999999991473 ) ) ;
#66265 = CARTESIAN_POINT ( 'NONE',  ( 5.598654528085809545, 139.1449999999999818, -7.705886871421373741 ) ) ;
#66266 = CARTESIAN_POINT ( 'NONE',  ( -85.85707362346617799, -5.598654528085803328, -7.705886871421366635 ) ) ;
#66267 = CARTESIAN_POINT ( 'NONE',  ( 4.041451884327376121, 7.000000000000007105, 7.500000000000000000 ) ) ;
#66268 = ORIENTED_EDGE ( 'NONE', *, *, #20569, .T. ) ;
#66269 = VECTOR ( 'NONE', #8276, 1000.000000000000000 ) ;
#66270 = CARTESIAN_POINT ( 'NONE',  ( 28.00000000000002842, 5.569094604152798667, -2.026984667724098355 ) ) ;
#66272 =( LENGTH_UNIT ( ) NAMED_UNIT ( * ) SI_UNIT ( .MILLI., .METRE. ) );
#66271 = CARTESIAN_POINT ( 'NONE',  ( -20.57648123223228254, 110.4999999999999858, -10.27659574468085069 ) ) ;
#66273 = DIRECTION ( 'NONE',  ( 1.000000000000000000, 0.000000000000000000, -0.000000000000000000 ) ) ;
#66274 = CARTESIAN_POINT ( 'NONE',  ( -134.9050000000000011, 2.607480562269068880, -8.024999999999993250 ) ) ;
#66275 = DIRECTION ( 'NONE',  ( -1.000000000000000000, 0.000000000000000000, 0.000000000000000000 ) ) ;
#66276 = CARTESIAN_POINT ( 'NONE',  ( -45.00000000000000000, -1.469576158976824302E-14, 10.00000000000000000 ) ) ;
#66277 = DIRECTION ( 'NONE',  ( 0.000000000000000000, 1.000000000000000000, 0.000000000000000000 ) ) ;
#66278 = CARTESIAN_POINT ( 'NONE',  ( -136.6449999999999818, 4.716976649647091513, -6.492361379858946790 ) ) ;
#66279 = CARTESIAN_POINT ( 'NONE',  ( -130.0449999999999875, 7.632228543268600340, 2.479861379858949277 ) ) ;
#66280 = DIRECTION ( 'NONE',  ( -0.000000000000000000, 0.000000000000000000, -1.000000000000000000 ) ) ;
#66281 = ORIENTED_EDGE ( 'NONE', *, *, #38007, .F. ) ;
#66282 =( GEOMETRIC_REPRESENTATION_CONTEXT ( 3 ) GLOBAL_UNCERTAINTY_ASSIGNED_CONTEXT ( ( #42566 ) ) GLOBAL_UNIT_ASSIGNED_CONTEXT ( ( #44030, #6674, #7034 ) ) REPRESENTATION_CONTEXT ( 'NONE', 'WORKASPACE' ) );
#66283 = DIRECTION ( 'NONE',  ( -0.000000000000000000, -1.000000000000000000, -0.000000000000000000 ) ) ;
#66284 = PRESENTATION_LAYER_ASSIGNMENT (  '', '', ( #30308 ) ) ;
#66285 = CARTESIAN_POINT ( 'NONE',  ( -15.98999599679679839, 146.4999999999999716, -7.000000000000000000 ) ) ;
#66286 = CARTESIAN_POINT ( 'NONE',  ( -181.9429263765338192, 0.000000000000000000, 9.524999999999991473 ) ) ;
#66287 = VECTOR ( 'NONE', #69573, 1000.000000000000000 ) ;
#66288 = DIRECTION ( 'NONE',  ( 0.000000000000000000, 0.000000000000000000, -1.000000000000000000 ) ) ;
#66289 = CARTESIAN_POINT ( 'NONE',  ( 10.00000000000001776, 17.78868675966041835, -1.300977106640437060E-15 ) ) ;
#66290 = CARTESIAN_POINT ( 'NONE',  ( -6.062177826491069510, -2.500000000000000000, 3.499999999999999556 ) ) ;
#66291 =( NAMED_UNIT ( * ) PLANE_ANGLE_UNIT ( ) SI_UNIT ( $, .RADIAN. ) );
#66292 = EDGE_CURVE ( 'NONE', #9509, #51977, #38005, .T. ) ;
#66293 = CARTESIAN_POINT ( 'NONE',  ( 45.00000000000000000, 9.999999999999980460, 4.000000000000000000 ) ) ;
#66294 = DIRECTION ( 'NONE',  ( 0.000000000000000000, 1.000000000000000000, 0.000000000000000000 ) ) ;
#66295 = VECTOR ( 'NONE', #47826, 1000.000000000000000 ) ;
#66296 = CARTESIAN_POINT ( 'NONE',  ( -96.89292637653379359, -8.102448949553172852, -5.886773742842741797 ) ) ;
#66297 = APPLICATION_PROTOCOL_DEFINITION ( 'draft international standard', 'automotive_design', 1998, #31147 ) ;
#66298 = CYLINDRICAL_SURFACE ( 'NONE', #12113, 0.2500000000000002220 ) ;
#66299 = CARTESIAN_POINT ( 'NONE',  ( -75.48275862068965125, 63.99167409976910648, 6.499999999999999112 ) ) ;
#66300 = VECTOR ( 'NONE', #31236, 1000.000000000000000 ) ;
#66301 = EDGE_CURVE ( 'NONE', #64454, #60681, #68558, .T. ) ;
#66302 = PRESENTATION_STYLE_ASSIGNMENT (( #23391 ) ) ;
#66303 = CARTESIAN_POINT ( 'NONE',  ( -41.68104242135606796, 107.4439537334013437, 3.570039632082458336 ) ) ;
#66304 = DIRECTION ( 'NONE',  ( 1.000000000000000000, 0.000000000000000000, 0.000000000000000000 ) ) ;
#66305 = EDGE_CURVE ( 'NONE', #6097, #19233, #14643, .T. ) ;
#66306 = ORIENTED_EDGE ( 'NONE', *, *, #35267, .F. ) ;
#66307 = CYLINDRICAL_SURFACE ( 'NONE', #45400, 5.000000000000004441 ) ;
#66308 = CARTESIAN_POINT ( 'NONE',  ( 23.71231517720798010, 112.4999999999999858, 10.00000000000000000 ) ) ;
#66309 = VERTEX_POINT ( 'NONE', #63171 ) ;
#66310 = DIRECTION ( 'NONE',  ( 0.000000000000000000, 0.000000000000000000, 1.000000000000000000 ) ) ;
#66311 = CARTESIAN_POINT ( 'NONE',  ( -4.716976649647098618, 122.2570736234661553, 6.492361379858953008 ) ) ;
#66313 = VECTOR ( 'NONE', #42829, 1000.000000000000000 ) ;
#66312 = LINE ( 'NONE', #61032, #58588 ) ;
#66314 = SURFACE_STYLE_USAGE ( .BOTH. , #66678 ) ;
#66315 = COLOUR_RGB ( '', 0.66274510, 0.83137255, 0.94901961) ;
#66316 = CARTESIAN_POINT ( 'NONE',  ( 34.99999999999999289, 99.99999999999998579, 7.000000000000000000 ) ) ;
#66317 = ORIENTED_EDGE ( 'NONE', *, *, #46685, .T. ) ;
#66318 = CARTESIAN_POINT ( 'NONE',  ( 10.00000000000001954, 50.00000000000000000, 46.00000000000000000 ) ) ;
#66319 = EDGE_CURVE ( 'NONE', #4746, #38702, #4389, .T. ) ;
#66320 =( NAMED_UNIT ( * ) PLANE_ANGLE_UNIT ( ) SI_UNIT ( $, .RADIAN. ) );
#66321 = DIRECTION ( 'NONE',  ( 0.000000000000000000, -1.000000000000000000, 0.000000000000000000 ) ) ;
#66322 = FACE_OUTER_BOUND ( 'NONE', #38909, .T. ) ;
#66323 = VECTOR ( 'NONE', #63961, 1000.000000000000000 ) ;
#66324 =( GEOMETRIC_REPRESENTATION_CONTEXT ( 3 ) GLOBAL_UNCERTAINTY_ASSIGNED_CONTEXT ( ( #60123 ) ) GLOBAL_UNIT_ASSIGNED_CONTEXT ( ( #50216, #54427, #5891 ) ) REPRESENTATION_CONTEXT ( 'NONE', 'WORKASPACE' ) );
#66325 = CARTESIAN_POINT ( 'NONE',  ( -71.15707362346617515, -9.058813317711329915, -2.943386871421370898 ) ) ;
#66326 = CARTESIAN_POINT ( 'NONE',  ( -89.69499999999999318, -8.437984349512085203, 5.166775262442717831E-16 ) ) ;
#66327 = ORIENTED_EDGE ( 'NONE', *, *, #13481, .F. ) ;
#66328 = PRODUCT_DEFINITION_FORMATION_WITH_SPECIFIED_SOURCE ( 'ANY', '', #52408, .NOT_KNOWN. ) ;
#66329 = CARTESIAN_POINT ( 'NONE',  ( -20.57648123223228254, 114.4999999999999574, -10.27659574468085069 ) ) ;
#66330 = CARTESIAN_POINT ( 'NONE',  ( 45.00000000000000000, 10.18984267075364336, 6.892226874380345869 ) ) ;
#66331 = DIRECTION ( 'NONE',  ( -1.000000000000000000, 0.000000000000000000, 0.000000000000000000 ) ) ;
#66332 = ORIENTED_EDGE ( 'NONE', *, *, #44149, .F. ) ;
#66333 = PLANE ( 'NONE',  #29114 ) ;
#66334 = DIRECTION ( 'NONE',  ( 1.000000000000000000, -0.000000000000000000, 0.000000000000000000 ) ) ;
#66335 = EDGE_LOOP ( 'NONE', ( #23046, #45969, #46782 ) ) ;
#66336 = DIRECTION ( 'NONE',  ( 0.000000000000000000, 0.000000000000000000, -1.000000000000000000 ) ) ;
#66337 = ORIENTED_EDGE ( 'NONE', *, *, #36594, .F. ) ;
#66338 = CYLINDRICAL_SURFACE ( 'NONE', #57454, 9.524999999999991473 ) ;
#66339 = CARTESIAN_POINT ( 'NONE',  ( -60.00000000000000000, -2.024042244987997205E-14, 6.500000000000000000 ) ) ;
#66340 = FILL_AREA_STYLE ('',( #66701 ) ) ;
#66341 = DIRECTION ( 'NONE',  ( 5.782411586589351722E-16, -1.000000000000000000, -0.000000000000000000 ) ) ;
#66342 = CARTESIAN_POINT ( 'NONE',  ( -179.9070736234661751, -3.094860106618429807, 9.524999999999991473 ) ) ;
#66343 = DIRECTION ( 'NONE',  ( 0.000000000000000000, 0.000000000000000000, 1.000000000000000000 ) ) ;
#66344 = CARTESIAN_POINT ( 'NONE',  ( -195.0000000000000000, 1.166476076187852838E-15, -9.524999999999991473 ) ) ;
#66345 = CARTESIAN_POINT ( 'NONE',  ( -115.4070736234661609, 3.094860106618428031, -9.524999999999993250 ) ) ;
#66346 = LINE ( 'NONE', #44942, #29594 ) ;
#66347 = PRESENTATION_LAYER_ASSIGNMENT (  '', '', ( #48469 ) ) ;
#66348 = DIRECTION ( 'NONE',  ( -1.000000000000000000, 0.000000000000000000, 0.000000000000000000 ) ) ;
#66349 = ORIENTED_EDGE ( 'NONE', *, *, #37871, .F. ) ;
#66350 = CARTESIAN_POINT ( 'NONE',  ( 0.9999999999999991118, 43.00000000000000000, 45.61250543006183733 ) ) ;
#66351 = PRESENTATION_STYLE_ASSIGNMENT (( #29771 ) ) ;
#66352 = CARTESIAN_POINT ( 'NONE',  ( 1.224646799147353256E-15, 2.299999999999999822, 10.00000000000000000 ) ) ;
#66353 = ORIENTED_EDGE ( 'NONE', *, *, #59354, .F. ) ;
#66354 = CARTESIAN_POINT ( 'NONE',  ( -157.4050000000000011, -2.607480562269069768, 8.024999999999991473 ) ) ;
#66355 = CARTESIAN_POINT ( 'NONE',  ( -4.041451884327381450, 7.000000000000006217, 7.500000000000000000 ) ) ;
#66356 = CARTESIAN_POINT ( 'NONE',  ( 48.81081081081080697, 14.09971791521133255, -7.000000000000000000 ) ) ;
#66357 = TOROIDAL_SURFACE ( 'NONE', #14709, 6.000000000000000000, 1.000000000000000000 ) ;
#66358 = CARTESIAN_POINT ( 'NONE',  ( -159.8950000000000102, 6.826472737025116366, 4.959722759717898555 ) ) ;
#66359 = CARTESIAN_POINT ( 'NONE',  ( -158.9950000000000045, -6.826472737025113702, 4.959722759717902107 ) ) ;
#66360 = EDGE_LOOP ( 'NONE', ( #49547, #61939, #68237 ) ) ;
#66361 = VECTOR ( 'NONE', #44637, 1000.000000000000000 ) ;
#66362 = CARTESIAN_POINT ( 'NONE',  ( -8.920833891111504599, 2.548662454712528724, 0.2685431138779709737 ) ) ;
#66363 = DIRECTION ( 'NONE',  ( 1.300977106640434891E-16, -0.000000000000000000, 1.000000000000000000 ) ) ;
#66364 = CARTESIAN_POINT ( 'NONE',  ( 8.252730563585672030, -2.464278740834330517, -3.705851362693084905 ) ) ;
#66365 = CARTESIAN_POINT ( 'NONE',  ( -72.65499999999998693, -7.632228543268600340, -2.479861379858950166 ) ) ;
#66366 = CARTESIAN_POINT ( 'NONE',  ( 2.527095087882868789E-16, 42.58578643762690774, 35.91421356237309226 ) ) ;
#66367 = AXIS2_PLACEMENT_3D ( 'NONE', #5643, #32742, #43371 ) ;
#66368 = CARTESIAN_POINT ( 'NONE',  ( -167.6929263765338192, 10.01517768586948698, -1.839758294383808966E-15 ) ) ;
#66369 = CARTESIAN_POINT ( 'NONE',  ( -73.49499999999999034, 6.826472737025113702, -4.959722759717902107 ) ) ;
#66370 = CARTESIAN_POINT ( 'NONE',  ( 3.094860106618435136, 143.4049999999999443, -9.525000000000000355 ) ) ;
#66371 = LINE ( 'NONE', #33673, #29767 ) ;
#66372 = AXIS2_PLACEMENT_3D ( 'NONE', #34092, #66092, #17918 ) ;
#66373 = EDGE_CURVE ( 'NONE', #48775, #20367, #31486, .T. ) ;
#66374 = CARTESIAN_POINT ( 'NONE',  ( 2.879676288001297824, 154.2659213600069847, 8.840802594141084825 ) ) ;
#66375 = UNCERTAINTY_MEASURE_WITH_UNIT (LENGTH_MEASURE( 1.000000000000000082E-05 ), #52714, 'distance_accuracy_value', 'NONE');
#66376 = STYLED_ITEM ( 'NONE', ( #31862 ), #16864 ) ;
#66377 = CARTESIAN_POINT ( 'NONE',  ( 11.00000000000001776, -3.148064030671221758, -29.68999999999999417 ) ) ;
#66378 = CARTESIAN_POINT ( 'NONE',  ( -48.81081081081080697, 14.09971791521132900, -7.500000000000000000 ) ) ;
#66379 = DIRECTION ( 'NONE',  ( 0.000000000000000000, -0.000000000000000000, 1.000000000000000000 ) ) ;
#66380 = CARTESIAN_POINT ( 'NONE',  ( 28.00000000000002842, 38.70020753820971748, 89.00000000000000000 ) ) ;
#66381 = ADVANCED_FACE ( 'NONE', ( #59606, #64558 ), #1509, .F. ) ;
#66382 = EDGE_CURVE ( 'NONE', #25647, #3068, #21183, .T. ) ;
#66383 = DIRECTION ( 'NONE',  ( -1.000000000000000000, 0.000000000000000000, 0.000000000000000000 ) ) ;
#66384 = VERTEX_POINT ( 'NONE', #37877 ) ;
#66385 = ORIENTED_EDGE ( 'NONE', *, *, #52653, .F. ) ;
#66386 = SURFACE_STYLE_FILL_AREA ( #44976 ) ;
#66387 = CIRCLE ( 'NONE', #45057, 5.000000000000004441 ) ;
#66388 = EDGE_CURVE ( 'NONE', #2387, #1595, #28261, .T. ) ;
#66389 = PLANE ( 'NONE',  #51837 ) ;
#66390 = MECHANICAL_DESIGN_GEOMETRIC_PRESENTATION_REPRESENTATION (  '', ( #15875 ), #68681 ) ;
#66391 = ADVANCED_FACE ( 'NONE', ( #54676 ), #55987, .T. ) ;
#66392 = CIRCLE ( 'NONE', #14758, 8.000000000000000000 ) ;
#66393 = CARTESIAN_POINT ( 'NONE',  ( -24.21231517720798010, 113.4999999999999858, -7.500000000000000000 ) ) ;
#66394 =( LENGTH_UNIT ( ) NAMED_UNIT ( * ) SI_UNIT ( .MILLI., .METRE. ) );
#66395 =( BOUNDED_CURVE ( )  B_SPLINE_CURVE ( 3, ( #37643, #42917, #32638, #65357 ),
 .UNSPECIFIED., .F., .F. ) 
 B_SPLINE_CURVE_WITH_KNOTS ( ( 4, 4 ),
 ( 3.141592653589793116, 4.712388980384689674 ),
 .UNSPECIFIED. ) 
 CURVE ( )  GEOMETRIC_REPRESENTATION_ITEM ( )  RATIONAL_B_SPLINE_CURVE ( ( 1.000000000000000000, 0.8047378541243649375, 0.8047378541243649375, 1.000000000000000000 ) ) 
 REPRESENTATION_ITEM ( '' )  );
#66396 = DIRECTION ( 'NONE',  ( -0.000000000000000000, -0.000000000000000000, -1.000000000000000000 ) ) ;
#66397 = ORIENTED_EDGE ( 'NONE', *, *, #37640, .F. ) ;
#66398 = CARTESIAN_POINT ( 'NONE',  ( -105.5049999999999670, -6.826472737025113702, -4.959722759717900331 ) ) ;
#66399 = ORIENTED_EDGE ( 'NONE', *, *, #64074, .T. ) ;
#66400 = FACE_OUTER_BOUND ( 'NONE', #50975, .T. ) ;
#66401 = CARTESIAN_POINT ( 'NONE',  ( 7.794228634059951588, -4.500000000000003553, 0.000000000000000000 ) ) ;
#66402 = VERTEX_POINT ( 'NONE', #38561 ) ;
#66403 = CARTESIAN_POINT ( 'NONE',  ( 9.058813317711338797, 112.9549999999999841, -2.943386871421372675 ) ) ;
#66404 = DIRECTION ( 'NONE',  ( 0.000000000000000000, 0.000000000000000000, -1.000000000000000000 ) ) ;
#66405 = ORIENTED_EDGE ( 'NONE', *, *, #23575, .F. ) ;
#66406 = AXIS2_PLACEMENT_3D ( 'NONE', #40473, #25306, #2404 ) ;
#66407 = CARTESIAN_POINT ( 'NONE',  ( -33.89861118948982721, -9.947368421052626530, -7.000000000000000000 ) ) ;
#66408 = PRESENTATION_LAYER_ASSIGNMENT (  '', '', ( #3452 ) ) ;
#66409 = PRESENTATION_STYLE_ASSIGNMENT (( #5928 ) ) ;
#66410 = CARTESIAN_POINT ( 'NONE',  ( -120.1449999999999818, -4.716976649647092401, 6.492361379858946790 ) ) ;
#66411 = VERTEX_POINT ( 'NONE', #17086 ) ;
#66412 = AXIS2_PLACEMENT_3D ( 'NONE', #32550, #15719, #36847 ) ;
#66413 = ORIENTED_EDGE ( 'NONE', *, *, #822, .F. ) ;
#66414 = CARTESIAN_POINT ( 'NONE',  ( -1.135663242406173001, 2.431311185535292907, 9.000000000000003553 ) ) ;
#66415 = SURFACE_STYLE_USAGE ( .BOTH. , #29470 ) ;
#66416 = CARTESIAN_POINT ( 'NONE',  ( 24.35019923159519450, 27.05390878412926270, -27.33833584792231974 ) ) ;
#66417 = CARTESIAN_POINT ( 'NONE',  ( 44.79289321881345387, 10.55564175590369658, 3.499999999999996447 ) ) ;
#66418 = ORIENTED_EDGE ( 'NONE', *, *, #6743, .F. ) ;
#66419 = CARTESIAN_POINT ( 'NONE',  ( 6.826472737025119919, 139.8929263765338362, 4.959722759717908325 ) ) ;
#66420 = DIRECTION ( 'NONE',  ( -0.000000000000000000, 1.000000000000000000, -0.000000000000000000 ) ) ;
#66421 = DIRECTION ( 'NONE',  ( 0.000000000000000000, 0.000000000000000000, -1.000000000000000000 ) ) ;
#66422 = FACE_OUTER_BOUND ( 'NONE', #38459, .T. ) ;
#66423 = EDGE_LOOP ( 'NONE', ( #60612, #39392, #6135, #39487, #27833, #63730 ) ) ;
#66424 = CARTESIAN_POINT ( 'NONE',  ( 7.000000000000017764, 17.04554193418302788, 0.6691306063588586817 ) ) ;
#66425 = VERTEX_POINT ( 'NONE', #27584 ) ;
#66426 = SURFACE_STYLE_USAGE ( .BOTH. , #50601 ) ;
#66427 = DIRECTION ( 'NONE',  ( 1.000000000000000000, 0.000000000000000000, -0.000000000000000000 ) ) ;
#66428 = DIRECTION ( 'NONE',  ( -0.000000000000000000, -1.000000000000000000, -0.000000000000000000 ) ) ;
#66429 = PLANE ( 'NONE',  #26506 ) ;
#66430 = CARTESIAN_POINT ( 'NONE',  ( -135.6550000000000011, -7.632228543268600340, -2.479861379858950166 ) ) ;
#66431 = SURFACE_STYLE_FILL_AREA ( #60789 ) ;
#66432 =( BOUNDED_CURVE ( )  B_SPLINE_CURVE ( 3, ( #24130, #61402, #34674, #23783 ),
 .UNSPECIFIED., .F., .F. ) 
 B_SPLINE_CURVE_WITH_KNOTS ( ( 4, 4 ),
 ( 1.649859741910239874, 3.741551587622924835 ),
 .UNSPECIFIED. ) 
 CURVE ( )  GEOMETRIC_REPRESENTATION_ITEM ( )  RATIONAL_B_SPLINE_CURVE ( ( 1.000000000000000000, 0.6674467249320013007, 0.6674467249320013007, 1.000000000000000000 ) ) 
 REPRESENTATION_ITEM ( '' )  );
#66433 = CARTESIAN_POINT ( 'NONE',  ( 45.50000000000000000, 1.797044900979284448E-15, 9.500000000000000000 ) ) ;
#66434 = ORIENTED_EDGE ( 'NONE', *, *, #40448, .T. ) ;
#66435 = CIRCLE ( 'NONE', #13600, 5.000000000000004441 ) ;
#66436 = DIRECTION ( 'NONE',  ( -1.000000000000000000, 0.000000000000000000, 0.000000000000000000 ) ) ;
#66437 = CARTESIAN_POINT ( 'NONE',  ( 4.383403428314264438, 9.000000000000012434, 1.003298500868274434 ) ) ;
#66438 = CARTESIAN_POINT ( 'NONE',  ( -4.041451884327378785, -1.417096231345241542, 7.000000000000000000 ) ) ;
#66439 = EDGE_LOOP ( 'NONE', ( #51517, #12944 ) ) ;
#66440 = COLOUR_RGB ( '', 0.40784314, 0.44705882, 0.49803922) ;
#66441 = VERTEX_POINT ( 'NONE', #33914 ) ;
#66442 = CARTESIAN_POINT ( 'NONE',  ( -31.83028512801498877, -8.710578351985672541, -1.097192391871058437 ) ) ;
#66443 = CARTESIAN_POINT ( 'NONE',  ( -52.10707362346616378, 8.102448949553172852, -5.886773742842744461 ) ) ;
#66444 = CARTESIAN_POINT ( 'NONE',  ( -50.90499999999997982, 2.607480562269068880, -8.024999999999993250 ) ) ;
#66445 = ORIENTED_EDGE ( 'NONE', *, *, #16175, .F. ) ;
#66446 =( NAMED_UNIT ( * ) SI_UNIT ( $, .STERADIAN. ) SOLID_ANGLE_UNIT ( ) );
#66447 = CARTESIAN_POINT ( 'NONE',  ( 59.00000000000000000, 11.99999999999999822, 3.499999999999992895 ) ) ;
#66448 = CARTESIAN_POINT ( 'NONE',  ( -163.9429263765338192, 0.000000000000000000, 9.524999999999991473 ) ) ;
#66449 = CYLINDRICAL_SURFACE ( 'NONE', #34089, 0.2500000000000002220 ) ;
#66450 = CARTESIAN_POINT ( 'NONE',  ( -178.4070736234662604, 3.094860106617537188, -9.525000000000639844 ) ) ;
#66451 = ORIENTED_EDGE ( 'NONE', *, *, #42127, .F. ) ;
#66452 = CARTESIAN_POINT ( 'NONE',  ( -74.74007105697891973, 36.01955776115826069, -9.942355741406379011 ) ) ;
#66453 = CIRCLE ( 'NONE', #38443, 0.9999999999999984457 ) ;
#66454 = VECTOR ( 'NONE', #13507, 1000.000000000000000 ) ;
#66455 = DIRECTION ( 'NONE',  ( 1.000000000000000000, 0.000000000000000000, 0.000000000000000000 ) ) ;
#66456 = DIRECTION ( 'NONE',  ( -0.000000000000000000, -0.000000000000000000, -1.000000000000000000 ) ) ;
#66457 = CARTESIAN_POINT ( 'NONE',  ( -99.95499999999998408, -7.632228543268599452, 2.479861379858951054 ) ) ;
#66458 = CARTESIAN_POINT ( 'NONE',  ( -29.24174177788027507, -8.499999999999996447, 0.6065382340992577781 ) ) ;
#66459 = DIRECTION ( 'NONE',  ( 0.000000000000000000, 0.000000000000000000, -1.000000000000000000 ) ) ;
#66460 = CARTESIAN_POINT ( 'NONE',  ( 0.000000000000000000, 30.74999999999999289, 3.750000000000000000 ) ) ;
#66461 = AXIS2_PLACEMENT_3D ( 'NONE', #28959, #27315, #29322 ) ;
#66462 = CARTESIAN_POINT ( 'NONE',  ( -98.09499999999997044, -2.607480562269071545, -8.024999999999991473 ) ) ;
#66463 = CARTESIAN_POINT ( 'NONE',  ( 9.058813317711337021, 118.6549999999999869, 2.943386871421375783 ) ) ;
#66464 = CARTESIAN_POINT ( 'NONE',  ( -80.09499999999998465, -2.607480562269071545, -8.024999999999991473 ) ) ;
#66465 = PRESENTATION_LAYER_ASSIGNMENT (  '', '', ( #50757 ) ) ;
#66466 = DIRECTION ( 'NONE',  ( -1.000000000000000000, 0.000000000000000000, 0.000000000000000000 ) ) ;
#66467 = EDGE_CURVE ( 'NONE', #23204, #30840, #43829, .T. ) ;
#66468 = DIRECTION ( 'NONE',  ( -0.000000000000000000, -0.000000000000000000, 1.000000000000000000 ) ) ;
#66469 = SURFACE_SIDE_STYLE ('',( #12288 ) ) ;
#66470 = DIRECTION ( 'NONE',  ( 1.000000000000000000, 0.000000000000000000, 0.000000000000000000 ) ) ;
#66471 = UNCERTAINTY_MEASURE_WITH_UNIT (LENGTH_MEASURE( 1.000000000000000082E-05 ), #53700, 'distance_accuracy_value', 'NONE');
#66472 = EDGE_CURVE ( 'NONE', #18083, #43779, #1979, .T. ) ;
#66473 = PRESENTATION_LAYER_ASSIGNMENT (  '', '', ( #13697 ) ) ;
#66474 = DIRECTION ( 'NONE',  ( 0.000000000000000000, 0.000000000000000000, -1.000000000000000000 ) ) ;
#66475 = CARTESIAN_POINT ( 'NONE',  ( 40.78947368421052033, 108.1536491499103221, -3.158024016299528558 ) ) ;
#66476 = ORIENTED_EDGE ( 'NONE', *, *, #51160, .F. ) ;
#66477 = CARTESIAN_POINT ( 'NONE',  ( -115.9429263765338050, 0.000000000000000000, 9.524999999999991473 ) ) ;
#66478 = PRESENTATION_STYLE_ASSIGNMENT (( #68831 ) ) ;
#66479 = CARTESIAN_POINT ( 'NONE',  ( -140.8449999999999989, -7.632228543268599452, 2.479861379858951054 ) ) ;
#66481 = DIRECTION ( 'NONE',  ( 0.000000000000000000, 0.000000000000000000, -1.000000000000000000 ) ) ;
#66480 = PRESENTATION_LAYER_ASSIGNMENT (  '', '', ( #54105 ) ) ;
#66482 = AXIS2_PLACEMENT_3D ( 'NONE', #62537, #51652, #30513 ) ;
#66483 = CARTESIAN_POINT ( 'NONE',  ( -5.710692600061829438, 4.108790270285304302, 3.163668057994810583E-15 ) ) ;
#66484 = VECTOR ( 'NONE', #1768, 1000.000000000000114 ) ;
#66485 = ADVANCED_FACE ( 'NONE', ( #67671 ), #48193, .T. ) ;
#66486 =( LENGTH_UNIT ( ) NAMED_UNIT ( * ) SI_UNIT ( .MILLI., .METRE. ) );
#66487 = CARTESIAN_POINT ( 'NONE',  ( -19.00000000000000000, 8.000000000000000000, -3.500000000000017764 ) ) ;
#66488 = ORIENTED_EDGE ( 'NONE', *, *, #25346, .F. ) ;
#66489 = ORIENTED_EDGE ( 'NONE', *, *, #67026, .F. ) ;
#66490 = LINE ( 'NONE', #8092, #22046 ) ;
#66491 = LINE ( 'NONE', #46463, #19599 ) ;
#66492 = AXIS2_PLACEMENT_3D ( 'NONE', #46776, #67834, #3044 ) ;
#66493 = EDGE_CURVE ( 'NONE', #13277, #57528, #12807, .T. ) ;
#66494 = FILL_AREA_STYLE ('',( #24262 ) ) ;
#66495 = CARTESIAN_POINT ( 'NONE',  ( -98.75707362346616947, -5.598654528085801552, 7.705886871421367523 ) ) ;
#66496 = VECTOR ( 'NONE', #52186, 1000.000000000000000 ) ;
#66497 = FILL_AREA_STYLE_COLOUR ( '', #31795 ) ;
#66498 = ORIENTED_EDGE ( 'NONE', *, *, #2571, .T. ) ;
#66499 = CARTESIAN_POINT ( 'NONE',  ( -129.6550000000000011, -7.632228543268600340, -2.479861379858950166 ) ) ;
#66500 = ORIENTED_EDGE ( 'NONE', *, *, #10517, .T. ) ;
#66501 = ORIENTED_EDGE ( 'NONE', *, *, #56938, .F. ) ;
#66502 = CARTESIAN_POINT ( 'NONE',  ( 53.24999999999999289, 27.74999999999998579, 3.750000000000000000 ) ) ;
#66503 = EDGE_LOOP ( 'NONE', ( #56961, #57071, #6534 ) ) ;
#66504 = TOROIDAL_SURFACE ( 'NONE', #5823, 1.000000000000000000, 0.5000000000000000000 ) ;
#66505 = CARTESIAN_POINT ( 'NONE',  ( 12.75000000000000533, 28.24999999999998224, 4.000000000000000000 ) ) ;
#66506 = CARTESIAN_POINT ( 'NONE',  ( 0.9999999999999991118, 43.00000000000000000, 45.61250543006183733 ) ) ;
#66507 = CARTESIAN_POINT ( 'NONE',  ( -3.094860106618432471, 139.5949999999999420, -9.525000000000000355 ) ) ;
#66508 = VERTEX_POINT ( 'NONE', #66271 ) ;
#66509 = VECTOR ( 'NONE', #59854, 1000.000000000000000 ) ;
#66510 = SURFACE_STYLE_FILL_AREA ( #60867 ) ;
#66511 = CARTESIAN_POINT ( 'NONE',  ( -10.01517768586949408, 144.3049999999999784, -6.132527647946036459E-16 ) ) ;
#66512 = MECHANICAL_DESIGN_GEOMETRIC_PRESENTATION_REPRESENTATION (  '', ( #28256 ), #45155 ) ;
#66513 = CARTESIAN_POINT ( 'NONE',  ( -56.00499999999996703, 6.826472737025115478, 4.959722759717899443 ) ) ;
#66514 = CARTESIAN_POINT ( 'NONE',  ( 40.78947369313011251, 108.1536491435769989, -3.152202064295424488 ) ) ;
#66515 = ORIENTED_EDGE ( 'NONE', *, *, #35267, .T. ) ;
#66516 = CARTESIAN_POINT ( 'NONE',  ( -8.102448949553181734, 159.0049999999999670, -5.886773742842749790 ) ) ;
#66517 = DIRECTION ( 'NONE',  ( 1.000000000000000000, 0.000000000000000000, 0.000000000000000000 ) ) ;
#66518 = UNCERTAINTY_MEASURE_WITH_UNIT (LENGTH_MEASURE( 1.000000000000000082E-05 ), #38352, 'distance_accuracy_value', 'NONE');
#66519 = PRESENTATION_LAYER_ASSIGNMENT (  '', '', ( #12559 ) ) ;
#66520 = SURFACE_STYLE_FILL_AREA ( #8128 ) ;
#66521 = ORIENTED_EDGE ( 'NONE', *, *, #46929, .F. ) ;
#66522 = AXIS2_PLACEMENT_3D ( 'NONE', #62841, #14682, #15054 ) ;
#66523 = FILL_AREA_STYLE ('',( #38792 ) ) ;
#66524 = ORIENTED_EDGE ( 'NONE', *, *, #42525, .F. ) ;
#66525 = PLANE ( 'NONE',  #52785 ) ;
#66526 = CARTESIAN_POINT ( 'NONE',  ( -29.91370621994235890, -7.761720733523295834, -0.7755720678495816589 ) ) ;
#66527 = CARTESIAN_POINT ( 'NONE',  ( -47.44854201893517143, -11.76587057138590886, 3.309444246618569174 ) ) ;
#66528 = CARTESIAN_POINT ( 'NONE',  ( -162.0550000000000068, -9.827790563157499189E-16, -8.024999999999991473 ) ) ;
#66529 = ORIENTED_EDGE ( 'NONE', *, *, #62637, .F. ) ;
#66530 = UNCERTAINTY_MEASURE_WITH_UNIT (LENGTH_MEASURE( 1.000000000000000082E-05 ), #56585, 'distance_accuracy_value', 'NONE');
#66531 = EDGE_CURVE ( 'NONE', #51470, #11299, #40259, .T. ) ;
#66532 = COLOUR_RGB ( '', 0.66274510, 0.83137255, 0.94901961) ;
#66533 = DIRECTION ( 'NONE',  ( 1.000000000000000000, 0.000000000000000000, 0.000000000000000000 ) ) ;
#66534 = DIRECTION ( 'NONE',  ( 0.000000000000000000, 0.000000000000000000, 1.000000000000000000 ) ) ;
#66535 = LINE ( 'NONE', #11406, #57260 ) ;
#66536 = DIRECTION ( 'NONE',  ( 0.000000000000000000, -1.000000000000000000, 0.000000000000000000 ) ) ;
#66537 = ORIENTED_EDGE ( 'NONE', *, *, #49967, .T. ) ;
#66538 = VERTEX_POINT ( 'NONE', #13146 ) ;
#66539 = DIRECTION ( 'NONE',  ( -1.000000000000000000, -0.000000000000000000, -0.000000000000000000 ) ) ;
#66540 = AXIS2_PLACEMENT_3D ( 'NONE', #21908, #43420, #60227 ) ;
#66541 = CARTESIAN_POINT ( 'NONE',  ( -78.20499999999996987, -2.607480562269071545, -8.024999999999991473 ) ) ;
#66542 = EDGE_LOOP ( 'NONE', ( #31289, #50315, #54247, #5480, #30170, #55957, #12594, #33783, #46585, #34401 ) ) ;
#66543 =( NAMED_UNIT ( * ) PLANE_ANGLE_UNIT ( ) SI_UNIT ( $, .RADIAN. ) );
#66544 = AXIS2_PLACEMENT_3D ( 'NONE', #41834, #9451, #25940 ) ;
#66545 = DIRECTION ( 'NONE',  ( 1.000000000000000000, -0.000000000000000000, -0.000000000000000000 ) ) ;
#66546 =( BOUNDED_CURVE ( )  B_SPLINE_CURVE ( 2, ( #3297, #29371, #30763, #52263, #8980, #4021, #24786, #24111, #19866, #30396, #10381 ),
 .UNSPECIFIED., .F., .F. ) 
 B_SPLINE_CURVE_WITH_KNOTS ( ( 3, 2, 2, 2, 2, 3 ),
 ( 0.5652173913043346820, 0.5673913043478129303, 0.5695652173912910676, 0.5717391304347693159, 0.5739130434782474532, 0.5760869565217255905 ),
 .UNSPECIFIED. ) 
 CURVE ( )  GEOMETRIC_REPRESENTATION_ITEM ( )  RATIONAL_B_SPLINE_CURVE ( ( 1.000000000000294875, 0.9510565162948585449, 1.000000000000000000, 0.9510565162951535312, 1.000000000000000000, 0.9510565162951535312, 1.000000000000000000, 0.9510565162951535312, 1.000000000000000000, 0.9510565162954585094, 0.9999999999996950217 ) ) 
 REPRESENTATION_ITEM ( '' )  );
#66547 = AXIS2_PLACEMENT_3D ( 'NONE', #63754, #31388, #52886 ) ;
#66548 = DIRECTION ( 'NONE',  ( 0.000000000000000000, 0.000000000000000000, -1.000000000000000000 ) ) ;
#66549 = ORIENTED_EDGE ( 'NONE', *, *, #60466, .F. ) ;
#66551 = DIRECTION ( 'NONE',  ( 0.000000000000000000, 0.000000000000000000, 1.000000000000000000 ) ) ;
#66550 = CARTESIAN_POINT ( 'NONE',  ( -84.49999999999998579, -2.499999999999999556, 24.00000000000000000 ) ) ;
#66552 = EDGE_CURVE ( 'NONE', #22382, #67437, #39585, .T. ) ;
#66553 = EDGE_CURVE ( 'NONE', #57942, #60077, #19108, .T. ) ;
#66554 = CARTESIAN_POINT ( 'NONE',  ( -3.094860106618432471, 142.5950000000000273, -9.525000000000000355 ) ) ;
#66555 = CARTESIAN_POINT ( 'NONE',  ( -105.5949999999999989, 2.607480562269073321, 8.024999999999991473 ) ) ;
#66556 = CIRCLE ( 'NONE', #14913, 0.5000000000000004441 ) ;
#66557 = CARTESIAN_POINT ( 'NONE',  ( -7.500000000000000000, 0.000000000000000000, 0.2499999999999924227 ) ) ;
#66559 = CARTESIAN_POINT ( 'NONE',  ( -15.66262743815122604, 10.92411111548398139, 4.966771479319564087 ) ) ;
#66558 = LINE ( 'NONE', #67247, #28962 ) ;
#66560 = CIRCLE ( 'NONE', #64290, 8.500000000000007105 ) ;
#66561 = EDGE_CURVE ( 'NONE', #10808, #20549, #62393, .T. ) ;
#66562 = CARTESIAN_POINT ( 'NONE',  ( -143.5429263765338135, 9.058813317711329915, 2.943386871421369566 ) ) ;
#66563 = CARTESIAN_POINT ( 'NONE',  ( -168.2950000000000159, -2.607480562269069768, 8.024999999999991473 ) ) ;
#66564 = VECTOR ( 'NONE', #3302, 1000.000000000000000 ) ;
#66565 = LINE ( 'NONE', #49702, #53476 ) ;
#66566 = AXIS2_PLACEMENT_3D ( 'NONE', #64776, #10623, #58461 ) ;
#66567 = EDGE_CURVE ( 'NONE', #59091, #22594, #18904, .T. ) ;
#66568 = CARTESIAN_POINT ( 'NONE',  ( -23.21231517720797655, 117.9999999999999716, -9.500000000000000000 ) ) ;
#66569 = ORIENTED_EDGE ( 'NONE', *, *, #63905, .F. ) ;
#66570 = DIRECTION ( 'NONE',  ( -1.189524669241239115E-16, -1.000000000000000000, -0.000000000000000000 ) ) ;
#66571 = ORIENTED_EDGE ( 'NONE', *, *, #27780, .F. ) ;
#66572 = B_SPLINE_CURVE_WITH_KNOTS ( 'NONE', 3,
 ( #45403, #34103, #56240, #66824, #50293, #17610, #2013, #40112 ),
 .UNSPECIFIED., .F., .F.,
 ( 4, 2, 2, 4 ),
 ( 0.000000000000000000, 0.0009392049334771340394, 0.001878409866954268079, 0.003756819733908536157 ),
 .UNSPECIFIED. ) ;
#66573 = LINE ( 'NONE', #50068, #38642 ) ;
#66574 = PRESENTATION_LAYER_ASSIGNMENT (  '', '', ( #32893 ) ) ;
#66575 = EDGE_CURVE ( 'NONE', #52539, #27715, #43770, .T. ) ;
#66576 =( NAMED_UNIT ( * ) PLANE_ANGLE_UNIT ( ) SI_UNIT ( $, .RADIAN. ) );
#66577 = DIRECTION ( 'NONE',  ( 0.000000000000000000, 0.000000000000000000, 1.000000000000000000 ) ) ;
#66578 = SURFACE_STYLE_FILL_AREA ( #29267 ) ;
#66579 = CYLINDRICAL_SURFACE ( 'NONE', #2659, 0.2500000000000002220 ) ;
#66580 =( GEOMETRIC_REPRESENTATION_CONTEXT ( 3 ) GLOBAL_UNCERTAINTY_ASSIGNED_CONTEXT ( ( #67934 ) ) GLOBAL_UNIT_ASSIGNED_CONTEXT ( ( #1570, #33975, #67042 ) ) REPRESENTATION_CONTEXT ( 'NONE', 'WORKASPACE' ) );
#66581 = ORIENTED_EDGE ( 'NONE', *, *, #29275, .F. ) ;
#66582 = CARTESIAN_POINT ( 'NONE',  ( -174.5049999999999955, -6.826472737025113702, -4.959722759717900331 ) ) ;
#66583 = AXIS2_PLACEMENT_3D ( 'NONE', #22162, #42979, #4945 ) ;
#66584 = VERTEX_POINT ( 'NONE', #13857 ) ;
#66585 = CONICAL_SURFACE ( 'NONE', #45279, 4.000000000000000000, 0.7853981633974482790 ) ;
#66586 = SURFACE_SIDE_STYLE ('',( #55679 ) ) ;
#66587 = SURFACE_STYLE_FILL_AREA ( #38854 ) ;
#66588 =( LENGTH_UNIT ( ) NAMED_UNIT ( * ) SI_UNIT ( .MILLI., .METRE. ) );
#66589 = CARTESIAN_POINT ( 'NONE',  ( 0.000000000000000000, 154.0570736234661524, -8.025000000000000355 ) ) ;
#66590 = CIRCLE ( 'NONE', #2511, 14.49999999999999822 ) ;
#66591 = ORIENTED_EDGE ( 'NONE', *, *, #67861, .T. ) ;
#66592 = DIRECTION ( 'NONE',  ( 0.000000000000000000, 0.000000000000000000, 1.000000000000000000 ) ) ;
#66593 = CARTESIAN_POINT ( 'NONE',  ( -84.65500000000000114, -7.632228543268600340, -2.479861379858950166 ) ) ;
#66594 =( NAMED_UNIT ( * ) SI_UNIT ( $, .STERADIAN. ) SOLID_ANGLE_UNIT ( ) );
#66595 = CARTESIAN_POINT ( 'NONE',  ( 3.094860106618431583, 127.2049999999999841, 9.525000000000000355 ) ) ;
#66596 = UNCERTAINTY_MEASURE_WITH_UNIT (LENGTH_MEASURE( 1.000000000000000082E-05 ), #28087, 'distance_accuracy_value', 'NONE');
#66597 = PLANE ( 'NONE',  #46517 ) ;
#66598 = SPHERICAL_SURFACE ( 'NONE', #4007, 0.5000000000000000000 ) ;
#66599 = LINE ( 'NONE', #28932, #8438 ) ;
#66600 = CARTESIAN_POINT ( 'NONE',  ( -87.50000000000000000, -7.499999999999990230, 23.00000000000000000 ) ) ;
#66601 = CARTESIAN_POINT ( 'NONE',  ( -113.3070736234661666, -10.01517768586948698, 6.132527647946031529E-16 ) ) ;
#66602 = ORIENTED_EDGE ( 'NONE', *, *, #24301, .F. ) ;
#66603 = VECTOR ( 'NONE', #17908, 1000.000000000000000 ) ;
#66604 = MECHANICAL_DESIGN_GEOMETRIC_PRESENTATION_REPRESENTATION (  '', ( #7048 ), #64337 ) ;
#66605 = CYLINDRICAL_SURFACE ( 'NONE', #64302, 7.999999999999992895 ) ;
#66606 = CARTESIAN_POINT ( 'NONE',  ( 36.00000000000002842, 0.000000000000000000, 77.00402776293825013 ) ) ;
#66607 = CARTESIAN_POINT ( 'NONE',  ( -51.14499999999999602, -4.716976649647092401, 6.492361379858946790 ) ) ;
#66608 = VERTEX_POINT ( 'NONE', #1852 ) ;
#66609 = LINE ( 'NONE', #7174, #29476 ) ;
#66610 = ADVANCED_FACE ( 'NONE', ( #29325 ), #34965, .T. ) ;
#66611 = AXIS2_PLACEMENT_3D ( 'NONE', #50103, #18075, #1832 ) ;
#66612 = CARTESIAN_POINT ( 'NONE',  ( -15.48999599679679662, 146.4999999999999716, -7.000000000000000000 ) ) ;
#66613 = CARTESIAN_POINT ( 'NONE',  ( 45.00000000000000000, 99.99999999999992895, 10.00000000000000000 ) ) ;
#66614 = PRESENTATION_STYLE_ASSIGNMENT (( #38273 ) ) ;
#66615 = ORIENTED_EDGE ( 'NONE', *, *, #11081, .F. ) ;
#66616 = CARTESIAN_POINT ( 'NONE',  ( -48.86169860080597971, -11.37553613063878366, 3.471446820368512043 ) ) ;
#66617 = CARTESIAN_POINT ( 'NONE',  ( -52.34499999999997755, 7.632228543268599452, -2.479861379858951942 ) ) ;
#66618 = ORIENTED_EDGE ( 'NONE', *, *, #46144, .T. ) ;
#66619 = CARTESIAN_POINT ( 'NONE',  ( -75.00000000000000000, 9.609158271987205069, 6.330303435919315547 ) ) ;
#66620 = CARTESIAN_POINT ( 'NONE',  ( -100.2549999999999812, -4.716976649647092401, 6.492361379858946790 ) ) ;
#66621 = ORIENTED_EDGE ( 'NONE', *, *, #69502, .F. ) ;
#66622 = CARTESIAN_POINT ( 'NONE',  ( -7.632228543268608334, 118.9570736234661581, 2.479861379858952830 ) ) ;
#66623 = SURFACE_SIDE_STYLE ('',( #15677 ) ) ;
#66624 = DIRECTION ( 'NONE',  ( -1.000000000000000000, -0.000000000000000000, -0.000000000000000000 ) ) ;
#66625 = CARTESIAN_POINT ( 'NONE',  ( -149.7570736234661979, -5.598654528085801552, 7.705886871421367523 ) ) ;
#66626 = B_SPLINE_CURVE_WITH_KNOTS ( 'NONE', 3,
 ( #60890, #54907, #11325, #1414, #33816, #32789 ),
 .UNSPECIFIED., .F., .F.,
 ( 4, 2, 4 ),
 ( 2.727025168375190138E-16, 0.001158410220312347267, 0.002316820440624422616 ),
 .UNSPECIFIED. ) ;
#66627 = FACE_OUTER_BOUND ( 'NONE', #12143, .T. ) ;
#66628 = CARTESIAN_POINT ( 'NONE',  ( 3.094860106618431583, 144.0949999999999420, 9.525000000000000355 ) ) ;
#66629 = CARTESIAN_POINT ( 'NONE',  ( -88.10707362346616378, 8.102448949553171076, -5.886773742842744461 ) ) ;
#66630 = PRESENTATION_LAYER_ASSIGNMENT (  '', '', ( #27265 ) ) ;
#66631 = ADVANCED_FACE ( 'NONE', ( #3245 ), #22293, .F. ) ;
#66632 = CARTESIAN_POINT ( 'NONE',  ( -74.99999999999998579, 50.00000000000000000, 10.00000000000000000 ) ) ;
#66633 = VERTEX_POINT ( 'NONE', #24734 ) ;
#66634 = DIRECTION ( 'NONE',  ( 1.000000000000000000, 0.000000000000000000, 0.000000000000000000 ) ) ;
#66635 = CIRCLE ( 'NONE', #328, 11.99999999999999645 ) ;
#66636 = EDGE_CURVE ( 'NONE', #4733, #17912, #15600, .T. ) ;
#66637 = COLOUR_RGB ( '', 0.08235294, 0.09019608, 0.10196078) ;
#66638 = CARTESIAN_POINT ( 'NONE',  ( -119.7549999999999812, 4.716976649647091513, -6.492361379858946790 ) ) ;
#66639 = FACE_OUTER_BOUND ( 'NONE', #47040, .T. ) ;
#66640 = ADVANCED_FACE ( 'NONE', ( #9288 ), #58852, .T. ) ;
#66641 = DIRECTION ( 'NONE',  ( 0.000000000000000000, 0.000000000000000000, -1.000000000000000000 ) ) ;
#66642 =( GEOMETRIC_REPRESENTATION_CONTEXT ( 3 ) GLOBAL_UNCERTAINTY_ASSIGNED_CONTEXT ( ( #65082 ) ) GLOBAL_UNIT_ASSIGNED_CONTEXT ( ( #3328, #3685, #42116 ) ) REPRESENTATION_CONTEXT ( 'NONE', 'WORKASPACE' ) );
#66643 = CARTESIAN_POINT ( 'NONE',  ( -136.7949999999999875, 2.607480562269068880, -8.024999999999993250 ) ) ;
#66644 = CARTESIAN_POINT ( 'NONE',  ( -125.5449999999999875, -7.632228543268600340, -2.479861379858950166 ) ) ;
#66645 = LINE ( 'NONE', #29698, #57210 ) ;
#66646 = VERTEX_POINT ( 'NONE', #37091 ) ;
#66647 = CARTESIAN_POINT ( 'NONE',  ( 12.50000000000000533, 27.99999999999998224, 4.000000000000000000 ) ) ;
#66648 = AXIS2_PLACEMENT_3D ( 'NONE', #42618, #48236, #58759 ) ;
#66649 = SURFACE_STYLE_FILL_AREA ( #19833 ) ;
#66650 = EDGE_CURVE ( 'NONE', #51313, #4242, #57820, .T. ) ;
#66651 = CARTESIAN_POINT ( 'NONE',  ( 0.000000000000000000, 2.000000000000000444, 0.000000000000000000 ) ) ;
#66652 = CARTESIAN_POINT ( 'NONE',  ( -181.6429263765338078, -5.598654528085801552, 7.705886871421367523 ) ) ;
#66653 = CARTESIAN_POINT ( 'NONE',  ( -53.99499999999998323, -6.826472737025115478, 4.959722759717900331 ) ) ;
#66654 = EDGE_CURVE ( 'NONE', #45514, #68810, #9646, .T. ) ;
#66655 = DIRECTION ( 'NONE',  ( 1.000000000000000000, 0.000000000000000000, 0.000000000000000000 ) ) ;
#66656 = PRESENTATION_LAYER_ASSIGNMENT (  '', '', ( #54287 ) ) ;
#66657 = PRESENTATION_LAYER_ASSIGNMENT (  '', '', ( #17226 ) ) ;
#66658 = PRESENTATION_STYLE_ASSIGNMENT (( #29710 ) ) ;
#66659 = CARTESIAN_POINT ( 'NONE',  ( 8.082903768654762899, -1.269775441351268174E-15, 1.082903768654759125 ) ) ;
#66660 = CARTESIAN_POINT ( 'NONE',  ( -92.09292637653381064, 3.094860106618433360, 9.524999999999991473 ) ) ;
#66661 = APPLICATION_PROTOCOL_DEFINITION ( 'draft international standard', 'automotive_design', 1998, #25304 ) ;
#66662 = CARTESIAN_POINT ( 'NONE',  ( -51.21480343399456814, -11.84745778642585989, 1.513780993297752175 ) ) ;
#66663 = CARTESIAN_POINT ( 'NONE',  ( -60.00000000000000000, -2.024042244987997205E-14, -6.500000000000000000 ) ) ;
#66664 = DIRECTION ( 'NONE',  ( 0.000000000000000000, 0.000000000000000000, -1.000000000000000000 ) ) ;
#66665 = CARTESIAN_POINT ( 'NONE',  ( 44.99999999999998579, 119.9999999999999716, -7.000000000000000000 ) ) ;
#66666 = CARTESIAN_POINT ( 'NONE',  ( -41.39002736484395228, 107.1345546009600014, 3.500000000000000000 ) ) ;
#66667 = AXIS2_PLACEMENT_3D ( 'NONE', #26155, #37819, #64835 ) ;
#66668 = EDGE_LOOP ( 'NONE', ( #42366, #35392, #53744, #22566 ) ) ;
#66669 = LINE ( 'NONE', #17122, #4874 ) ;
#66670 = CARTESIAN_POINT ( 'NONE',  ( -12.34222745343792127, 115.4999999999999574, 10.18181818181818166 ) ) ;
#66671 =( NAMED_UNIT ( * ) SI_UNIT ( $, .STERADIAN. ) SOLID_ANGLE_UNIT ( ) );
#66672 = ORIENTED_EDGE ( 'NONE', *, *, #65532, .F. ) ;
#66673 = CARTESIAN_POINT ( 'NONE',  ( 0.000000000000000000, 109.9999999999999858, 22.50000000000000000 ) ) ;
#66674 = ADVANCED_FACE ( 'NONE', ( #10328 ), #53244, .F. ) ;
#66675 = CARTESIAN_POINT ( 'NONE',  ( -4.716976649647098618, 125.2570736234661695, 6.492361379858953008 ) ) ;
#66676 = STYLED_ITEM ( 'NONE', ( #9085 ), #55669 ) ;
#66678 = SURFACE_SIDE_STYLE ('',( #60679 ) ) ;
#66677 = CONICAL_SURFACE ( 'NONE', #30702, 5.000000000000004441, 0.7853981633974587151 ) ;
#66679 = LINE ( 'NONE', #55418, #64551 ) ;
#66680 = VERTEX_POINT ( 'NONE', #69408 ) ;
#66681 = CYLINDRICAL_SURFACE ( 'NONE', #55653, 0.5000000000000004441 ) ;
#66682 = MECHANICAL_DESIGN_GEOMETRIC_PRESENTATION_REPRESENTATION (  '', ( #7185 ), #63318 ) ;
#66683 = DIRECTION ( 'NONE',  ( -1.000000000000000000, 0.000000000000000000, 0.000000000000000000 ) ) ;
#66684 = FACE_BOUND ( 'NONE', #9741, .T. ) ;
#66685 = PRESENTATION_STYLE_ASSIGNMENT (( #7251 ) ) ;
#66686 = CARTESIAN_POINT ( 'NONE',  ( -71.60707362346617799, -8.102448949553174629, 5.886773742842742685 ) ) ;
#66687 = CARTESIAN_POINT ( 'NONE',  ( -84.29499999999998749, -2.607480562269069768, 8.024999999999991473 ) ) ;
#66688 = EDGE_LOOP ( 'NONE', ( #64700, #47314, #14251, #31217 ) ) ;
#66689 = TOROIDAL_SURFACE ( 'NONE', #36414, 1.000000000000000000, 0.5000000000000000000 ) ;
#66690 = PLANE ( 'NONE',  #58085 ) ;
#66691 = CARTESIAN_POINT ( 'NONE',  ( 7.999999999999998224, 5.000000000000000000, -37.00402776293825724 ) ) ;
#66692 = ORIENTED_EDGE ( 'NONE', *, *, #65764, .F. ) ;
#66693 = CARTESIAN_POINT ( 'NONE',  ( -41.49999999999997868, 10.49999999999998046, -3.000000000000000000 ) ) ;
#66694 = FILL_AREA_STYLE_COLOUR ( '', #68470 ) ;
#66696 = CARTESIAN_POINT ( 'NONE',  ( -7.766391886667110001, -0.5482146608018571010, 0.7663918866669822139 ) ) ;
#66695 = AXIS2_PLACEMENT_3D ( 'NONE', #38283, #33647, #55085 ) ;
#66697 = ORIENTED_EDGE ( 'NONE', *, *, #56048, .F. ) ;
#66698 = ADVANCED_FACE ( 'NONE', ( #21197 ), #43427, .T. ) ;
#66699 = DIRECTION ( 'NONE',  ( -0.000000000000000000, -1.000000000000000000, -0.000000000000000000 ) ) ;
#66700 = ORIENTED_EDGE ( 'NONE', *, *, #58452, .F. ) ;
#66701 = FILL_AREA_STYLE_COLOUR ( '', #21782 ) ;
#66702 = FACE_OUTER_BOUND ( 'NONE', #68951, .T. ) ;
#66703 = CIRCLE ( 'NONE', #40884, 5.000000000000004441 ) ;
#66704 = CARTESIAN_POINT ( 'NONE',  ( -174.8070736234661240, 10.01517768586948698, -1.839758294383808571E-15 ) ) ;
#66705 = CARTESIAN_POINT ( 'NONE',  ( 9.058813317711337021, 114.5449999999999733, 2.943386871421375783 ) ) ;
#66706 = CARTESIAN_POINT ( 'NONE',  ( -109.4070736234661609, 3.094860106618428031, -9.524999999999993250 ) ) ;
#66707 =( REPRESENTATION_RELATIONSHIP ('NONE','NONE', #5102, #10054 ) REPRESENTATION_RELATIONSHIP_WITH_TRANSFORMATION ( #26821 )SHAPE_REPRESENTATION_RELATIONSHIP( ) );
#66708 = AXIS2_PLACEMENT_3D ( 'NONE', #53137, #53477, #37339 ) ;
#66709 = EDGE_CURVE ( 'NONE', #3378, #631, #10007, .T. ) ;
#66710 = DIRECTION ( 'NONE',  ( 0.000000000000000000, 0.000000000000000000, 1.000000000000000000 ) ) ;
#66711 = CARTESIAN_POINT ( 'NONE',  ( -4.250000000000001776, 22.24999999999998579, 4.000000000000000000 ) ) ;
#66712 = ORIENTED_EDGE ( 'NONE', *, *, #47898, .T. ) ;
#66713 = DIRECTION ( 'NONE',  ( -0.000000000000000000, -1.000000000000000000, -0.000000000000000000 ) ) ;
#66714 = CARTESIAN_POINT ( 'NONE',  ( 71.62068965517238439, 63.58603185604027885, -9.500000000000000000 ) ) ;
#66715 = SURFACE_STYLE_FILL_AREA ( #29773 ) ;
#66716 = ORIENTED_EDGE ( 'NONE', *, *, #36330, .T. ) ;
#66717 = ADVANCED_FACE ( 'NONE', ( #65150 ), #39159, .T. ) ;
#66718 = AXIS2_PLACEMENT_3D ( 'NONE', #6430, #27858, #17378 ) ;
#66719 = CARTESIAN_POINT ( 'NONE',  ( -164.4549999999999841, 7.632228543268599452, -2.479861379858951942 ) ) ;
#66720 =( NAMED_UNIT ( * ) SI_UNIT ( $, .STERADIAN. ) SOLID_ANGLE_UNIT ( ) );
#66721 = CARTESIAN_POINT ( 'NONE',  ( -183.6962785619511749, -6.980536562595337280, -5.441974211641010584 ) ) ;
#66722 = CARTESIAN_POINT ( 'NONE',  ( -164.2450000000000045, -4.716976649647093289, -6.492361379858945902 ) ) ;
#66723 = MECHANICAL_DESIGN_GEOMETRIC_PRESENTATION_REPRESENTATION (  '', ( #19562 ), #26282 ) ;
#66724 = CARTESIAN_POINT ( 'NONE',  ( -160.1949999999999932, 8.437984349512086979, -1.550032578732815448E-15 ) ) ;
#66725 = ORIENTED_EDGE ( 'NONE', *, *, #27388, .T. ) ;
#66726 = CIRCLE ( 'NONE', #46592, 0.5000000000000004441 ) ;
#66727 = CARTESIAN_POINT ( 'NONE',  ( 24.21231517720798010, 113.4999999999999858, 7.500000000000000000 ) ) ;
#66728 = CARTESIAN_POINT ( 'NONE',  ( -122.9929263765338021, 8.102448949553172852, -5.886773742842744461 ) ) ;
#66729 = AXIS2_PLACEMENT_3D ( 'NONE', #52151, #25383, #3163 ) ;
#66730 = CARTESIAN_POINT ( 'NONE',  ( -70.85499999999998977, 4.716976649647094177, 6.492361379858945902 ) ) ;
#66731 = DIRECTION ( 'NONE',  ( -0.000000000000000000, -0.000000000000000000, -1.000000000000000000 ) ) ;
#66732 = CARTESIAN_POINT ( 'NONE',  ( 44.00000000000000000, 19.24999999999998224, -3.750000000000000000 ) ) ;
#66733 = EDGE_CURVE ( 'NONE', #16450, #35776, #59173, .T. ) ;
#66734 = VECTOR ( 'NONE', #37201, 1000.000000000000000 ) ;
#66735 = CARTESIAN_POINT ( 'NONE',  ( -71.84499999999999886, -7.632228543268599452, 2.479861379858951054 ) ) ;
#66736 = CARTESIAN_POINT ( 'NONE',  ( -5.598654528085808657, 144.7549999999999955, 7.705886871421373741 ) ) ;
#66737 = PRESENTATION_STYLE_ASSIGNMENT (( #45316 ) ) ;
#66738 = CARTESIAN_POINT ( 'NONE',  ( -155.9070736234665162, -3.094860106612816519, 9.525000000004069989 ) ) ;
#66739 = PRESENTATION_LAYER_ASSIGNMENT (  '', '', ( #15109 ) ) ;
#66740 = CARTESIAN_POINT ( 'NONE',  ( -22.75000000000000711, 36.75000000000000000, -3.750000000000000000 ) ) ;
#66741 =( NAMED_UNIT ( * ) PLANE_ANGLE_UNIT ( ) SI_UNIT ( $, .RADIAN. ) );
#66742 = AXIS2_PLACEMENT_3D ( 'NONE', #67301, #24374, #18428 ) ;
#66743 = LINE ( 'NONE', #56881, #41497 ) ;
#66744 = CARTESIAN_POINT ( 'NONE',  ( 3.999798566743338668, 49.09558629977726696, -7.322456175549363344 ) ) ;
#66745 = DIRECTION ( 'NONE',  ( -0.000000000000000000, -0.000000000000000000, -1.000000000000000000 ) ) ;
#66746 = CARTESIAN_POINT ( 'NONE',  ( -74.50000000000000000, -2.208799022165584366E-14, -7.000000000000000888 ) ) ;
#66747 = ORIENTED_EDGE ( 'NONE', *, *, #20567, .F. ) ;
#66749 = ORIENTED_EDGE ( 'NONE', *, *, #4264, .F. ) ;
#66748 = COLOUR_RGB ( '', 0.09019608, 0.27058824, 0.51372549) ;
#66750 = CIRCLE ( 'NONE', #16229, 11.99999999999999467 ) ;
#66751 = ADVANCED_FACE ( 'NONE', ( #11000 ), #49340, .F. ) ;
#66752 = DIRECTION ( 'NONE',  ( -0.000000000000000000, 1.000000000000000000, -0.000000000000000000 ) ) ;
#66753 = DIRECTION ( 'NONE',  ( -1.000000000000000000, 0.000000000000000000, 0.000000000000000000 ) ) ;
#66754 = CARTESIAN_POINT ( 'NONE',  ( 3.542752237027638085, 1.835478060177118120, 9.000000000000003553 ) ) ;
#66755 = CARTESIAN_POINT ( 'NONE',  ( 23.21231517720797655, 113.4999999999999858, 10.00000000000000000 ) ) ;
#66756 = VERTEX_POINT ( 'NONE', #35234 ) ;
#66757 = ORIENTED_EDGE ( 'NONE', *, *, #19452, .T. ) ;
#66758 = DIRECTION ( 'NONE',  ( -0.000000000000000000, -0.000000000000000000, -1.000000000000000000 ) ) ;
#66759 =( NAMED_UNIT ( * ) SI_UNIT ( $, .STERADIAN. ) SOLID_ANGLE_UNIT ( ) );
#66760 = CIRCLE ( 'NONE', #21833, 0.2500000000000002220 ) ;
#66761 = ORIENTED_EDGE ( 'NONE', *, *, #278, .T. ) ;
#66762 = CARTESIAN_POINT ( 'NONE',  ( -65.24292637653380211, 5.598654528085804216, 7.705886871421366635 ) ) ;
#66763 = CARTESIAN_POINT ( 'NONE',  ( 8.000000000000030198, 5.000000000000000000, 29.00402776293826079 ) ) ;
#66764 = VERTEX_POINT ( 'NONE', #55293 ) ;
#66765 = PRESENTATION_LAYER_ASSIGNMENT (  '', '', ( #3880 ) ) ;
#66766 = SURFACE_STYLE_USAGE ( .BOTH. , #30139 ) ;
#66767 = CARTESIAN_POINT ( 'NONE',  ( 30.99999999999998579, 0.000000000000000000, -72.00402776293822171 ) ) ;
#66768 = CARTESIAN_POINT ( 'NONE',  ( -109.4949999999999761, 6.826472737025113702, -4.959722759717902107 ) ) ;
#66769 = ORIENTED_EDGE ( 'NONE', *, *, #8696, .T. ) ;
#66770 = AXIS2_PLACEMENT_3D ( 'NONE', #62623, #8503, #62296 ) ;
#66771 = EDGE_LOOP ( 'NONE', ( #42638, #49974, #8033 ) ) ;
#66772 = CARTESIAN_POINT ( 'NONE',  ( -0.4575609230677321060, 2.491211107078691089, 9.000000000000003553 ) ) ;
#66773 = DIRECTION ( 'NONE',  ( 0.000000000000000000, 0.000000000000000000, -1.000000000000000000 ) ) ;
#66774 = CARTESIAN_POINT ( 'NONE',  ( -12.77502540130583952, -11.12935009515152807, -4.489552594659124374 ) ) ;
#66775 = CARTESIAN_POINT ( 'NONE',  ( -180.4429263765338192, -1.166476076187852838E-15, -9.524999999999991473 ) ) ;
#66776 = CIRCLE ( 'NONE', #26331, 0.5000000000000004441 ) ;
#66777 = ORIENTED_EDGE ( 'NONE', *, *, #67748, .T. ) ;
#66778 = CARTESIAN_POINT ( 'NONE',  ( 0.000000000000000000, 140.9429263765338192, -8.025000000000000355 ) ) ;
#66779 = CARTESIAN_POINT ( 'NONE',  ( -54.52476335569559041, -9.117691409003279901, -3.352975844306524511 ) ) ;
#66780 = DIRECTION ( 'NONE',  ( 0.000000000000000000, 0.000000000000000000, 1.000000000000000000 ) ) ;
#66781 = VECTOR ( 'NONE', #48976, 1000.000000000000000 ) ;
#66782 = PRESENTATION_STYLE_ASSIGNMENT (( #62174 ) ) ;
#66783 = PLANE ( 'NONE',  #16389 ) ;
#66784 = ORIENTED_EDGE ( 'NONE', *, *, #29447, .T. ) ;
#66785 = EDGE_CURVE ( 'NONE', #13126, #20404, #24322, .T. ) ;
#66786 = FACE_OUTER_BOUND ( 'NONE', #56976, .T. ) ;
#66787 = ORIENTED_EDGE ( 'NONE', *, *, #44181, .T. ) ;
#66788 = SURFACE_STYLE_USAGE ( .BOTH. , #45368 ) ;
#66789 =( NAMED_UNIT ( * ) SI_UNIT ( $, .STERADIAN. ) SOLID_ANGLE_UNIT ( ) );
#66790 = DIRECTION ( 'NONE',  ( 1.000000000000000000, -0.000000000000000000, -1.300977106640434891E-16 ) ) ;
#66791 = DIRECTION ( 'NONE',  ( 0.000000000000000000, 0.000000000000000000, -1.000000000000000000 ) ) ;
#66792 = CARTESIAN_POINT ( 'NONE',  ( -137.9049999999999727, 2.607480562269068880, -8.024999999999993250 ) ) ;
#66793 = CARTESIAN_POINT ( 'NONE',  ( 53.25000000000000000, 25.24999999999998579, 3.750000000000000000 ) ) ;
#66794 = CARTESIAN_POINT ( 'NONE',  ( 8.250000000000001776, 30.74999999999998579, -3.750000000000000000 ) ) ;
#66795 = ORIENTED_EDGE ( 'NONE', *, *, #33742, .T. ) ;
#66796 =( NAMED_UNIT ( * ) SI_UNIT ( $, .STERADIAN. ) SOLID_ANGLE_UNIT ( ) );
#66797 = AXIS2_PLACEMENT_3D ( 'NONE', #61340, #6479, #66275 ) ;
#66798 = VECTOR ( 'NONE', #183, 1000.000000000000000 ) ;
#66799 = CARTESIAN_POINT ( 'NONE',  ( 3.062509476195515228E-31, -2.500728763858896269E-15, 12.50000000000000000 ) ) ;
#66800 = CARTESIAN_POINT ( 'NONE',  ( -107.9070736234670989, -3.094860106603102512, 9.525000000011129231 ) ) ;
#66801 = CARTESIAN_POINT ( 'NONE',  ( -60.00000000000000000, -2.024042244987997205E-14, -7.000000000000024869 ) ) ;
#66802 = EDGE_LOOP ( 'NONE', ( #67350, #26201, #11643, #22 ) ) ;
#66803 = VERTEX_POINT ( 'NONE', #45815 ) ;
#66804 = DIRECTION ( 'NONE',  ( -0.000000000000000000, -0.000000000000000000, 1.000000000000000000 ) ) ;
#66805 = B_SPLINE_CURVE_WITH_KNOTS ( 'NONE', 3,
 ( #51420, #20449, #51777, #40898, #15214, #56703, #3526, #57745, #41952, #46178, #68648, #29958 ),
 .UNSPECIFIED., .F., .F.,
 ( 4, 2, 2, 2, 2, 4 ),
 ( 0.000000000000000000, 0.0001470450322352830183, 0.0002940900644705660366, 0.0005881801289411579857, 0.0008822701934117498264, 0.001176360257882341775 ),
 .UNSPECIFIED. ) ;
#66806 = DIRECTION ( 'NONE',  ( -1.000000000000000000, 0.000000000000000000, 0.000000000000000000 ) ) ;
#66807 = CARTESIAN_POINT ( 'NONE',  ( 7.766391886667106448, -1.733608113333017453, 0.5482146608018618750 ) ) ;
#66809 = CARTESIAN_POINT ( 'NONE',  ( -50.15499999999997982, 7.632228543268600340, 2.479861379858949277 ) ) ;
#66808 = AXIS2_PLACEMENT_3D ( 'NONE', #10236, #31313, #46524 ) ;
#66810 = ORIENTED_EDGE ( 'NONE', *, *, #27934, .F. ) ;
#66811 = EDGE_CURVE ( 'NONE', #37989, #14037, #3210, .T. ) ;
#66812 = CARTESIAN_POINT ( 'NONE',  ( -184.4049999999999727, -2.607480562269069768, 8.024999999999991473 ) ) ;
#66813 = FILL_AREA_STYLE_COLOUR ( '', #45337 ) ;
#66814 = LINE ( 'NONE', #23208, #3121 ) ;
#66815 = CARTESIAN_POINT ( 'NONE',  ( -59.30707362346615952, -10.01517768586948698, 6.132527647946031529E-16 ) ) ;
#66816 = VECTOR ( 'NONE', #13720, 1000.000000000000000 ) ;
#66817 = EDGE_CURVE ( 'NONE', #53684, #40833, #50922, .T. ) ;
#66818 = EDGE_LOOP ( 'NONE', ( #40200, #51763, #44076, #66947 ) ) ;
#66819 = CARTESIAN_POINT ( 'NONE',  ( -161.4570736234661865, -9.058813317711329915, 2.943386871421371787 ) ) ;
#66820 = EDGE_CURVE ( 'NONE', #50411, #23842, #42629, .T. ) ;
#66821 = DIRECTION ( 'NONE',  ( 0.000000000000000000, 1.000000000000000000, -0.000000000000000000 ) ) ;
#66822 =( LENGTH_UNIT ( ) NAMED_UNIT ( * ) SI_UNIT ( .MILLI., .METRE. ) );
#66823 = CARTESIAN_POINT ( 'NONE',  ( -98.00500000000000966, 6.826472737025116366, 4.959722759717898555 ) ) ;
#66824 = CARTESIAN_POINT ( 'NONE',  ( -59.45644908980804644, -8.499999999999992895, 0.8985947643278344721 ) ) ;
#66825 =( LENGTH_UNIT ( ) NAMED_UNIT ( * ) SI_UNIT ( .MILLI., .METRE. ) );
#66826 = CIRCLE ( 'NONE', #69087, 1.000000000000000888 ) ;
#66827 = EDGE_CURVE ( 'NONE', #26732, #27703, #51571, .T. ) ;
#66828 = CARTESIAN_POINT ( 'NONE',  ( -100.4949999999999761, 6.826472737025113702, -4.959722759717902107 ) ) ;
#66829 = CARTESIAN_POINT ( 'NONE',  ( -5.598654528085806881, 113.8549999999999898, -7.705886871421374629 ) ) ;
#66830 = CARTESIAN_POINT ( 'NONE',  ( -77.39499999999999602, -6.826472737025115478, -4.959722759717899443 ) ) ;
#66831 =( LENGTH_UNIT ( ) NAMED_UNIT ( * ) SI_UNIT ( .MILLI., .METRE. ) );
#66832 = CIRCLE ( 'NONE', #29756, 0.5000000000000004441 ) ;
#66833 = VECTOR ( 'NONE', #55668, 1000.000000000000000 ) ;
#66834 = DIRECTION ( 'NONE',  ( -1.445602896647339656E-16, -1.000000000000000000, 0.000000000000000000 ) ) ;
#66835 = LINE ( 'NONE', #8772, #2308 ) ;
#66836 = CIRCLE ( 'NONE', #36543, 0.5000000000000004441 ) ;
#66837 = CARTESIAN_POINT ( 'NONE',  ( -67.99999999999998579, -2.024042244987997205E-14, -11.50000000000000000 ) ) ;
#66838 = DIRECTION ( 'NONE',  ( -0.000000000000000000, 1.000000000000000000, -0.000000000000000000 ) ) ;
#66839 = ORIENTED_EDGE ( 'NONE', *, *, #53546, .T. ) ;
#66840 = CARTESIAN_POINT ( 'NONE',  ( -117.5929263765338106, -3.094860106618431139, -9.524999999999991473 ) ) ;
#66841 = CIRCLE ( 'NONE', #1637, 5.000000000000004441 ) ;
#66842 =( BOUNDED_CURVE ( )  B_SPLINE_CURVE ( 2, ( #3153, #14829, #19735, #26040, #68630, #36307, #47578, #57731, #41229, #30977, #68985 ),
 .UNSPECIFIED., .F., .F. ) 
 B_SPLINE_CURVE_WITH_KNOTS ( ( 3, 2, 2, 2, 2, 3 ),
 ( 0.6630434782608540800, 0.6652173913043323283, 0.6673913043478105767, 0.6695652173912887140, 0.6717391304347669623, 0.6739130434782450996 ),
 .UNSPECIFIED. ) 
 CURVE ( )  GEOMETRIC_REPRESENTATION_ITEM ( )  RATIONAL_B_SPLINE_CURVE ( ( 1.000000000000347500, 0.9510565162948061424, 1.000000000000000000, 0.9510565162951535312, 1.000000000000000000, 0.9510565162951535312, 1.000000000000000000, 0.9510565162951535312, 1.000000000000000000, 0.9510565162955084695, 0.9999999999996450617 ) ) 
 REPRESENTATION_ITEM ( '' )  );
#66843 = CARTESIAN_POINT ( 'NONE',  ( -136.3449999999999989, 7.632228543268599452, -2.479861379858951942 ) ) ;
#66844 = CARTESIAN_POINT ( 'NONE',  ( 0.000000000000000000, 87.30187232391182306, 0.000000000000000000 ) ) ;
#66845 = LINE ( 'NONE', #45754, #26908 ) ;
#66846 = ORIENTED_EDGE ( 'NONE', *, *, #5707, .F. ) ;
#66847 = ORIENTED_EDGE ( 'NONE', *, *, #27124, .F. ) ;
#66848 = DIRECTION ( 'NONE',  ( -1.000000000000000000, 0.000000000000000000, 0.000000000000000000 ) ) ;
#66849 = CARTESIAN_POINT ( 'NONE',  ( 13.50000000000000355, 28.24999999999998934, 3.750000000000000000 ) ) ;
#66850 = COLOUR_RGB ( '', 0.40784314, 0.44705882, 0.49803922) ;
#66851 = COLOUR_RGB ( '', 0.72549020, 0.75294118, 0.79215686) ;
#66852 = SURFACE_SIDE_STYLE ('',( #61209 ) ) ;
#66853 = DIRECTION ( 'NONE',  ( -1.000000000000000000, 0.000000000000000000, 0.000000000000000000 ) ) ;
#66854 = DIRECTION ( 'NONE',  ( 0.000000000000000000, 1.000000000000000000, -0.000000000000000000 ) ) ;
#66855 = DIRECTION ( 'NONE',  ( 0.000000000000000000, 1.000000000000000000, 0.000000000000000000 ) ) ;
#66856 = ORIENTED_EDGE ( 'NONE', *, *, #41585, .F. ) ;
#66857 = CARTESIAN_POINT ( 'NONE',  ( -131.0049999999999670, 6.826472737025115478, 4.959722759717899443 ) ) ;
#66858 = ORIENTED_EDGE ( 'NONE', *, *, #39693, .T. ) ;
#66859 = AXIS2_PLACEMENT_3D ( 'NONE', #54509, #16576, #53490 ) ;
#66860 = VERTEX_POINT ( 'NONE', #61950 ) ;
#66861 = DIRECTION ( 'NONE',  ( 0.000000000000000000, 0.000000000000000000, -1.000000000000000000 ) ) ;
#66862 = CARTESIAN_POINT ( 'NONE',  ( -83.54292637653381348, 9.058813317711329915, 2.943386871421369566 ) ) ;
#66863 = ORIENTED_EDGE ( 'NONE', *, *, #33369, .T. ) ;
#66864 = MECHANICAL_DESIGN_GEOMETRIC_PRESENTATION_REPRESENTATION (  '', ( #5079 ), #59019 ) ;
#66865 = FACE_OUTER_BOUND ( 'NONE', #41027, .T. ) ;
#66866 = CARTESIAN_POINT ( 'NONE',  ( 10.01517768586949231, 141.6949999999999363, 1.839758294383810543E-15 ) ) ;
#66867 =( NAMED_UNIT ( * ) SI_UNIT ( $, .STERADIAN. ) SOLID_ANGLE_UNIT ( ) );
#66868 = ORIENTED_EDGE ( 'NONE', *, *, #59363, .T. ) ;
#66869 = LINE ( 'NONE', #29912, #59949 ) ;
#66870 = CARTESIAN_POINT ( 'NONE',  ( 9.058813317711337021, 139.6550000000000011, 2.943386871421375783 ) ) ;
#66871 = DIRECTION ( 'NONE',  ( 0.000000000000000000, 0.000000000000000000, 1.000000000000000000 ) ) ;
#66872 = FACE_OUTER_BOUND ( 'NONE', #50577, .T. ) ;
#66873 = EDGE_LOOP ( 'NONE', ( #54331, #6219, #39009, #11659 ) ) ;
#66874 = CARTESIAN_POINT ( 'NONE',  ( -7.632228543268608334, 117.8429263765338249, 2.479861379858952830 ) ) ;
#66875 = DIRECTION ( 'NONE',  ( 0.000000000000000000, 0.000000000000000000, 1.000000000000000000 ) ) ;
#66876 = CARTESIAN_POINT ( 'NONE',  ( -87.44292637653380496, -1.166476076187852838E-15, -9.524999999999991473 ) ) ;
#66877 = DIRECTION ( 'NONE',  ( 1.000000000000000000, 0.000000000000000000, 0.000000000000000000 ) ) ;
#66878 = AXIS2_PLACEMENT_3D ( 'NONE', #4256, #25733, #21504 ) ;
#66879 = FACE_OUTER_BOUND ( 'NONE', #39018, .T. ) ;
#66880 = ORIENTED_EDGE ( 'NONE', *, *, #7013, .T. ) ;
#66881 = EDGE_CURVE ( 'NONE', #64131, #28127, #18010, .T. ) ;
#66882 = CARTESIAN_POINT ( 'NONE',  ( -0.4573008633723373850, -9.000000000000007105, 0.008766315107676130383 ) ) ;
#66883 = VERTEX_POINT ( 'NONE', #66188 ) ;
#66884 =( NAMED_UNIT ( * ) SI_UNIT ( $, .STERADIAN. ) SOLID_ANGLE_UNIT ( ) );
#66885 = CARTESIAN_POINT ( 'NONE',  ( -123.0570736234661808, 0.000000000000000000, 9.524999999999991473 ) ) ;
#66886 = FACE_OUTER_BOUND ( 'NONE', #30502, .T. ) ;
#66887 = CARTESIAN_POINT ( 'NONE',  ( -161.1550000000000011, 7.632228543268600340, 2.479861379858949277 ) ) ;
#66888 = ORIENTED_EDGE ( 'NONE', *, *, #51295, .T. ) ;
#66889 = CIRCLE ( 'NONE', #35445, 17.99999999999999645 ) ;
#66890 = EDGE_CURVE ( 'NONE', #42594, #16526, #56694, .T. ) ;
#66891 = EDGE_CURVE ( 'NONE', #51825, #41337, #30204, .T. ) ;
#66892 = DIRECTION ( 'NONE',  ( -0.000000000000000000, -0.000000000000000000, 1.000000000000000000 ) ) ;
#66893 =( NAMED_UNIT ( * ) PLANE_ANGLE_UNIT ( ) SI_UNIT ( $, .RADIAN. ) );
#66894 = ORIENTED_EDGE ( 'NONE', *, *, #57344, .F. ) ;
#66895 = EDGE_CURVE ( 'NONE', #9170, #60684, #16752, .T. ) ;
#66896 = EDGE_LOOP ( 'NONE', ( #23010, #67582, #15772, #16926 ) ) ;
#66897 = CARTESIAN_POINT ( 'NONE',  ( 24.00000000000000355, 36.75000000000000000, 3.000000000000000000 ) ) ;
#66898 = DIRECTION ( 'NONE',  ( -0.000000000000000000, 1.000000000000000000, -0.000000000000000000 ) ) ;
#66899 = CARTESIAN_POINT ( 'NONE',  ( -72.80499999999997840, -8.437984349512085203, 5.166775262442717831E-16 ) ) ;
#66900 = VERTEX_POINT ( 'NONE', #60550 ) ;
#66901 = EDGE_CURVE ( 'NONE', #69157, #23317, #12366, .T. ) ;
#66902 = EDGE_CURVE ( 'NONE', #48671, #7813, #29042, .T. ) ;
#66903 = SURFACE_SIDE_STYLE ('',( #23286 ) ) ;
#66904 = AXIS2_PLACEMENT_3D ( 'NONE', #39315, #34684, #61750 ) ;
#66905 = ADVANCED_FACE ( 'NONE', ( #23976 ), #34197, .F. ) ;
#66906 = CARTESIAN_POINT ( 'NONE',  ( -74.35506026930195844, 8.371839367610338201, -6.471715848474757671 ) ) ;
#66907 = ORIENTED_EDGE ( 'NONE', *, *, #44925, .T. ) ;
#66908 =( NAMED_UNIT ( * ) SI_UNIT ( $, .STERADIAN. ) SOLID_ANGLE_UNIT ( ) );
#66910 = DIRECTION ( 'NONE',  ( 0.000000000000000000, 0.000000000000000000, -1.000000000000000000 ) ) ;
#66909 = SURFACE_STYLE_USAGE ( .BOTH. , #18374 ) ;
#66911 = CARTESIAN_POINT ( 'NONE',  ( -9.058813317711337021, 143.0449999999999875, -2.943386871421374895 ) ) ;
#66912 = CARTESIAN_POINT ( 'NONE',  ( -106.0449999999999875, 7.632228543268600340, 2.479861379858949277 ) ) ;
#66913 = DIRECTION ( 'NONE',  ( 0.3420201433256663814, -0.9396926207859092051, 0.000000000000000000 ) ) ;
#66914 = CIRCLE ( 'NONE', #34312, 0.4999999999999994449 ) ;
#66915 = AXIS2_PLACEMENT_3D ( 'NONE', #22242, #23522, #56931 ) ;
#66916 = DIRECTION ( 'NONE',  ( 0.000000000000000000, -1.000000000000000000, -0.000000000000000000 ) ) ;
#66918 = DIRECTION ( 'NONE',  ( -0.000000000000000000, -0.000000000000000000, -1.000000000000000000 ) ) ;
#66917 = CARTESIAN_POINT ( 'NONE',  ( 54.49999999999999289, 2.470600640510329340E-15, -6.500000000000000000 ) ) ;
#66919 = CARTESIAN_POINT ( 'NONE',  ( -144.7429263765338021, -5.598654528085803328, -7.705886871421366635 ) ) ;
#66920 =( LENGTH_UNIT ( ) NAMED_UNIT ( * ) SI_UNIT ( .MILLI., .METRE. ) );
#66921 = CARTESIAN_POINT ( 'NONE',  ( -164.9949999999999761, -6.826472737025115478, 4.959722759717900331 ) ) ;
#66922 = AXIS2_PLACEMENT_3D ( 'NONE', #33449, #66138, #22551 ) ;
#66923 = B_SPLINE_CURVE_WITH_KNOTS ( 'NONE', 3,
 ( #1576, #60703, #54730, #17152, #851, #23102 ),
 .UNSPECIFIED., .F., .F.,
 ( 4, 2, 4 ),
 ( 0.004189585287972440175, 0.006269578072783811573, 0.008349570857595182971 ),
 .UNSPECIFIED. ) ;
#66924 = DIRECTION ( 'NONE',  ( -1.000000000000000000, 0.000000000000000000, 0.000000000000000000 ) ) ;
#66925 = AXIS2_PLACEMENT_3D ( 'NONE', #20041, #67557, #36280 ) ;
#66926 = DIRECTION ( 'NONE',  ( 0.000000000000000000, 0.000000000000000000, -1.000000000000000000 ) ) ;
#66927 = ORIENTED_EDGE ( 'NONE', *, *, #42064, .F. ) ;
#66928 = CARTESIAN_POINT ( 'NONE',  ( -7.632228543268607446, 127.6570736234661467, -2.479861379858953718 ) ) ;
#66929 = ORIENTED_EDGE ( 'NONE', *, *, #53162, .T. ) ;
#66930 = CIRCLE ( 'NONE', #44432, 0.5000000000000004441 ) ;
#66931 =( NAMED_UNIT ( * ) PLANE_ANGLE_UNIT ( ) SI_UNIT ( $, .RADIAN. ) );
#66932 = EDGE_CURVE ( 'NONE', #22147, #30954, #46995, .T. ) ;
#66933 = CIRCLE ( 'NONE', #13489, 0.5000000000000004441 ) ;
#66934 = FILL_AREA_STYLE_COLOUR ( '', #30394 ) ;
#66935 = CARTESIAN_POINT ( 'NONE',  ( -45.50000000000000000, 7.768687147774683943, 6.500000000000000888 ) ) ;
#66936 = CARTESIAN_POINT ( 'NONE',  ( 12.25000000000002132, 7.083454193571968087E-15, 4.000000000000000000 ) ) ;
#66937 = CARTESIAN_POINT ( 'NONE',  ( 23.71231517720798010, 113.4999999999999858, -7.500000000000000000 ) ) ;
#66938 = EDGE_LOOP ( 'NONE', ( #15175, #63247, #69281, #50428 ) ) ;
#66939 = CARTESIAN_POINT ( 'NONE',  ( -165.2049999999999841, -2.607480562269071545, -8.024999999999991473 ) ) ;
#66940 = ORIENTED_EDGE ( 'NONE', *, *, #9944, .T. ) ;
#66941 = CARTESIAN_POINT ( 'NONE',  ( -190.0000000000000000, 9.184850993605132167E-16, -7.499999999999985789 ) ) ;
#66942 = CYLINDRICAL_SURFACE ( 'NONE', #42222, 0.2500000000000002220 ) ;
#66943 = EDGE_LOOP ( 'NONE', ( #23267, #37998, #14279, #49134 ) ) ;
#66944 = CARTESIAN_POINT ( 'NONE',  ( 0.000000000000000000, 30.74999999999998579, 4.000000000000000000 ) ) ;
#66945 = SURFACE_SIDE_STYLE ('',( #60587 ) ) ;
#66946 = CARTESIAN_POINT ( 'NONE',  ( 10.01517768586949231, 114.6949999999999932, 1.839758294383810543E-15 ) ) ;
#66947 = ORIENTED_EDGE ( 'NONE', *, *, #66048, .F. ) ;
#66948 = FACE_OUTER_BOUND ( 'NONE', #47545, .T. ) ;
#66949 = CARTESIAN_POINT ( 'NONE',  ( -78.80500000000000682, -8.437984349512086979, 5.166775262442717831E-16 ) ) ;
#66950 = CARTESIAN_POINT ( 'NONE',  ( 0.000000000000000000, 134.5549999999999784, -9.525000000000000355 ) ) ;
#66951 = CARTESIAN_POINT ( 'NONE',  ( 2.607480562269034241, 132.9070736234661467, -8.025000000000032330 ) ) ;
#66952 = CARTESIAN_POINT ( 'NONE',  ( 20.99077900071323199, 114.7777241159145518, 10.00000000000000000 ) ) ;
#66953 = EDGE_CURVE ( 'NONE', #34565, #28179, #4590, .T. ) ;
#66954 = CARTESIAN_POINT ( 'NONE',  ( -113.1570736234661751, -9.058813317711329915, -2.943386871421370898 ) ) ;
#66955 = PRESENTATION_LAYER_ASSIGNMENT (  '', '', ( #10810 ) ) ;
#66956 = AXIS2_PLACEMENT_3D ( 'NONE', #10889, #42271, #16545 ) ;
#66957 = ORIENTED_EDGE ( 'NONE', *, *, #42530, .T. ) ;
#66958 = PRESENTATION_LAYER_ASSIGNMENT (  '', '', ( #57929 ) ) ;
#66959 = FACE_OUTER_BOUND ( 'NONE', #7791, .T. ) ;
#66960 = FILL_AREA_STYLE ('',( #13124 ) ) ;
#66961 = CARTESIAN_POINT ( 'NONE',  ( -49.94499999999998607, -9.827790563157499189E-16, -8.024999999999991473 ) ) ;
#66962 = ORIENTED_EDGE ( 'NONE', *, *, #41098, .F. ) ;
#66963 = SURFACE_STYLE_FILL_AREA ( #66246 ) ;
#66964 = EDGE_CURVE ( 'NONE', #9321, #42390, #47586, .T. ) ;
#66965 =( BOUNDED_CURVE ( )  B_SPLINE_CURVE ( 3, ( #34038, #21763, #44644, #54450 ),
 .UNSPECIFIED., .F., .F. ) 
 B_SPLINE_CURVE_WITH_KNOTS ( ( 4, 4 ),
 ( 4.712388980384689674, 6.283185307179586232 ),
 .UNSPECIFIED. ) 
 CURVE ( )  GEOMETRIC_REPRESENTATION_ITEM ( )  RATIONAL_B_SPLINE_CURVE ( ( 1.000000000000000000, 0.8047378541243649375, 0.8047378541243649375, 1.000000000000000000 ) ) 
 REPRESENTATION_ITEM ( '' )  );
#66966 = CARTESIAN_POINT ( 'NONE',  ( 0.000000000000000000, 120.0249999999999773, 0.000000000000000000 ) ) ;
#66967 = CARTESIAN_POINT ( 'NONE',  ( 69.99999999999998579, 8.572527594031471415E-15, 3.000000000000000000 ) ) ;
#66968 = DIRECTION ( 'NONE',  ( 1.000000000000000000, 0.000000000000000000, 0.000000000000000000 ) ) ;
#66969 = ORIENTED_EDGE ( 'NONE', *, *, #41088, .T. ) ;
#66970 = CARTESIAN_POINT ( 'NONE',  ( -49.91467138050326469, -10.97405843795318070, 3.683894230925336633 ) ) ;
#66971 = CARTESIAN_POINT ( 'NONE',  ( -57.59499999999997755, 2.607480562269072433, 8.024999999999991473 ) ) ;
#66972 = ORIENTED_EDGE ( 'NONE', *, *, #58867, .T. ) ;
#66973 = VECTOR ( 'NONE', #15153, 1000.000000000000000 ) ;
#66974 = CARTESIAN_POINT ( 'NONE',  ( -74.99999999999998579, 8.119648659858185624, 6.397056658262309625 ) ) ;
#66975 = CARTESIAN_POINT ( 'NONE',  ( -105.0549999999999926, -9.827790563157499189E-16, -8.024999999999991473 ) ) ;
#66976 = EDGE_LOOP ( 'NONE', ( #67200, #7845, #59519, #10045 ) ) ;
#66977 = DIRECTION ( 'NONE',  ( -1.000000000000000000, -0.000000000000000000, -0.000000000000000000 ) ) ;
#66978 = EDGE_CURVE ( 'NONE', #16387, #28040, #556, .T. ) ;
#66979 = CARTESIAN_POINT ( 'NONE',  ( 40.49999999999998579, 107.7459666924148252, 10.00000000000000000 ) ) ;
#66980 = CARTESIAN_POINT ( 'NONE',  ( 17.00000000000000711, 27.99999999999998224, 4.000000000000000000 ) ) ;
#66981 = CARTESIAN_POINT ( 'NONE',  ( -137.3070736234661808, -10.01517768586948698, 6.132527647946031529E-16 ) ) ;
#66982 = DIRECTION ( 'NONE',  ( 0.000000000000000000, -1.000000000000000000, 0.000000000000000000 ) ) ;
#66983 = CARTESIAN_POINT ( 'NONE',  ( -3.094860106618434248, 140.7950000000000159, 9.525000000000000355 ) ) ;
#66984 =( GEOMETRIC_REPRESENTATION_CONTEXT ( 3 ) GLOBAL_UNCERTAINTY_ASSIGNED_CONTEXT ( ( #61510 ) ) GLOBAL_UNIT_ASSIGNED_CONTEXT ( ( #760, #64163, #33209 ) ) REPRESENTATION_CONTEXT ( 'NONE', 'WORKASPACE' ) );
#66985 = CARTESIAN_POINT ( 'NONE',  ( -86.30707362346615241, -10.01517768586948698, 6.132527647946031529E-16 ) ) ;
#66986 = EDGE_CURVE ( 'NONE', #28960, #24001, #58418, .T. ) ;
#66987 = PLANE ( 'NONE',  #20426 ) ;
#66988 = SURFACE_STYLE_USAGE ( .BOTH. , #45567 ) ;
#66989 = FILL_AREA_STYLE ('',( #28965 ) ) ;
#66990 = CARTESIAN_POINT ( 'NONE',  ( -119.1550000000000011, 7.632228543268600340, 2.479861379858949277 ) ) ;
#66991 = CARTESIAN_POINT ( 'NONE',  ( 23.50000000000041211, 24.55989583709592949, -27.18999999999997286 ) ) ;
#66992 =( NAMED_UNIT ( * ) SI_UNIT ( $, .STERADIAN. ) SOLID_ANGLE_UNIT ( ) );
#66993 = CARTESIAN_POINT ( 'NONE',  ( -131.3949999999999818, -6.826472737025115478, -4.959722759717899443 ) ) ;
#66994 = CARTESIAN_POINT ( 'NONE',  ( -123.5949999999999704, 2.607480562269072433, 8.024999999999991473 ) ) ;
#66995 = FACE_OUTER_BOUND ( 'NONE', #49301, .T. ) ;
#66996 = ORIENTED_EDGE ( 'NONE', *, *, #69657, .T. ) ;
#66997 = DIRECTION ( 'NONE',  ( 0.000000000000000000, 0.000000000000000000, -1.000000000000000000 ) ) ;
#66998 =( NAMED_UNIT ( * ) SI_UNIT ( $, .STERADIAN. ) SOLID_ANGLE_UNIT ( ) );
#66999 = CYLINDRICAL_SURFACE ( 'NONE', #40672, 23.00000000000000000 ) ;
#67000 = CARTESIAN_POINT ( 'NONE',  ( -170.9929263765337737, 8.102448949553171076, -5.886773742842744461 ) ) ;
#67001 =( LENGTH_UNIT ( ) NAMED_UNIT ( * ) SI_UNIT ( .MILLI., .METRE. ) );
#67002 = CARTESIAN_POINT ( 'NONE',  ( -49.64499999999999602, 4.716976649647091513, -6.492361379858946790 ) ) ;
#67003 = CIRCLE ( 'NONE', #25414, 0.5000000000000004441 ) ;
#67004 = CARTESIAN_POINT ( 'NONE',  ( -66.44292637653380496, -1.166476076187852838E-15, -9.524999999999991473 ) ) ;
#67005 = MECHANICAL_DESIGN_GEOMETRIC_PRESENTATION_REPRESENTATION (  '', ( #53545 ), #68159 ) ;
#67006 = DIRECTION ( 'NONE',  ( -1.000000000000000000, -0.000000000000000000, -0.000000000000000000 ) ) ;
#67007 = LINE ( 'NONE', #55754, #3110 ) ;
#67008 = LINE ( 'NONE', #18799, #48492 ) ;
#67009 = ORIENTED_EDGE ( 'NONE', *, *, #57162, .F. ) ;
#67010 = CARTESIAN_POINT ( 'NONE',  ( -96.29292637653381348, 3.094860106618428031, -9.524999999999993250 ) ) ;
#67011 = APPLICATION_PROTOCOL_DEFINITION ( 'draft international standard', 'automotive_design', 1998, #32476 ) ;
#67012 = FILL_AREA_STYLE ('',( #67700 ) ) ;
#67013 = DIRECTION ( 'NONE',  ( 1.000000000000000000, 0.000000000000000000, 0.000000000000000000 ) ) ;
#67014 = EDGE_CURVE ( 'NONE', #18409, #17310, #68288, .T. ) ;
#67015 = CARTESIAN_POINT ( 'NONE',  ( -179.0929263765338817, 3.094860106619634177, 9.524999999999119282 ) ) ;
#67016 = CARTESIAN_POINT ( 'NONE',  ( 6.826472737025121695, 123.6070736234661496, -4.959722759717905660 ) ) ;
#67017 = CARTESIAN_POINT ( 'NONE',  ( -78.35707362346616378, 5.598654528085804216, 7.705886871421366635 ) ) ;
#67018 = AXIS2_PLACEMENT_3D ( 'NONE', #41438, #42849, #31538 ) ;
#67019 = FILL_AREA_STYLE_COLOUR ( '', #39537 ) ;
#67020 = ORIENTED_EDGE ( 'NONE', *, *, #20697, .F. ) ;
#67021 = CARTESIAN_POINT ( 'NONE',  ( -13.23915246117191025, 52.65078610323165265, -2.000000000000000000 ) ) ;
#67022 = CARTESIAN_POINT ( 'NONE',  ( 60.00000000000000000, 1.797044900979284448E-15, -11.50000000000000000 ) ) ;
#67023 = VERTEX_POINT ( 'NONE', #42304 ) ;
#67024 = DIRECTION ( 'NONE',  ( -1.000000000000000000, 0.000000000000000000, 0.000000000000000000 ) ) ;
#67025 = CARTESIAN_POINT ( 'NONE',  ( -2.607480562269073765, 133.2070736234661013, -8.025000000000000355 ) ) ;
#67026 = EDGE_CURVE ( 'NONE', #31792, #25558, #53666, .T. ) ;
#67027 = DIRECTION ( 'NONE',  ( -0.000000000000000000, -0.000000000000000000, 1.000000000000000000 ) ) ;
#67028 = FILL_AREA_STYLE ('',( #13539 ) ) ;
#67029 = DIRECTION ( 'NONE',  ( 1.000000000000000000, 0.000000000000000000, 0.000000000000000000 ) ) ;
#67030 = EDGE_LOOP ( 'NONE', ( #13386, #24648, #41687, #27440 ) ) ;
#67031 = DIRECTION ( 'NONE',  ( -1.000000000000000000, 0.000000000000000000, 0.000000000000000000 ) ) ;
#67032 = EDGE_CURVE ( 'NONE', #5967, #12255, #10243, .T. ) ;
#67033 = EDGE_CURVE ( 'NONE', #54480, #21322, #25584, .T. ) ;
#67034 = CARTESIAN_POINT ( 'NONE',  ( 7.632228543268608334, 150.4570736234661581, -2.479861379858951942 ) ) ;
#67035 = FACE_OUTER_BOUND ( 'NONE', #1283, .T. ) ;
#67036 = DIRECTION ( 'NONE',  ( -1.000000000000000000, 0.000000000000000000, 0.000000000000000000 ) ) ;
#67037 = CARTESIAN_POINT ( 'NONE',  ( -85.34499999999998465, 7.632228543268599452, -2.479861379858951942 ) ) ;
#67038 = ORIENTED_EDGE ( 'NONE', *, *, #36163, .T. ) ;
#67039 = DIRECTION ( 'NONE',  ( -0.3420201433256663814, 0.9396926207859092051, 0.000000000000000000 ) ) ;
#67040 = FACE_OUTER_BOUND ( 'NONE', #51640, .T. ) ;
#67041 = EDGE_CURVE ( 'NONE', #14317, #35896, #61526, .T. ) ;
#67042 =( NAMED_UNIT ( * ) SI_UNIT ( $, .STERADIAN. ) SOLID_ANGLE_UNIT ( ) );
#67043 = UNCERTAINTY_MEASURE_WITH_UNIT (LENGTH_MEASURE( 1.000000000000000082E-05 ), #13061, 'distance_accuracy_value', 'NONE');
#67044 = VERTEX_POINT ( 'NONE', #35938 ) ;
#67045 = EDGE_CURVE ( 'NONE', #8875, #13986, #4231, .T. ) ;
#67046 = CIRCLE ( 'NONE', #43500, 0.2500000000000002220 ) ;
#67047 = PRESENTATION_STYLE_ASSIGNMENT (( #9352 ) ) ;
#67048 = ORIENTED_EDGE ( 'NONE', *, *, #61237, .T. ) ;
#67049 = CIRCLE ( 'NONE', #53586, 0.5000000000000004441 ) ;
#67050 = CYLINDRICAL_SURFACE ( 'NONE', #20683, 9.524999999999991473 ) ;
#67051 = ORIENTED_EDGE ( 'NONE', *, *, #53677, .F. ) ;
#67053 = EDGE_CURVE ( 'NONE', #18813, #32327, #52597, .T. ) ;
#67052 = MECHANICAL_DESIGN_GEOMETRIC_PRESENTATION_REPRESENTATION (  '', ( #56956 ), #61399 ) ;
#67054 = FACE_OUTER_BOUND ( 'NONE', #20588, .T. ) ;
#67055 = FILL_AREA_STYLE ('',( #40007 ) ) ;
#67056 = CARTESIAN_POINT ( 'NONE',  ( -165.5070736234661126, 8.102448949553176405, 5.886773742842740909 ) ) ;
#67057 = DIRECTION ( 'NONE',  ( 0.000000000000000000, -1.000000000000000000, 0.000000000000000000 ) ) ;
#67058 = LINE ( 'NONE', #57174, #57723 ) ;
#67059 = CARTESIAN_POINT ( 'NONE',  ( -114.3570736234661780, 5.598654528085804216, 7.705886871421366635 ) ) ;
#67060 = CARTESIAN_POINT ( 'NONE',  ( -183.1155613406150167, 5.490944093040150520, -7.649849691780579164 ) ) ;
#67061 = EDGE_CURVE ( 'NONE', #12165, #48372, #14134, .T. ) ;
#67062 = DIRECTION ( 'NONE',  ( -0.000000000000000000, -0.000000000000000000, 1.000000000000000000 ) ) ;
#67063 = ORIENTED_EDGE ( 'NONE', *, *, #37950, .T. ) ;
#67064 = DIRECTION ( 'NONE',  ( -1.000000000000000000, -0.000000000000000000, -0.000000000000000000 ) ) ;
#67065 = CARTESIAN_POINT ( 'NONE',  ( -74.50000000000000000, -2.220952357103124925E-14, -9.500000000000000000 ) ) ;
#67066 = CYLINDRICAL_SURFACE ( 'NONE', #49223, 1.000000000000000888 ) ;
#67067 = MECHANICAL_DESIGN_GEOMETRIC_PRESENTATION_REPRESENTATION (  '', ( #58094 ), #39022 ) ;
#67068 = CARTESIAN_POINT ( 'NONE',  ( -150.3549999999999898, -4.716976649647093289, -6.492361379858945902 ) ) ;
#67069 = CARTESIAN_POINT ( 'NONE',  ( -75.00000000000000000, 8.164352767049518178, 6.987111781054302639 ) ) ;
#67070 = CARTESIAN_POINT ( 'NONE',  ( -6.854883122194315170, 111.1401193526694726, -5.667071715363107387 ) ) ;
#67071 = CARTESIAN_POINT ( 'NONE',  ( -167.8449999999999989, -7.632228543268599452, 2.479861379858951054 ) ) ;
#67072 = CARTESIAN_POINT ( 'NONE',  ( -148.4949999999999761, 6.826472737025113702, -4.959722759717902107 ) ) ;
#67073 = ORIENTED_EDGE ( 'NONE', *, *, #9902, .T. ) ;
#67074 = CARTESIAN_POINT ( 'NONE',  ( 8.701243704650551081, -2.329718218673044738, -2.929003814506405678 ) ) ;
#67075 = CARTESIAN_POINT ( 'NONE',  ( -66.95499999999998408, -7.632228543268599452, 2.479861379858951054 ) ) ;
#67076 = DIRECTION ( 'NONE',  ( -1.300977106640434891E-16, 0.000000000000000000, -1.000000000000000000 ) ) ;
#67077 = CARTESIAN_POINT ( 'NONE',  ( -67.19499999999999318, 8.437984349512086979, -1.550032578732815448E-15 ) ) ;
#67078 = CARTESIAN_POINT ( 'NONE',  ( 5.598654528085805993, 145.3549999999999898, 7.705886871421374629 ) ) ;
#67079 = CARTESIAN_POINT ( 'NONE',  ( 60.49999999999998579, 50.00000000000000000, 6.999999999999999112 ) ) ;
#67080 = SURFACE_STYLE_USAGE ( .BOTH. , #2996 ) ;
#67081 = UNCERTAINTY_MEASURE_WITH_UNIT (LENGTH_MEASURE( 1.000000000000000082E-05 ), #48697, 'distance_accuracy_value', 'NONE');
#67082 = CARTESIAN_POINT ( 'NONE',  ( 17.75000000000000711, 30.74999999999999289, 4.000000000000000000 ) ) ;
#67083 = CYLINDRICAL_SURFACE ( 'NONE', #10234, 1.000000000000000000 ) ;
#67084 =( LENGTH_UNIT ( ) NAMED_UNIT ( * ) SI_UNIT ( .MILLI., .METRE. ) );
#67085 = DIRECTION ( 'NONE',  ( -0.000000000000000000, 1.000000000000000000, -0.000000000000000000 ) ) ;
#67086 = AXIS2_PLACEMENT_3D ( 'NONE', #43558, #20674, #64258 ) ;
#67087 = VECTOR ( 'NONE', #32014, 1000.000000000000000 ) ;
#67088 = CARTESIAN_POINT ( 'NONE',  ( 23.50000000000001776, 14.00000000000000000, -29.68999999999999417 ) ) ;
#67089 = DIRECTION ( 'NONE',  ( -0.000000000000000000, -0.000000000000000000, -1.000000000000000000 ) ) ;
#67090 = CARTESIAN_POINT ( 'NONE',  ( 0.000000000000000000, 114.9999999999999574, 0.000000000000000000 ) ) ;
#67091 = ORIENTED_EDGE ( 'NONE', *, *, #50364, .F. ) ;
#67092 = ORIENTED_EDGE ( 'NONE', *, *, #61308, .T. ) ;
#67093 = CARTESIAN_POINT ( 'NONE',  ( 48.49999999999999289, 24.99999999999998579, 3.750000000000000000 ) ) ;
#67094 = EDGE_CURVE ( 'NONE', #69289, #18031, #41237, .T. ) ;
#67095 =( NAMED_UNIT ( * ) PLANE_ANGLE_UNIT ( ) SI_UNIT ( $, .RADIAN. ) );
#67097 = ADVANCED_FACE ( 'NONE', ( #25364 ), #45622, .T. ) ;
#67096 = LINE ( 'NONE', #45341, #17283 ) ;
#67098 = EDGE_LOOP ( 'NONE', ( #62086, #60111, #61452, #58640 ) ) ;
#67099 = VERTEX_POINT ( 'NONE', #38995 ) ;
#67100 = DIRECTION ( 'NONE',  ( 1.000000000000000000, 0.000000000000000000, 0.000000000000000000 ) ) ;
#67101 = COLOUR_RGB ( '', 0.40784314, 0.44705882, 0.49803922) ;
#67102 = ADVANCED_FACE ( 'NONE', ( #43923 ), #5353, .F. ) ;
#67103 = ORIENTED_EDGE ( 'NONE', *, *, #22979, .F. ) ;
#67104 = CARTESIAN_POINT ( 'NONE',  ( -66.29292637653379927, 3.094860106618428031, -9.524999999999993250 ) ) ;
#67105 = DIRECTION ( 'NONE',  ( 0.000000000000000000, 0.000000000000000000, 1.000000000000000000 ) ) ;
#67106 = VERTEX_POINT ( 'NONE', #11868 ) ;
#67107 =( NAMED_UNIT ( * ) SI_UNIT ( $, .STERADIAN. ) SOLID_ANGLE_UNIT ( ) );
#67108 = PLANE ( 'NONE',  #48583 ) ;
#67109 = CARTESIAN_POINT ( 'NONE',  ( -113.9949999999999903, -6.826472737025115478, 4.959722759717900331 ) ) ;
#67110 = VERTEX_POINT ( 'NONE', #7295 ) ;
#67111 = APPLICATION_CONTEXT ( 'automotive_design' ) ;
#67112 = DIRECTION ( 'NONE',  ( 0.000000000000000000, 0.000000000000000000, 1.000000000000000000 ) ) ;
#67113 = CARTESIAN_POINT ( 'NONE',  ( -10.03253578442417115, -11.98633051154418183, 0.6595741458992528949 ) ) ;
#67114 = CARTESIAN_POINT ( 'NONE',  ( 12.72792206135785698, 114.9999999999999574, 10.50000000000000000 ) ) ;
#67115 = ORIENTED_EDGE ( 'NONE', *, *, #56882, .F. ) ;
#67116 = CARTESIAN_POINT ( 'NONE',  ( -6.826472737025120807, 144.9929263765337737, 4.959722759717906548 ) ) ;
#67117 = CYLINDRICAL_SURFACE ( 'NONE', #43652, 0.5000000000000004441 ) ;
#67118 = CYLINDRICAL_SURFACE ( 'NONE', #6561, 0.2500000000000002220 ) ;
#67119 = EDGE_CURVE ( 'NONE', #22594, #8864, #28722, .T. ) ;
#67120 = DIRECTION ( 'NONE',  ( 0.000000000000000000, 0.000000000000000000, 1.000000000000000000 ) ) ;
#67121 = DIRECTION ( 'NONE',  ( -0.000000000000000000, -1.000000000000000000, -0.000000000000000000 ) ) ;
#67122 = ORIENTED_EDGE ( 'NONE', *, *, #24509, .F. ) ;
#67123 = EDGE_LOOP ( 'NONE', ( #55007, #46826, #40241, #5338 ) ) ;
#67124 =( GEOMETRIC_REPRESENTATION_CONTEXT ( 3 ) GLOBAL_UNCERTAINTY_ASSIGNED_CONTEXT ( ( #36873 ) ) GLOBAL_UNIT_ASSIGNED_CONTEXT ( ( #68256, #50092, #20764 ) ) REPRESENTATION_CONTEXT ( 'NONE', 'WORKASPACE' ) );
#67125 = LINE ( 'NONE', #25251, #28756 ) ;
#67126 = CARTESIAN_POINT ( 'NONE',  ( -133.7049999999999557, 2.607480562269073321, 8.024999999999991473 ) ) ;
#67127 = CARTESIAN_POINT ( 'NONE',  ( 25.00000000000001421, 42.00000000000000000, 0.000000000000000000 ) ) ;
#67128 = VERTEX_POINT ( 'NONE', #61090 ) ;
#67129 = PRESENTATION_STYLE_ASSIGNMENT (( #19630 ) ) ;
#67130 = DIRECTION ( 'NONE',  ( -1.000000000000000000, -0.000000000000000000, -0.000000000000000000 ) ) ;
#67131 = DIRECTION ( 'NONE',  ( -0.3162277660168378857, 0.9486832980505138790, 0.000000000000000000 ) ) ;
#67132 = CARTESIAN_POINT ( 'NONE',  ( -6.826472737025120807, 120.3929263765338220, -4.959722759717907437 ) ) ;
#67133 = ORIENTED_EDGE ( 'NONE', *, *, #5230, .F. ) ;
#67134 = CIRCLE ( 'NONE', #43588, 0.2500000000000002220 ) ;
#67135 = ORIENTED_EDGE ( 'NONE', *, *, #55269, .T. ) ;
#67136 = CIRCLE ( 'NONE', #30026, 3.600000000000005862 ) ;
#67137 = CARTESIAN_POINT ( 'NONE',  ( -30.38818854855176355, -7.808010524275851516, -1.023245363186933155 ) ) ;
#67138 = CARTESIAN_POINT ( 'NONE',  ( 29.00000000000000000, 43.00000000000000000, -79.00402776293826435 ) ) ;
#67139 = DIRECTION ( 'NONE',  ( -0.000000000000000000, -0.000000000000000000, -1.000000000000000000 ) ) ;
#67140 = ORIENTED_EDGE ( 'NONE', *, *, #11634, .T. ) ;
#67141 = CARTESIAN_POINT ( 'NONE',  ( -179.7549999999999955, 4.716976649647091513, -6.492361379858946790 ) ) ;
#67142 = DIRECTION ( 'NONE',  ( 0.000000000000000000, -1.000000000000000000, 0.000000000000000000 ) ) ;
#67143 = ADVANCED_FACE ( 'NONE', ( #27670 ), #50212, .T. ) ;
#67144 = DIRECTION ( 'NONE',  ( 0.000000000000000000, 0.000000000000000000, -1.000000000000000000 ) ) ;
#67145 = CARTESIAN_POINT ( 'NONE',  ( -54.95707362346616520, 9.058813317711329915, -2.943386871421373119 ) ) ;
#67146 =( NAMED_UNIT ( * ) PLANE_ANGLE_UNIT ( ) SI_UNIT ( $, .RADIAN. ) );
#67147 = EDGE_CURVE ( 'NONE', #4422, #45200, #65336, .T. ) ;
#67148 = CARTESIAN_POINT ( 'NONE',  ( 71.50000000000000000, 14.49137674618942562, -7.500000000000000000 ) ) ;
#67149 = EDGE_LOOP ( 'NONE', ( #64721, #40942, #25387 ) ) ;
#67150 =( BOUNDED_CURVE ( )  B_SPLINE_CURVE ( 2, ( #54487, #938, #22491, #56919, #9090, #39733, #51301, #56564, #14345, #61154, #50604 ),
 .UNSPECIFIED., .F., .F. ) 
 B_SPLINE_CURVE_WITH_KNOTS ( ( 3, 2, 2, 2, 2, 3 ),
 ( 0.1739130434782567292, 0.1760869565217349497, 0.1782608695652131703, 0.1804347826086913908, 0.1826086956521696114, 0.1847826086956478042 ),
 .UNSPECIFIED. ) 
 CURVE ( )  GEOMETRIC_REPRESENTATION_ITEM ( )  RATIONAL_B_SPLINE_CURVE ( ( 1.000000000000093037, 0.9510565162950602724, 1.000000000000000000, 0.9510565162951535312, 1.000000000000000000, 0.9510565162951535312, 1.000000000000000000, 0.9510565162951535312, 1.000000000000000000, 0.9510565162952516749, 0.9999999999999018563 ) ) 
 REPRESENTATION_ITEM ( '' )  );
#67151 = CYLINDRICAL_SURFACE ( 'NONE', #31297, 8.999999999999994671 ) ;
#67152 = CARTESIAN_POINT ( 'NONE',  ( 31.00000000000000000, 43.00000000000000000, -80.00402776293826435 ) ) ;
#67153 = CARTESIAN_POINT ( 'NONE',  ( -105.6549999999999869, -7.632228543268600340, -2.479861379858950166 ) ) ;
#67154 = CARTESIAN_POINT ( 'NONE',  ( -74.49999999999998579, 119.9999999999997726, 9.500000000000000000 ) ) ;
#67155 = CYLINDRICAL_SURFACE ( 'NONE', #46095, 1.000000000000000888 ) ;
#67157 = LINE ( 'NONE', #35844, #44974 ) ;
#67156 = TOROIDAL_SURFACE ( 'NONE', #3013, 111.0000000000000142, 1.000000000000000000 ) ;
#67158 = PRESENTATION_LAYER_ASSIGNMENT (  '', '', ( #27808 ) ) ;
#67159 = CARTESIAN_POINT ( 'NONE',  ( -100.0450000000000017, 7.632228543268600340, 2.479861379858949277 ) ) ;
#67160 = CARTESIAN_POINT ( 'NONE',  ( -8.102448949553181734, 117.0049999999999670, -5.886773742842749790 ) ) ;
#67161 = CARTESIAN_POINT ( 'NONE',  ( -65.24499999999999034, -4.716976649647093289, -6.492361379858945902 ) ) ;
#67162 = DIRECTION ( 'NONE',  ( 0.000000000000000000, -1.000000000000000000, 0.000000000000000000 ) ) ;
#67163 =( NAMED_UNIT ( * ) PLANE_ANGLE_UNIT ( ) SI_UNIT ( $, .RADIAN. ) );
#67164 = UNCERTAINTY_MEASURE_WITH_UNIT (LENGTH_MEASURE( 1.000000000000000082E-05 ), #35708, 'distance_accuracy_value', 'NONE');
#67165 =( NAMED_UNIT ( * ) PLANE_ANGLE_UNIT ( ) SI_UNIT ( $, .RADIAN. ) );
#67166 =( NAMED_UNIT ( * ) PLANE_ANGLE_UNIT ( ) SI_UNIT ( $, .RADIAN. ) );
#67167 = EDGE_LOOP ( 'NONE', ( #43860, #65109 ) ) ;
#67168 = CARTESIAN_POINT ( 'NONE',  ( -112.0429263765337993, -9.058813317711329915, -2.943386871421370898 ) ) ;
#67169 = CARTESIAN_POINT ( 'NONE',  ( -142.4949999999999761, 6.826472737025113702, -4.959722759717902107 ) ) ;
#67170 = CARTESIAN_POINT ( 'NONE',  ( 86.21825843581756033, 5.000000000000000000, 39.83014742847163348 ) ) ;
#67171 = EDGE_CURVE ( 'NONE', #41931, #529, #816, .T. ) ;
#67172 = DIRECTION ( 'NONE',  ( 0.000000000000000000, 0.000000000000000000, -1.000000000000000000 ) ) ;
#67173 = LINE ( 'NONE', #23233, #36210 ) ;
#67174 = EDGE_LOOP ( 'NONE', ( #23774, #69488, #17911, #44339 ) ) ;
#67175 = ORIENTED_EDGE ( 'NONE', *, *, #24418, .F. ) ;
#67176 = DIRECTION ( 'NONE',  ( 0.000000000000000000, 0.000000000000000000, 1.000000000000000000 ) ) ;
#67177 =( NAMED_UNIT ( * ) SI_UNIT ( $, .STERADIAN. ) SOLID_ANGLE_UNIT ( ) );
#67178 = DIRECTION ( 'NONE',  ( -1.000000000000000000, -0.000000000000000000, -0.000000000000000000 ) ) ;
#67179 = AXIS2_PLACEMENT_3D ( 'NONE', #63493, #15344, #12425 ) ;
#67180 = CARTESIAN_POINT ( 'NONE',  ( -6.062177826491071286, 3.500000000000000888, 0.000000000000000000 ) ) ;
#67181 = FACE_OUTER_BOUND ( 'NONE', #64841, .T. ) ;
#67182 = ORIENTED_EDGE ( 'NONE', *, *, #53310, .F. ) ;
#67183 = CARTESIAN_POINT ( 'NONE',  ( -134.9050000000000011, 2.607480562269069324, -8.024999999999993250 ) ) ;
#67184 = ORIENTED_EDGE ( 'NONE', *, *, #40528, .F. ) ;
#67185 = CARTESIAN_POINT ( 'NONE',  ( -125.4570736234661723, -9.058813317711329915, 2.943386871421371787 ) ) ;
#67186 = ADVANCED_FACE ( 'NONE', ( #18544 ), #56867, .T. ) ;
#67187 = ORIENTED_EDGE ( 'NONE', *, *, #11122, .T. ) ;
#67188 = CARTESIAN_POINT ( 'NONE',  ( 44.25000000000000000, 21.99999999999998579, -3.750000000000000000 ) ) ;
#67189 = VERTEX_POINT ( 'NONE', #41060 ) ;
#67190 = VECTOR ( 'NONE', #24412, 1000.000000000000000 ) ;
#67191 = DIRECTION ( 'NONE',  ( 1.000000000000000000, -0.000000000000000000, -0.000000000000000000 ) ) ;
#67192 = LINE ( 'NONE', #19698, #23091 ) ;
#67193 = CARTESIAN_POINT ( 'NONE',  ( 3.094860106618435136, 136.2949999999999875, -9.525000000000000355 ) ) ;
#67194 = FILL_AREA_STYLE_COLOUR ( '', #3605 ) ;
#67195 = ORIENTED_EDGE ( 'NONE', *, *, #42075, .T. ) ;
#67196 = FILL_AREA_STYLE ('',( #45777 ) ) ;
#67197 = CARTESIAN_POINT ( 'NONE',  ( -8.102448949553179958, 138.6049999999999613, 5.886773742842747126 ) ) ;
#67198 =( NAMED_UNIT ( * ) PLANE_ANGLE_UNIT ( ) SI_UNIT ( $, .RADIAN. ) );
#67199 = DIRECTION ( 'NONE',  ( 1.000000000000000000, 0.000000000000000000, 0.000000000000000000 ) ) ;
#67200 = ORIENTED_EDGE ( 'NONE', *, *, #35241, .F. ) ;
#67201 = CARTESIAN_POINT ( 'NONE',  ( -6.826472737025120807, 114.3929263765337936, -4.959722759717907437 ) ) ;
#67202 = DIRECTION ( 'NONE',  ( -1.000000000000000000, 0.000000000000000000, 0.000000000000000000 ) ) ;
#67203 = UNCERTAINTY_MEASURE_WITH_UNIT (LENGTH_MEASURE( 1.000000000000000082E-05 ), #25480, 'distance_accuracy_value', 'NONE');
#67204 = AXIS2_PLACEMENT_3D ( 'NONE', #3985, #46967, #33 ) ;
#67205 = CARTESIAN_POINT ( 'NONE',  ( -195.0000000000000000, 0.000000000000000000, 0.000000000000000000 ) ) ;
#67206 = EDGE_CURVE ( 'NONE', #13013, #11295, #7621, .T. ) ;
#67207 = PRESENTATION_STYLE_ASSIGNMENT (( #29204 ) ) ;
#67208 = PRESENTATION_STYLE_ASSIGNMENT (( #8811 ) ) ;
#67209 = EDGE_LOOP ( 'NONE', ( #63823, #54050, #34681, #64052 ) ) ;
#67210 = DIRECTION ( 'NONE',  ( 0.000000000000000000, 0.000000000000000000, 1.000000000000000000 ) ) ;
#67211 = ORIENTED_EDGE ( 'NONE', *, *, #37480, .F. ) ;
#67212 = DIRECTION ( 'NONE',  ( 0.000000000000000000, -1.000000000000000000, 0.000000000000000000 ) ) ;
#67213 = CARTESIAN_POINT ( 'NONE',  ( -31.73356630351995733, -8.286794552894653165, -1.921513618645009913 ) ) ;
#67214 = CARTESIAN_POINT ( 'NONE',  ( -51.15237142740936349, -10.37588836492439448, 4.088776396995604578 ) ) ;
#67215 = CARTESIAN_POINT ( 'NONE',  ( -162.9549999999999841, -7.632228543268599452, 2.479861379858951054 ) ) ;
#67216 = ORIENTED_EDGE ( 'NONE', *, *, #8587, .F. ) ;
#67217 = FACE_OUTER_BOUND ( 'NONE', #68795, .T. ) ;
#67218 = UNCERTAINTY_MEASURE_WITH_UNIT (LENGTH_MEASURE( 1.000000000000000082E-05 ), #43924, 'distance_accuracy_value', 'NONE');
#67219 = VECTOR ( 'NONE', #55903, 1000.000000000000000 ) ;
#67220 =( NAMED_UNIT ( * ) PLANE_ANGLE_UNIT ( ) SI_UNIT ( $, .RADIAN. ) );
#67221 = CARTESIAN_POINT ( 'NONE',  ( 48.50000000000000000, 13.41640786499872284, -7.500000000000000000 ) ) ;
#67222 = VERTEX_POINT ( 'NONE', #45307 ) ;
#67223 =( NAMED_UNIT ( * ) PLANE_ANGLE_UNIT ( ) SI_UNIT ( $, .RADIAN. ) );
#67224 = VERTEX_POINT ( 'NONE', #2988 ) ;
#67225 = SURFACE_STYLE_FILL_AREA ( #45803 ) ;
#67226 = DIRECTION ( 'NONE',  ( 0.000000000000000000, 0.000000000000000000, -1.000000000000000000 ) ) ;
#67227 = CARTESIAN_POINT ( 'NONE',  ( -72.20499999999998408, -2.607480562269071545, -8.024999999999991473 ) ) ;
#67228 = EDGE_LOOP ( 'NONE', ( #45864, #19447, #64624, #43313 ) ) ;
#67229 = DIRECTION ( 'NONE',  ( 0.000000000000000000, -0.000000000000000000, 1.000000000000000000 ) ) ;
#67230 = VECTOR ( 'NONE', #20471, 1000.000000000000000 ) ;
#67231 = CARTESIAN_POINT ( 'NONE',  ( -63.05707362346617373, 0.000000000000000000, 9.524999999999991473 ) ) ;
#67232 = DIRECTION ( 'NONE',  ( -0.000000000000000000, 1.000000000000000000, -0.000000000000000000 ) ) ;
#67233 = AXIS2_PLACEMENT_3D ( 'NONE', #59674, #47818, #48481 ) ;
#67234 = CARTESIAN_POINT ( 'NONE',  ( -75.00000000000000000, 8.062885781073912739, -5.999999999999991118 ) ) ;
#67235 = ORIENTED_EDGE ( 'NONE', *, *, #22642, .T. ) ;
#67236 = CARTESIAN_POINT ( 'NONE',  ( 22.41829134511430155, 26.69040202514700866, -27.43543867392220648 ) ) ;
#67237 = AXIS2_PLACEMENT_3D ( 'NONE', #43408, #44087, #26783 ) ;
#67239 = DIRECTION ( 'NONE',  ( 0.000000000000000000, 1.350863103983176297E-16, -1.000000000000000000 ) ) ;
#67238 = CARTESIAN_POINT ( 'NONE',  ( 1.000000000000000000, 1.000000000000000222, -3.000000000000000000 ) ) ;
#67240 = PRESENTATION_LAYER_ASSIGNMENT (  '', '', ( #41412 ) ) ;
#67241 = CARTESIAN_POINT ( 'NONE',  ( 3.094860106618435136, 139.2949999999999591, -9.525000000000000355 ) ) ;
#67242 = CARTESIAN_POINT ( 'NONE',  ( -109.0449999999999875, 7.632228543268600340, 2.479861379858949277 ) ) ;
#67243 = LINE ( 'NONE', #61956, #44330 ) ;
#67244 = MECHANICAL_DESIGN_GEOMETRIC_PRESENTATION_REPRESENTATION (  '', ( #5406 ), #54817 ) ;
#67245 = UNCERTAINTY_MEASURE_WITH_UNIT (LENGTH_MEASURE( 1.000000000000000082E-05 ), #26996, 'distance_accuracy_value', 'NONE');
#67246 = VECTOR ( 'NONE', #60361, 1000.000000000000000 ) ;
#67248 = DIRECTION ( 'NONE',  ( 1.000000000000000000, 0.000000000000000000, 0.000000000000000000 ) ) ;
#67247 = CARTESIAN_POINT ( 'NONE',  ( 1.000000000000000000, 43.00000000000000000, 80.00402776293826435 ) ) ;
#67249 = CARTESIAN_POINT ( 'NONE',  ( -139.9429263765337907, 0.000000000000000000, 9.524999999999991473 ) ) ;
#67250 = CARTESIAN_POINT ( 'NONE',  ( -165.5949999999999704, 2.607480562269073321, 8.024999999999991473 ) ) ;
#67251 = COLOUR_RGB ( '', 0.09019608, 0.27058824, 0.51372549) ;
#67252 = FILL_AREA_STYLE ('',( #62649 ) ) ;
#67253 = EDGE_CURVE ( 'NONE', #57014, #15803, #51583, .T. ) ;
#67254 = DIRECTION ( 'NONE',  ( -1.000000000000000000, 0.000000000000000000, 0.000000000000000000 ) ) ;
#67255 = ORIENTED_EDGE ( 'NONE', *, *, #22431, .F. ) ;
#67256 = DIRECTION ( 'NONE',  ( -0.000000000000000000, -1.000000000000000000, 0.000000000000000000 ) ) ;
#67257 = ORIENTED_EDGE ( 'NONE', *, *, #27614, .F. ) ;
#67258 = EDGE_CURVE ( 'NONE', #48671, #64454, #2277, .T. ) ;
#67259 = UNCERTAINTY_MEASURE_WITH_UNIT (LENGTH_MEASURE( 1.000000000000000082E-05 ), #62298, 'distance_accuracy_value', 'NONE');
#67260 = DIRECTION ( 'NONE',  ( 0.9704308468600219006, 0.2413793103448194366, 0.000000000000000000 ) ) ;
#67261 = ADVANCED_FACE ( 'NONE', ( #40712 ), #67768, .F. ) ;
#67262 = DIRECTION ( 'NONE',  ( -1.000000000000000000, 0.000000000000000000, 0.000000000000000000 ) ) ;
#67263 =( GEOMETRIC_REPRESENTATION_CONTEXT ( 3 ) GLOBAL_UNCERTAINTY_ASSIGNED_CONTEXT ( ( #47540 ) ) GLOBAL_UNIT_ASSIGNED_CONTEXT ( ( #52883, #11680, #44443 ) ) REPRESENTATION_CONTEXT ( 'NONE', 'WORKASPACE' ) );
#67264 = ORIENTED_EDGE ( 'NONE', *, *, #49196, .T. ) ;
#67265 = CARTESIAN_POINT ( 'NONE',  ( -165.0550000000000068, -9.827790563157499189E-16, -8.024999999999991473 ) ) ;
#67266 = EDGE_CURVE ( 'NONE', #52535, #29977, #7977, .T. ) ;
#67267 = ORIENTED_EDGE ( 'NONE', *, *, #36363, .F. ) ;
#67268 = DIRECTION ( 'NONE',  ( -0.000000000000000000, 1.000000000000000000, -0.000000000000000000 ) ) ;
#67269 =( NAMED_UNIT ( * ) PLANE_ANGLE_UNIT ( ) SI_UNIT ( $, .RADIAN. ) );
#67271 = EDGE_CURVE ( 'NONE', #36102, #6580, #60388, .T. ) ;
#67270 = EDGE_LOOP ( 'NONE', ( #60893, #32356, #20912 ) ) ;
#67272 = CIRCLE ( 'NONE', #23471, 0.2500000000000002220 ) ;
#67273 = CARTESIAN_POINT ( 'NONE',  ( 19.89974874213240597, 115.4999999999999574, 10.00000000000000000 ) ) ;
#67274 = ADVANCED_FACE ( 'NONE', ( #29784 ), #35056, .T. ) ;
#67275 =( NAMED_UNIT ( * ) PLANE_ANGLE_UNIT ( ) SI_UNIT ( $, .RADIAN. ) );
#67276 = CARTESIAN_POINT ( 'NONE',  ( -10.01517768586949231, 113.1949999999999790, -6.132527647946036459E-16 ) ) ;
#67277 = STYLED_ITEM ( 'NONE', ( #37159 ), #4526 ) ;
#67278 = ORIENTED_EDGE ( 'NONE', *, *, #13976, .F. ) ;
#67279 = CARTESIAN_POINT ( 'NONE',  ( 35.99999999999999289, 0.000000000000000000, -24.00402776293825369 ) ) ;
#67281 = EDGE_CURVE ( 'NONE', #67128, #55864, #40208, .T. ) ;
#67280 = DIRECTION ( 'NONE',  ( 0.000000000000000000, 0.000000000000000000, 1.000000000000000000 ) ) ;
#67282 = CARTESIAN_POINT ( 'NONE',  ( -76.40499999999997272, -2.607480562269069768, 8.024999999999991473 ) ) ;
#67283 = CARTESIAN_POINT ( 'NONE',  ( -2.607480562269095969, 122.4070736234661609, 8.024999999999986144 ) ) ;
#67284 = ORIENTED_EDGE ( 'NONE', *, *, #51697, .F. ) ;
#67285 = CARTESIAN_POINT ( 'NONE',  ( 10.01517768586949231, 142.8049999999999500, 1.839758294383810543E-15 ) ) ;
#67286 = UNCERTAINTY_MEASURE_WITH_UNIT (LENGTH_MEASURE( 1.000000000000000082E-05 ), #13781, 'distance_accuracy_value', 'NONE');
#67287 = SURFACE_STYLE_USAGE ( .BOTH. , #51820 ) ;
#67288 = STYLED_ITEM ( 'NONE', ( #20813 ), #51194 ) ;
#67289 = VECTOR ( 'NONE', #3601, 1000.000000000000000 ) ;
#67290 = FILL_AREA_STYLE_COLOUR ( '', #63577 ) ;
#67291 = SURFACE_STYLE_USAGE ( .BOTH. , #2872 ) ;
#67292 = FACE_OUTER_BOUND ( 'NONE', #4585, .T. ) ;
#67293 = CARTESIAN_POINT ( 'NONE',  ( 3.000000000000003109, 42.58578643762690774, -80.00402776293826435 ) ) ;
#67294 = ORIENTED_EDGE ( 'NONE', *, *, #29463, .F. ) ;
#67295 =( GEOMETRIC_REPRESENTATION_CONTEXT ( 3 ) GLOBAL_UNCERTAINTY_ASSIGNED_CONTEXT ( ( #37688 ) ) GLOBAL_UNIT_ASSIGNED_CONTEXT ( ( #12808, #65934, #17765 ) ) REPRESENTATION_CONTEXT ( 'NONE', 'WORKASPACE' ) );
#67296 =( NAMED_UNIT ( * ) PLANE_ANGLE_UNIT ( ) SI_UNIT ( $, .RADIAN. ) );
#67297 = CARTESIAN_POINT ( 'NONE',  ( -49.04499999999998039, 7.632228543268600340, 2.479861379858949277 ) ) ;
#67298 = ORIENTED_EDGE ( 'NONE', *, *, #5886, .F. ) ;
#67299 = FACE_BOUND ( 'NONE', #338, .T. ) ;
#67300 = MECHANICAL_DESIGN_GEOMETRIC_PRESENTATION_REPRESENTATION (  '', ( #21232 ), #24590 ) ;
#67301 = CARTESIAN_POINT ( 'NONE',  ( 0.000000000000000000, 0.000000000000000000, 7.500000000000000000 ) ) ;
#67302 = CARTESIAN_POINT ( 'NONE',  ( 31.00000000000000000, 42.00000000000000000, -75.00000000000001421 ) ) ;
#67303 = VERTEX_POINT ( 'NONE', #4064 ) ;
#67304 = CARTESIAN_POINT ( 'NONE',  ( -55.64499999999997470, 4.716976649647091513, -6.492361379858946790 ) ) ;
#67305 = CARTESIAN_POINT ( 'NONE',  ( -23.71231517720798010, 118.4999999999999716, -7.500000000000000000 ) ) ;
#67306 = ORIENTED_EDGE ( 'NONE', *, *, #33550, .T. ) ;
#67307 = VECTOR ( 'NONE', #7614, 1000.000000000000000 ) ;
#67308 = CARTESIAN_POINT ( 'NONE',  ( -102.5049999999999955, -6.826472737025115478, -4.959722759717899443 ) ) ;
#67309 = ORIENTED_EDGE ( 'NONE', *, *, #17869, .F. ) ;
#67310 = FACE_BOUND ( 'NONE', #5946, .T. ) ;
#67311 = CARTESIAN_POINT ( 'NONE',  ( -138.0570736234661808, 0.000000000000000000, 9.524999999999991473 ) ) ;
#67312 = PRESENTATION_STYLE_ASSIGNMENT (( #34597 ) ) ;
#67313 = CARTESIAN_POINT ( 'NONE',  ( 8.102448949553181734, 141.9950000000000045, -5.886773742842746238 ) ) ;
#67314 = CARTESIAN_POINT ( 'NONE',  ( -79.25707362346618368, 5.598654528085800663, -7.705886871421367523 ) ) ;
#67315 = AXIS2_PLACEMENT_3D ( 'NONE', #2563, #40266, #28639 ) ;
#67316 = CARTESIAN_POINT ( 'NONE',  ( 21.02379604162863913, 114.4999999999999574, 10.00000000000000000 ) ) ;
#67317 = CARTESIAN_POINT ( 'NONE',  ( -16.31094249435444254, -10.98238678365111021, -4.836562941872261767 ) ) ;
#67319 = CARTESIAN_POINT ( 'NONE',  ( -100.4929263765337879, -8.102448949553174629, 5.886773742842742685 ) ) ;
#67318 = DIRECTION ( 'NONE',  ( -0.000000000000000000, -0.000000000000000000, -1.000000000000000000 ) ) ;
#67320 = CIRCLE ( 'NONE', #25728, 0.5000000000000004441 ) ;
#67321 = CARTESIAN_POINT ( 'NONE',  ( -117.5049999999999670, -6.826472737025115478, -4.959722759717899443 ) ) ;
#67322 = DIRECTION ( 'NONE',  ( 0.000000000000000000, 1.000000000000000000, -0.000000000000000000 ) ) ;
#67323 = CARTESIAN_POINT ( 'NONE',  ( -136.1949999999999363, 8.437984349512085203, -1.550032578732815448E-15 ) ) ;
#67324 = PRESENTATION_LAYER_ASSIGNMENT (  '', '', ( #47131 ) ) ;
#67325 = CARTESIAN_POINT ( 'NONE',  ( -123.2949999999999875, -2.607480562269069768, 8.024999999999991473 ) ) ;
#67326 = DIRECTION ( 'NONE',  ( -1.000000000000000000, 0.000000000000000000, 0.000000000000000000 ) ) ;
#67327 = MECHANICAL_DESIGN_GEOMETRIC_PRESENTATION_REPRESENTATION (  '', ( #51605 ), #2119 ) ;
#67328 = ORIENTED_EDGE ( 'NONE', *, *, #6279, .T. ) ;
#67329 = PRESENTATION_LAYER_ASSIGNMENT (  '', '', ( #4382 ) ) ;
#67330 = LINE ( 'NONE', #39248, #2073 ) ;
#67331 = MECHANICAL_DESIGN_GEOMETRIC_PRESENTATION_REPRESENTATION (  '', ( #69585 ), #35911 ) ;
#67332 = DIRECTION ( 'NONE',  ( 0.000000000000000000, 0.000000000000000000, 1.000000000000000000 ) ) ;
#67333 = DIRECTION ( 'NONE',  ( 0.000000000000000000, 0.000000000000000000, 1.000000000000000000 ) ) ;
#67334 = CARTESIAN_POINT ( 'NONE',  ( -174.7429263765338305, -5.598654528085803328, -7.705886871421366635 ) ) ;
#67335 =( NAMED_UNIT ( * ) PLANE_ANGLE_UNIT ( ) SI_UNIT ( $, .RADIAN. ) );
#67336 = CARTESIAN_POINT ( 'NONE',  ( -50.09499999999996334, -2.607480562269071545, -8.024999999999991473 ) ) ;
#67337 = AXIS2_PLACEMENT_3D ( 'NONE', #2030, #33769, #66481 ) ;
#67338 = EDGE_CURVE ( 'NONE', #4398, #41529, #24409, .T. ) ;
#67339 = FACE_OUTER_BOUND ( 'NONE', #3939, .T. ) ;
#67340 = DIRECTION ( 'NONE',  ( -0.000000000000000000, -0.000000000000000000, 1.000000000000000000 ) ) ;
#67341 = EDGE_LOOP ( 'NONE', ( #4545, #23394, #51760, #8967 ) ) ;
#67342 = CARTESIAN_POINT ( 'NONE',  ( -84.14292637653379359, 5.598654528085800663, -7.705886871421367523 ) ) ;
#67343 = ITEM_DEFINED_TRANSFORMATION ( 'NONE', 'NONE', #53976,  #42840 ) ;
#67344 = COLOUR_RGB ( '', 0.09019608, 0.27058824, 0.51372549) ;
#67345 = EDGE_CURVE ( 'NONE', #37946, #39825, #69492, .T. ) ;
#67346 = DIRECTION ( 'NONE',  ( 0.000000000000000000, 0.000000000000000000, -1.000000000000000000 ) ) ;
#67347 = CARTESIAN_POINT ( 'NONE',  ( -179.6929263765337907, 10.01517768586948698, -1.839758294383808966E-15 ) ) ;
#67348 = CARTESIAN_POINT ( 'NONE',  ( -78.50707362346616947, 8.102448949553176405, 5.886773742842740909 ) ) ;
#67349 = AXIS2_PLACEMENT_3D ( 'NONE', #10753, #32200, #53647 ) ;
#67350 = ORIENTED_EDGE ( 'NONE', *, *, #23980, .T. ) ;
#67351 = CARTESIAN_POINT ( 'NONE',  ( -136.7929263765344103, -3.094860106608278816, 9.525000000007368683 ) ) ;
#67352 = CARTESIAN_POINT ( 'NONE',  ( -74.99999999999998579, 50.00000000000000000, 9.500000000000000000 ) ) ;
#67353 = EDGE_CURVE ( 'NONE', #29444, #6055, #118, .T. ) ;
#67354 =( NAMED_UNIT ( * ) SI_UNIT ( $, .STERADIAN. ) SOLID_ANGLE_UNIT ( ) );
#67355 = ORIENTED_EDGE ( 'NONE', *, *, #66235, .T. ) ;
#67356 = CARTESIAN_POINT ( 'NONE',  ( -64.04292637653379927, -9.058813317711329915, -2.943386871421370898 ) ) ;
#67357 = TOROIDAL_SURFACE ( 'NONE', #10078, 6.000000000000000000, 1.000000000000000000 ) ;
#67358 = CARTESIAN_POINT ( 'NONE',  ( 2.607480562269076430, 132.9070736234661183, -8.025000000000000355 ) ) ;
#67359 = ORIENTED_EDGE ( 'NONE', *, *, #50456, .T. ) ;
#67361 = EDGE_CURVE ( 'NONE', #34747, #2790, #41329, .T. ) ;
#67360 = FACE_OUTER_BOUND ( 'NONE', #29511, .T. ) ;
#67362 = PLANE ( 'NONE',  #54157 ) ;
#67364 = EDGE_LOOP ( 'NONE', ( #64241, #16488, #48023, #28941 ) ) ;
#67363 = COLOUR_RGB ( '', 0.08235294, 0.09019608, 0.10196078) ;
#67365 = CARTESIAN_POINT ( 'NONE',  ( -94.34292637653379643, -9.058813317711329915, 2.943386871421371787 ) ) ;
#67366 = CARTESIAN_POINT ( 'NONE',  ( 15.98999599679679839, 146.4999999999999716, -7.500000000000000000 ) ) ;
#67367 = CARTESIAN_POINT ( 'NONE',  ( -9.000000000000003553, 24.99999999999998579, 3.750000000000000000 ) ) ;
#67368 =( LENGTH_UNIT ( ) NAMED_UNIT ( * ) SI_UNIT ( .MILLI., .METRE. ) );
#67369 = CIRCLE ( 'NONE', #8983, 3.000000000000000444 ) ;
#67370 = VECTOR ( 'NONE', #52615, 1000.000000000000000 ) ;
#67371 = LINE ( 'NONE', #2235, #18257 ) ;
#67372 = CARTESIAN_POINT ( 'NONE',  ( -77.69499999999999318, -8.437984349512085203, 5.166775262442717831E-16 ) ) ;
#67374 = ORIENTED_EDGE ( 'NONE', *, *, #18970, .F. ) ;
#67373 = VECTOR ( 'NONE', #37035, 1000.000000000000000 ) ;
#67375 = DIRECTION ( 'NONE',  ( 1.000000000000000000, 0.000000000000000000, 0.000000000000000000 ) ) ;
#67376 = VECTOR ( 'NONE', #5092, 1000.000000000000000 ) ;
#67377 = EDGE_LOOP ( 'NONE', ( #60669, #35906, #68349, #31675 ) ) ;
#67378 = FILL_AREA_STYLE_COLOUR ( '', #17920 ) ;
#67379 = VECTOR ( 'NONE', #63196, 1000.000000000000000 ) ;
#67380 = FILL_AREA_STYLE ('',( #56840 ) ) ;
#67381 = LINE ( 'NONE', #24799, #35729 ) ;
#67382 = ORIENTED_EDGE ( 'NONE', *, *, #9666, .T. ) ;
#67383 = SURFACE_SIDE_STYLE ('',( #45958 ) ) ;
#67384 = ORIENTED_EDGE ( 'NONE', *, *, #52011, .T. ) ;
#67385 = SURFACE_STYLE_USAGE ( .BOTH. , #57532 ) ;
#67386 = SURFACE_SIDE_STYLE ('',( #60707 ) ) ;
#67388 = STYLED_ITEM ( 'NONE', ( #69660 ), #15314 ) ;
#67387 = DIRECTION ( 'NONE',  ( 0.000000000000000000, 0.000000000000000000, -1.000000000000000000 ) ) ;
#67389 = CARTESIAN_POINT ( 'NONE',  ( -173.7570736234661695, -5.598654528085801552, 7.705886871421367523 ) ) ;
#67390 = LINE ( 'NONE', #35397, #38786 ) ;
#67391 = CARTESIAN_POINT ( 'NONE',  ( -1.166476076187854022E-15, 113.9449999999999932, 9.525000000000000355 ) ) ;
#67392 = CARTESIAN_POINT ( 'NONE',  ( -117.5070736234661553, 8.102448949553176405, 5.886773742842740909 ) ) ;
#67393 = EDGE_CURVE ( 'NONE', #25423, #46060, #8705, .T. ) ;
#67394 =( LENGTH_UNIT ( ) NAMED_UNIT ( * ) SI_UNIT ( .MILLI., .METRE. ) );
#67395 = CARTESIAN_POINT ( 'NONE',  ( 0.000000000000000000, 0.000000000000000000, 0.000000000000000000 ) ) ;
#67396 = ORIENTED_EDGE ( 'NONE', *, *, #63133, .F. ) ;
#67397 =( GEOMETRIC_REPRESENTATION_CONTEXT ( 3 ) GLOBAL_UNCERTAINTY_ASSIGNED_CONTEXT ( ( #5124 ) ) GLOBAL_UNIT_ASSIGNED_CONTEXT ( ( #49961, #50982, #60817 ) ) REPRESENTATION_CONTEXT ( 'NONE', 'WORKASPACE' ) );
#67398 = CARTESIAN_POINT ( 'NONE',  ( 7.632228543268607446, 122.0429263765338135, 2.479861379858954606 ) ) ;
#67400 = CARTESIAN_POINT ( 'NONE',  ( -114.0570736234661808, 0.000000000000000000, 9.524999999999991473 ) ) ;
#67399 = DIRECTION ( 'NONE',  ( -1.000000000000000000, 0.000000000000000000, 0.000000000000000000 ) ) ;
#67401 = CARTESIAN_POINT ( 'NONE',  ( -150.6549999999999727, -7.632228543268600340, -2.479861379858950166 ) ) ;
#67402 = DIRECTION ( 'NONE',  ( 0.000000000000000000, 0.000000000000000000, -1.000000000000000000 ) ) ;
#67403 = CARTESIAN_POINT ( 'NONE',  ( -166.0449999999999875, 7.632228543268600340, 2.479861379858949277 ) ) ;
#67404 = CARTESIAN_POINT ( 'NONE',  ( -150.7449999999999761, 4.716976649647094177, 6.492361379858945902 ) ) ;
#67405 = COLOUR_RGB ( '', 0.66274510, 0.83137255, 0.94901961) ;
#67406 = VERTEX_POINT ( 'NONE', #42462 ) ;
#67407 = CARTESIAN_POINT ( 'NONE',  ( 71.74137931034481142, 36.89918356738973415, 10.00000000000000000 ) ) ;
#67408 = COLOUR_RGB ( '', 0.66274510, 0.83137255, 0.94901961) ;
#67409 = CARTESIAN_POINT ( 'NONE',  ( -65.45499999999998408, 7.632228543268599452, -2.479861379858951942 ) ) ;
#67410 = DIRECTION ( 'NONE',  ( -1.000000000000000000, 4.336808689941999001E-16, -0.000000000000000000 ) ) ;
#67411 = FACE_OUTER_BOUND ( 'NONE', #23496, .T. ) ;
#67412 = ADVANCED_FACE ( 'NONE', ( #47765 ), #59257, .T. ) ;
#67413 = CARTESIAN_POINT ( 'NONE',  ( -64.94499999999999318, -9.827790563157499189E-16, -8.024999999999991473 ) ) ;
#67414 = EDGE_CURVE ( 'NONE', #35956, #49132, #63520, .T. ) ;
#67415 = CARTESIAN_POINT ( 'NONE',  ( 0.000000000000000000, 155.5550000000000068, -9.525000000000000355 ) ) ;
#67416 = PRESENTATION_LAYER_ASSIGNMENT (  '', '', ( #46118 ) ) ;
#67417 = TOROIDAL_SURFACE ( 'NONE', #16889, 0.5000000000000000000, 0.2500000000000000000 ) ;
#67418 = CARTESIAN_POINT ( 'NONE',  ( -160.2570736234661979, 5.598654528085800663, -7.705886871421367523 ) ) ;
#67419 = CARTESIAN_POINT ( 'NONE',  ( 5.603568002170367102, 8.294335516573697831, 0.9848892659495218638 ) ) ;
#67420 = ADVANCED_FACE ( 'NONE', ( #15700 ), #67156, .T. ) ;
#67421 = MECHANICAL_DESIGN_GEOMETRIC_PRESENTATION_REPRESENTATION (  '', ( #40497 ), #41600 ) ;
#67422 = AXIS2_PLACEMENT_3D ( 'NONE', #48790, #42828, #69174 ) ;
#67423 = FILL_AREA_STYLE ('',( #41779 ) ) ;
#67424 = DIRECTION ( 'NONE',  ( -0.000000000000000000, -1.000000000000000000, -0.000000000000000000 ) ) ;
#67425 = ADVANCED_FACE ( 'NONE', ( #64572 ), #10421, .F. ) ;
#67426 = FACE_OUTER_BOUND ( 'NONE', #47816, .T. ) ;
#67427 = ORIENTED_EDGE ( 'NONE', *, *, #32409, .F. ) ;
#67428 = MECHANICAL_DESIGN_GEOMETRIC_PRESENTATION_REPRESENTATION (  '', ( #19115 ), #32572 ) ;
#67429 = ORIENTED_EDGE ( 'NONE', *, *, #15745, .T. ) ;
#67430 = LINE ( 'NONE', #45335, #49841 ) ;
#67431 = CARTESIAN_POINT ( 'NONE',  ( 3.728455551740340823, -1.573594397638760745, -7.000000000000004441 ) ) ;
#67433 = ADVANCED_FACE ( 'NONE', ( #16748 ), #49782, .F. ) ;
#67432 = SURFACE_SIDE_STYLE ('',( #35782 ) ) ;
#67434 = DIRECTION ( 'NONE',  ( -0.000000000000000000, -0.000000000000000000, 1.000000000000000000 ) ) ;
#67435 = AXIS2_PLACEMENT_3D ( 'NONE', #60729, #34014, #33334 ) ;
#67436 = ORIENTED_EDGE ( 'NONE', *, *, #8185, .F. ) ;
#67437 = VERTEX_POINT ( 'NONE', #22346 ) ;
#67438 = DIRECTION ( 'NONE',  ( 0.000000000000000000, 0.000000000000000000, 1.000000000000000000 ) ) ;
#67439 = ORIENTED_EDGE ( 'NONE', *, *, #58166, .F. ) ;
#67440 = CARTESIAN_POINT ( 'NONE',  ( 22.00000000000002132, 42.00000000000000000, 75.00000000000000000 ) ) ;
#67441 = CARTESIAN_POINT ( 'NONE',  ( -144.4429263765337907, -1.166476076187852838E-15, -9.524999999999991473 ) ) ;
#67442 = ORIENTED_EDGE ( 'NONE', *, *, #32272, .T. ) ;
#67444 = CARTESIAN_POINT ( 'NONE',  ( 61.74999999999998579, 30.74999999999999289, 3.750000000000000000 ) ) ;
#67443 =( GEOMETRIC_REPRESENTATION_CONTEXT ( 3 ) GLOBAL_UNCERTAINTY_ASSIGNED_CONTEXT ( ( #51688 ) ) GLOBAL_UNIT_ASSIGNED_CONTEXT ( ( #62567, #51341, #25970 ) ) REPRESENTATION_CONTEXT ( 'NONE', 'WORKASPACE' ) );
#67445 = DIRECTION ( 'NONE',  ( 1.000000000000000000, 0.000000000000000000, 0.000000000000000000 ) ) ;
#67446 = CARTESIAN_POINT ( 'NONE',  ( -111.8949999999999960, 6.826472737025116366, 4.959722759717898555 ) ) ;
#67447 = ORIENTED_EDGE ( 'NONE', *, *, #2671, .F. ) ;
#67448 = CARTESIAN_POINT ( 'NONE',  ( 48.00000000000000000, 14.49137674618942562, 7.500000000000000000 ) ) ;
#67449 =( NAMED_UNIT ( * ) SI_UNIT ( $, .STERADIAN. ) SOLID_ANGLE_UNIT ( ) );
#67450 =( GEOMETRIC_REPRESENTATION_CONTEXT ( 3 ) GLOBAL_UNCERTAINTY_ASSIGNED_CONTEXT ( ( #22698 ) ) GLOBAL_UNIT_ASSIGNED_CONTEXT ( ( #16278, #44414, #6023 ) ) REPRESENTATION_CONTEXT ( 'NONE', 'WORKASPACE' ) );
#67451 = COLOUR_RGB ( '', 0.40784314, 0.44705882, 0.49803922) ;
#67452 = CARTESIAN_POINT ( 'NONE',  ( -179.1570736234662036, -9.058813317711329915, -2.943386871421370898 ) ) ;
#67453 = VERTEX_POINT ( 'NONE', #65947 ) ;
#67454 = CARTESIAN_POINT ( 'NONE',  ( 4.716976649647096842, 148.7429263765338021, 6.492361379858953896 ) ) ;
#67455 = LINE ( 'NONE', #61467, #27757 ) ;
#67456 = FACE_OUTER_BOUND ( 'NONE', #5846, .T. ) ;
#67457 = CARTESIAN_POINT ( 'NONE',  ( 39.74999999999999289, 16.24999999999997513, -3.750000000000000000 ) ) ;
#67458 =( LENGTH_UNIT ( ) NAMED_UNIT ( * ) SI_UNIT ( .MILLI., .METRE. ) );
#67459 = ORIENTED_EDGE ( 'NONE', *, *, #32392, .F. ) ;
#67460 = VECTOR ( 'NONE', #8187, 1000.000000000000227 ) ;
#67461 = PRESENTATION_STYLE_ASSIGNMENT (( #29107 ) ) ;
#67462 = ORIENTED_EDGE ( 'NONE', *, *, #55276, .T. ) ;
#67463 = FILL_AREA_STYLE ('',( #45019 ) ) ;
#67464 = CARTESIAN_POINT ( 'NONE',  ( -45.89905495956740111, 9.405628579031729330, 3.102072197697236966 ) ) ;
#67465 = DIRECTION ( 'NONE',  ( 0.4468085106382997385, 0.000000000000000000, -0.8946296187927071930 ) ) ;
#67466 = CARTESIAN_POINT ( 'NONE',  ( -60.00000000000000000, -2.024042244987997205E-14, 7.500000000000000000 ) ) ;
#67467 = CARTESIAN_POINT ( 'NONE',  ( -128.4549999999999841, 7.632228543268599452, -2.479861379858951942 ) ) ;
#67468 = DIRECTION ( 'NONE',  ( 1.000000000000000000, 0.000000000000000000, -0.000000000000000000 ) ) ;
#67469 = PRESENTATION_LAYER_ASSIGNMENT (  '', '', ( #68645 ) ) ;
#67470 = CARTESIAN_POINT ( 'NONE',  ( 2.607480562268946311, 140.7070736234661581, 8.025000000000092726 ) ) ;
#67471 = DIRECTION ( 'NONE',  ( -0.000000000000000000, -0.000000000000000000, -1.000000000000000000 ) ) ;
#67472 = ADVANCED_FACE ( 'NONE', ( #27929 ), #22008, .T. ) ;
#67473 = STYLED_ITEM ( 'NONE', ( #47240 ), #53652 ) ;
#67474 = CARTESIAN_POINT ( 'NONE',  ( -74.50000000000001421, 36.50926243676796190, 10.00000000000000000 ) ) ;
#67475 = CARTESIAN_POINT ( 'NONE',  ( 8.319377385370872346, -3.000000000000000888, 12.50000000000000000 ) ) ;
#67476 = ORIENTED_EDGE ( 'NONE', *, *, #41274, .T. ) ;
#67477 = STYLED_ITEM ( 'NONE', ( #33521 ), #52450 ) ;
#67478 = ORIENTED_EDGE ( 'NONE', *, *, #32902, .F. ) ;
#67479 = SURFACE_SIDE_STYLE ('',( #30171 ) ) ;
#67480 = FACE_OUTER_BOUND ( 'NONE', #847, .T. ) ;
#67481 = CARTESIAN_POINT ( 'NONE',  ( -48.95499999999996987, -7.632228543268599452, 2.479861379858951054 ) ) ;
#67482 = ORIENTED_EDGE ( 'NONE', *, *, #61431, .F. ) ;
#67483 = CARTESIAN_POINT ( 'NONE',  ( -123.3570736234661780, 5.598654528085804216, 7.705886871421366635 ) ) ;
#67484 = CARTESIAN_POINT ( 'NONE',  ( -182.6049999999999613, 6.826472737025113702, -4.959722759717902107 ) ) ;
#67485 = DIRECTION ( 'NONE',  ( -1.000000000000000000, -0.000000000000000000, -0.000000000000000000 ) ) ;
#67486 = CARTESIAN_POINT ( 'NONE',  ( -58.10707362346618510, 8.102448949553171076, -5.886773742842744461 ) ) ;
#67487 = CARTESIAN_POINT ( 'NONE',  ( -179.5450000000000159, -7.632228543268600340, -2.479861379858950166 ) ) ;
#67488 = CIRCLE ( 'NONE', #37205, 8.499999999999992895 ) ;
#67489 = ORIENTED_EDGE ( 'NONE', *, *, #11675, .F. ) ;
#67490 = EDGE_LOOP ( 'NONE', ( #22664, #26343, #69126, #21285 ) ) ;
#67491 = CARTESIAN_POINT ( 'NONE',  ( -74.69168400679268416, 36.11678010213625356, -9.964505089229481527 ) ) ;
#67492 = EDGE_CURVE ( 'NONE', #20552, #18963, #67685, .T. ) ;
#67493 =( LENGTH_UNIT ( ) NAMED_UNIT ( * ) SI_UNIT ( .MILLI., .METRE. ) );
#67494 = CARTESIAN_POINT ( 'NONE',  ( -91.85499999999998977, 4.716976649647094177, 6.492361379858945902 ) ) ;
#67495 = CARTESIAN_POINT ( 'NONE',  ( 8.150468726202566572, 154.4999999999999147, 4.948482742093330167 ) ) ;
#67496 = MECHANICAL_DESIGN_GEOMETRIC_PRESENTATION_REPRESENTATION (  '', ( #5671 ), #37210 ) ;
#67497 = CYLINDRICAL_SURFACE ( 'NONE', #49475, 1.000000000000000888 ) ;
#67498 = EDGE_CURVE ( 'NONE', #25042, #8229, #24449, .T. ) ;
#67499 = CARTESIAN_POINT ( 'NONE',  ( -92.54499999999998749, -7.632228543268600340, -2.479861379858950166 ) ) ;
#67500 = EDGE_CURVE ( 'NONE', #49555, #583, #37981, .T. ) ;
#67501 = CARTESIAN_POINT ( 'NONE',  ( -5.598654528085808657, 117.7549999999999812, 7.705886871421373741 ) ) ;
#67502 = CARTESIAN_POINT ( 'NONE',  ( -71.99500000000000455, -6.826472737025115478, 4.959722759717900331 ) ) ;
#67503 =( NAMED_UNIT ( * ) SI_UNIT ( $, .STERADIAN. ) SOLID_ANGLE_UNIT ( ) );
#67504 = CARTESIAN_POINT ( 'NONE',  ( 25.00000000000001421, 42.00000000000000000, 29.68999999999999417 ) ) ;
#67505 = STYLED_ITEM ( 'NONE', ( #54438 ), #59718 ) ;
#67506 = CARTESIAN_POINT ( 'NONE',  ( 11.00000000000001776, 26.00000000000000355, -24.00000000000000355 ) ) ;
#67507 = CARTESIAN_POINT ( 'NONE',  ( 10.00000000000000711, 50.00000000000000000, -65.00000000000000000 ) ) ;
#67509 = ORIENTED_EDGE ( 'NONE', *, *, #33894, .T. ) ;
#67508 =( GEOMETRIC_REPRESENTATION_CONTEXT ( 3 ) GLOBAL_UNCERTAINTY_ASSIGNED_CONTEXT ( ( #65600 ) ) GLOBAL_UNIT_ASSIGNED_CONTEXT ( ( #69195, #69520, #54029 ) ) REPRESENTATION_CONTEXT ( 'NONE', 'WORKASPACE' ) );
#67510 = ADVANCED_FACE ( 'NONE', ( #35334 ), #45901, .T. ) ;
#67511 = CARTESIAN_POINT ( 'NONE',  ( -113.3929263765337936, 8.102448949553176405, 5.886773742842740909 ) ) ;
#67512 = PRESENTATION_LAYER_ASSIGNMENT (  '', '', ( #14701 ) ) ;
#67513 = CARTESIAN_POINT ( 'NONE',  ( -130.4950000000000045, 6.826472737025113702, -4.959722759717902107 ) ) ;
#67514 = CARTESIAN_POINT ( 'NONE',  ( -7.632228543268607446, 145.6570736234661751, -2.479861379858953718 ) ) ;
#67515 = EDGE_CURVE ( 'NONE', #57165, #64235, #39948, .T. ) ;
#67516 = PRESENTATION_LAYER_ASSIGNMENT (  '', '', ( #15879 ) ) ;
#67517 = DIRECTION ( 'NONE',  ( 0.000000000000000000, 0.000000000000000000, 1.000000000000000000 ) ) ;
#67518 = VECTOR ( 'NONE', #52067, 1000.000000000000000 ) ;
#67520 = CARTESIAN_POINT ( 'NONE',  ( 71.62068965517238439, 63.58603185604027885, 7.000000000000000000 ) ) ;
#67519 = CARTESIAN_POINT ( 'NONE',  ( -131.9929263765338021, 8.102448949553172852, -5.886773742842744461 ) ) ;
#67521 = DIRECTION ( 'NONE',  ( -1.000000000000000000, 0.000000000000000000, 0.000000000000000000 ) ) ;
#67522 = EDGE_LOOP ( 'NONE', ( #25919, #56356, #48625, #37827, #16317 ) ) ;
#67523 = ORIENTED_EDGE ( 'NONE', *, *, #1851, .T. ) ;
#67524 = AXIS2_PLACEMENT_3D ( 'NONE', #11465, #831, #22726 ) ;
#67525 = DIRECTION ( 'NONE',  ( -1.000000000000000000, -7.709882115452469292E-16, 0.000000000000000000 ) ) ;
#67526 = CIRCLE ( 'NONE', #16991, 5.000000000000000000 ) ;
#67527 = PRESENTATION_STYLE_ASSIGNMENT (( #55929 ) ) ;
#67528 = AXIS2_PLACEMENT_3D ( 'NONE', #69352, #43010, #46905 ) ;
#67529 = CARTESIAN_POINT ( 'NONE',  ( -69.74999999999998579, -3.000000000000000000, 24.00000000000000000 ) ) ;
#67530 = PRESENTATION_STYLE_ASSIGNMENT (( #18659 ) ) ;
#67531 = ORIENTED_EDGE ( 'NONE', *, *, #49250, .T. ) ;
#67532 = CARTESIAN_POINT ( 'NONE',  ( -132.9549999999999841, -7.632228543268599452, 2.479861379858951054 ) ) ;
#67533 = VERTEX_POINT ( 'NONE', #30036 ) ;
#67534 = CARTESIAN_POINT ( 'NONE',  ( -124.8570736234661780, -5.598654528085803328, -7.705886871421366635 ) ) ;
#67535 = ADVANCED_FACE ( 'NONE', ( #46263 ), #13158, .F. ) ;
#67536 = EDGE_LOOP ( 'NONE', ( #31082, #28692 ) ) ;
#67537 = CARTESIAN_POINT ( 'NONE',  ( 31.00000000000001421, 15.00000000000000000, 34.49999999999998579 ) ) ;
#67538 = DIRECTION ( 'NONE',  ( 0.000000000000000000, 0.000000000000000000, 1.000000000000000000 ) ) ;
#67539 = ORIENTED_EDGE ( 'NONE', *, *, #31527, .F. ) ;
#67540 = ADVANCED_FACE ( 'NONE', ( #9297 ), #25455, .T. ) ;
#67541 = CARTESIAN_POINT ( 'NONE',  ( -9.000000000000003553, 27.74999999999998934, 4.000000000000000000 ) ) ;
#67542 = CARTESIAN_POINT ( 'NONE',  ( -10.01517768586949231, 143.1949999999999932, -6.132527647946036459E-16 ) ) ;
#67543 = FACE_OUTER_BOUND ( 'NONE', #27187, .T. ) ;
#67544 = AXIS2_PLACEMENT_3D ( 'NONE', #34301, #23737, #35695 ) ;
#67545 = CARTESIAN_POINT ( 'NONE',  ( -141.3570736234661638, 5.598654528085804216, 7.705886871421366635 ) ) ;
#67546 = VERTEX_POINT ( 'NONE', #36032 ) ;
#67547 = CARTESIAN_POINT ( 'NONE',  ( -54.35707362346617089, 5.598654528085804216, 7.705886871421366635 ) ) ;
#67548 = CARTESIAN_POINT ( 'NONE',  ( 10.01517768586949408, 142.8049999999999500, 1.839758294383810543E-15 ) ) ;
#67549 = DIRECTION ( 'NONE',  ( 0.000000000000000000, 0.000000000000000000, -1.000000000000000000 ) ) ;
#67550 = SURFACE_STYLE_USAGE ( .BOTH. , #51372 ) ;
#67551 = ORIENTED_EDGE ( 'NONE', *, *, #42864, .F. ) ;
#67552 = CARTESIAN_POINT ( 'NONE',  ( 4.716976649647099507, 119.6429263765338078, -6.492361379858953008 ) ) ;
#67553 = DIRECTION ( 'NONE',  ( -0.000000000000000000, -0.000000000000000000, -1.000000000000000000 ) ) ;
#67554 = AXIS2_PLACEMENT_3D ( 'NONE', #56309, #12349, #29223 ) ;
#67555 = CARTESIAN_POINT ( 'NONE',  ( -99.29292637653485087, 3.094860106600546334, -9.525000000012985524 ) ) ;
#67556 = CARTESIAN_POINT ( 'NONE',  ( -71.50000000000000000, 35.92875272052971525, 7.500000000000000000 ) ) ;
#67557 = DIRECTION ( 'NONE',  ( -0.000000000000000000, -1.000000000000000000, -0.000000000000000000 ) ) ;
#67558 = ORIENTED_EDGE ( 'NONE', *, *, #26464, .T. ) ;
#67559 = CARTESIAN_POINT ( 'NONE',  ( -1.136396319700227586, -9.000000000000005329, 0.06877762208649663977 ) ) ;
#67560 = ORIENTED_EDGE ( 'NONE', *, *, #32228, .T. ) ;
#67561 = PRESENTATION_STYLE_ASSIGNMENT (( #7444 ) ) ;
#67562 = CARTESIAN_POINT ( 'NONE',  ( -120.4429263765338050, -1.166476076187852838E-15, -9.524999999999991473 ) ) ;
#67563 = CARTESIAN_POINT ( 'NONE',  ( -11.74999999999999645, -3.000000000000000000, 19.00000000000000000 ) ) ;
#67565 = CARTESIAN_POINT ( 'NONE',  ( -159.8049999999999784, -8.437984349512085203, 5.166775262442717831E-16 ) ) ;
#67564 = CIRCLE ( 'NONE', #7998, 3.100000000000003642 ) ;
#67566 = EDGE_LOOP ( 'NONE', ( #30967, #6088, #36654, #42417, #26272, #67264, #1729, #60492, #53651, #25192, #40248, #37770, #48982, #42325, #18742, #7666, #57412, #67608, #18664, #21812, #27812, #21694, #67622, #49003, #43488, #64061, #68264, #7366, #24904, #69603, #28761, #38187, #36739, #48912 ) ) ;
#67567 = DIRECTION ( 'NONE',  ( 0.000000000000000000, 1.000000000000000000, 0.000000000000000000 ) ) ;
#67568 = SHAPE_REPRESENTATION ( '15. Washer M6', ( #42840 ), #47260 ) ;
#67569 = CIRCLE ( 'NONE', #10335, 4.499999999999976019 ) ;
#67570 = AXIS2_PLACEMENT_3D ( 'NONE', #22781, #38996, #60389 ) ;
#67571 = CARTESIAN_POINT ( 'NONE',  ( 7.500000000000000000, 9.184850993605147944E-16, 0.7500000000000000000 ) ) ;
#67572 = CARTESIAN_POINT ( 'NONE',  ( -7.632228543268607446, 151.6570736234661751, -2.479861379858953718 ) ) ;
#67573 = CARTESIAN_POINT ( 'NONE',  ( 75.00000000000000000, 19.97932849626379692, 6.162720495828319045 ) ) ;
#67574 =( NAMED_UNIT ( * ) SI_UNIT ( $, .STERADIAN. ) SOLID_ANGLE_UNIT ( ) );
#67575 = VERTEX_POINT ( 'NONE', #37102 ) ;
#67576 = DIRECTION ( 'NONE',  ( 1.000000000000000000, -1.156482317317866302E-16, 0.000000000000000000 ) ) ;
#67577 = ORIENTED_EDGE ( 'NONE', *, *, #25950, .T. ) ;
#67578 = PRESENTATION_STYLE_ASSIGNMENT (( #23617 ) ) ;
#67579 = AXIS2_PLACEMENT_3D ( 'NONE', #48849, #2551, #17169 ) ;
#67580 = SURFACE_STYLE_FILL_AREA ( #9197 ) ;
#67581 = CARTESIAN_POINT ( 'NONE',  ( -71.45499999999998408, 7.632228543268599452, -2.479861379858951942 ) ) ;
#67582 = ORIENTED_EDGE ( 'NONE', *, *, #2041, .F. ) ;
#67583 = FILL_AREA_STYLE_COLOUR ( '', #34040 ) ;
#67584 = ADVANCED_FACE ( 'NONE', ( #36757 ), #58173, .F. ) ;
#67585 = SURFACE_STYLE_USAGE ( .BOTH. , #46160 ) ;
#67586 = LINE ( 'NONE', #40886, #3849 ) ;
#67587 = EDGE_CURVE ( 'NONE', #62632, #16376, #7377, .T. ) ;
#67588 = SURFACE_SIDE_STYLE ('',( #8510 ) ) ;
#67589 = DIRECTION ( 'NONE',  ( -1.000000000000000000, 0.000000000000000000, 0.000000000000000000 ) ) ;
#67590 = ORIENTED_EDGE ( 'NONE', *, *, #13920, .F. ) ;
#67591 = CARTESIAN_POINT ( 'NONE',  ( 22.31835362224387964, 26.35424528420515955, -27.48617327699382074 ) ) ;
#67592 = AXIS2_PLACEMENT_3D ( 'NONE', #13169, #51873, #34628 ) ;
#67594 = CARTESIAN_POINT ( 'NONE',  ( -37.50000000000000000, 83.99999999999998579, 6.349999999999999645 ) ) ;
#67593 = DIRECTION ( 'NONE',  ( -1.000000000000000000, 0.000000000000000000, 0.000000000000000000 ) ) ;
#67595 = EDGE_CURVE ( 'NONE', #61721, #454, #43648, .T. ) ;
#67596 = CARTESIAN_POINT ( 'NONE',  ( -9.058813317711338797, 143.3449999999999989, 2.943386871421373563 ) ) ;
#67597 = CARTESIAN_POINT ( 'NONE',  ( -92.99500000000000455, -6.826472737025115478, 4.959722759717900331 ) ) ;
#67598 = DIRECTION ( 'NONE',  ( -0.000000000000000000, -1.000000000000000000, -0.000000000000000000 ) ) ;
#67599 = LINE ( 'NONE', #14140, #69616 ) ;
#67600 = DIRECTION ( 'NONE',  ( 0.000000000000000000, -1.000000000000000000, 0.000000000000000000 ) ) ;
#67601 = CARTESIAN_POINT ( 'NONE',  ( -144.1429263765338078, 5.598654528085800663, -7.705886871421367523 ) ) ;
#67602 = LINE ( 'NONE', #55396, #16366 ) ;
#67603 = CARTESIAN_POINT ( 'NONE',  ( -156.8950000000000102, 6.826472737025116366, 4.959722759717898555 ) ) ;
#67604 = AXIS2_PLACEMENT_3D ( 'NONE', #30771, #52272, #46673 ) ;
#67605 = ADVANCED_FACE ( 'NONE', ( #57471 ), #36415, .T. ) ;
#67606 = SURFACE_STYLE_USAGE ( .BOTH. , #46185 ) ;
#67607 = DIRECTION ( 'NONE',  ( -1.000000000000000000, -0.000000000000000000, -0.000000000000000000 ) ) ;
#67608 = ORIENTED_EDGE ( 'NONE', *, *, #35017, .T. ) ;
#67609 = DIRECTION ( 'NONE',  ( 0.000000000000000000, 0.000000000000000000, -1.000000000000000000 ) ) ;
#67610 = ORIENTED_EDGE ( 'NONE', *, *, #20909, .F. ) ;
#67611 = CIRCLE ( 'NONE', #17077, 0.5000000000000004441 ) ;
#67612 = DIRECTION ( 'NONE',  ( 1.000000000000000000, 0.000000000000000000, 0.000000000000000000 ) ) ;
#67613 = VECTOR ( 'NONE', #7163, 1000.000000000000000 ) ;
#67614 = AXIS2_PLACEMENT_3D ( 'NONE', #62728, #48954, #51865 ) ;
#67615 = CARTESIAN_POINT ( 'NONE',  ( 8.437984349512095861, 119.1929263765337907, 1.550032578732816828E-15 ) ) ;
#67616 = CARTESIAN_POINT ( 'NONE',  ( -173.3070736234661808, -10.01517768586948698, 6.132527647946031529E-16 ) ) ;
#67617 = CIRCLE ( 'NONE', #46315, 0.2500000000000002220 ) ;
#67619 = AXIS2_PLACEMENT_3D ( 'NONE', #16318, #37796, #59172 ) ;
#67618 = DIRECTION ( 'NONE',  ( -1.000000000000000000, 0.000000000000000000, 0.000000000000000000 ) ) ;
#67620 = ORIENTED_EDGE ( 'NONE', *, *, #59558, .F. ) ;
#67621 = CARTESIAN_POINT ( 'NONE',  ( -163.5550000000000068, 0.000000000000000000, 8.024999999999991473 ) ) ;
#67622 = ORIENTED_EDGE ( 'NONE', *, *, #55415, .T. ) ;
#67623 = CARTESIAN_POINT ( 'NONE',  ( 14.60000000000000142, 11.99999999999999289, -4.000000000000000000 ) ) ;
#67624 = PLANE ( 'NONE',  #69134 ) ;
#67625 = COLOUR_RGB ( '', 0.09019608, 0.27058824, 0.51372549) ;
#67626 = VERTEX_POINT ( 'NONE', #69083 ) ;
#67627 = AXIS2_PLACEMENT_3D ( 'NONE', #29652, #66592, #18744 ) ;
#67628 = EDGE_CURVE ( 'NONE', #62473, #20781, #42962, .T. ) ;
#67629 = CARTESIAN_POINT ( 'NONE',  ( -57.95707362346616520, 9.058813317711329915, -2.943386871421373119 ) ) ;
#67630 = CARTESIAN_POINT ( 'NONE',  ( 0.000000000000000000, 160.0570736234661524, -8.025000000000000355 ) ) ;
#67631 = ORIENTED_EDGE ( 'NONE', *, *, #68464, .T. ) ;
#67632 = DIRECTION ( 'NONE',  ( 0.000000000000000000, 1.000000000000000000, 0.000000000000000000 ) ) ;
#67633 = CARTESIAN_POINT ( 'NONE',  ( -1.166476076187854022E-15, 112.0549999999999926, 9.525000000000000355 ) ) ;
#67634 = CARTESIAN_POINT ( 'NONE',  ( -74.15499999999998693, 7.632228543268600340, 2.479861379858949277 ) ) ;
#67635 = ORIENTED_EDGE ( 'NONE', *, *, #42396, .T. ) ;
#67636 = CARTESIAN_POINT ( 'NONE',  ( 5.598654528085805993, 139.3549999999999898, 7.705886871421374629 ) ) ;
#67637 = VECTOR ( 'NONE', #66570, 1000.000000000000000 ) ;
#67638 =( NAMED_UNIT ( * ) PLANE_ANGLE_UNIT ( ) SI_UNIT ( $, .RADIAN. ) );
#67639 = CIRCLE ( 'NONE', #56377, 0.5000000000000004441 ) ;
#67640 =( NAMED_UNIT ( * ) PLANE_ANGLE_UNIT ( ) SI_UNIT ( $, .RADIAN. ) );
#67641 = CARTESIAN_POINT ( 'NONE',  ( -40.99999999999998579, 107.7459666924148252, 3.099782425413943443 ) ) ;
#67642 =( GEOMETRIC_REPRESENTATION_CONTEXT ( 3 ) GLOBAL_UNCERTAINTY_ASSIGNED_CONTEXT ( ( #41260 ) ) GLOBAL_UNIT_ASSIGNED_CONTEXT ( ( #2355, #18617, #51655 ) ) REPRESENTATION_CONTEXT ( 'NONE', 'WORKASPACE' ) );
#67643 = SURFACE_STYLE_FILL_AREA ( #63049 ) ;
#67644 = VERTEX_POINT ( 'NONE', #37462 ) ;
#67645 = DIRECTION ( 'NONE',  ( 0.000000000000000000, 0.000000000000000000, 1.000000000000000000 ) ) ;
#67646 = PRESENTATION_STYLE_ASSIGNMENT (( #45540 ) ) ;
#67647 = CARTESIAN_POINT ( 'NONE',  ( -56.54499999999998749, -7.632228543268600340, -2.479861379858950166 ) ) ;
#67648 = EDGE_LOOP ( 'NONE', ( #33009, #42489 ) ) ;
#67649 = CARTESIAN_POINT ( 'NONE',  ( -15.75000000000000000, -4.000000000000000000, 19.00000000000000000 ) ) ;
#67650 = FACE_OUTER_BOUND ( 'NONE', #1029, .T. ) ;
#67651 = FACE_OUTER_BOUND ( 'NONE', #47105, .T. ) ;
#67652 =( NAMED_UNIT ( * ) PLANE_ANGLE_UNIT ( ) SI_UNIT ( $, .RADIAN. ) );
#67653 = ORIENTED_EDGE ( 'NONE', *, *, #53162, .F. ) ;
#67654 = CARTESIAN_POINT ( 'NONE',  ( -10.39230484541327293, 3.469446951953614189E-15, 7.500000000000000000 ) ) ;
#67655 = ORIENTED_EDGE ( 'NONE', *, *, #39851, .F. ) ;
#67656 = COLOUR_RGB ( '', 0.72549020, 0.75294118, 0.79215686) ;
#67657 = DIRECTION ( 'NONE',  ( 1.000000000000000000, 0.000000000000000000, 0.000000000000000000 ) ) ;
#67658 = CARTESIAN_POINT ( 'NONE',  ( -108.5049999999999812, -6.826472737025115478, -4.959722759717899443 ) ) ;
#67659 = ORIENTED_EDGE ( 'NONE', *, *, #51249, .T. ) ;
#67660 = LINE ( 'NONE', #24382, #8094 ) ;
#67661 = ADVANCED_FACE ( 'NONE', ( #58864 ), #53255, .T. ) ;
#67662 = CARTESIAN_POINT ( 'NONE',  ( -74.99999999999998579, 50.00000000000000000, 7.000000000000000000 ) ) ;
#67663 = CARTESIAN_POINT ( 'NONE',  ( -140.7570736234661695, -5.598654528085801552, 7.705886871421367523 ) ) ;
#67664 = CARTESIAN_POINT ( 'NONE',  ( -58.85707362346617799, -5.598654528085803328, -7.705886871421366635 ) ) ;
#67665 = CARTESIAN_POINT ( 'NONE',  ( 3.094860106618431583, 141.0949999999999989, 9.525000000000000355 ) ) ;
#67666 = CARTESIAN_POINT ( 'NONE',  ( -70.40707362346616094, 3.094860106618428031, -9.524999999999993250 ) ) ;
#67667 = VECTOR ( 'NONE', #35201, 1000.000000000000000 ) ;
#67668 = FACE_OUTER_BOUND ( 'NONE', #55527, .T. ) ;
#67670 = CARTESIAN_POINT ( 'NONE',  ( -19.96607921494393167, -11.98575909856985611, 0.6678542743433295570 ) ) ;
#67669 = PRESENTATION_LAYER_ASSIGNMENT (  '', '', ( #49701 ) ) ;
#67672 = DIRECTION ( 'NONE',  ( 0.000000000000000000, 0.000000000000000000, -1.000000000000000000 ) ) ;
#67671 = FACE_OUTER_BOUND ( 'NONE', #50436, .T. ) ;
#67673 = CARTESIAN_POINT ( 'NONE',  ( -125.3049999999999926, 8.437984349512085203, -1.550032578732815448E-15 ) ) ;
#67674 = EDGE_CURVE ( 'NONE', #30672, #27999, #48111, .T. ) ;
#67675 = CARTESIAN_POINT ( 'NONE',  ( 21.02379604162863913, 110.4999999999999858, 10.50000000000000000 ) ) ;
#67676 = CARTESIAN_POINT ( 'NONE',  ( 0.000000000000000000, 110.4999999999999858, 0.000000000000000000 ) ) ;
#67677 = COLOUR_RGB ( '', 0.31764706, 0.68627451, 0.89019608) ;
#67678 = CARTESIAN_POINT ( 'NONE',  ( -122.8449999999999847, -7.632228543268599452, 2.479861379858951054 ) ) ;
#67679 = ADVANCED_FACE ( 'NONE', ( #7122 ), #28909, .T. ) ;
#67680 = CARTESIAN_POINT ( 'NONE',  ( -121.1949999999999790, 8.437984349512086979, -1.550032578732815448E-15 ) ) ;
#67682 = EDGE_CURVE ( 'NONE', #24916, #14317, #397, .T. ) ;
#67681 = TOROIDAL_SURFACE ( 'NONE', #22737, 2.000000000000000000, 1.000000000000000000 ) ;
#67683 = VERTEX_POINT ( 'NONE', #6759 ) ;
#67684 = AXIS2_PLACEMENT_3D ( 'NONE', #68693, #52184, #2874 ) ;
#67685 = LINE ( 'NONE', #2197, #1904 ) ;
#67686 = EDGE_CURVE ( 'NONE', #14650, #34547, #43437, .T. ) ;
#67687 = DIRECTION ( 'NONE',  ( -0.000000000000000000, -1.000000000000000000, -0.000000000000000000 ) ) ;
#67688 = MECHANICAL_DESIGN_GEOMETRIC_PRESENTATION_REPRESENTATION (  '', ( #37412 ), #46374 ) ;
#67689 = CARTESIAN_POINT ( 'NONE',  ( -169.7929263765338135, -3.094860106618429807, 9.524999999999991473 ) ) ;
#67690 = CARTESIAN_POINT ( 'NONE',  ( -49.34499999999997044, 7.632228543268599452, -2.479861379858951942 ) ) ;
#67691 = EDGE_CURVE ( 'NONE', #14431, #30410, #54607, .T. ) ;
#67692 = PRESENTATION_LAYER_ASSIGNMENT (  '', '', ( #39606 ) ) ;
#67693 = LINE ( 'NONE', #30043, #57901 ) ;
#67694 = PRESENTATION_LAYER_ASSIGNMENT (  '', '', ( #31727 ) ) ;
#67695 = CARTESIAN_POINT ( 'NONE',  ( 74.50000000000000000, 19.30628705663858469, 6.999999999999999112 ) ) ;
#67696 = CARTESIAN_POINT ( 'NONE',  ( 57.49999999999999289, 27.99999999999998934, 4.000000000000000000 ) ) ;
#67697 = VERTEX_POINT ( 'NONE', #59530 ) ;
#67698 = CARTESIAN_POINT ( 'NONE',  ( -87.89292637653379359, -8.102448949553172852, -5.886773742842741797 ) ) ;
#67699 = APPLICATION_PROTOCOL_DEFINITION ( 'draft international standard', 'automotive_design', 1998, #62165 ) ;
#67700 = FILL_AREA_STYLE_COLOUR ( '', #23979 ) ;
#67701 = AXIS2_PLACEMENT_3D ( 'NONE', #24314, #34189, #44781 ) ;
#67702 = PRESENTATION_LAYER_ASSIGNMENT (  '', '', ( #55332 ) ) ;
#67703 = DIRECTION ( 'NONE',  ( 0.000000000000000000, 0.000000000000000000, 1.000000000000000000 ) ) ;
#67704 =( LENGTH_UNIT ( ) NAMED_UNIT ( * ) SI_UNIT ( .MILLI., .METRE. ) );
#67705 = COLOUR_RGB ( '', 0.72549020, 0.75294118, 0.79215686) ;
#67706 = DIRECTION ( 'NONE',  ( 1.000000000000000000, -0.000000000000000000, -0.000000000000000000 ) ) ;
#67707 = ORIENTED_EDGE ( 'NONE', *, *, #2497, .T. ) ;
#67708 = LINE ( 'NONE', #8282, #50515 ) ;
#67709 = FILL_AREA_STYLE ('',( #51188 ) ) ;
#67710 = SURFACE_SIDE_STYLE ('',( #63119 ) ) ;
#67711 = VERTEX_POINT ( 'NONE', #33174 ) ;
#67712 = CARTESIAN_POINT ( 'NONE',  ( -142.9429263765337907, 0.000000000000000000, 9.524999999999991473 ) ) ;
#67713 = AXIS2_PLACEMENT_3D ( 'NONE', #65750, #38376, #39056 ) ;
#67714 = VECTOR ( 'NONE', #53000, 1000.000000000000000 ) ;
#67715 =( LENGTH_UNIT ( ) NAMED_UNIT ( * ) SI_UNIT ( .MILLI., .METRE. ) );
#67716 = CARTESIAN_POINT ( 'NONE',  ( -6.826472737025120807, 131.1070736234661638, 4.959722759717906548 ) ) ;
#67717 = CARTESIAN_POINT ( 'NONE',  ( 26.00000000000001066, 18.74999999999997868, -3.750000000000000000 ) ) ;
#67718 = TOROIDAL_SURFACE ( 'NONE', #58724, 7.499999999999998224, 0.5000000000000000000 ) ;
#67719 = EDGE_LOOP ( 'NONE', ( #9937, #2626, #4455 ) ) ;
#67720 = CARTESIAN_POINT ( 'NONE',  ( -106.8549999999999898, 4.716976649647094177, 6.492361379858945902 ) ) ;
#67721 = CARTESIAN_POINT ( 'NONE',  ( 57.00000000000000000, 14.00000000000000000, -47.50402776293824303 ) ) ;
#67722 = ORIENTED_EDGE ( 'NONE', *, *, #66111, .T. ) ;
#67723 =( NAMED_UNIT ( * ) SI_UNIT ( $, .STERADIAN. ) SOLID_ANGLE_UNIT ( ) );
#67724 = CLOSED_SHELL ( 'NONE', ( #35026, #9582, #16339, #42236, #28172, #50445, #28816, #41486, #40130, #28357, #30819, #29193, #60270, #63194, #55339, #52202, #20002, #68392, #58615, #51459, #3627, #56794, #29389, #32716, #35773, #44065, #41333, #10900, #39144, #56131, #63614, #30940, #48652, #38257, #33605, #32276, #68723, #41232, #64025, #60292, #42141, #21789, #10891, #54120, #46264, #42623, #56833, #35309, #1334, #57995, #47003, #49121, #61247, #16648, #1783, #35828, #8906, #20646, #60433, #57326, #65354, #47693, #60819, #47057, #17813, #28829, #23900, #24173, #65777, #65246, #4948, #32251, #65992, #35779, #43534, #52940, #23274, #32163, #25118, #16951, #51001, #38234, #43363, #30359, #26600, #68785, #57848, #39347, #36751, #52566, #51621, #66751, #29449, #13999, #66674, #38962, #1868, #12527, #4768, #28085, #5388, #56460, #1741, #37215, #63755, #8013, #50279, #30399, #646, #50506, #65643, #19120, #44686, #11205, #29799, #49191, #67921, #36818, #19531, #64822, #22340, #33954, #60917, #67274, #10382, #24919, #24302, #12629, #48180, #56267, #69040, #17883, #13010, #22638, #12491, #50999, #15619, #252, #69257, #58937, #32089, #6906, #8759, #58207, #1109, #8233, #38742, #45698, #3698, #5127, #28234, #43439, #17160, #7878, #12804, #50394, #21691, #63859, #40143, #34613, #11664, #2568, #28103, #1177, #7618, #36673, #26973, #40225, #4196, #21278, #11533, #28849, #48335, #324, #11987, #2427, #4509, #48029, #60410, #61971, #14160, #508, #63109, #51228, #52385, #953, #47220, #46858, #60190, #43560, #25627, #41280, #14700, #33134, #31064, #26656, #39122, #59292, #22661, #35927, #30480, #67540, #26884, #51511, #19930, #10177, #36502, #28413, #6454, #14985, #10590, #68566, #16001, #28742, #655, #32306, #22097, #9712, #4435, #18831, #35444, #27838, #28807, #51092, #2312, #11509, #19473, #17923, #7774, #55842, #12139, #5150, #49780, #15038, #50993, #20075, #19408, #8448, #14875, #56123, #47145, #11966, #63145, #5396, #40879, #65115, #48177, #13601, #36174, #54871, #24846, #6072, #47845, #46191, #16422, #59708, #37996, #50731, #41858, #6977, #31349, #23814, #20089, #24837, #14060, #34863, #52528, #26459, #61849, #8360, #25190, #52450, #4408, #7858, #57156, #61447, #43323, #21929, #60998, #53924, #62992, #5718, #57712, #65101, #14964, #8571, #65984, #27772, #46256, #40490, #16855, #42856, #41578, #34548, #52916, #5800, #15603, #34790, #45092, #19668, #67102, #11468, #55087, #26115, #59600, #36609, #12707, #38514, #48567, #38236, #27846, #54644, #51078, #58874, #17314, #17033, #41361, #14812, #52525, #48750, #55669, #39202, #6816, #9569, #29206, #22077, #59871, #63938, #30860, #35510, #16578, #68959, #9738, #64489, #2910, #49130, #45997, #34733, #54849, #32465, #21057, #20656, #67433, #26314, #66610, #50223, #38664, #66717, #46513, #8662, #32592, #54548, #69676, #15314, #64573, #18369, #22165, #54393, #24315, #67472, #49897, #22481, #41802, #21122, #20490, #11453, #35839, #29531, #29705, #3795, #64439, #24930, #1450, #6571, #45407, #16264, #37076, #48104, #56231, #61368, #33173, #34693, #66905, #60722, #64234, #23634, #8375, #1791, #54541, #310, #43940, #61927, #47136, #48654, #53301, #46, #62492, #40798, #43032, #54315, #44762, #53599, #38897, #58308, #22837, #53616, #1993, #4754, #14526, #57826, #30729, #16335, #971, #35600, #51466, #66391, #38903, #61844, #46308, #66631, #54983, #44058, #17719, #67425, #55902, #23821, #56306, #48203, #41399, #47812, #62618, #10848, #67661, #14177, #1457, #42555, #54765, #5619, #60505, #51390, #41836, #56073, #34512, #61952, #69414, #56173, #17576, #19772, #50074, #58687, #7806, #53305, #31515, #37546, #4526, #33046, #25881, #59098, #55054, #1547, #25017, #47148, #68068, #50902, #3945, #49822, #61294, #57568, #21212, #7080, #57094, #55997, #54527, #35438, #38249, #39675, #58471, #27767, #27490, #39268, #49883, #33509, #7097, #17186, #62491, #18880, #65394, #3751, #10598, #6209, #64083, #56464, #64125, #36824, #49078, #45950, #34609, #32962, #59192, #4680, #35833, #6402, #35959, #35666, #64492, #26271, #10958, #38152, #26043, #61053, #60985, #19050, #64804, #6352, #56376, #10970, #53752, #19535, #18384, #43738, #57369, #68169, #7416, #37006, #18826, #36661, #2752, #36069, #43194, #21526, #29103, #9719, #22257, #41659, #7795, #47025, #15456, #50284, #60022, #67143, #30235, #54093, #67097, #59169, #2733, #48072, #20423, #22385, #64745, #4295, #49572, #58993, #2084, #51808, #25549, #63996, #52907, #10426 ) ) ;
#67725 = FILL_AREA_STYLE_COLOUR ( '', #61973 ) ;
#67726 =( LENGTH_UNIT ( ) NAMED_UNIT ( * ) SI_UNIT ( .MILLI., .METRE. ) );
#67727 = CARTESIAN_POINT ( 'NONE',  ( -71.30707362346616662, -10.01517768586948698, 6.132527647946031529E-16 ) ) ;
#67728 = CARTESIAN_POINT ( 'NONE',  ( -77.09499999999997044, -2.607480562269071545, -8.024999999999991473 ) ) ;
#67729 = ORIENTED_EDGE ( 'NONE', *, *, #59001, .F. ) ;
#67730 =( GEOMETRIC_REPRESENTATION_CONTEXT ( 3 ) GLOBAL_UNCERTAINTY_ASSIGNED_CONTEXT ( ( #13000 ) ) GLOBAL_UNIT_ASSIGNED_CONTEXT ( ( #34505, #6723, #54573 ) ) REPRESENTATION_CONTEXT ( 'NONE', 'WORKASPACE' ) );
#67731 = CARTESIAN_POINT ( 'NONE',  ( -71.99999999999998579, 119.9999999999997868, 7.000000000000000000 ) ) ;
#67732 = UNCERTAINTY_MEASURE_WITH_UNIT (LENGTH_MEASURE( 1.000000000000000082E-05 ), #9636, 'distance_accuracy_value', 'NONE');
#67733 = ORIENTED_EDGE ( 'NONE', *, *, #40293, .T. ) ;
#67734 = PRESENTATION_LAYER_ASSIGNMENT (  '', '', ( #30614 ) ) ;
#67735 = AXIS2_PLACEMENT_3D ( 'NONE', #63344, #35585, #8841 ) ;
#67736 = DIRECTION ( 'NONE',  ( 0.000000000000000000, 1.000000000000000000, 0.000000000000000000 ) ) ;
#67737 = SURFACE_SIDE_STYLE ('',( #9709 ) ) ;
#67738 = ORIENTED_EDGE ( 'NONE', *, *, #45487, .F. ) ;
#67739 = AXIS2_PLACEMENT_3D ( 'NONE', #4757, #9369, #9014 ) ;
#67740 = CARTESIAN_POINT ( 'NONE',  ( -13.25000000000000355, 27.99999999999998934, 3.750000000000000000 ) ) ;
#67742 = ORIENTED_EDGE ( 'NONE', *, *, #3621, .F. ) ;
#67741 = EDGE_CURVE ( 'NONE', #26455, #8636, #65513, .T. ) ;
#67743 = CARTESIAN_POINT ( 'NONE',  ( 0.000000000000000000, 15.74999999999997513, 3.750000000000000000 ) ) ;
#67744 = CARTESIAN_POINT ( 'NONE',  ( 18.25000000000000711, 0.000000000000000000, 4.000000000000000000 ) ) ;
#67745 = CARTESIAN_POINT ( 'NONE',  ( -172.4070736234661467, 3.094860106618428031, -9.524999999999993250 ) ) ;
#67746 = SURFACE_SIDE_STYLE ('',( #24807 ) ) ;
#67747 = CARTESIAN_POINT ( 'NONE',  ( -5.598654528085806881, 115.7449999999999903, -7.705886871421374629 ) ) ;
#67748 = EDGE_CURVE ( 'NONE', #3437, #18730, #39166, .T. ) ;
#67749 = CARTESIAN_POINT ( 'NONE',  ( -108.2070736234661723, 3.094860106618433360, 9.524999999999991473 ) ) ;
#67750 = CARTESIAN_POINT ( 'NONE',  ( 66.74999999999998579, 36.75000000000000000, -3.750000000000000000 ) ) ;
#67751 = DIRECTION ( 'NONE',  ( 0.000000000000000000, 0.000000000000000000, 1.000000000000000000 ) ) ;
#67752 = ORIENTED_EDGE ( 'NONE', *, *, #23832, .T. ) ;
#67753 = CARTESIAN_POINT ( 'NONE',  ( -22.50000000000000711, 36.75000000000000000, -3.750000000000000000 ) ) ;
#67754 = EDGE_CURVE ( 'NONE', #42377, #8109, #16330, .T. ) ;
#67755 = CARTESIAN_POINT ( 'NONE',  ( 31.00000000000000000, 43.00000000000000000, -79.00402776293826435 ) ) ;
#67757 = CARTESIAN_POINT ( 'NONE',  ( -60.44292637653379785, -1.166476076187852838E-15, -9.524999999999991473 ) ) ;
#67756 = DIRECTION ( 'NONE',  ( 1.000000000000000000, 0.000000000000000000, 0.000000000000000000 ) ) ;
#67758 = CARTESIAN_POINT ( 'NONE',  ( -154.1049999999999898, -6.826472737025115478, 4.959722759717900331 ) ) ;
#67759 = FILL_AREA_STYLE_COLOUR ( '', #26254 ) ;
#67760 = SURFACE_SIDE_STYLE ('',( #29415 ) ) ;
#67761 = CARTESIAN_POINT ( 'NONE',  ( -168.5949999999999989, 2.607480562269073321, 8.024999999999991473 ) ) ;
#67762 = EDGE_CURVE ( 'NONE', #18324, #56663, #7773, .T. ) ;
#67763 =( GEOMETRIC_REPRESENTATION_CONTEXT ( 3 ) GLOBAL_UNCERTAINTY_ASSIGNED_CONTEXT ( ( #5118 ) ) GLOBAL_UNIT_ASSIGNED_CONTEXT ( ( #52629, #24812, #46331 ) ) REPRESENTATION_CONTEXT ( 'NONE', 'WORKASPACE' ) );
#67764 = CARTESIAN_POINT ( 'NONE',  ( -147.1450000000000102, -4.716976649647092401, 6.492361379858946790 ) ) ;
#67765 = VERTEX_POINT ( 'NONE', #49037 ) ;
#67766 = CARTESIAN_POINT ( 'NONE',  ( -87.50000000000000000, -3.500000000000000000, 24.00000000000000000 ) ) ;
#67767 = CIRCLE ( 'NONE', #68883, 0.5000000000000004441 ) ;
#67768 = CYLINDRICAL_SURFACE ( 'NONE', #51421, 16.00000000000000711 ) ;
#67769 = EDGE_CURVE ( 'NONE', #2776, #10312, #726, .T. ) ;
#67770 = DIRECTION ( 'NONE',  ( 1.000000000000000000, 0.000000000000000000, -0.000000000000000000 ) ) ;
#67771 = UNCERTAINTY_MEASURE_WITH_UNIT (LENGTH_MEASURE( 1.000000000000000082E-05 ), #63060, 'distance_accuracy_value', 'NONE');
#67772 = CARTESIAN_POINT ( 'NONE',  ( -60.95499999999998408, -7.632228543268599452, 2.479861379858951054 ) ) ;
#67773 = CARTESIAN_POINT ( 'NONE',  ( -45.00000000000000000, 9.999999999999980460, 3.000000000000000000 ) ) ;
#67774 = CARTESIAN_POINT ( 'NONE',  ( -64.64499999999998181, 4.716976649647091513, -6.492361379858946790 ) ) ;
#67775 = CARTESIAN_POINT ( 'NONE',  ( -8.102448949553181734, 159.0049999999999670, -5.886773742842749790 ) ) ;
#67776 = DIRECTION ( 'NONE',  ( -0.000000000000000000, -0.000000000000000000, 1.000000000000000000 ) ) ;
#67777 = AXIS2_PLACEMENT_3D ( 'NONE', #29578, #19721, #46141 ) ;
#67778 = UNCERTAINTY_MEASURE_WITH_UNIT (LENGTH_MEASURE( 1.000000000000000082E-05 ), #21918, 'distance_accuracy_value', 'NONE');
#67779 = CARTESIAN_POINT ( 'NONE',  ( 30.00000000000002132, 14.00000000000001599, 34.99999999999998579 ) ) ;
#67780 = COLOUR_RGB ( '', 0.72549020, 0.75294118, 0.79215686) ;
#67781 = CARTESIAN_POINT ( 'NONE',  ( 26.25000000000001066, 19.24999999999997868, 3.750000000000000000 ) ) ;
#67782 = PRESENTATION_LAYER_ASSIGNMENT (  '', '', ( #19469 ) ) ;
#67783 = CARTESIAN_POINT ( 'NONE',  ( 32.00000000000002132, 42.00000000000000000, 79.00402776293823592 ) ) ;
#67784 = DIRECTION ( 'NONE',  ( -0.000000000000000000, -0.000000000000000000, 1.000000000000000000 ) ) ;
#67785 = VECTOR ( 'NONE', #47627, 1000.000000000000000 ) ;
#67786 = AXIS2_PLACEMENT_3D ( 'NONE', #38756, #54185, #69678 ) ;
#67787 = DIRECTION ( 'NONE',  ( -1.000000000000000000, -0.000000000000000000, -0.000000000000000000 ) ) ;
#67788 = LINE ( 'NONE', #62832, #64524 ) ;
#67789 = SURFACE_STYLE_FILL_AREA ( #9408 ) ;
#67790 = ORIENTED_EDGE ( 'NONE', *, *, #5314, .F. ) ;
#67791 = VERTEX_POINT ( 'NONE', #56702 ) ;
#67792 = SURFACE_SIDE_STYLE ('',( #56888 ) ) ;
#67793 = UNCERTAINTY_MEASURE_WITH_UNIT (LENGTH_MEASURE( 1.000000000000000082E-05 ), #31833, 'distance_accuracy_value', 'NONE');
#67794 = CARTESIAN_POINT ( 'NONE',  ( -75.50000000000000000, -6.499999999999992006, 21.00000000000000000 ) ) ;
#67795 = EDGE_CURVE ( 'NONE', #50095, #62857, #35242, .T. ) ;
#67796 = VECTOR ( 'NONE', #37613, 1000.000000000000000 ) ;
#67797 = AXIS2_PLACEMENT_3D ( 'NONE', #68480, #2400, #20277 ) ;
#67798 = DIRECTION ( 'NONE',  ( 0.000000000000000000, 0.000000000000000000, -1.000000000000000000 ) ) ;
#67799 = CARTESIAN_POINT ( 'NONE',  ( -77.15707362346617515, -9.058813317711329915, -2.943386871421370898 ) ) ;
#67800 = ORIENTED_EDGE ( 'NONE', *, *, #23132, .F. ) ;
#67801 = ORIENTED_EDGE ( 'NONE', *, *, #67045, .T. ) ;
#67802 = SURFACE_SIDE_STYLE ('',( #56895 ) ) ;
#67803 = ORIENTED_EDGE ( 'NONE', *, *, #69634, .T. ) ;
#67804 = CARTESIAN_POINT ( 'NONE',  ( 48.00000000000000000, 99.99999999999992895, -7.500000000000000000 ) ) ;
#67805 = CARTESIAN_POINT ( 'NONE',  ( -2.755190520427474699, 7.000000000000004441, 0.4949495880430779260 ) ) ;
#67806 = ORIENTED_EDGE ( 'NONE', *, *, #31129, .T. ) ;
#67807 = COLOUR_RGB ( '', 0.72549020, 0.75294118, 0.79215686) ;
#67808 = AXIS2_PLACEMENT_3D ( 'NONE', #40382, #44986, #55135 ) ;
#67809 = CARTESIAN_POINT ( 'NONE',  ( 40.49999999999998579, 107.7459666924148252, -3.000000000000000444 ) ) ;
#67810 = CARTESIAN_POINT ( 'NONE',  ( -114.5949999999999704, 2.607480562269073321, 8.024999999999991473 ) ) ;
#67811 = EDGE_LOOP ( 'NONE', ( #21800, #63511, #53113, #39441 ) ) ;
#67812 = AXIS2_PLACEMENT_3D ( 'NONE', #26108, #58147, #14903 ) ;
#67813 = CARTESIAN_POINT ( 'NONE',  ( -9.527307077157137982, 110.5000000000000568, 0.3845708726071553896 ) ) ;
#67814 = PRESENTATION_LAYER_ASSIGNMENT (  '', '', ( #28468 ) ) ;
#67815 = CARTESIAN_POINT ( 'NONE',  ( 9.250000000000003553, 27.74999999999998934, -3.750000000000000000 ) ) ;
#67816 = ORIENTED_EDGE ( 'NONE', *, *, #10653, .F. ) ;
#67817 = CARTESIAN_POINT ( 'NONE',  ( 7.632228543268608334, 143.3429263765338249, -2.479861379858951942 ) ) ;
#67818 = CARTESIAN_POINT ( 'NONE',  ( -53.18268485490532527, -10.02774732068181507, -3.508434557029057821 ) ) ;
#67819 = FILL_AREA_STYLE ('',( #61812 ) ) ;
#67820 = EDGE_CURVE ( 'NONE', #43189, #15660, #39508, .T. ) ;
#67821 =( LENGTH_UNIT ( ) NAMED_UNIT ( * ) SI_UNIT ( .MILLI., .METRE. ) );
#67822 = FACE_OUTER_BOUND ( 'NONE', #6289, .T. ) ;
#67823 = CIRCLE ( 'NONE', #31901, 9.000000000000007105 ) ;
#67824 = EDGE_CURVE ( 'NONE', #55900, #18673, #57714, .T. ) ;
#67825 = VERTEX_POINT ( 'NONE', #8170 ) ;
#67826 = ORIENTED_EDGE ( 'NONE', *, *, #56285, .F. ) ;
#67827 = CARTESIAN_POINT ( 'NONE',  ( 26.00000000000001776, -3.148064030671221758, -34.49999999999999289 ) ) ;
#67828 = FILL_AREA_STYLE_COLOUR ( '', #18896 ) ;
#67829 = DIRECTION ( 'NONE',  ( -0.000000000000000000, -0.000000000000000000, -1.000000000000000000 ) ) ;
#67830 = DIRECTION ( 'NONE',  ( -0.000000000000000000, -0.000000000000000000, -1.000000000000000000 ) ) ;
#67831 = CARTESIAN_POINT ( 'NONE',  ( -121.7049999999999841, 2.607480562269073321, 8.024999999999991473 ) ) ;
#67832 = CIRCLE ( 'NONE', #22899, 3.000000000000000444 ) ;
#67833 = CARTESIAN_POINT ( 'NONE',  ( -184.0000000000000000, -7.358988424933670558, 3.200923985616050071 ) ) ;
#67834 = DIRECTION ( 'NONE',  ( -3.469446951953617344E-15, -0.000000000000000000, 1.000000000000000000 ) ) ;
#67835 = SURFACE_SIDE_STYLE ('',( #46410 ) ) ;
#67836 = VECTOR ( 'NONE', #19620, 1000.000000000000000 ) ;
#67837 = EDGE_CURVE ( 'NONE', #32655, #57077, #26709, .T. ) ;
#67838 = DIRECTION ( 'NONE',  ( 0.000000000000000000, -1.000000000000000000, 0.000000000000000000 ) ) ;
#67839 = DIRECTION ( 'NONE',  ( -0.000000000000000000, 0.000000000000000000, -1.000000000000000000 ) ) ;
#67840 =( NAMED_UNIT ( * ) SI_UNIT ( $, .STERADIAN. ) SOLID_ANGLE_UNIT ( ) );
#67841 = VERTEX_POINT ( 'NONE', #66917 ) ;
#67842 = ORIENTED_EDGE ( 'NONE', *, *, #48594, .F. ) ;
#67843 = CARTESIAN_POINT ( 'NONE',  ( 15.48999599679679662, 118.4999999999999716, 9.500000000000000000 ) ) ;
#67844 = AXIS2_PLACEMENT_3D ( 'NONE', #26356, #608, #69617 ) ;
#67845 = CIRCLE ( 'NONE', #55477, 26.99999999999999645 ) ;
#67846 = FILL_AREA_STYLE_COLOUR ( '', #6226 ) ;
#67847 = ORIENTED_EDGE ( 'NONE', *, *, #1504, .T. ) ;
#67848 = DIRECTION ( 'NONE',  ( 0.000000000000000000, 0.000000000000000000, 1.000000000000000000 ) ) ;
#67849 = CARTESIAN_POINT ( 'NONE',  ( -182.7549999999999955, 4.716976649647091513, -6.492361379858946790 ) ) ;
#67850 = DIRECTION ( 'NONE',  ( -3.469446951953611033E-15, 0.000000000000000000, -1.000000000000000000 ) ) ;
#67851 = DIRECTION ( 'NONE',  ( -0.000000000000000000, -1.000000000000000000, -0.000000000000000000 ) ) ;
#67852 = CARTESIAN_POINT ( 'NONE',  ( -56.00707362346614815, -8.102448949553172852, -5.886773742842741797 ) ) ;
#67853 = EDGE_CURVE ( 'NONE', #60166, #24214, #35728, .T. ) ;
#67854 = CIRCLE ( 'NONE', #68966, 5.000000000000004441 ) ;
#67855 = CARTESIAN_POINT ( 'NONE',  ( -181.0449999999999875, 7.632228543268600340, 2.479861379858949277 ) ) ;
#67856 = SURFACE_STYLE_USAGE ( .BOTH. , #24915 ) ;
#67857 = ORIENTED_EDGE ( 'NONE', *, *, #43660, .F. ) ;
#67858 = PRESENTATION_LAYER_ASSIGNMENT (  '', '', ( #43193 ) ) ;
#67859 = FACE_OUTER_BOUND ( 'NONE', #4816, .T. ) ;
#67860 = FACE_OUTER_BOUND ( 'NONE', #55807, .T. ) ;
#67861 = EDGE_CURVE ( 'NONE', #2313, #69517, #40190, .T. ) ;
#67862 = SURFACE_STYLE_USAGE ( .BOTH. , #46436 ) ;
#67863 = CARTESIAN_POINT ( 'NONE',  ( -92.30499999999999261, 8.437984349512085203, -1.550032578732815448E-15 ) ) ;
#67864 = DIRECTION ( 'NONE',  ( 0.000000000000000000, 0.000000000000000000, -1.000000000000000000 ) ) ;
#67865 = DIRECTION ( 'NONE',  ( 0.000000000000000000, 0.000000000000000000, 1.000000000000000000 ) ) ;
#67866 = CARTESIAN_POINT ( 'NONE',  ( -37.50000000000000000, 58.31681314173471975, -6.349999999999996092 ) ) ;
#67867 = CARTESIAN_POINT ( 'NONE',  ( -87.59499999999999886, 2.607480562269072433, 8.024999999999991473 ) ) ;
#67868 = CARTESIAN_POINT ( 'NONE',  ( -10.01517768586949231, 129.3050000000000068, -6.132527647946036459E-16 ) ) ;
#67869 = CARTESIAN_POINT ( 'NONE',  ( -72.14499999999998181, -4.716976649647092401, 6.492361379858946790 ) ) ;
#67870 = CARTESIAN_POINT ( 'NONE',  ( -195.0000000000000000, 1.166476076187852838E-15, -9.524999999999991473 ) ) ;
#67871 =( GEOMETRIC_REPRESENTATION_CONTEXT ( 3 ) GLOBAL_UNCERTAINTY_ASSIGNED_CONTEXT ( ( #65690 ) ) GLOBAL_UNIT_ASSIGNED_CONTEXT ( ( #7244, #29008, #23402 ) ) REPRESENTATION_CONTEXT ( 'NONE', 'WORKASPACE' ) );
#67872 = DIRECTION ( 'NONE',  ( -0.000000000000000000, -0.000000000000000000, -1.000000000000000000 ) ) ;
#67873 =( NAMED_UNIT ( * ) SI_UNIT ( $, .STERADIAN. ) SOLID_ANGLE_UNIT ( ) );
#67874 = UNCERTAINTY_MEASURE_WITH_UNIT (LENGTH_MEASURE( 1.000000000000000082E-05 ), #53082, 'distance_accuracy_value', 'NONE');
#67875 = DIRECTION ( 'NONE',  ( 1.000000000000000000, 0.000000000000000000, 0.000000000000000000 ) ) ;
#67876 = DIRECTION ( 'NONE',  ( 0.000000000000000000, 1.000000000000000000, 0.000000000000000000 ) ) ;
#67877 = VERTEX_POINT ( 'NONE', #29611 ) ;
#67878 = CARTESIAN_POINT ( 'NONE',  ( -116.8429263765338106, 9.058813317711329915, -2.943386871421373119 ) ) ;
#67879 = CARTESIAN_POINT ( 'NONE',  ( -130.6449999999999818, 4.716976649647091513, -6.492361379858946790 ) ) ;
#67880 = CARTESIAN_POINT ( 'NONE',  ( -2.607480562268989832, 145.2070736234661581, -8.025000000000060751 ) ) ;
#67881 = MECHANICAL_DESIGN_GEOMETRIC_PRESENTATION_REPRESENTATION (  '', ( #19557 ), #25186 ) ;
#67882 = DIRECTION ( 'NONE',  ( -0.000000000000000000, -0.000000000000000000, -1.000000000000000000 ) ) ;
#67884 = CARTESIAN_POINT ( 'NONE',  ( -195.0000000000000000, 0.000000000000000000, 0.000000000000000000 ) ) ;
#67883 = CARTESIAN_POINT ( 'NONE',  ( 4.716976649647096842, 134.8570736234661638, 6.492361379858953896 ) ) ;
#67885 = ORIENTED_EDGE ( 'NONE', *, *, #54494, .T. ) ;
#67886 = ORIENTED_EDGE ( 'NONE', *, *, #68560, .T. ) ;
#67887 =( BOUNDED_CURVE ( )  B_SPLINE_CURVE ( 3, ( #19528, #8991, #45625, #13552 ),
 .UNSPECIFIED., .F., .F. ) 
 B_SPLINE_CURVE_WITH_KNOTS ( ( 4, 4 ),
 ( 3.931838538365183489, 4.712388980384689674 ),
 .UNSPECIFIED. ) 
 CURVE ( )  GEOMETRIC_REPRESENTATION_ITEM ( )  RATIONAL_B_SPLINE_CURVE ( ( 1.000000000000000000, 0.9498695926598449413, 0.9498695926598449413, 1.000000000000000000 ) ) 
 REPRESENTATION_ITEM ( '' )  );
#67888 = CARTESIAN_POINT ( 'NONE',  ( 107.0858988931383493, 5.000000000000000000, 16.89933289725615850 ) ) ;
#67889 = ADVANCED_FACE ( 'NONE', ( #23297 ), #50383, .T. ) ;
#67890 = COLOUR_RGB ( '', 0.31764706, 0.68627451, 0.89019608) ;
#67891 = CARTESIAN_POINT ( 'NONE',  ( 8.250000000000001776, 31.24999999999998579, 4.000000000000000000 ) ) ;
#67892 = CARTESIAN_POINT ( 'NONE',  ( -43.99999999999998579, 0.000000000000000000, 0.000000000000000000 ) ) ;
#67893 = FACE_OUTER_BOUND ( 'NONE', #27381, .T. ) ;
#67894 = DIRECTION ( 'NONE',  ( -1.000000000000000000, -5.782411586589351722E-16, 0.000000000000000000 ) ) ;
#67895 = VERTEX_POINT ( 'NONE', #23635 ) ;
#67896 = CARTESIAN_POINT ( 'NONE',  ( -132.0549999999999784, -9.827790563157499189E-16, -8.024999999999991473 ) ) ;
#67897 = ORIENTED_EDGE ( 'NONE', *, *, #57909, .F. ) ;
#67898 = PRESENTATION_LAYER_ASSIGNMENT (  '', '', ( #46603 ) ) ;
#67899 = CARTESIAN_POINT ( 'NONE',  ( -122.0070736234661553, -8.102448949553172852, -5.886773742842741797 ) ) ;
#67900 = ORIENTED_EDGE ( 'NONE', *, *, #48728, .T. ) ;
#67901 = CARTESIAN_POINT ( 'NONE',  ( -13.75000000000000533, 30.74999999999999289, -3.750000000000000000 ) ) ;
#67902 = DIRECTION ( 'NONE',  ( -1.000000000000000000, 0.000000000000000000, 0.000000000000000000 ) ) ;
#67903 = ORIENTED_EDGE ( 'NONE', *, *, #29743, .T. ) ;
#67904 = PLANE ( 'NONE',  #52331 ) ;
#67905 = CARTESIAN_POINT ( 'NONE',  ( 9.058813317711337021, 138.5449999999999875, 2.943386871421375783 ) ) ;
#67906 = PRODUCT_DEFINITION ( 'UNKNOWN', '', #11305, #55039 ) ;
#67907 = ORIENTED_EDGE ( 'NONE', *, *, #2893, .F. ) ;
#67908 = AXIS2_PLACEMENT_3D ( 'NONE', #21442, #27396, #15855 ) ;
#67909 = EDGE_CURVE ( 'NONE', #56593, #55122, #66558, .T. ) ;
#67910 = CARTESIAN_POINT ( 'NONE',  ( 1.000000000000000000, 42.00000000000000000, 0.000000000000000000 ) ) ;
#67911 = CARTESIAN_POINT ( 'NONE',  ( -9.058813317711338797, 150.4550000000000125, 2.943386871421373563 ) ) ;
#67912 = CARTESIAN_POINT ( 'NONE',  ( -48.95499999999996987, -7.632228543268599452, 2.479861379858951054 ) ) ;
#67913 = FILL_AREA_STYLE_COLOUR ( '', #19517 ) ;
#67914 = EDGE_CURVE ( 'NONE', #40754, #49089, #38023, .T. ) ;
#67915 = ORIENTED_EDGE ( 'NONE', *, *, #47065, .T. ) ;
#67916 = CARTESIAN_POINT ( 'NONE',  ( -4.716976649647098618, 112.1429263765338220, 6.492361379858953008 ) ) ;
#67917 = CARTESIAN_POINT ( 'NONE',  ( -52.00000000000000000, -1.926070501056209087E-14, 12.00000000000000000 ) ) ;
#67918 = UNCERTAINTY_MEASURE_WITH_UNIT (LENGTH_MEASURE( 1.000000000000000082E-05 ), #11817, 'distance_accuracy_value', 'NONE');
#67919 = LINE ( 'NONE', #19709, #9379 ) ;
#67920 =( NAMED_UNIT ( * ) PLANE_ANGLE_UNIT ( ) SI_UNIT ( $, .RADIAN. ) );
#67921 = ADVANCED_FACE ( 'NONE', ( #19034, #13080 ), #21822, .T. ) ;
#67922 = DIRECTION ( 'NONE',  ( -5.782411586589351722E-16, 1.000000000000000000, 0.000000000000000000 ) ) ;
#67923 = EDGE_CURVE ( 'NONE', #49856, #31350, #10578, .T. ) ;
#67924 = EDGE_LOOP ( 'NONE', ( #67482, #52693, #28476, #4160 ) ) ;
#67925 = CARTESIAN_POINT ( 'NONE',  ( -6.767634268437469736, 2.278113600022081631, 0.1324414877861203599 ) ) ;
#67926 = ORIENTED_EDGE ( 'NONE', *, *, #48160, .F. ) ;
#67927 = CARTESIAN_POINT ( 'NONE',  ( -63.14292637653380780, 5.598654528085800663, -7.705886871421367523 ) ) ;
#67928 = MECHANICAL_DESIGN_GEOMETRIC_PRESENTATION_REPRESENTATION (  '', ( #55551 ), #36518 ) ;
#67929 = AXIS2_PLACEMENT_3D ( 'NONE', #24783, #2944, #29734 ) ;
#67930 = PRESENTATION_STYLE_ASSIGNMENT (( #46861 ) ) ;
#67931 = LINE ( 'NONE', #13054, #26139 ) ;
#67932 = CARTESIAN_POINT ( 'NONE',  ( -152.1549999999999727, 7.632228543268600340, 2.479861379858949277 ) ) ;
#67933 = ORIENTED_EDGE ( 'NONE', *, *, #17591, .F. ) ;
#67934 = UNCERTAINTY_MEASURE_WITH_UNIT (LENGTH_MEASURE( 1.000000000000000082E-05 ), #1570, 'distance_accuracy_value', 'NONE');
#67935 = EDGE_CURVE ( 'NONE', #16524, #57704, #54506, .T. ) ;
#67936 = DIRECTION ( 'NONE',  ( 0.000000000000000000, 0.000000000000000000, 1.000000000000000000 ) ) ;
#67937 = CARTESIAN_POINT ( 'NONE',  ( -6.826472737025120807, 151.5070736234661979, -4.959722759717907437 ) ) ;
#67938 = CARTESIAN_POINT ( 'NONE',  ( 75.00000000000000000, 19.38064346792905823, 6.520279032830130994 ) ) ;
#67939 = DIRECTION ( 'NONE',  ( 1.000000000000000000, -0.000000000000000000, 0.000000000000000000 ) ) ;
#67940 = ORIENTED_EDGE ( 'NONE', *, *, #25557, .T. ) ;
#67941 = PRESENTATION_STYLE_ASSIGNMENT (( #40877 ) ) ;
#67942 = VECTOR ( 'NONE', #33989, 1000.000000000000000 ) ;
#67944 = EDGE_CURVE ( 'NONE', #61162, #65527, #24544, .T. ) ;
#67943 = VERTEX_POINT ( 'NONE', #54158 ) ;
#67945 = DIRECTION ( 'NONE',  ( -1.000000000000000000, 0.000000000000000000, 0.000000000000000000 ) ) ;
#67946 = FACE_OUTER_BOUND ( 'NONE', #65170, .T. ) ;
#67947 = CARTESIAN_POINT ( 'NONE',  ( -67.85499999999998977, 4.716976649647094177, 6.492361379858945902 ) ) ;
#67949 = ORIENTED_EDGE ( 'NONE', *, *, #41571, .T. ) ;
#67948 = AXIS2_PLACEMENT_3D ( 'NONE', #48366, #423, #21589 ) ;
#67950 = FACE_OUTER_BOUND ( 'NONE', #40598, .T. ) ;
#67951 = VECTOR ( 'NONE', #65086, 1000.000000000000000 ) ;
#67952 = CARTESIAN_POINT ( 'NONE',  ( 98.00000000000000000, 16.00000000000000000, -12.50000000000000178 ) ) ;
#67953 = CIRCLE ( 'NONE', #17393, 5.000000000000004441 ) ;
#67954 = ORIENTED_EDGE ( 'NONE', *, *, #37200, .F. ) ;
#67955 = CARTESIAN_POINT ( 'NONE',  ( -75.00000000000000000, 9.708372675170618749, -6.000000000000000000 ) ) ;
#67956 = AXIS2_PLACEMENT_3D ( 'NONE', #39003, #60735, #7629 ) ;
#67957 = DIRECTION ( 'NONE',  ( 1.000000000000000000, 0.000000000000000000, 0.000000000000000000 ) ) ;
#67958 = DIRECTION ( 'NONE',  ( -0.000000000000000000, -0.000000000000000000, -1.000000000000000000 ) ) ;
#67959 = CARTESIAN_POINT ( 'NONE',  ( -8.102448949553181734, 151.8950000000000102, -5.886773742842749790 ) ) ;
#67960 = CARTESIAN_POINT ( 'NONE',  ( -95.24499999999997613, -4.716976649647093289, -6.492361379858945902 ) ) ;
#67961 = CARTESIAN_POINT ( 'NONE',  ( 73.01088739851485343, 0.000000000000000000, 65.71817553072288831 ) ) ;
#67962 = LINE ( 'NONE', #35943, #31441 ) ;
#67963 = EDGE_CURVE ( 'NONE', #20480, #28179, #42543, .T. ) ;
#67964 = UNCERTAINTY_MEASURE_WITH_UNIT (LENGTH_MEASURE( 1.000000000000000082E-05 ), #50689, 'distance_accuracy_value', 'NONE');
#67965 = MECHANICAL_DESIGN_GEOMETRIC_PRESENTATION_REPRESENTATION (  '', ( #23011 ), #58957 ) ;
#67966 = CARTESIAN_POINT ( 'NONE',  ( -7.632228543268607446, 144.5429263765338135, -2.479861379858953718 ) ) ;
#67967 = AXIS2_PLACEMENT_3D ( 'NONE', #43904, #1227, #39305 ) ;
#67968 = EDGE_LOOP ( 'NONE', ( #24358, #37517, #27789, #68193 ) ) ;
#67969 = CARTESIAN_POINT ( 'NONE',  ( -147.8929263765338362, -8.102448949553172852, -5.886773742842741797 ) ) ;
#67970 = LINE ( 'NONE', #28649, #33207 ) ;
#67971 = CARTESIAN_POINT ( 'NONE',  ( -161.3950000000000102, -6.826472737025115478, -4.959722759717899443 ) ) ;
#67972 = AXIS2_PLACEMENT_3D ( 'NONE', #30620, #25359, #68282 ) ;
#67973 = CARTESIAN_POINT ( 'NONE',  ( 41.49999999999998579, 99.99999999999998579, 3.000000000000000000 ) ) ;
#67974 = DIRECTION ( 'NONE',  ( 1.000000000000000000, 0.000000000000000000, 0.000000000000000000 ) ) ;
#67975 = MECHANICAL_DESIGN_GEOMETRIC_PRESENTATION_REPRESENTATION (  '', ( #54484 ), #52266 ) ;
#67976 =( NAMED_UNIT ( * ) SI_UNIT ( $, .STERADIAN. ) SOLID_ANGLE_UNIT ( ) );
#67977 = VERTEX_POINT ( 'NONE', #43335 ) ;
#67978 = CARTESIAN_POINT ( 'NONE',  ( -7.632228543268607446, 129.5429263765338135, -2.479861379858953718 ) ) ;
#67979 = ORIENTED_EDGE ( 'NONE', *, *, #67492, .F. ) ;
#67980 = MECHANICAL_DESIGN_GEOMETRIC_PRESENTATION_REPRESENTATION (  '', ( #23028 ), #25273 ) ;
#67981 = CARTESIAN_POINT ( 'NONE',  ( -6.422934014168760974, 111.9999999999999858, 4.811085495980506721 ) ) ;
#67982 = CARTESIAN_POINT ( 'NONE',  ( 31.00000000000002132, 42.00000000000000000, 79.00402776293823592 ) ) ;
#67983 = VECTOR ( 'NONE', #61739, 1000.000000000000000 ) ;
#67984 = CARTESIAN_POINT ( 'NONE',  ( -60.07898600000864775, -8.499999999999992895, 0.9999999981295574214 ) ) ;
#67985 = ORIENTED_EDGE ( 'NONE', *, *, #24679, .T. ) ;
#67986 = CARTESIAN_POINT ( 'NONE',  ( -159.8049999999999784, -8.437984349512086979, 5.166775262442717831E-16 ) ) ;
#67987 = COLOUR_RGB ( '', 0.09019608, 0.27058824, 0.51372549) ;
#67988 = EDGE_LOOP ( 'NONE', ( #56220, #36345, #27214, #54804 ) ) ;
#67989 = CARTESIAN_POINT ( 'NONE',  ( -48.14292637653380780, 5.598654528085800663, -7.705886871421367523 ) ) ;
#67990 = CARTESIAN_POINT ( 'NONE',  ( 32.00000000000001421, 42.00000000000000711, 44.99999999999998579 ) ) ;
#67991 = ORIENTED_EDGE ( 'NONE', *, *, #14205, .T. ) ;
#67992 = SURFACE_SIDE_STYLE ('',( #3929 ) ) ;
#67993 = CARTESIAN_POINT ( 'NONE',  ( -7.632228543268607446, 157.6570736234661467, -2.479861379858953718 ) ) ;
#67994 = COLOUR_RGB ( '', 0.08235294, 0.09019608, 0.10196078) ;
#67995 =( BOUNDED_CURVE ( )  B_SPLINE_CURVE ( 2, ( #25384, #25716, #52837, #20457, #46899, #4613, #25041, #57400, #20090, #9224, #52498 ),
 .UNSPECIFIED., .F., .F. ) 
 B_SPLINE_CURVE_WITH_KNOTS ( ( 3, 2, 2, 2, 2, 3 ),
 ( 0.3695652173912954974, 0.3717391304347737457, 0.3739130434782519385, 0.3760869565217300758, 0.3782608695652082687, 0.3804347826086865170 ),
 .UNSPECIFIED. ) 
 CURVE ( )  GEOMETRIC_REPRESENTATION_ITEM ( )  RATIONAL_B_SPLINE_CURVE ( ( 1.000000000000198730, 0.9510565162949548013, 1.000000000000000000, 0.9510565162951535312, 1.000000000000000000, 0.9510565162951535312, 1.000000000000000000, 0.9510565162951535312, 1.000000000000000000, 0.9510565162953596996, 0.9999999999997938316 ) ) 
 REPRESENTATION_ITEM ( '' )  );
#67996 = ORIENTED_EDGE ( 'NONE', *, *, #12053, .F. ) ;
#67997 = ADVANCED_FACE ( 'NONE', ( #69651 ), #53809, .F. ) ;
#67998 = CARTESIAN_POINT ( 'NONE',  ( 179.4361977533490347, 14.00000000000000000, 103.7004518695263044 ) ) ;
#67999 = CARTESIAN_POINT ( 'NONE',  ( 3.094860106618431583, 115.2049999999999841, 9.525000000000000355 ) ) ;
#68000 = CARTESIAN_POINT ( 'NONE',  ( -78.20499999999996987, -2.607480562269071545, -8.024999999999991473 ) ) ;
#68001 = AXIS2_PLACEMENT_3D ( 'NONE', #50901, #60396, #2995 ) ;
#68002 = VERTEX_POINT ( 'NONE', #22510 ) ;
#68003 = CARTESIAN_POINT ( 'NONE',  ( -8.102448949553181734, 135.6049999999999613, 5.886773742842747126 ) ) ;
#68004 = UNCERTAINTY_MEASURE_WITH_UNIT (LENGTH_MEASURE( 1.000000000000000082E-05 ), #20803, 'distance_accuracy_value', 'NONE');
#68005 = DIRECTION ( 'NONE',  ( -1.000000000000000000, -0.000000000000000000, -0.000000000000000000 ) ) ;
#68006 = EDGE_CURVE ( 'NONE', #61112, #51828, #5271, .T. ) ;
#68007 =( LENGTH_UNIT ( ) NAMED_UNIT ( * ) SI_UNIT ( .MILLI., .METRE. ) );
#68008 =( LENGTH_UNIT ( ) NAMED_UNIT ( * ) SI_UNIT ( .MILLI., .METRE. ) );
#68009 = DIRECTION ( 'NONE',  ( 0.000000000000000000, 0.000000000000000000, 1.000000000000000000 ) ) ;
#68010 = ORIENTED_EDGE ( 'NONE', *, *, #55610, .F. ) ;
#68011 = DIRECTION ( 'NONE',  ( 0.000000000000000000, 0.000000000000000000, 1.000000000000000000 ) ) ;
#68012 = CARTESIAN_POINT ( 'NONE',  ( -181.2549999999999955, -4.716976649647092401, 6.492361379858946790 ) ) ;
#68013 = VERTEX_POINT ( 'NONE', #22160 ) ;
#68014 = CARTESIAN_POINT ( 'NONE',  ( 31.91038508792758677, 42.48853761352473413, 45.29557347147077451 ) ) ;
#68015 = STYLED_ITEM ( 'NONE', ( #63594 ), #8360 ) ;
#68016 = SURFACE_STYLE_USAGE ( .BOTH. , #57086 ) ;
#68017 = EDGE_LOOP ( 'NONE', ( #27571, #4573, #39027, #6815 ) ) ;
#68018 =( NAMED_UNIT ( * ) SI_UNIT ( $, .STERADIAN. ) SOLID_ANGLE_UNIT ( ) );
#68019 = ORIENTED_EDGE ( 'NONE', *, *, #10725, .T. ) ;
#68020 = EDGE_CURVE ( 'NONE', #30008, #20328, #4941, .T. ) ;
#68021 = DIRECTION ( 'NONE',  ( -0.000000000000000000, -0.000000000000000000, -1.000000000000000000 ) ) ;
#68022 = MECHANICAL_DESIGN_GEOMETRIC_PRESENTATION_REPRESENTATION (  '', ( #51143 ), #20814 ) ;
#68023 = CARTESIAN_POINT ( 'NONE',  ( 65.49999999999997158, 1.797044900979284448E-15, 12.00000000000000000 ) ) ;
#68024 = CARTESIAN_POINT ( 'NONE',  ( -106.4049999999999727, -2.607480562269069768, 8.024999999999991473 ) ) ;
#68025 = VERTEX_POINT ( 'NONE', #43659 ) ;
#68026 = DIRECTION ( 'NONE',  ( 0.000000000000000000, 0.000000000000000000, 1.000000000000000000 ) ) ;
#68027 = FACE_OUTER_BOUND ( 'NONE', #46138, .T. ) ;
#68028 = AXIS2_PLACEMENT_3D ( 'NONE', #60004, #38607, #27271 ) ;
#68029 = CARTESIAN_POINT ( 'NONE',  ( -138.8070736234661524, 10.01517768586948698, -1.839758294383808571E-15 ) ) ;
#68030 = VECTOR ( 'NONE', #3055, 1000.000000000000000 ) ;
#68031 =( NAMED_UNIT ( * ) PLANE_ANGLE_UNIT ( ) SI_UNIT ( $, .RADIAN. ) );
#68032 = CARTESIAN_POINT ( 'NONE',  ( 5.598654528085805993, 147.2449999999999761, 7.705886871421374629 ) ) ;
#68033 = CARTESIAN_POINT ( 'NONE',  ( -73.85707362346617799, -5.598654528085803328, -7.705886871421366635 ) ) ;
#68034 = CARTESIAN_POINT ( 'NONE',  ( -87.50000000000000000, -8.499999999999989342, 24.00000000000000000 ) ) ;
#68035 = ORIENTED_EDGE ( 'NONE', *, *, #5783, .T. ) ;
#68036 = CARTESIAN_POINT ( 'NONE',  ( -74.49999999999998579, 64.49137674618943095, -9.500000000000000000 ) ) ;
#68037 = CARTESIAN_POINT ( 'NONE',  ( -24.00000000000000355, 37.00000000000000000, 3.750000000000000000 ) ) ;
#68038 = CARTESIAN_POINT ( 'NONE',  ( 1.709458476932651091E-14, 43.00000000000000000, -35.50000000000000000 ) ) ;
#68039 = COLOUR_RGB ( '', 0.31764706, 0.68627451, 0.89019608) ;
#68040 = CARTESIAN_POINT ( 'NONE',  ( -123.8049999999999926, -8.437984349512085203, 5.166775262442717831E-16 ) ) ;
#68041 = EDGE_CURVE ( 'NONE', #7407, #65484, #5609, .T. ) ;
#68042 = CARTESIAN_POINT ( 'NONE',  ( 9.058813317711337021, 111.5449999999999875, 2.943386871421375783 ) ) ;
#68043 = CARTESIAN_POINT ( 'NONE',  ( -126.8949999999999818, 6.826472737025116366, 4.959722759717898555 ) ) ;
#68044 = STYLED_ITEM ( 'NONE', ( #1754 ), #57995 ) ;
#68045 = CARTESIAN_POINT ( 'NONE',  ( -111.3570736234661780, 5.598654528085804216, 7.705886871421366635 ) ) ;
#68046 = EDGE_CURVE ( 'NONE', #28073, #65666, #61599, .T. ) ;
#68047 = ORIENTED_EDGE ( 'NONE', *, *, #7553, .F. ) ;
#68048 = AXIS2_PLACEMENT_3D ( 'NONE', #21508, #59472, #54208 ) ;
#68049 = FILL_AREA_STYLE ('',( #51863 ) ) ;
#68050 = CARTESIAN_POINT ( 'NONE',  ( -166.5570736234661808, -1.166476076187852838E-15, -9.524999999999991473 ) ) ;
#68051 = VECTOR ( 'NONE', #67006, 1000.000000000000000 ) ;
#68052 = CARTESIAN_POINT ( 'NONE',  ( -175.1929263765337623, -10.01517768586948698, 6.132527647946031529E-16 ) ) ;
#68053 = PRESENTATION_STYLE_ASSIGNMENT (( #46972 ) ) ;
#68054 = CARTESIAN_POINT ( 'NONE',  ( -2.607480562269073321, 124.2070736234661581, -8.025000000000000355 ) ) ;
#68055 = CARTESIAN_POINT ( 'NONE',  ( -54.47897255799113481, -9.244539326313761407, -2.264342823408200367 ) ) ;
#68056 = LINE ( 'NONE', #3625, #65319 ) ;
#68057 = EDGE_LOOP ( 'NONE', ( #68189, #2309, #6110, #57809 ) ) ;
#68058 = CARTESIAN_POINT ( 'NONE',  ( -82.34292637653379643, -9.058813317711329915, 2.943386871421371787 ) ) ;
#68059 = ITEM_DEFINED_TRANSFORMATION ( 'NONE', 'NONE', #60693,  #42840 ) ;
#68060 = DIRECTION ( 'NONE',  ( -1.000000000000000000, 0.000000000000000000, 0.000000000000000000 ) ) ;
#68061 = AXIS2_PLACEMENT_3D ( 'NONE', #46703, #52970, #19896 ) ;
#68062 = CARTESIAN_POINT ( 'NONE',  ( -180.2929263765338987, 3.094860106617521200, -9.525000000000654055 ) ) ;
#68063 = DIRECTION ( 'NONE',  ( 1.000000000000000000, -0.000000000000000000, -0.000000000000000000 ) ) ;
#68064 = FILL_AREA_STYLE_COLOUR ( '', #48283 ) ;
#68065 = AXIS2_PLACEMENT_3D ( 'NONE', #57395, #47232, #4963 ) ;
#68066 = ORIENTED_EDGE ( 'NONE', *, *, #1699, .F. ) ;
#68067 = CARTESIAN_POINT ( 'NONE',  ( -136.4929263765338305, -8.102448949553174629, 5.886773742842742685 ) ) ;
#68068 = ADVANCED_FACE ( 'NONE', ( #38389 ), #59791, .T. ) ;
#68069 = PRESENTATION_STYLE_ASSIGNMENT (( #14587 ) ) ;
#68071 = ORIENTED_EDGE ( 'NONE', *, *, #22570, .T. ) ;
#68070 = PRESENTATION_LAYER_ASSIGNMENT (  '', '', ( #29830 ) ) ;
#68072 = CARTESIAN_POINT ( 'NONE',  ( 0.000000000000000000, 2.299999999999999822, 0.000000000000000000 ) ) ;
#68073 = STYLED_ITEM ( 'NONE', ( #65715 ), #5718 ) ;
#68074 = SURFACE_SIDE_STYLE ('',( #25142 ) ) ;
#68075 = CARTESIAN_POINT ( 'NONE',  ( 4.716976649647099507, 132.7570736234661695, -6.492361379858953008 ) ) ;
#68076 = DIRECTION ( 'NONE',  ( -1.000000000000000000, 0.000000000000000000, 0.000000000000000000 ) ) ;
#68077 = VERTEX_POINT ( 'NONE', #34440 ) ;
#68078 =( LENGTH_UNIT ( ) NAMED_UNIT ( * ) SI_UNIT ( .MILLI., .METRE. ) );
#68079 = CARTESIAN_POINT ( 'NONE',  ( -103.5549999999999926, 0.000000000000000000, 8.024999999999991473 ) ) ;
#68080 = DIRECTION ( 'NONE',  ( -1.000000000000000000, 0.000000000000000000, 0.000000000000000000 ) ) ;
#68081 = EDGE_LOOP ( 'NONE', ( #16865, #3877, #17164, #22662, #33308, #15346, #40374, #6021 ) ) ;
#68082 = DIRECTION ( 'NONE',  ( -0.000000000000000000, -1.000000000000000000, 0.000000000000000000 ) ) ;
#68083 = CIRCLE ( 'NONE', #2843, 7.500000000000007105 ) ;
#68084 = ADVANCED_FACE ( 'NONE', ( #45390 ), #31282, .F. ) ;
#68085 = CARTESIAN_POINT ( 'NONE',  ( -60.00000000000000000, -2.024042244987997205E-14, -11.50000000000000355 ) ) ;
#68086 = CARTESIAN_POINT ( 'NONE',  ( -60.43227690047157807, -7.519512524622562033, 4.573977915173213819E-17 ) ) ;
#68087 =( GEOMETRIC_REPRESENTATION_CONTEXT ( 3 ) GLOBAL_UNCERTAINTY_ASSIGNED_CONTEXT ( ( #55211 ) ) GLOBAL_UNIT_ASSIGNED_CONTEXT ( ( #26364, #22137, #37328 ) ) REPRESENTATION_CONTEXT ( 'NONE', 'WORKASPACE' ) );
#68088 = ORIENTED_EDGE ( 'NONE', *, *, #68972, .F. ) ;
#68089 = EDGE_CURVE ( 'NONE', #27009, #32736, #25666, .T. ) ;
#68090 = CARTESIAN_POINT ( 'NONE',  ( -87.50000000000000000, -6.499999999999990230, 3.000000000000000000 ) ) ;
#68091 = CARTESIAN_POINT ( 'NONE',  ( -86.24499999999999034, -4.716976649647093289, -6.492361379858945902 ) ) ;
#68092 = ORIENTED_EDGE ( 'NONE', *, *, #65978, .F. ) ;
#68093 = PRESENTATION_LAYER_ASSIGNMENT (  '', '', ( #28735 ) ) ;
#68094 = FILL_AREA_STYLE ('',( #47010 ) ) ;
#68095 = CARTESIAN_POINT ( 'NONE',  ( 74.89452121010485541, 14.00000000000000000, -66.39042820928574429 ) ) ;
#68096 = ADVANCED_FACE ( 'NONE', ( #45039 ), #29133, .T. ) ;
#68097 = ORIENTED_EDGE ( 'NONE', *, *, #26693, .T. ) ;
#68098 = CARTESIAN_POINT ( 'NONE',  ( 65.50000000000000000, 1.797044900979284448E-15, -6.500000000000000000 ) ) ;
#68099 = B_SPLINE_CURVE_WITH_KNOTS ( 'NONE', 3,
 ( #24182, #8379, #67805, #51623, #61454, #56899, #13272, #56184 ),
 .UNSPECIFIED., .F., .F.,
 ( 4, 2, 2, 4 ),
 ( 0.007148677244982143929, 0.009235234034391179292, 0.01027851242909569654, 0.01132179082380021552 ),
 .UNSPECIFIED. ) ;
#68100 = SURFACE_SIDE_STYLE ('',( #52616 ) ) ;
#68101 = EDGE_CURVE ( 'NONE', #64166, #9969, #66814, .T. ) ;
#68102 = DIRECTION ( 'NONE',  ( 1.000000000000000000, -0.000000000000000000, -0.000000000000000000 ) ) ;
#68103 = ORIENTED_EDGE ( 'NONE', *, *, #68161, .T. ) ;
#68104 = LINE ( 'NONE', #42105, #16245 ) ;
#68105 = VERTEX_POINT ( 'NONE', #66448 ) ;
#68106 = CARTESIAN_POINT ( 'NONE',  ( -34.99999999999992895, 110.4999999999999858, -10.00000000000000000 ) ) ;
#68107 = CARTESIAN_POINT ( 'NONE',  ( 12.75000000000000533, 28.24999999999998224, 4.000000000000000000 ) ) ;
#68108 = CARTESIAN_POINT ( 'NONE',  ( -167.1570736234661751, -9.058813317711329915, -2.943386871421370898 ) ) ;
#68109 = CARTESIAN_POINT ( 'NONE',  ( -5.598654528085808657, 113.6449999999999818, 7.705886871421373741 ) ) ;
#68110 = CARTESIAN_POINT ( 'NONE',  ( -102.3570736234661780, 5.598654528085804216, 7.705886871421366635 ) ) ;
#68111 = CIRCLE ( 'NONE', #25402, 1.000000000000000000 ) ;
#68112 = PRODUCT_DEFINITION_SHAPE ( 'NONE', 'NONE',  #43006 ) ;
#68113 = ORIENTED_EDGE ( 'NONE', *, *, #30971, .T. ) ;
#68114 = CARTESIAN_POINT ( 'NONE',  ( -82.64292637653379359, -5.598654528085801552, 7.705886871421367523 ) ) ;
#68115 = CARTESIAN_POINT ( 'NONE',  ( -52.00000000000000000, -1.926070501056209087E-14, 10.50000000000000000 ) ) ;
#68116 = FACE_OUTER_BOUND ( 'NONE', #30863, .T. ) ;
#68117 = CARTESIAN_POINT ( 'NONE',  ( -148.7049999999999841, 2.607480562269073321, 8.024999999999991473 ) ) ;
#68118 = DIRECTION ( 'NONE',  ( 0.000000000000000000, 0.000000000000000000, 1.000000000000000000 ) ) ;
#68119 = VECTOR ( 'NONE', #62855, 1000.000000000000000 ) ;
#68120 = CARTESIAN_POINT ( 'NONE',  ( -156.8950000000000102, 6.826472737025116366, 4.959722759717898555 ) ) ;
#68121 = PRESENTATION_LAYER_ASSIGNMENT (  '', '', ( #69216 ) ) ;
#68122 = CARTESIAN_POINT ( 'NONE',  ( -150.1450000000000102, -4.716976649647092401, 6.492361379858946790 ) ) ;
#68123 = B_SPLINE_CURVE_WITH_KNOTS ( 'NONE', 3,
 ( #42683, #41996, #4644, #21169 ),
 .UNSPECIFIED., .F., .F.,
 ( 4, 4 ),
 ( 0.000000000000000000, 0.001157321451656189446 ),
 .UNSPECIFIED. ) ;
#68124 = EDGE_LOOP ( 'NONE', ( #38937, #52967, #366, #19937 ) ) ;
#68125 = CARTESIAN_POINT ( 'NONE',  ( 98.00000000000000000, 0.000000000000000000, 0.000000000000000000 ) ) ;
#68126 = SURFACE_STYLE_FILL_AREA ( #46712 ) ;
#68127 = CARTESIAN_POINT ( 'NONE',  ( 20.83146879675249963, 149.9524772093542708, -9.749920261344563244 ) ) ;
#68128 = CARTESIAN_POINT ( 'NONE',  ( -66.05499999999999261, -9.827790563157499189E-16, -8.024999999999991473 ) ) ;
#68129 = CARTESIAN_POINT ( 'NONE',  ( -74.99999999999998579, 50.00000000000000000, -10.00000000000000000 ) ) ;
#68130 = FACE_OUTER_BOUND ( 'NONE', #35800, .T. ) ;
#68131 = AXIS2_PLACEMENT_3D ( 'NONE', #55508, #17881, #66050 ) ;
#68132 = CARTESIAN_POINT ( 'NONE',  ( -60.74499999999997613, 4.716976649647094177, 6.492361379858945902 ) ) ;
#68133 = CARTESIAN_POINT ( 'NONE',  ( -5.598654528085808657, 156.7549999999999670, 7.705886871421373741 ) ) ;
#68134 = MECHANICAL_DESIGN_GEOMETRIC_PRESENTATION_REPRESENTATION (  '', ( #20930 ), #42321 ) ;
#68135 = DIRECTION ( 'NONE',  ( -0.7185283436805277590, 0.09541336063812150270, -0.6889218460315054138 ) ) ;
#68136 = CARTESIAN_POINT ( 'NONE',  ( -195.0000000000000000, 0.000000000000000000, 9.524999999999991473 ) ) ;
#68137 = DIRECTION ( 'NONE',  ( 1.300977106640434891E-16, -0.000000000000000000, 1.000000000000000000 ) ) ;
#68138 = DIRECTION ( 'NONE',  ( 0.000000000000000000, 0.000000000000000000, 1.000000000000000000 ) ) ;
#68139 = CARTESIAN_POINT ( 'NONE',  ( -145.5570736234661808, -1.166476076187852838E-15, -9.524999999999991473 ) ) ;
#68140 = EDGE_CURVE ( 'NONE', #64410, #63457, #54874, .T. ) ;
#68141 = LINE ( 'NONE', #19926, #7232 ) ;
#68142 = ORIENTED_EDGE ( 'NONE', *, *, #48644, .F. ) ;
#68143 = ORIENTED_EDGE ( 'NONE', *, *, #40014, .F. ) ;
#68144 = CARTESIAN_POINT ( 'NONE',  ( 7.511572993685799101E-16, -2.500000000000000000, -6.999999999999997335 ) ) ;
#68145 = EDGE_CURVE ( 'NONE', #55963, #22804, #47403, .T. ) ;
#68146 = ADVANCED_FACE ( 'NONE', ( #18267 ), #2362, .T. ) ;
#68147 = CARTESIAN_POINT ( 'NONE',  ( -20.71462257042821520, 114.4999999999999574, 10.00000000000000355 ) ) ;
#68148 = CARTESIAN_POINT ( 'NONE',  ( 22.31817967265634195, 25.64624525132450472, -27.48625952250267801 ) ) ;
#68149 = EDGE_CURVE ( 'NONE', #7058, #43960, #49287, .T. ) ;
#68150 =( NAMED_UNIT ( * ) SI_UNIT ( $, .STERADIAN. ) SOLID_ANGLE_UNIT ( ) );
#68151 = EDGE_LOOP ( 'NONE', ( #22440, #1489, #34001, #41346 ) ) ;
#68152 = ORIENTED_EDGE ( 'NONE', *, *, #42457, .F. ) ;
#68153 = AXIS2_PLACEMENT_3D ( 'NONE', #4377, #47367, #16042 ) ;
#68154 = CYLINDRICAL_SURFACE ( 'NONE', #6188, 0.5000000000000004441 ) ;
#68155 = ADVANCED_FACE ( 'NONE', ( #65422 ), #60462, .F. ) ;
#68156 = EDGE_LOOP ( 'NONE', ( #60315, #29076, #65078, #13554 ) ) ;
#68157 = CARTESIAN_POINT ( 'NONE',  ( 10.01517768586949231, 121.8049999999999784, 1.839758294383810543E-15 ) ) ;
#68158 = DIRECTION ( 'NONE',  ( -0.000000000000000000, -0.000000000000000000, -1.000000000000000000 ) ) ;
#68159 =( GEOMETRIC_REPRESENTATION_CONTEXT ( 3 ) GLOBAL_UNCERTAINTY_ASSIGNED_CONTEXT ( ( #49006 ) ) GLOBAL_UNIT_ASSIGNED_CONTEXT ( ( #16538, #37668, #5576 ) ) REPRESENTATION_CONTEXT ( 'NONE', 'WORKASPACE' ) );
#68160 = SURFACE_STYLE_USAGE ( .BOTH. , #3738 ) ;
#68161 = EDGE_CURVE ( 'NONE', #6517, #11358, #3782, .T. ) ;
#68162 = AXIS2_PLACEMENT_3D ( 'NONE', #21887, #21524, #53542 ) ;
#68163 = ADVANCED_FACE ( 'NONE', ( #14361 ), #9810, .T. ) ;
#68164 = CARTESIAN_POINT ( 'NONE',  ( 0.000000000000000000, 43.00000000000000000, 0.000000000000000000 ) ) ;
#68165 = CARTESIAN_POINT ( 'NONE',  ( -106.1949999999999932, 8.437984349512085203, -1.550032578732815448E-15 ) ) ;
#68166 = EDGE_LOOP ( 'NONE', ( #15351, #22123, #67447, #32694 ) ) ;
#68167 = CARTESIAN_POINT ( 'NONE',  ( -9.436264504443260037, 110.5000000000000284, -1.368519874741629172 ) ) ;
#68168 = CARTESIAN_POINT ( 'NONE',  ( -164.9070736234663741, -3.094860106614866879, 9.525000000002579625 ) ) ;
#68169 = ADVANCED_FACE ( 'NONE', ( #52383 ), #51318, .T. ) ;
#68170 = LINE ( 'NONE', #8022, #58689 ) ;
#68171 = EDGE_LOOP ( 'NONE', ( #38517, #56683, #56076, #34482, #35181, #58975, #25938, #61056 ) ) ;
#68172 = CARTESIAN_POINT ( 'NONE',  ( 7.632228543268608334, 155.3429263765338249, -2.479861379858951942 ) ) ;
#68173 = SURFACE_STYLE_FILL_AREA ( #67819 ) ;
#68174 = VECTOR ( 'NONE', #65636, 1000.000000000000000 ) ;
#68175 = DIRECTION ( 'NONE',  ( 0.000000000000000000, -0.000000000000000000, 1.000000000000000000 ) ) ;
#68176 = ORIENTED_EDGE ( 'NONE', *, *, #51876, .T. ) ;
#68177 = DIRECTION ( 'NONE',  ( 0.000000000000000000, 0.000000000000000000, 1.000000000000000000 ) ) ;
#68178 = ORIENTED_EDGE ( 'NONE', *, *, #53556, .F. ) ;
#68179 = CARTESIAN_POINT ( 'NONE',  ( 20.44220712062818635, 115.3857587453612865, 10.00000000000000000 ) ) ;
#68180 = CARTESIAN_POINT ( 'NONE',  ( -195.0000000000000000, 0.000000000000000000, 0.000000000000000000 ) ) ;
#68181 = SURFACE_SIDE_STYLE ('',( #63580 ) ) ;
#68182 = CARTESIAN_POINT ( 'NONE',  ( -33.08284415674632584, -9.238994630453197132, 5.297413886133312211 ) ) ;
#68183 = CARTESIAN_POINT ( 'NONE',  ( -120.9549999999999983, -7.632228543268599452, 2.479861379858951054 ) ) ;
#68184 = DIRECTION ( 'NONE',  ( 1.000000000000000000, 0.000000000000000000, 0.000000000000000000 ) ) ;
#68185 = VECTOR ( 'NONE', #64932, 1000.000000000000000 ) ;
#68186 = CARTESIAN_POINT ( 'NONE',  ( -74.13102528387565826, 9.253287829606156478, 6.241231906388601480 ) ) ;
#68187 = DIRECTION ( 'NONE',  ( -0.000000000000000000, -0.000000000000000000, 1.000000000000000000 ) ) ;
#68188 = ORIENTED_EDGE ( 'NONE', *, *, #15292, .T. ) ;
#68189 = ORIENTED_EDGE ( 'NONE', *, *, #35606, .T. ) ;
#68190 = CARTESIAN_POINT ( 'NONE',  ( -15.98999599679679839, 146.9999999999999716, -7.500000000000000000 ) ) ;
#68191 = DIRECTION ( 'NONE',  ( -1.000000000000000000, 0.000000000000000000, 0.000000000000000000 ) ) ;
#68192 = CARTESIAN_POINT ( 'NONE',  ( -75.50000000000000000, 64.49137674618943095, 6.499999999999999112 ) ) ;
#68193 = ORIENTED_EDGE ( 'NONE', *, *, #39228, .F. ) ;
#68194 = SURFACE_SIDE_STYLE ('',( #57274 ) ) ;
#68195 = CARTESIAN_POINT ( 'NONE',  ( -176.4550000000000125, 7.632228543268599452, -2.479861379858951942 ) ) ;
#68196 = CARTESIAN_POINT ( 'NONE',  ( -91.04292637653379927, -9.058813317711329915, -2.943386871421370898 ) ) ;
#68197 = CARTESIAN_POINT ( 'NONE',  ( -48.05707362346617373, 0.000000000000000000, 9.524999999999991473 ) ) ;
#68198 = CARTESIAN_POINT ( 'NONE',  ( -177.1450000000000102, -4.716976649647092401, 6.492361379858946790 ) ) ;
#68199 = CARTESIAN_POINT ( 'NONE',  ( 40.83001745922079806, 108.1251451958518146, 3.311254650320280213 ) ) ;
#68200 = ORIENTED_EDGE ( 'NONE', *, *, #10289, .F. ) ;
#68201 = EDGE_CURVE ( 'NONE', #20613, #55582, #25711, .T. ) ;
#68202 = DIRECTION ( 'NONE',  ( 0.000000000000000000, 1.000000000000000000, -0.000000000000000000 ) ) ;
#68203 = FILL_AREA_STYLE ('',( #9117 ) ) ;
#68204 = DIRECTION ( 'NONE',  ( -1.300977106640434891E-16, 0.000000000000000000, -1.000000000000000000 ) ) ;
#68205 = CARTESIAN_POINT ( 'NONE',  ( -89.00499999999999545, 6.826472737025116366, 4.959722759717898555 ) ) ;
#68206 = FILL_AREA_STYLE_COLOUR ( '', #33160 ) ;
#68207 = PRESENTATION_STYLE_ASSIGNMENT (( #14745 ) ) ;
#68208 = CARTESIAN_POINT ( 'NONE',  ( -20.71231517720798010, 110.4999999999999858, 10.00000000000000000 ) ) ;
#68209 = PRESENTATION_LAYER_ASSIGNMENT (  '', '', ( #45784 ) ) ;
#68210 = CARTESIAN_POINT ( 'NONE',  ( -92.69499999999996476, -8.437984349512086979, 5.166775262442717831E-16 ) ) ;
#68211 = CARTESIAN_POINT ( 'NONE',  ( -9.058813317711337021, 123.1549999999999869, -2.943386871421374895 ) ) ;
#68212 = PRESENTATION_LAYER_ASSIGNMENT (  '', '', ( #9772 ) ) ;
#68213 = CARTESIAN_POINT ( 'NONE',  ( -64.49499999999997613, 6.826472737025113702, -4.959722759717902107 ) ) ;
#68214 = LINE ( 'NONE', #67870, #57800 ) ;
#68215 = CIRCLE ( 'NONE', #21001, 0.5000000000000000000 ) ;
#68216 = DIRECTION ( 'NONE',  ( 0.000000000000000000, 0.000000000000000000, -1.000000000000000000 ) ) ;
#68217 = SURFACE_STYLE_FILL_AREA ( #62565 ) ;
#68218 = DIRECTION ( 'NONE',  ( 0.000000000000000000, -1.000000000000000000, 0.000000000000000000 ) ) ;
#68219 = ORIENTED_EDGE ( 'NONE', *, *, #45629, .F. ) ;
#68220 = CARTESIAN_POINT ( 'NONE',  ( -104.2429263765338021, 5.598654528085804216, 7.705886871421366635 ) ) ;
#68221 = CARTESIAN_POINT ( 'NONE',  ( -128.5449999999999875, -7.632228543268600340, -2.479861379858950166 ) ) ;
#68222 = CARTESIAN_POINT ( 'NONE',  ( -47.00571487472603138, -11.02952041815452766, 0.9185643661977246355 ) ) ;
#68223 = AXIS2_PLACEMENT_3D ( 'NONE', #36070, #25489, #26770 ) ;
#68224 = EDGE_CURVE ( 'NONE', #38783, #57325, #25600, .T. ) ;
#68225 = CARTESIAN_POINT ( 'NONE',  ( -75.50000000000000000, 64.49137674618943095, -10.00000000000000000 ) ) ;
#68227 =( NAMED_UNIT ( * ) SI_UNIT ( $, .STERADIAN. ) SOLID_ANGLE_UNIT ( ) );
#68226 = DIRECTION ( 'NONE',  ( 0.000000000000000000, 0.000000000000000000, -1.000000000000000000 ) ) ;
#68228 = CARTESIAN_POINT ( 'NONE',  ( 68.99999999999998579, 8.450062914116736267E-15, -3.000000000000000000 ) ) ;
#68229 = ORIENTED_EDGE ( 'NONE', *, *, #10261, .F. ) ;
#68230 = ORIENTED_EDGE ( 'NONE', *, *, #26904, .F. ) ;
#68231 = CARTESIAN_POINT ( 'NONE',  ( 0.000000000000000000, 131.9429263765338192, -8.025000000000000355 ) ) ;
#68232 = EDGE_CURVE ( 'NONE', #16380, #66646, #40352, .T. ) ;
#68233 = CARTESIAN_POINT ( 'NONE',  ( 2.000000000000008882, 26.00000000000000355, -24.00000000000000355 ) ) ;
#68234 = CARTESIAN_POINT ( 'NONE',  ( 10.00000000000001776, 42.00000000000000000, -28.38386403503541899 ) ) ;
#68235 = PRESENTATION_STYLE_ASSIGNMENT (( #30567 ) ) ;
#68236 =( NAMED_UNIT ( * ) PLANE_ANGLE_UNIT ( ) SI_UNIT ( $, .RADIAN. ) );
#68237 = ORIENTED_EDGE ( 'NONE', *, *, #9414, .F. ) ;
#68238 = CARTESIAN_POINT ( 'NONE',  ( -125.0049999999999812, 6.826472737025115478, 4.959722759717899443 ) ) ;
#68239 = ORIENTED_EDGE ( 'NONE', *, *, #56048, .T. ) ;
#68240 = DIRECTION ( 'NONE',  ( 0.000000000000000000, 0.000000000000000000, 1.000000000000000000 ) ) ;
#68241 = CARTESIAN_POINT ( 'NONE',  ( -126.3570736234661780, 5.598654528085804216, 7.705886871421366635 ) ) ;
#68242 = ORIENTED_EDGE ( 'NONE', *, *, #51949, .T. ) ;
#68243 = DIRECTION ( 'NONE',  ( 0.000000000000000000, 1.000000000000000000, 0.000000000000000000 ) ) ;
#68244 = CARTESIAN_POINT ( 'NONE',  ( 48.50000000000000000, 22.24999999999998579, 4.000000000000000000 ) ) ;
#68245 = ORIENTED_EDGE ( 'NONE', *, *, #52996, .T. ) ;
#68246 = EDGE_CURVE ( 'NONE', #31871, #17336, #6618, .T. ) ;
#68247 = CARTESIAN_POINT ( 'NONE',  ( 6.062177826491070398, 3.500000000000002665, 0.000000000000000000 ) ) ;
#68248 = CARTESIAN_POINT ( 'NONE',  ( 8.102448949553183510, 150.9950000000000045, -5.886773742842746238 ) ) ;
#68249 = ORIENTED_EDGE ( 'NONE', *, *, #58016, .T. ) ;
#68250 = CARTESIAN_POINT ( 'NONE',  ( -3.094860106618434248, 150.9049999999999727, 9.525000000000000355 ) ) ;
#68251 = CARTESIAN_POINT ( 'NONE',  ( -8.750000000000001776, 24.74999999999998579, 3.750000000000000000 ) ) ;
#68252 = ADVANCED_FACE ( 'NONE', ( #41141 ), #20338, .F. ) ;
#68253 = DIRECTION ( 'NONE',  ( 0.000000000000000000, 0.000000000000000000, -1.000000000000000000 ) ) ;
#68254 = ORIENTED_EDGE ( 'NONE', *, *, #34541, .T. ) ;
#68255 = CARTESIAN_POINT ( 'NONE',  ( -6.826472737025120807, 114.9929263765338163, 4.959722759717906548 ) ) ;
#68256 =( LENGTH_UNIT ( ) NAMED_UNIT ( * ) SI_UNIT ( .MILLI., .METRE. ) );
#68257 = CARTESIAN_POINT ( 'NONE',  ( 45.00000000000000000, 9.999999999999992895, 6.000000000000001776 ) ) ;
#68258 = CIRCLE ( 'NONE', #45827, 0.5000000000000004441 ) ;
#68259 = CARTESIAN_POINT ( 'NONE',  ( 17.75000000000000711, 30.99999999999999289, 3.750000000000000000 ) ) ;
#68260 = CARTESIAN_POINT ( 'NONE',  ( 20.94636006565341191, 149.9999999999999716, -9.500000000000000000 ) ) ;
#68261 =( GEOMETRIC_REPRESENTATION_CONTEXT ( 3 ) GLOBAL_UNCERTAINTY_ASSIGNED_CONTEXT ( ( #22939 ) ) GLOBAL_UNIT_ASSIGNED_CONTEXT ( ( #36645, #52790, #68266 ) ) REPRESENTATION_CONTEXT ( 'NONE', 'WORKASPACE' ) );
#68262 = ORIENTED_EDGE ( 'NONE', *, *, #59242, .F. ) ;
#68263 = CARTESIAN_POINT ( 'NONE',  ( 29.00000000000002842, 34.80256050929376954, 80.00402776293826435 ) ) ;
#68264 = ORIENTED_EDGE ( 'NONE', *, *, #27893, .T. ) ;
#68265 = CARTESIAN_POINT ( 'NONE',  ( -58.49292637653379501, -8.102448949553172852, 5.886773742842742685 ) ) ;
#68266 =( NAMED_UNIT ( * ) SI_UNIT ( $, .STERADIAN. ) SOLID_ANGLE_UNIT ( ) );
#68267 = DIRECTION ( 'NONE',  ( -1.000000000000000000, 0.000000000000000000, 0.000000000000000000 ) ) ;
#68268 = CARTESIAN_POINT ( 'NONE',  ( -155.6049999999999329, 6.826472737025113702, -4.959722759717902107 ) ) ;
#68269 = ORIENTED_EDGE ( 'NONE', *, *, #54384, .F. ) ;
#68270 = FACE_OUTER_BOUND ( 'NONE', #26079, .T. ) ;
#68271 = CARTESIAN_POINT ( 'NONE',  ( -74.99999999999998579, 50.00000000000000000, -10.00000000000000000 ) ) ;
#68272 = PLANE ( 'NONE',  #3481 ) ;
#68273 = CARTESIAN_POINT ( 'NONE',  ( -70.94292637653380496, 0.000000000000000000, 9.524999999999991473 ) ) ;
#68274 = CARTESIAN_POINT ( 'NONE',  ( 8.437984349512095861, 146.1929263765338192, 1.550032578732816828E-15 ) ) ;
#68275 = EDGE_LOOP ( 'NONE', ( #66500, #33361, #35796, #25773 ) ) ;
#68276 = ORIENTED_EDGE ( 'NONE', *, *, #28177, .T. ) ;
#68277 = DIRECTION ( 'NONE',  ( -7.709882115452468306E-16, -1.000000000000000000, 0.000000000000000000 ) ) ;
#68278 = CIRCLE ( 'NONE', #12059, 1.000000000000000000 ) ;
#68279 = CARTESIAN_POINT ( 'NONE',  ( -62.00499999999999545, 6.826472737025116366, 4.959722759717898555 ) ) ;
#68280 = EDGE_LOOP ( 'NONE', ( #51988, #27705, #29210, #36615 ) ) ;
#68281 = FILL_AREA_STYLE ('',( #67583 ) ) ;
#68282 = DIRECTION ( 'NONE',  ( 0.000000000000000000, -3.469446951953614189E-15, -1.000000000000000000 ) ) ;
#68283 = ORIENTED_EDGE ( 'NONE', *, *, #28325, .F. ) ;
#68284 = EDGE_CURVE ( 'NONE', #45556, #33218, #49339, .T. ) ;
#68285 = CARTESIAN_POINT ( 'NONE',  ( -74.09571531523221211, 9.387774908331740775, -6.120769290545540642 ) ) ;
#68286 = DIRECTION ( 'NONE',  ( 0.000000000000000000, -0.6449798928094538919, 0.7641995406119433953 ) ) ;
#68287 = EDGE_CURVE ( 'NONE', #5366, #55052, #41466, .T. ) ;
#68289 = LINE ( 'NONE', #25365, #55019 ) ;
#68288 = LINE ( 'NONE', #35590, #9912 ) ;
#68290 = CARTESIAN_POINT ( 'NONE',  ( -9.058813317711338797, 149.3449999999999989, 2.943386871421373563 ) ) ;
#68291 = CARTESIAN_POINT ( 'NONE',  ( -93.74499999999999034, 4.716976649647094177, 6.492361379858945902 ) ) ;
#68292 = B_SPLINE_CURVE_WITH_KNOTS ( 'NONE', 3,
 ( #50547, #12896, #65327, #34004, #61413, #55101, #28715, #55810, #38991, #44271, #6237, #34361, #2269, #66721, #40024, #7288, #13230, #49173, #60382, #43916, #33658, #54747, #1598, #874, #55464, #23126 ),
 .UNSPECIFIED., .F., .F.,
 ( 4, 2, 2, 2, 2, 2, 2, 2, 2, 2, 2, 2, 4 ),
 ( 0.008651501742289673114, 0.01053121843691355759, 0.01241093513153744381, 0.01335079347884938865, 0.01429065182616133696, 0.01523051017347328354, 0.01617036852078523185, 0.01805008521540912153, 0.01898994356272106984, 0.01992980191003301815, 0.02086966025734496299, 0.02180951860465690784, 0.02368923529928080099 ),
 .UNSPECIFIED. ) ;
#68293 = CARTESIAN_POINT ( 'NONE',  ( 44.00000000000000000, 21.74999999999998579, 3.750000000000000000 ) ) ;
#68294 = CARTESIAN_POINT ( 'NONE',  ( 28.00000000000000000, 38.00000000000000711, -90.00000000000000000 ) ) ;
#68295 =( BOUNDED_CURVE ( )  B_SPLINE_CURVE ( 2, ( #15464, #11182, #48175, #26649, #15126, #31240, #5539, #36926, #10850, #42230, #64667 ),
 .UNSPECIFIED., .F., .F. ) 
 B_SPLINE_CURVE_WITH_KNOTS ( ( 3, 2, 2, 2, 2, 3 ),
 ( 0.7934782608695651884, 0.7956521739130434367, 0.7978260869565216851, 0.8000000000000000444, 0.8021739130434782927, 0.8043478260869565410 ),
 .UNSPECIFIED. ) 
 CURVE ( )  GEOMETRIC_REPRESENTATION_ITEM ( )  RATIONAL_B_SPLINE_CURVE ( ( 1.000000000000000000, 0.9510565162951535312, 1.000000000000000000, 0.9510565162951535312, 1.000000000000000000, 0.9510565162951535312, 1.000000000000000000, 0.9510565162951535312, 1.000000000000000000, 0.9510565162951535312, 1.000000000000000000 ) ) 
 REPRESENTATION_ITEM ( '' )  );
#68296 = CARTESIAN_POINT ( 'NONE',  ( -7.632228543268608334, 144.8429263765338249, 2.479861379858952830 ) ) ;
#68297 = ORIENTED_EDGE ( 'NONE', *, *, #35373, .T. ) ;
#68298 = VECTOR ( 'NONE', #19567, 1000.000000000000000 ) ;
#68299 = CARTESIAN_POINT ( 'NONE',  ( -137.8429263765337964, 9.058813317711329915, -2.943386871421373119 ) ) ;
#68300 =( NAMED_UNIT ( * ) SI_UNIT ( $, .STERADIAN. ) SOLID_ANGLE_UNIT ( ) );
#68301 = CARTESIAN_POINT ( 'NONE',  ( -154.6450000000000102, 4.716976649647091513, -6.492361379858946790 ) ) ;
#68302 = DIRECTION ( 'NONE',  ( 0.000000000000000000, -1.000000000000000000, 0.000000000000000000 ) ) ;
#68303 = CIRCLE ( 'NONE', #30065, 0.2500000000000002220 ) ;
#68304 = AXIS2_PLACEMENT_3D ( 'NONE', #64193, #68812, #30795 ) ;
#68305 = EDGE_CURVE ( 'NONE', #20640, #17311, #32273, .T. ) ;
#68306 = ADVANCED_FACE ( 'NONE', ( #43240 ), #31575, .T. ) ;
#68307 = DIRECTION ( 'NONE',  ( 1.000000000000000000, 0.000000000000000000, 0.000000000000000000 ) ) ;
#68308 = SURFACE_STYLE_USAGE ( .BOTH. , #69347 ) ;
#68309 = FILL_AREA_STYLE ('',( #30284 ) ) ;
#68310 = ORIENTED_EDGE ( 'NONE', *, *, #26889, .T. ) ;
#68311 =( GEOMETRIC_REPRESENTATION_CONTEXT ( 3 ) GLOBAL_UNCERTAINTY_ASSIGNED_CONTEXT ( ( #33392 ) ) GLOBAL_UNIT_ASSIGNED_CONTEXT ( ( #42824, #31858, #20975 ) ) REPRESENTATION_CONTEXT ( 'NONE', 'WORKASPACE' ) );
#68312 =( NAMED_UNIT ( * ) PLANE_ANGLE_UNIT ( ) SI_UNIT ( $, .RADIAN. ) );
#68313 = EDGE_LOOP ( 'NONE', ( #46468, #1902, #4915, #17582 ) ) ;
#68314 = EDGE_CURVE ( 'NONE', #7436, #15321, #56043, .T. ) ;
#68315 = CARTESIAN_POINT ( 'NONE',  ( -4.716976649647098618, 118.1429263765338078, 6.492361379858953008 ) ) ;
#68316 = CARTESIAN_POINT ( 'NONE',  ( 4.716976649647099507, 119.6429263765338078, -6.492361379858953008 ) ) ;
#68317 = CARTESIAN_POINT ( 'NONE',  ( 22.00000000000000711, 50.00000000000000000, -60.00000000000000000 ) ) ;
#68318 = AXIS2_PLACEMENT_3D ( 'NONE', #2108, #44797, #45140 ) ;
#68319 = EDGE_CURVE ( 'NONE', #14417, #68764, #47106, .T. ) ;
#68320 = MECHANICAL_DESIGN_GEOMETRIC_PRESENTATION_REPRESENTATION (  '', ( #21112 ), #42492 ) ;
#68321 = ORIENTED_EDGE ( 'NONE', *, *, #56539, .T. ) ;
#68322 = CARTESIAN_POINT ( 'NONE',  ( -149.4550000000000125, 7.632228543268599452, -2.479861379858951942 ) ) ;
#68323 = VERTEX_POINT ( 'NONE', #38293 ) ;
#68324 = CARTESIAN_POINT ( 'NONE',  ( -21.02379604162863558, 114.6409683457797115, -9.999999999999998224 ) ) ;
#68325 = DIRECTION ( 'NONE',  ( 5.782411586589351722E-16, 1.000000000000000000, -0.000000000000000000 ) ) ;
#68326 = EDGE_LOOP ( 'NONE', ( #63676, #22632, #36256, #20760 ) ) ;
#68327 = ADVANCED_FACE ( 'NONE', ( #10142 ), #22363, .T. ) ;
#68328 = CARTESIAN_POINT ( 'NONE',  ( -10.01517768586949231, 125.1950000000000074, -6.132527647946036459E-16 ) ) ;
#68329 = ORIENTED_EDGE ( 'NONE', *, *, #26577, .F. ) ;
#68330 = CARTESIAN_POINT ( 'NONE',  ( -58.79292637653379927, -3.094860106618429807, 9.524999999999991473 ) ) ;
#68331 = CARTESIAN_POINT ( 'NONE',  ( -5.598654528085806881, 116.8549999999999898, -7.705886871421374629 ) ) ;
#68332 = CARTESIAN_POINT ( 'NONE',  ( -72.20499999999998408, -2.607480562269071545, -8.024999999999991473 ) ) ;
#68333 = EDGE_CURVE ( 'NONE', #24476, #44314, #35822, .T. ) ;
#68334 = CARTESIAN_POINT ( 'NONE',  ( 28.00000000000002842, 38.70020753820971748, 89.00000000000000000 ) ) ;
#68335 = ORIENTED_EDGE ( 'NONE', *, *, #37138, .F. ) ;
#68336 = CARTESIAN_POINT ( 'NONE',  ( 10.01517768586949231, 133.8049999999999784, 1.839758294383810543E-15 ) ) ;
#68337 = DIRECTION ( 'NONE',  ( -1.000000000000000000, 0.000000000000000000, 0.000000000000000000 ) ) ;
#68338 = DIRECTION ( 'NONE',  ( 0.000000000000000000, 0.000000000000000000, -1.000000000000000000 ) ) ;
#68339 = FACE_OUTER_BOUND ( 'NONE', #27693, .T. ) ;
#68340 = DIRECTION ( 'NONE',  ( 1.000000000000000000, 0.000000000000000000, 0.000000000000000000 ) ) ;
#68341 = ORIENTED_EDGE ( 'NONE', *, *, #59566, .T. ) ;
#68342 = CARTESIAN_POINT ( 'NONE',  ( 3.999798566743339556, 8.867945265733707672, 2.000000000000000000 ) ) ;
#68343 = DIRECTION ( 'NONE',  ( -1.000000000000000000, 0.000000000000000000, 0.000000000000000000 ) ) ;
#68344 = DIRECTION ( 'NONE',  ( 1.000000000000000000, 0.000000000000000000, 0.000000000000000000 ) ) ;
#68345 = CARTESIAN_POINT ( 'NONE',  ( -177.5049999999999670, -6.826472737025115478, -4.959722759717899443 ) ) ;
#68346 = VERTEX_POINT ( 'NONE', #37614 ) ;
#68347 = LINE ( 'NONE', #37067, #2467 ) ;
#68348 = SURFACE_STYLE_FILL_AREA ( #40954 ) ;
#68349 = ORIENTED_EDGE ( 'NONE', *, *, #64074, .F. ) ;
#68350 = CYLINDRICAL_SURFACE ( 'NONE', #34300, 0.5000000000000004441 ) ;
#68351 = CARTESIAN_POINT ( 'NONE',  ( 96.10348817448824832, 5.000000000000000000, -27.38099488609876531 ) ) ;
#68352 = ORIENTED_EDGE ( 'NONE', *, *, #39976, .T. ) ;
#68353 = AXIS2_PLACEMENT_3D ( 'NONE', #37431, #63059, #64095 ) ;
#68354 = AXIS2_PLACEMENT_3D ( 'NONE', #16736, #16403, #43151 ) ;
#68355 = DIRECTION ( 'NONE',  ( 1.000000000000000000, -0.000000000000000000, -0.000000000000000000 ) ) ;
#68356 = PRESENTATION_STYLE_ASSIGNMENT (( #9273 ) ) ;
#68357 = CARTESIAN_POINT ( 'NONE',  ( -93.50499999999999545, -6.826472737025115478, -4.959722759717899443 ) ) ;
#68358 = ORIENTED_EDGE ( 'NONE', *, *, #55603, .F. ) ;
#68359 = PLANE ( 'NONE',  #29468 ) ;
#68360 = TOROIDAL_SURFACE ( 'NONE', #45880, 1.499999999999998668, 1.000000000000000000 ) ;
#68361 = CARTESIAN_POINT ( 'NONE',  ( -138.9570736234661865, 9.058813317711329915, -2.943386871421373119 ) ) ;
#68362 = FACE_OUTER_BOUND ( 'NONE', #26960, .T. ) ;
#68363 = CARTESIAN_POINT ( 'NONE',  ( -78.65707362346617515, 9.058813317711329915, 2.943386871421369566 ) ) ;
#68364 = EDGE_CURVE ( 'NONE', #33812, #63576, #65294, .T. ) ;
#68365 = FACE_OUTER_BOUND ( 'NONE', #32564, .T. ) ;
#68366 = ORIENTED_EDGE ( 'NONE', *, *, #33071, .F. ) ;
#68367 = DIRECTION ( 'NONE',  ( 0.000000000000000000, 0.000000000000000000, -1.000000000000000000 ) ) ;
#68368 = DIRECTION ( 'NONE',  ( 3.469446951953611033E-15, 0.000000000000000000, 1.000000000000000000 ) ) ;
#68369 = CARTESIAN_POINT ( 'NONE',  ( -110.9049999999999727, 2.607480562269068880, -8.024999999999993250 ) ) ;
#68370 = CARTESIAN_POINT ( 'NONE',  ( -45.00000000000000000, 99.99999999999992895, 10.00000000000000000 ) ) ;
#68371 = CARTESIAN_POINT ( 'NONE',  ( 9.058813317711338797, 117.8449999999999847, -2.943386871421372675 ) ) ;
#68372 = CARTESIAN_POINT ( 'NONE',  ( -126.4450000000000074, 0.000000000000000000, 8.024999999999991473 ) ) ;
#68373 = CARTESIAN_POINT ( 'NONE',  ( -111.2070736234670534, 3.094860106633222863, 9.524999999989246291 ) ) ;
#68374 = CARTESIAN_POINT ( 'NONE',  ( 29.00000000000000355, 42.58578643762690774, -80.00402776293826435 ) ) ;
#68375 = EDGE_CURVE ( 'NONE', #8613, #40384, #31334, .T. ) ;
#68376 = ORIENTED_EDGE ( 'NONE', *, *, #22968, .F. ) ;
#68377 = CARTESIAN_POINT ( 'NONE',  ( 23.21231517720798010, 117.4999999999999716, -9.500000000000000000 ) ) ;
#68378 = CIRCLE ( 'NONE', #64988, 1.000000000000000888 ) ;
#68379 = CARTESIAN_POINT ( 'NONE',  ( -174.4429263765337907, -1.166476076187852838E-15, -9.524999999999991473 ) ) ;
#68380 = SURFACE_STYLE_FILL_AREA ( #3617 ) ;
#68381 = EDGE_CURVE ( 'NONE', #30219, #38604, #64285, .T. ) ;
#68382 = STYLED_ITEM ( 'NONE', ( #32427 ), #41887 ) ;
#68383 = EDGE_CURVE ( 'NONE', #29587, #60780, #10491, .T. ) ;
#68384 = ADVANCED_FACE ( 'NONE', ( #48852 ), #26798, .T. ) ;
#68385 = FILL_AREA_STYLE ('',( #29708 ) ) ;
#68386 = MECHANICAL_DESIGN_GEOMETRIC_PRESENTATION_REPRESENTATION (  '', ( #36997 ), #4320 ) ;
#68387 = DIRECTION ( 'NONE',  ( -0.7833176619561783571, 0.6216216216216310375, 0.000000000000000000 ) ) ;
#68388 = ORIENTED_EDGE ( 'NONE', *, *, #40463, .F. ) ;
#68389 = CARTESIAN_POINT ( 'NONE',  ( -81.29292637653379927, 3.094860106618428031, -9.524999999999993250 ) ) ;
#68390 = AXIS2_PLACEMENT_3D ( 'NONE', #51220, #30417, #36090 ) ;
#68391 =( BOUNDED_CURVE ( )  B_SPLINE_CURVE ( 2, ( #62053, #68062, #51878, #41341, #35352, #67347, #51182, #3635, #56093, #67015, #14235 ),
 .UNSPECIFIED., .F., .F. ) 
 B_SPLINE_CURVE_WITH_KNOTS ( ( 3, 2, 2, 2, 2, 3 ),
 ( 0.03260869565217316274, 0.03478260869565137636, 0.03695652173912958999, 0.03913043478260780361, 0.04130434782608601030, 0.04347826086956422392 ),
 .UNSPECIFIED. ) 
 CURVE ( )  GEOMETRIC_REPRESENTATION_ITEM ( )  RATIONAL_B_SPLINE_CURVE ( ( 1.000000000000016653, 0.9510565162951365448, 1.000000000000000000, 0.9510565162951535312, 1.000000000000000000, 0.9510565162951535312, 1.000000000000000000, 0.9510565162951535312, 1.000000000000000000, 0.9510565162951758467, 0.9999999999999776845 ) ) 
 REPRESENTATION_ITEM ( '' )  );
#68392 = ADVANCED_FACE ( 'NONE', ( #42892 ), #22076, .F. ) ;
#68393 = FACE_OUTER_BOUND ( 'NONE', #8557, .T. ) ;
#68394 = FACE_OUTER_BOUND ( 'NONE', #19714, .T. ) ;
#68395 = EDGE_CURVE ( 'NONE', #57600, #56195, #39661, .T. ) ;
#68396 =( LENGTH_UNIT ( ) NAMED_UNIT ( * ) SI_UNIT ( .MILLI., .METRE. ) );
#68397 = ORIENTED_EDGE ( 'NONE', *, *, #15691, .T. ) ;
#68398 = CARTESIAN_POINT ( 'NONE',  ( -135.8929263765338078, -8.102448949553174629, -5.886773742842741797 ) ) ;
#68399 =( NAMED_UNIT ( * ) SI_UNIT ( $, .STERADIAN. ) SOLID_ANGLE_UNIT ( ) );
#68400 =( LENGTH_UNIT ( ) NAMED_UNIT ( * ) SI_UNIT ( .MILLI., .METRE. ) );
#68401 = VERTEX_POINT ( 'NONE', #18537 ) ;
#68402 = CYLINDRICAL_SURFACE ( 'NONE', #62282, 5.000000000000000000 ) ;
#68403 = VECTOR ( 'NONE', #21999, 1000.000000000000000 ) ;
#68404 = DIRECTION ( 'NONE',  ( 0.000000000000000000, -1.000000000000000000, 0.000000000000000000 ) ) ;
#68405 = CARTESIAN_POINT ( 'NONE',  ( -6.826472737025120807, 137.1070736234661354, 4.959722759717906548 ) ) ;
#68406 = SURFACE_STYLE_USAGE ( .BOTH. , #30390 ) ;
#68407 = AXIS2_PLACEMENT_3D ( 'NONE', #41665, #63081, #31061 ) ;
#68408 = ORIENTED_EDGE ( 'NONE', *, *, #41565, .F. ) ;
#68409 = CARTESIAN_POINT ( 'NONE',  ( -100.1049999999999898, -6.826472737025113702, 4.959722759717902107 ) ) ;
#68410 = TOROIDAL_SURFACE ( 'NONE', #7737, 3.499999999999998668, 1.000000000000000000 ) ;
#68411 = CARTESIAN_POINT ( 'NONE',  ( -55.94292637653380496, 0.000000000000000000, 9.524999999999991473 ) ) ;
#68412 = EDGE_LOOP ( 'NONE', ( #3185, #24366, #60881, #36805 ) ) ;
#68413 = SURFACE_STYLE_USAGE ( .BOTH. , #4019 ) ;
#68414 = CARTESIAN_POINT ( 'NONE',  ( 34.99999999999999289, 99.99999999999998579, -3.500000000000000000 ) ) ;
#68415 = DIRECTION ( 'NONE',  ( 0.000000000000000000, 1.000000000000000000, -0.000000000000000000 ) ) ;
#68416 = EDGE_CURVE ( 'NONE', #47418, #4847, #6928, .T. ) ;
#68417 = ORIENTED_EDGE ( 'NONE', *, *, #47750, .T. ) ;
#68418 = CARTESIAN_POINT ( 'NONE',  ( -13.10261986875638129, 54.37406082015609599, 6.765796499695130528 ) ) ;
#68419 = EDGE_CURVE ( 'NONE', #64166, #24250, #66129, .T. ) ;
#68420 = CARTESIAN_POINT ( 'NONE',  ( -76.79499999999998749, 2.607480562269068880, -8.024999999999993250 ) ) ;
#68421 = ORIENTED_EDGE ( 'NONE', *, *, #37719, .T. ) ;
#68422 = CARTESIAN_POINT ( 'NONE',  ( -74.99999999999998579, 50.00000000000000000, -12.00000000000000000 ) ) ;
#68423 = CARTESIAN_POINT ( 'NONE',  ( 21.75000000000001066, 22.24999999999998224, -3.750000000000000000 ) ) ;
#68424 =( GEOMETRIC_REPRESENTATION_CONTEXT ( 3 ) GLOBAL_UNCERTAINTY_ASSIGNED_CONTEXT ( ( #26360 ) ) GLOBAL_UNIT_ASSIGNED_CONTEXT ( ( #9467, #35499, #24921 ) ) REPRESENTATION_CONTEXT ( 'NONE', 'WORKASPACE' ) );
#68425 = UNCERTAINTY_MEASURE_WITH_UNIT (LENGTH_MEASURE( 1.000000000000000082E-05 ), #34656, 'distance_accuracy_value', 'NONE');
#68426 = ORIENTED_EDGE ( 'NONE', *, *, #58339, .T. ) ;
#68427 = FACE_OUTER_BOUND ( 'NONE', #15507, .T. ) ;
#68428 = DIRECTION ( 'NONE',  ( -1.000000000000000000, 0.000000000000000000, 0.000000000000000000 ) ) ;
#68429 = DIRECTION ( 'NONE',  ( 1.000000000000000000, 9.376883653928687363E-17, -0.000000000000000000 ) ) ;
#68430 = DIRECTION ( 'NONE',  ( 0.000000000000000000, 1.000000000000000000, 0.000000000000000000 ) ) ;
#68431 = ORIENTED_EDGE ( 'NONE', *, *, #41671, .T. ) ;
#68432 =( NAMED_UNIT ( * ) SI_UNIT ( $, .STERADIAN. ) SOLID_ANGLE_UNIT ( ) );
#68433 = EDGE_LOOP ( 'NONE', ( #2346, #54821, #59655, #17344 ) ) ;
#68434 = AXIS2_PLACEMENT_3D ( 'NONE', #2987, #18182, #34009 ) ;
#68435 =( NAMED_UNIT ( * ) SI_UNIT ( $, .STERADIAN. ) SOLID_ANGLE_UNIT ( ) );
#68436 = CARTESIAN_POINT ( 'NONE',  ( -150.4429263765338192, -1.166476076187852838E-15, -9.524999999999991473 ) ) ;
#68437 = DIRECTION ( 'NONE',  ( -0.000000000000000000, 0.000000000000000000, -1.000000000000000000 ) ) ;
#68438 = CIRCLE ( 'NONE', #2114, 1.000000000000000888 ) ;
#68439 = CARTESIAN_POINT ( 'NONE',  ( -165.6570736234661751, 9.058813317711329915, 2.943386871421369566 ) ) ;
#68440 = CARTESIAN_POINT ( 'NONE',  ( -10.01517768586949408, 119.1949999999999790, -6.132527647946036459E-16 ) ) ;
#68441 = CIRCLE ( 'NONE', #65055, 0.2500000000000002220 ) ;
#68442 = CARTESIAN_POINT ( 'NONE',  ( -104.1570736234661751, -9.058813317711329915, -2.943386871421370898 ) ) ;
#68443 = FACE_OUTER_BOUND ( 'NONE', #17802, .T. ) ;
#68444 = LINE ( 'NONE', #25515, #69516 ) ;
#68445 = ORIENTED_EDGE ( 'NONE', *, *, #62638, .F. ) ;
#68446 = AXIS2_PLACEMENT_3D ( 'NONE', #7897, #52147, #29343 ) ;
#68447 = SURFACE_STYLE_USAGE ( .BOTH. , #57904 ) ;
#68448 = CARTESIAN_POINT ( 'NONE',  ( -28.74999999999999645, -13.99999999999999822, 15.00000000000000178 ) ) ;
#68449 = CARTESIAN_POINT ( 'NONE',  ( -71.62068965517238439, 63.58603185604027885, 7.500000000000000000 ) ) ;
#68450 = CARTESIAN_POINT ( 'NONE',  ( -145.8549999999999898, 4.716976649647094177, 6.492361379858945902 ) ) ;
#68451 = CARTESIAN_POINT ( 'NONE',  ( -3.148793198257116455, 110.7976376722492802, -8.711325744658216408 ) ) ;
#68452 = EDGE_CURVE ( 'NONE', #18083, #40281, #66013, .T. ) ;
#68453 = CARTESIAN_POINT ( 'NONE',  ( -159.1449999999999818, -4.716976649647092401, 6.492361379858946790 ) ) ;
#68454 = MECHANICAL_DESIGN_GEOMETRIC_PRESENTATION_REPRESENTATION (  '', ( #54963 ), #19019 ) ;
#68455 = CARTESIAN_POINT ( 'NONE',  ( -146.5449999999999875, -7.632228543268600340, -2.479861379858950166 ) ) ;
#68456 = EDGE_LOOP ( 'NONE', ( #51874, #47204, #32829 ) ) ;
#68457 = COLOUR_RGB ( '', 0.72549020, 0.75294118, 0.79215686) ;
#68458 = DIRECTION ( 'NONE',  ( 1.000000000000000000, 0.000000000000000000, 0.000000000000000000 ) ) ;
#68459 = EDGE_CURVE ( 'NONE', #47153, #34665, #23454, .T. ) ;
#68460 = CARTESIAN_POINT ( 'NONE',  ( 20.76401515593078884, 149.8168068008927492, -9.892342186632994583 ) ) ;
#68461 = UNCERTAINTY_MEASURE_WITH_UNIT (LENGTH_MEASURE( 1.000000000000000082E-05 ), #55868, 'distance_accuracy_value', 'NONE');
#68462 = CARTESIAN_POINT ( 'NONE',  ( -66.50499999999996703, -6.826472737025115478, -4.959722759717899443 ) ) ;
#68463 = DIRECTION ( 'NONE',  ( 0.9704308468600219006, 0.2413793103448194366, -0.000000000000000000 ) ) ;
#68464 = EDGE_CURVE ( 'NONE', #6587, #36170, #29049, .T. ) ;
#68465 = CARTESIAN_POINT ( 'NONE',  ( -62.54499999999998749, -7.632228543268600340, -2.479861379858950166 ) ) ;
#68466 = CARTESIAN_POINT ( 'NONE',  ( -3.094860106618434248, 159.9050000000000011, 9.525000000000000355 ) ) ;
#68467 = CARTESIAN_POINT ( 'NONE',  ( -44.50000000000000000, 99.99999999999992895, -3.500000000000000000 ) ) ;
#68468 = CARTESIAN_POINT ( 'NONE',  ( -143.0070736234661695, -8.102448949553174629, -5.886773742842741797 ) ) ;
#68469 = FILL_AREA_STYLE_COLOUR ( '', #828 ) ;
#68470 = COLOUR_RGB ( '', 0.08235294, 0.09019608, 0.10196078) ;
#68471 = VECTOR ( 'NONE', #2961, 1000.000000000000000 ) ;
#68472 = UNCERTAINTY_MEASURE_WITH_UNIT (LENGTH_MEASURE( 1.000000000000000082E-05 ), #20347, 'distance_accuracy_value', 'NONE');
#68473 = CARTESIAN_POINT ( 'NONE',  ( -152.9929263765337737, 8.102448949553172852, -5.886773742842744461 ) ) ;
#68474 = AXIS2_PLACEMENT_3D ( 'NONE', #31764, #53253, #69415 ) ;
#68475 = CARTESIAN_POINT ( 'NONE',  ( -5.000000000000000000, 0.000000000000000000, 1.000000000000000000 ) ) ;
#68476 = DIRECTION ( 'NONE',  ( -0.000000000000000000, -1.000000000000000000, 0.000000000000000000 ) ) ;
#68477 = AXIS2_PLACEMENT_3D ( 'NONE', #26128, #6065, #27150 ) ;
#68478 = EDGE_CURVE ( 'NONE', #50010, #24888, #68292, .T. ) ;
#68479 = CARTESIAN_POINT ( 'NONE',  ( -24.21231517720798365, 50.00000000000000000, 7.500000000000000000 ) ) ;
#68480 = CARTESIAN_POINT ( 'NONE',  ( 0.000000000000000000, 115.4999999999999574, 0.000000000000000000 ) ) ;
#68481 = CIRCLE ( 'NONE', #61716, 9.999999999999998224 ) ;
#68482 = FACE_OUTER_BOUND ( 'NONE', #22793, .T. ) ;
#68483 = DIRECTION ( 'NONE',  ( -0.000000000000000000, -0.000000000000000000, -1.000000000000000000 ) ) ;
#68484 = VERTEX_POINT ( 'NONE', #12540 ) ;
#68485 =( GEOMETRIC_REPRESENTATION_CONTEXT ( 3 ) GLOBAL_UNCERTAINTY_ASSIGNED_CONTEXT ( ( #47557 ) ) GLOBAL_UNIT_ASSIGNED_CONTEXT ( ( #60289, #33219, #43804 ) ) REPRESENTATION_CONTEXT ( 'NONE', 'WORKASPACE' ) );
#68486 = ORIENTED_EDGE ( 'NONE', *, *, #45328, .T. ) ;
#68487 = AXIS2_PLACEMENT_3D ( 'NONE', #9318, #41343, #9677 ) ;
#68489 =( GEOMETRIC_REPRESENTATION_CONTEXT ( 3 ) GLOBAL_UNCERTAINTY_ASSIGNED_CONTEXT ( ( #21537 ) ) GLOBAL_UNIT_ASSIGNED_CONTEXT ( ( #31389, #37080, #69399 ) ) REPRESENTATION_CONTEXT ( 'NONE', 'WORKASPACE' ) );
#68488 = LINE ( 'NONE', #36522, #34949 ) ;
#68490 = CIRCLE ( 'NONE', #41552, 0.2500000000000002220 ) ;
#68492 = CARTESIAN_POINT ( 'NONE',  ( -20.03861782943699765, 115.4999999895429994, 10.00000000000000000 ) ) ;
#68491 = AXIS2_PLACEMENT_3D ( 'NONE', #5015, #58489, #21184 ) ;
#68493 = FACE_OUTER_BOUND ( 'NONE', #36519, .T. ) ;
#68494 = COLOUR_RGB ( '', 0.09019608, 0.27058824, 0.51372549) ;
#68495 = CARTESIAN_POINT ( 'NONE',  ( -76.70707362346617231, -3.094860106618431139, -9.524999999999991473 ) ) ;
#68496 = ORIENTED_EDGE ( 'NONE', *, *, #24435, .T. ) ;
#68497 = ORIENTED_EDGE ( 'NONE', *, *, #56720, .T. ) ;
#68498 = FACE_OUTER_BOUND ( 'NONE', #29666, .T. ) ;
#68499 = DIRECTION ( 'NONE',  ( -0.8660254037844385966, 0.5000000000000002220, 0.000000000000000000 ) ) ;
#68500 = CYLINDRICAL_SURFACE ( 'NONE', #38394, 0.5000000000000004441 ) ;
#68501 = VERTEX_POINT ( 'NONE', #60721 ) ;
#68502 = CARTESIAN_POINT ( 'NONE',  ( 10.01517768586949231, 115.8049999999999784, 1.839758294383810543E-15 ) ) ;
#68503 = SURFACE_SIDE_STYLE ('',( #58981 ) ) ;
#68504 = DIRECTION ( 'NONE',  ( -0.000000000000000000, -0.000000000000000000, -1.000000000000000000 ) ) ;
#68505 = CARTESIAN_POINT ( 'NONE',  ( -104.0949999999999989, -2.607480562269071545, -8.024999999999991473 ) ) ;
#68506 = ORIENTED_EDGE ( 'NONE', *, *, #48826, .T. ) ;
#68507 = PRESENTATION_LAYER_ASSIGNMENT (  '', '', ( #29158 ) ) ;
#68508 = CARTESIAN_POINT ( 'NONE',  ( -9.384346074379580571, 110.5000000000000000, 1.688215766215464653 ) ) ;
#68509 = CARTESIAN_POINT ( 'NONE',  ( -164.7570736234661695, -5.598654528085801552, 7.705886871421367523 ) ) ;
#68510 = PLANE ( 'NONE',  #24998 ) ;
#68511 = EDGE_LOOP ( 'NONE', ( #6161, #27361, #37671 ) ) ;
#68512 = CARTESIAN_POINT ( 'NONE',  ( 4.716976649647096842, 151.7429263765338021, 6.492361379858953896 ) ) ;
#68513 = FILL_AREA_STYLE ('',( #61813 ) ) ;
#68514 = ORIENTED_EDGE ( 'NONE', *, *, #39438, .F. ) ;
#68515 = CARTESIAN_POINT ( 'NONE',  ( -61.70707362346615810, -3.094860106618431139, -9.524999999999991473 ) ) ;
#68516 = ORIENTED_EDGE ( 'NONE', *, *, #28974, .T. ) ;
#68517 = CYLINDRICAL_SURFACE ( 'NONE', #27087, 4.999999999999997335 ) ;
#68518 =( LENGTH_UNIT ( ) NAMED_UNIT ( * ) SI_UNIT ( .MILLI., .METRE. ) );
#68519 = CARTESIAN_POINT ( 'NONE',  ( -32.58324634911704720, -8.999709270181572407, 4.695517540643423082 ) ) ;
#68520 = CARTESIAN_POINT ( 'NONE',  ( -119.7549999999999812, 4.716976649647091513, -6.492361379858946790 ) ) ;
#68521 = CIRCLE ( 'NONE', #20197, 0.2500000000000002220 ) ;
#68522 = CARTESIAN_POINT ( 'NONE',  ( 7.632228543268607446, 141.1570736234661751, 2.479861379858954606 ) ) ;
#68523 = DIRECTION ( 'NONE',  ( -1.000000000000000000, -0.000000000000000000, -0.000000000000000000 ) ) ;
#68524 = VECTOR ( 'NONE', #62641, 1000.000000000000000 ) ;
#68525 = CARTESIAN_POINT ( 'NONE',  ( -69.99999999999998579, 50.00000000000000000, 11.50000000000003730 ) ) ;
#68526 = FACE_OUTER_BOUND ( 'NONE', #16635, .T. ) ;
#68527 =( NAMED_UNIT ( * ) PLANE_ANGLE_UNIT ( ) SI_UNIT ( $, .RADIAN. ) );
#68528 = DIRECTION ( 'NONE',  ( 0.000000000000000000, -1.000000000000000000, 0.000000000000000000 ) ) ;
#68529 = VERTEX_POINT ( 'NONE', #22414 ) ;
#68530 = ORIENTED_EDGE ( 'NONE', *, *, #7326, .F. ) ;
#68531 = CARTESIAN_POINT ( 'NONE',  ( 12.25000000000000355, 30.74999999999998579, 3.750000000000000000 ) ) ;
#68532 = DIRECTION ( 'NONE',  ( 0.000000000000000000, 0.000000000000000000, 1.000000000000000000 ) ) ;
#68533 = CARTESIAN_POINT ( 'NONE',  ( -183.0000000000000000, 7.623482428031956637, -5.710353812986356026 ) ) ;
#68534 = VERTEX_POINT ( 'NONE', #38646 ) ;
#68535 = FILL_AREA_STYLE ('',( #31572 ) ) ;
#68536 = CARTESIAN_POINT ( 'NONE',  ( -183.6549999999999727, -7.632228543268600340, -2.479861379858950166 ) ) ;
#68537 = CARTESIAN_POINT ( 'NONE',  ( 3.999798566743339556, 49.09558629977726696, 2.000000000000000000 ) ) ;
#68538 = DIRECTION ( 'NONE',  ( -1.000000000000000000, 0.000000000000000000, 0.000000000000000000 ) ) ;
#68539 = EDGE_CURVE ( 'NONE', #11684, #24423, #51588, .T. ) ;
#68540 = CARTESIAN_POINT ( 'NONE',  ( -182.8449999999999989, -7.632228543268599452, 2.479861379858951054 ) ) ;
#68541 = COLOUR_RGB ( '', 0.66274510, 0.83137255, 0.94901961) ;
#68542 = CARTESIAN_POINT ( 'NONE',  ( -173.6949999999999648, -8.437984349512086979, 5.166775262442717831E-16 ) ) ;
#68543 = VECTOR ( 'NONE', #14072, 1000.000000000000000 ) ;
#68544 = ORIENTED_EDGE ( 'NONE', *, *, #16734, .F. ) ;
#68545 = CARTESIAN_POINT ( 'NONE',  ( 4.750000000000002665, 24.74999999999998579, -4.000000000000000000 ) ) ;
#68546 = VECTOR ( 'NONE', #66924, 1000.000000000000000 ) ;
#68547 = CARTESIAN_POINT ( 'NONE',  ( -13.37648924254744642, 11.02484219126050391, -4.740415575798497372 ) ) ;
#68548 = CARTESIAN_POINT ( 'NONE',  ( -97.10499999999998977, -6.826472737025115478, 4.959722759717900331 ) ) ;
#68549 = AXIS2_PLACEMENT_3D ( 'NONE', #38593, #59988, #11800 ) ;
#68550 = EDGE_CURVE ( 'NONE', #19233, #69035, #50205, .T. ) ;
#68551 = ADVANCED_FACE ( 'NONE', ( #44616 ), #68410, .F. ) ;
#68552 = CARTESIAN_POINT ( 'NONE',  ( -95.24499999999997613, -4.716976649647093289, -6.492361379858945902 ) ) ;
#68553 = CARTESIAN_POINT ( 'NONE',  ( 9.058813317711338797, 130.9549999999999841, -2.943386871421372675 ) ) ;
#68554 = CARTESIAN_POINT ( 'NONE',  ( -71.54499999999998749, -7.632228543268600340, -2.479861379858950166 ) ) ;
#68555 = EDGE_CURVE ( 'NONE', #37991, #61027, #23800, .T. ) ;
#68556 = CARTESIAN_POINT ( 'NONE',  ( -75.00000000000001421, 9.708372675170622301, -6.100541755698617230 ) ) ;
#68557 = STYLED_ITEM ( 'NONE', ( #38387 ), #17664 ) ;
#68558 = B_SPLINE_CURVE_WITH_KNOTS ( 'NONE', 3,
 ( #19894, #9729, #31136, #36819 ),
 .UNSPECIFIED., .F., .F.,
 ( 4, 4 ),
 ( 0.000000000000000000, 0.0004221139024916740600 ),
 .UNSPECIFIED. ) ;
#68559 = MECHANICAL_DESIGN_GEOMETRIC_PRESENTATION_REPRESENTATION (  '', ( #46139 ), #47256 ) ;
#68560 = EDGE_CURVE ( 'NONE', #65490, #24108, #36147, .T. ) ;
#68561 = CARTESIAN_POINT ( 'NONE',  ( 68.00000000000000000, 2.776762340297169183E-15, -11.50000000000000000 ) ) ;
#68562 = UNCERTAINTY_MEASURE_WITH_UNIT (LENGTH_MEASURE( 1.000000000000000082E-05 ), #51975, 'distance_accuracy_value', 'NONE');
#68563 = AXIS2_PLACEMENT_3D ( 'NONE', #49973, #39779, #39430 ) ;
#68564 = SURFACE_SIDE_STYLE ('',( #25621 ) ) ;
#68565 = VERTEX_POINT ( 'NONE', #36111 ) ;
#68566 = ADVANCED_FACE ( 'NONE', ( #62116 ), #6682, .T. ) ;
#68567 = CARTESIAN_POINT ( 'NONE',  ( -100.3429263765337964, -9.058813317711329915, 2.943386871421371787 ) ) ;
#68568 = CARTESIAN_POINT ( 'NONE',  ( -128.8449999999999989, -7.632228543268599452, 2.479861379858951054 ) ) ;
#68570 = FACE_OUTER_BOUND ( 'NONE', #41216, .T. ) ;
#68569 = CARTESIAN_POINT ( 'NONE',  ( -132.2929263765344672, 3.094860106607336903, -9.525000000008052581 ) ) ;
#68571 = SURFACE_STYLE_USAGE ( .BOTH. , #4159 ) ;
#68572 = EDGE_LOOP ( 'NONE', ( #51790, #45490, #65673, #16899, #59941, #7826 ) ) ;
#68573 = ORIENTED_EDGE ( 'NONE', *, *, #23832, .F. ) ;
#68574 =( NAMED_UNIT ( * ) PLANE_ANGLE_UNIT ( ) SI_UNIT ( $, .RADIAN. ) );
#68575 = CIRCLE ( 'NONE', #13517, 1.000000000000000000 ) ;
#68576 = CARTESIAN_POINT ( 'NONE',  ( -134.3929263765338078, 8.102448949553176405, 5.886773742842740909 ) ) ;
#68577 = UNCERTAINTY_MEASURE_WITH_UNIT (LENGTH_MEASURE( 1.000000000000000082E-05 ), #15638, 'distance_accuracy_value', 'NONE');
#68578 = VECTOR ( 'NONE', #57063, 1000.000000000000000 ) ;
#68579 = CARTESIAN_POINT ( 'NONE',  ( -97.85707362346616378, -5.598654528085803328, -7.705886871421366635 ) ) ;
#68580 = CARTESIAN_POINT ( 'NONE',  ( -57.99999999999997868, 50.00000000000000000, -6.500000000000000000 ) ) ;
#68581 = DIRECTION ( 'NONE',  ( -0.000000000000000000, 1.000000000000000000, -0.000000000000000000 ) ) ;
#68582 = EDGE_LOOP ( 'NONE', ( #49993, #67806, #49825, #44659 ) ) ;
#68583 = CARTESIAN_POINT ( 'NONE',  ( -126.5049999999999528, -6.826472737025113702, -4.959722759717900331 ) ) ;
#68584 = ORIENTED_EDGE ( 'NONE', *, *, #67824, .T. ) ;
#68585 = CARTESIAN_POINT ( 'NONE',  ( -126.6570736234661751, 9.058813317711329915, 2.943386871421369566 ) ) ;
#68586 = ORIENTED_EDGE ( 'NONE', *, *, #12783, .T. ) ;
#68587 = SURFACE_SIDE_STYLE ('',( #15487 ) ) ;
#68588 = VERTEX_POINT ( 'NONE', #13943 ) ;
#68589 = PRESENTATION_LAYER_ASSIGNMENT (  '', '', ( #29245 ) ) ;
#68590 = VECTOR ( 'NONE', #21362, 1000.000000000000000 ) ;
#68591 = LINE ( 'NONE', #67541, #2811 ) ;
#68592 = CIRCLE ( 'NONE', #52888, 12.50000000000001066 ) ;
#68593 = CARTESIAN_POINT ( 'NONE',  ( -5.598654528085808657, 146.6450000000000102, 7.705886871421373741 ) ) ;
#68594 = VERTEX_POINT ( 'NONE', #26881 ) ;
#68595 = DIRECTION ( 'NONE',  ( -1.000000000000000000, 0.000000000000000000, 0.000000000000000000 ) ) ;
#68596 = CARTESIAN_POINT ( 'NONE',  ( -8.102448949553179958, 150.0049999999999386, -5.886773742842749790 ) ) ;
#68597 = FILL_AREA_STYLE ('',( #69615 ) ) ;
#68598 = VECTOR ( 'NONE', #51596, 1000.000000000000000 ) ;
#68599 = DIRECTION ( 'NONE',  ( -0.000000000000000000, -0.000000000000000000, 1.000000000000000000 ) ) ;
#68600 = ORIENTED_EDGE ( 'NONE', *, *, #22984, .F. ) ;
#68601 = CARTESIAN_POINT ( 'NONE',  ( 8.437984349512095861, 128.1929263765338192, 1.550032578732817026E-15 ) ) ;
#68602 = CARTESIAN_POINT ( 'NONE',  ( 45.65811388300841855, 10.21937129433612057, -3.598410089384286081 ) ) ;
#68603 = UNCERTAINTY_MEASURE_WITH_UNIT (LENGTH_MEASURE( 1.000000000000000082E-05 ), #56852, 'distance_accuracy_value', 'NONE');
#68604 = CARTESIAN_POINT ( 'NONE',  ( -47.15707362346616094, -9.058813317711329915, -2.943386871421370898 ) ) ;
#68605 = CARTESIAN_POINT ( 'NONE',  ( 43.75000000000000000, 18.74999999999998224, 4.000000000000000000 ) ) ;
#68606 = CARTESIAN_POINT ( 'NONE',  ( 0.000000000000000000, 127.0570736234661666, -8.025000000000000355 ) ) ;
#68607 = ORIENTED_EDGE ( 'NONE', *, *, #48879, .T. ) ;
#68608 = CIRCLE ( 'NONE', #47308, 9.999999999999998224 ) ;
#68609 = CARTESIAN_POINT ( 'NONE',  ( 0.000000000000000000, 0.000000000000000000, 12.50000000000000000 ) ) ;
#68610 = VERTEX_POINT ( 'NONE', #37176 ) ;
#68611 = CARTESIAN_POINT ( 'NONE',  ( -58.94292637653381206, 0.000000000000000000, 9.524999999999991473 ) ) ;
#68612 = DIRECTION ( 'NONE',  ( 1.000000000000000000, 0.000000000000000000, 0.000000000000000000 ) ) ;
#68613 = CARTESIAN_POINT ( 'NONE',  ( -148.2549999999999955, -4.716976649647092401, 6.492361379858946790 ) ) ;
#68614 = ORIENTED_EDGE ( 'NONE', *, *, #2107, .F. ) ;
#68615 = DIRECTION ( 'NONE',  ( -0.000000000000000000, -0.000000000000000000, -1.000000000000000000 ) ) ;
#68616 = UNCERTAINTY_MEASURE_WITH_UNIT (LENGTH_MEASURE( 1.000000000000000082E-05 ), #51543, 'distance_accuracy_value', 'NONE');
#68617 = AXIS2_PLACEMENT_3D ( 'NONE', #52049, #19309, #3806 ) ;
#68618 = AXIS2_PLACEMENT_3D ( 'NONE', #63868, #47770, #54009 ) ;
#68619 = CARTESIAN_POINT ( 'NONE',  ( 57.74999999999998579, 30.74999999999999289, 4.000000000000000000 ) ) ;
#68620 = CARTESIAN_POINT ( 'NONE',  ( -55.16874038549254067, -8.628515624790349392, 6.699332285580846147 ) ) ;
#68621 = CARTESIAN_POINT ( 'NONE',  ( -71.50000000000000000, 14.49137674618942562, -7.500000000000000000 ) ) ;
#68622 = ORIENTED_EDGE ( 'NONE', *, *, #32750, .T. ) ;
#68623 = ORIENTED_EDGE ( 'NONE', *, *, #24557, .F. ) ;
#68624 = CARTESIAN_POINT ( 'NONE',  ( -195.0000000000000000, 0.000000000000000000, 0.000000000000000000 ) ) ;
#68625 = DIRECTION ( 'NONE',  ( -1.000000000000000000, 0.000000000000000000, 0.000000000000000000 ) ) ;
#68626 = CARTESIAN_POINT ( 'NONE',  ( -70.10499999999998977, -6.826472737025115478, 4.959722759717900331 ) ) ;
#68627 = ORIENTED_EDGE ( 'NONE', *, *, #30321, .F. ) ;
#68628 = CYLINDRICAL_SURFACE ( 'NONE', #61770, 5.000000000000000000 ) ;
#68629 = EDGE_CURVE ( 'NONE', #51066, #19343, #15371, .T. ) ;
#68630 = CARTESIAN_POINT ( 'NONE',  ( -90.95707362346617231, 9.058813317711329915, -2.943386871421373119 ) ) ;
#68631 = FACE_OUTER_BOUND ( 'NONE', #4981, .T. ) ;
#68633 = EDGE_CURVE ( 'NONE', #53241, #14677, #20608, .T. ) ;
#68632 = EDGE_LOOP ( 'NONE', ( #1734, #46154, #44973, #16288 ) ) ;
#68634 = CARTESIAN_POINT ( 'NONE',  ( -74.08452722211991670, 9.430195805462506797, -6.024500123752368985 ) ) ;
#68635 = DIRECTION ( 'NONE',  ( -1.000000000000000000, 0.000000000000000000, 0.000000000000000000 ) ) ;
#68636 = DIRECTION ( 'NONE',  ( 0.000000000000000000, 0.000000000000000000, -1.000000000000000000 ) ) ;
#68637 = CARTESIAN_POINT ( 'NONE',  ( 8.082903768654762899, -1.105959442090949618E-15, 7.500000000000000000 ) ) ;
#68638 = AXIS2_PLACEMENT_3D ( 'NONE', #49877, #44631, #64983 ) ;
#68639 = CARTESIAN_POINT ( 'NONE',  ( 0.000000000000000000, 145.4449999999999932, -9.525000000000000355 ) ) ;
#68640 = CARTESIAN_POINT ( 'NONE',  ( -92.54499999999998749, -7.632228543268600340, -2.479861379858950166 ) ) ;
#68641 = CIRCLE ( 'NONE', #14762, 0.5000000000000004441 ) ;
#68642 = ADVANCED_FACE ( 'NONE', ( #58584 ), #64199, .T. ) ;
#68643 = SURFACE_SIDE_STYLE ('',( #37015 ) ) ;
#68644 = CARTESIAN_POINT ( 'NONE',  ( 10.00000000000001954, 42.00000000000000000, -28.38386403503541899 ) ) ;
#68645 = STYLED_ITEM ( 'NONE', ( #28840 ), #34733 ) ;
#68646 = UNCERTAINTY_MEASURE_WITH_UNIT (LENGTH_MEASURE( 1.000000000000000082E-05 ), #67084, 'distance_accuracy_value', 'NONE');
#68647 = VECTOR ( 'NONE', #52651, 1000.000000000000000 ) ;
#68648 = CARTESIAN_POINT ( 'NONE',  ( -41.45361433042954502, 107.0152407614178713, -3.500000000000000888 ) ) ;
#68649 = ORIENTED_EDGE ( 'NONE', *, *, #32300, .F. ) ;
#68650 = EDGE_CURVE ( 'NONE', #23421, #49208, #16842, .T. ) ;
#68651 = CARTESIAN_POINT ( 'NONE',  ( -133.4929263765338021, -8.102448949553172852, 5.886773742842742685 ) ) ;
#68652 =( LENGTH_UNIT ( ) NAMED_UNIT ( * ) SI_UNIT ( .MILLI., .METRE. ) );
#68653 = CARTESIAN_POINT ( 'NONE',  ( -34.31243252642735087, -10.02680648607962510, -3.499999999999997335 ) ) ;
#68654 = CARTESIAN_POINT ( 'NONE',  ( -160.1950000000000216, 8.437984349512085203, -1.550032578732815448E-15 ) ) ;
#68656 = FILL_AREA_STYLE_COLOUR ( '', #45970 ) ;
#68655 = VECTOR ( 'NONE', #56348, 1000.000000000000000 ) ;
#68657 = CARTESIAN_POINT ( 'NONE',  ( 71.49999999999998579, 64.07124727947029896, 7.500000000000000000 ) ) ;
#68658 = MECHANICAL_DESIGN_GEOMETRIC_PRESENTATION_REPRESENTATION (  '', ( #32677 ), #16999 ) ;
#68659 = ORIENTED_EDGE ( 'NONE', *, *, #36100, .F. ) ;
#68660 = EDGE_LOOP ( 'NONE', ( #9194, #47521 ) ) ;
#68661 = MECHANICAL_DESIGN_GEOMETRIC_PRESENTATION_REPRESENTATION (  '', ( #11348 ), #13549 ) ;
#68662 = DIRECTION ( 'NONE',  ( -0.000000000000000000, 1.000000000000000000, -0.000000000000000000 ) ) ;
#68663 = UNCERTAINTY_MEASURE_WITH_UNIT (LENGTH_MEASURE( 1.000000000000000082E-05 ), #12972, 'distance_accuracy_value', 'NONE');
#68664 = ORIENTED_EDGE ( 'NONE', *, *, #56059, .T. ) ;
#68665 = CYLINDRICAL_SURFACE ( 'NONE', #58543, 0.2500000000000002220 ) ;
#68666 = CARTESIAN_POINT ( 'NONE',  ( -45.00000000000000000, 8.189963308881127446, 5.659193869480894534 ) ) ;
#68667 = CARTESIAN_POINT ( 'NONE',  ( -110.9070736234670846, -3.094860106603640304, 9.525000000010738432 ) ) ;
#68668 = COLOUR_RGB ( '', 0.09019608, 0.27058824, 0.51372549) ;
#68669 = CARTESIAN_POINT ( 'NONE',  ( -58.54039790200148730, -8.499999999999465317, -0.1927383919051781080 ) ) ;
#68670 = ORIENTED_EDGE ( 'NONE', *, *, #14038, .F. ) ;
#68671 = CARTESIAN_POINT ( 'NONE',  ( -148.5550000000000068, 0.000000000000000000, 8.024999999999991473 ) ) ;
#68672 = ORIENTED_EDGE ( 'NONE', *, *, #33871, .T. ) ;
#68673 = CARTESIAN_POINT ( 'NONE',  ( -22.50000000000000711, 34.24999999999999289, -4.000000000000000000 ) ) ;
#68674 = VERTEX_POINT ( 'NONE', #4394 ) ;
#68675 = CARTESIAN_POINT ( 'NONE',  ( 15.98999599679679839, 146.9999999999999716, -10.00000000000000000 ) ) ;
#68676 = LINE ( 'NONE', #20107, #14052 ) ;
#68677 = CARTESIAN_POINT ( 'NONE',  ( -9.058813317711338797, 122.3449999999999847, 2.943386871421373563 ) ) ;
#68678 = CARTESIAN_POINT ( 'NONE',  ( 0.3542414993972742288, 42.77450856510288446, -74.52798351431924573 ) ) ;
#68679 = EDGE_CURVE ( 'NONE', #22515, #30516, #31168, .T. ) ;
#68680 = EDGE_LOOP ( 'NONE', ( #14439, #21645, #42928, #61283 ) ) ;
#68681 =( GEOMETRIC_REPRESENTATION_CONTEXT ( 3 ) GLOBAL_UNCERTAINTY_ASSIGNED_CONTEXT ( ( #22010 ) ) GLOBAL_UNIT_ASSIGNED_CONTEXT ( ( #38946, #66320, #49470 ) ) REPRESENTATION_CONTEXT ( 'NONE', 'WORKASPACE' ) );
#68682 = CARTESIAN_POINT ( 'NONE',  ( 0.000000000000000000, 116.5549999999999926, -9.525000000000000355 ) ) ;
#68683 = CARTESIAN_POINT ( 'NONE',  ( -65.75499999999998124, 4.716976649647091513, -6.492361379858946790 ) ) ;
#68684 = CYLINDRICAL_SURFACE ( 'NONE', #62139, 5.000000000000000000 ) ;
#68685 = PRODUCT_DEFINITION_SHAPE ( 'NONE', 'NONE',  #52435 ) ;
#68686 =( BOUNDED_CURVE ( )  B_SPLINE_CURVE ( 2, ( #22248, #69070, #20874, #32116, #63763, #42716, #37088, #64114, #5027, #15968, #58848 ),
 .UNSPECIFIED., .F., .F. ) 
 B_SPLINE_CURVE_WITH_KNOTS ( ( 3, 2, 2, 2, 2, 3 ),
 ( 0.7500000000000000000, 0.7521739130434782483, 0.7543478260869564966, 0.7565217391304347450, 0.7586956521739129933, 0.7608695652173913526 ),
 .UNSPECIFIED. ) 
 CURVE ( )  GEOMETRIC_REPRESENTATION_ITEM ( )  RATIONAL_B_SPLINE_CURVE ( ( 1.000000000000000000, 0.9510565162951535312, 1.000000000000000000, 0.9510565162951535312, 1.000000000000000000, 0.9510565162951535312, 1.000000000000000000, 0.9510565162951535312, 1.000000000000000000, 0.9510565162951535312, 1.000000000000000000 ) ) 
 REPRESENTATION_ITEM ( '' )  );
#68687 = EDGE_LOOP ( 'NONE', ( #61395, #22589, #54650, #51476 ) ) ;
#68688 = CARTESIAN_POINT ( 'NONE',  ( -1.166476076187854022E-15, 148.0549999999999784, 9.525000000000000355 ) ) ;
#68689 = UNCERTAINTY_MEASURE_WITH_UNIT (LENGTH_MEASURE( 1.000000000000000082E-05 ), #14834, 'distance_accuracy_value', 'NONE');
#68690 = CARTESIAN_POINT ( 'NONE',  ( 98.00000000000000000, 16.00000000000000000, -5.000000000000004441 ) ) ;
#68691 = CARTESIAN_POINT ( 'NONE',  ( -14.98999599679679662, 118.4999999999999716, -9.500000000000000000 ) ) ;
#68692 =( GEOMETRIC_REPRESENTATION_CONTEXT ( 3 ) GLOBAL_UNCERTAINTY_ASSIGNED_CONTEXT ( ( #16014 ) ) GLOBAL_UNIT_ASSIGNED_CONTEXT ( ( #7411, #995, #38425 ) ) REPRESENTATION_CONTEXT ( 'NONE', 'WORKASPACE' ) );
#68693 = CARTESIAN_POINT ( 'NONE',  ( -11.24540022918535698, 52.49282396394303873, 2.000000000000000000 ) ) ;
#68694 = ORIENTED_EDGE ( 'NONE', *, *, #5531, .T. ) ;
#68695 = DIRECTION ( 'NONE',  ( -1.000000000000000000, 0.000000000000000000, -0.000000000000000000 ) ) ;
#68696 = CARTESIAN_POINT ( 'NONE',  ( 74.50000000000000000, 19.30628705663858113, -6.500000000000000000 ) ) ;
#68697 = DIRECTION ( 'NONE',  ( 1.000000000000000000, -0.000000000000000000, -0.000000000000000000 ) ) ;
#68698 = CARTESIAN_POINT ( 'NONE',  ( -178.2549999999999955, -4.716976649647092401, 6.492361379858946790 ) ) ;
#68700 = ORIENTED_EDGE ( 'NONE', *, *, #51619, .T. ) ;
#68699 = CIRCLE ( 'NONE', #38407, 0.2500000000000002220 ) ;
#68701 = CARTESIAN_POINT ( 'NONE',  ( 8.586026971066655022, 111.4549650702766570, -0.1239747060112400823 ) ) ;
#68702 = PRESENTATION_LAYER_ASSIGNMENT (  '', '', ( #21483 ) ) ;
#68703 = CARTESIAN_POINT ( 'NONE',  ( 10.39230484541327115, -3.482307324624967703E-15, 1.392304845413258718 ) ) ;
#68704 = ORIENTED_EDGE ( 'NONE', *, *, #278, .F. ) ;
#68705 =( NAMED_UNIT ( * ) SI_UNIT ( $, .STERADIAN. ) SOLID_ANGLE_UNIT ( ) );
#68706 = CARTESIAN_POINT ( 'NONE',  ( -15.98999599679679839, 146.4999999999999716, 10.00000000000000000 ) ) ;
#68707 = PRESENTATION_LAYER_ASSIGNMENT (  '', '', ( #9206 ) ) ;
#68708 = VERTEX_POINT ( 'NONE', #63849 ) ;
#68709 = CARTESIAN_POINT ( 'NONE',  ( 0.000000000000000000, -2.500000000000000000, 0.000000000000000000 ) ) ;
#68710 = EDGE_CURVE ( 'NONE', #31245, #7454, #986, .T. ) ;
#68711 =( LENGTH_UNIT ( ) NAMED_UNIT ( * ) SI_UNIT ( .MILLI., .METRE. ) );
#68712 = CARTESIAN_POINT ( 'NONE',  ( -99.35499999999998977, -4.716976649647093289, -6.492361379858945902 ) ) ;
#68713 = ORIENTED_EDGE ( 'NONE', *, *, #37933, .T. ) ;
#68714 = ADVANCED_FACE ( 'NONE', ( #37535 ), #58941, .T. ) ;
#68715 = DIRECTION ( 'NONE',  ( 1.000000000000000000, 0.000000000000000000, -0.000000000000000000 ) ) ;
#68716 = CIRCLE ( 'NONE', #19257, 1.000000000000000888 ) ;
#68717 = SURFACE_SIDE_STYLE ('',( #37789 ) ) ;
#68718 = CARTESIAN_POINT ( 'NONE',  ( -135.2070736234661865, 3.094860106618433360, 9.524999999999991473 ) ) ;
#68719 = AXIS2_PLACEMENT_3D ( 'NONE', #66663, #39960, #61364 ) ;
#68720 = CARTESIAN_POINT ( 'NONE',  ( -5.598654528085808657, 152.6449999999999818, 7.705886871421373741 ) ) ;
#68721 = CARTESIAN_POINT ( 'NONE',  ( -72.20707362346617231, 3.094860106618433360, 9.524999999999991473 ) ) ;
#68722 = AXIS2_PLACEMENT_3D ( 'NONE', #60450, #34079, #18610 ) ;
#68723 = ADVANCED_FACE ( 'NONE', ( #58241 ), #36826, .F. ) ;
#68724 = CARTESIAN_POINT ( 'NONE',  ( -91.94292637653380496, 0.000000000000000000, 9.524999999999991473 ) ) ;
#68725 = ORIENTED_EDGE ( 'NONE', *, *, #44458, .F. ) ;
#68726 = FACE_OUTER_BOUND ( 'NONE', #10869, .T. ) ;
#68727 = CARTESIAN_POINT ( 'NONE',  ( -15.65791276157354694, -10.92369435878044293, -4.967701894473437463 ) ) ;
#68728 =( GEOMETRIC_REPRESENTATION_CONTEXT ( 3 ) GLOBAL_UNCERTAINTY_ASSIGNED_CONTEXT ( ( #39899 ) ) GLOBAL_UNIT_ASSIGNED_CONTEXT ( ( #279, #53478, #10567 ) ) REPRESENTATION_CONTEXT ( 'NONE', 'WORKASPACE' ) );
#68729 = PRESENTATION_STYLE_ASSIGNMENT (( #47301 ) ) ;
#68730 = CARTESIAN_POINT ( 'NONE',  ( -112.4050000000000011, -2.607480562269069768, 8.024999999999991473 ) ) ;
#68731 = CARTESIAN_POINT ( 'NONE',  ( -11.99999999999999822, -8.499999999999998224, 3.000000000000000000 ) ) ;
#68732 = CARTESIAN_POINT ( 'NONE',  ( -8.102448949553181734, 118.8949999999999676, -5.886773742842749790 ) ) ;
#68733 = CARTESIAN_POINT ( 'NONE',  ( -130.6449999999999818, 4.716976649647091513, -6.492361379858946790 ) ) ;
#68734 = EDGE_CURVE ( 'NONE', #21323, #17133, #59251, .T. ) ;
#68735 = AXIS2_PLACEMENT_3D ( 'NONE', #35862, #58027, #14765 ) ;
#68736 = CARTESIAN_POINT ( 'NONE',  ( -111.9570736234661723, 9.058813317711329915, -2.943386871421373119 ) ) ;
#68737 = CARTESIAN_POINT ( 'NONE',  ( -118.6429263765337936, -5.598654528085801552, 7.705886871421367523 ) ) ;
#68738 = CIRCLE ( 'NONE', #39519, 1.000000000000000888 ) ;
#68739 = ORIENTED_EDGE ( 'NONE', *, *, #67909, .T. ) ;
#68740 = AXIS2_PLACEMENT_3D ( 'NONE', #3615, #14935, #64397 ) ;
#68741 = ADVANCED_FACE ( 'NONE', ( #26218 ), #47386, .T. ) ;
#68742 = CARTESIAN_POINT ( 'NONE',  ( -162.2929263765337851, 3.094860106618428031, -9.524999999999993250 ) ) ;
#68743 = CARTESIAN_POINT ( 'NONE',  ( -183.4449999999999932, 0.000000000000000000, 8.024999999999991473 ) ) ;
#68744 = AXIS2_PLACEMENT_3D ( 'NONE', #21002, #5153, #22738 ) ;
#68745 = CARTESIAN_POINT ( 'NONE',  ( 0.000000000000000000, 124.0570736234661524, -8.025000000000000355 ) ) ;
#68746 = AXIS2_PLACEMENT_3D ( 'NONE', #4164, #25636, #21405 ) ;
#68747 = CARTESIAN_POINT ( 'NONE',  ( -195.0000000000000000, 1.166476076187852838E-15, -9.524999999999991473 ) ) ;
#68748 = DIRECTION ( 'NONE',  ( -7.816271194327172234E-17, 0.000000000000000000, -1.000000000000000000 ) ) ;
#68749 = CARTESIAN_POINT ( 'NONE',  ( 52.99999999999999289, 27.74999999999998579, 4.000000000000000000 ) ) ;
#68750 = ORIENTED_EDGE ( 'NONE', *, *, #24897, .F. ) ;
#68751 = CARTESIAN_POINT ( 'NONE',  ( -79.34292637653379643, -9.058813317711329915, 2.943386871421371787 ) ) ;
#68752 = DIRECTION ( 'NONE',  ( -1.000000000000000000, -0.000000000000000000, -0.000000000000000000 ) ) ;
#68753 = DIRECTION ( 'NONE',  ( 0.000000000000000000, 0.000000000000000000, -1.000000000000000000 ) ) ;
#68754 = VECTOR ( 'NONE', #55948, 1000.000000000000000 ) ;
#68755 = CARTESIAN_POINT ( 'NONE',  ( 7.632228543268607446, 152.0429263765338135, 2.479861379858954606 ) ) ;
#68756 = CARTESIAN_POINT ( 'NONE',  ( 4.716976649647096842, 146.8570736234661638, 6.492361379858953896 ) ) ;
#68757 = CARTESIAN_POINT ( 'NONE',  ( -182.4550000000000125, 7.632228543268599452, -2.479861379858951942 ) ) ;
#68758 = AXIS2_PLACEMENT_3D ( 'NONE', #12800, #3238, #23706 ) ;
#68759 = EDGE_LOOP ( 'NONE', ( #39738, #55277, #29304, #56394 ) ) ;
#68760 = VECTOR ( 'NONE', #48586, 1000.000000000000000 ) ;
#68761 = FILL_AREA_STYLE ('',( #21588 ) ) ;
#68762 =( NAMED_UNIT ( * ) PLANE_ANGLE_UNIT ( ) SI_UNIT ( $, .RADIAN. ) );
#68763 = CARTESIAN_POINT ( 'NONE',  ( 22.00000000000000711, 50.00000000000000000, -59.99999999999999289 ) ) ;
#68764 = VERTEX_POINT ( 'NONE', #25868 ) ;
#68765 = CYLINDRICAL_SURFACE ( 'NONE', #10645, 5.000000000000004441 ) ;
#68766 = CARTESIAN_POINT ( 'NONE',  ( -7.632228543268607446, 145.6570736234661751, -2.479861379858953718 ) ) ;
#68767 = EDGE_CURVE ( 'NONE', #37491, #7436, #37075, .T. ) ;
#68768 = ORIENTED_EDGE ( 'NONE', *, *, #41149, .F. ) ;
#68769 = DIRECTION ( 'NONE',  ( -0.000000000000000000, -0.000000000000000000, -1.000000000000000000 ) ) ;
#68770 = CARTESIAN_POINT ( 'NONE',  ( -101.7549999999999812, 4.716976649647091513, -6.492361379858946790 ) ) ;
#68771 = UNCERTAINTY_MEASURE_WITH_UNIT (LENGTH_MEASURE( 1.000000000000000082E-05 ), #14219, 'distance_accuracy_value', 'NONE');
#68772 = PRESENTATION_LAYER_ASSIGNMENT (  '', '', ( #11456 ) ) ;
#68773 = CARTESIAN_POINT ( 'NONE',  ( 31.00000000000001421, 42.00000000000000000, 35.50000000000000000 ) ) ;
#68774 = VERTEX_POINT ( 'NONE', #6844 ) ;
#68775 = DIRECTION ( 'NONE',  ( 0.000000000000000000, 1.000000000000000000, -0.000000000000000000 ) ) ;
#68776 = CARTESIAN_POINT ( 'NONE',  ( -9.827790563157511022E-16, 134.5570736234661808, 8.025000000000000355 ) ) ;
#68777 = DIRECTION ( 'NONE',  ( -0.000000000000000000, -1.000000000000000000, -0.000000000000000000 ) ) ;
#68778 = CARTESIAN_POINT ( 'NONE',  ( -33.89861118948982721, -9.947368421052626530, 2.722470280083843619 ) ) ;
#68779 = ORIENTED_EDGE ( 'NONE', *, *, #25967, .T. ) ;
#68780 = CARTESIAN_POINT ( 'NONE',  ( 60.00000000000000000, -2.024042244987997205E-14, -9.500000000000000000 ) ) ;
#68781 = CARTESIAN_POINT ( 'NONE',  ( -73.19499999999999318, 8.437984349512085203, -1.550032578732815448E-15 ) ) ;
#68782 = VERTEX_POINT ( 'NONE', #60310 ) ;
#68783 = CARTESIAN_POINT ( 'NONE',  ( 23.21231517720797655, 118.4999999999999716, -7.500000000000000000 ) ) ;
#68784 =( GEOMETRIC_REPRESENTATION_CONTEXT ( 3 ) GLOBAL_UNCERTAINTY_ASSIGNED_CONTEXT ( ( #30446 ) ) GLOBAL_UNIT_ASSIGNED_CONTEXT ( ( #6040, #16628, #55257 ) ) REPRESENTATION_CONTEXT ( 'NONE', 'WORKASPACE' ) );
#68785 = ADVANCED_FACE ( 'NONE', ( #2187 ), #12455, .F. ) ;
#68786 = CARTESIAN_POINT ( 'NONE',  ( -120.0570736234661808, 0.000000000000000000, 9.524999999999991473 ) ) ;
#68787 = TOROIDAL_SURFACE ( 'NONE', #11464, 0.5000000000000000000, 0.2500000000000000000 ) ;
#68788 = LINE ( 'NONE', #58915, #9465 ) ;
#68789 = ORIENTED_EDGE ( 'NONE', *, *, #7635, .F. ) ;
#68790 = CARTESIAN_POINT ( 'NONE',  ( 0.000000000000000000, -2.500000000000000000, 0.000000000000000000 ) ) ;
#68791 = DIRECTION ( 'NONE',  ( -1.665334536937733825E-15, 0.000000000000000000, -1.000000000000000000 ) ) ;
#68792 = VECTOR ( 'NONE', #53291, 1000.000000000000000 ) ;
#68793 = EDGE_CURVE ( 'NONE', #24621, #4102, #44869, .T. ) ;
#68794 = SURFACE_STYLE_USAGE ( .BOTH. , #42435 ) ;
#68795 = EDGE_LOOP ( 'NONE', ( #11914, #49669, #17497, #20754 ) ) ;
#68796 = EDGE_CURVE ( 'NONE', #13760, #42774, #50459, .T. ) ;
#68797 = AXIS2_PLACEMENT_3D ( 'NONE', #19934, #63209, #42486 ) ;
#68798 = CARTESIAN_POINT ( 'NONE',  ( -7.511572993685801073E-16, 7.000000000000000888, 0.000000000000000000 ) ) ;
#68799 = ORIENTED_EDGE ( 'NONE', *, *, #18459, .F. ) ;
#68800 = DIRECTION ( 'NONE',  ( 1.000000000000000000, -0.000000000000000000, -0.000000000000000000 ) ) ;
#68801 = CARTESIAN_POINT ( 'NONE',  ( 22.00000000000002132, 43.00000000000000000, 75.00000000000000000 ) ) ;
#68802 = SURFACE_SIDE_STYLE ('',( #58227 ) ) ;
#68803 = CARTESIAN_POINT ( 'NONE',  ( -157.5570736234661808, -1.166476076187852838E-15, -9.524999999999991473 ) ) ;
#68804 = CARTESIAN_POINT ( 'NONE',  ( -9.058813317711337021, 122.0449999999999875, -2.943386871421374895 ) ) ;
#68805 = CARTESIAN_POINT ( 'NONE',  ( -99.65707362346617515, 9.058813317711329915, 2.943386871421369566 ) ) ;
#68806 = TOROIDAL_SURFACE ( 'NONE', #21582, 1.000000000000000000, 0.5000000000000000000 ) ;
#68807 = SPHERICAL_SURFACE ( 'NONE', #2575, 0.2500000000000000000 ) ;
#68808 = EDGE_CURVE ( 'NONE', #27703, #57733, #11427, .T. ) ;
#68809 = FACE_OUTER_BOUND ( 'NONE', #38674, .T. ) ;
#68810 = VERTEX_POINT ( 'NONE', #44537 ) ;
#68811 = EDGE_CURVE ( 'NONE', #17063, #19777, #15705, .T. ) ;
#68813 = DIRECTION ( 'NONE',  ( 1.000000000000000000, 0.000000000000000000, -0.000000000000000000 ) ) ;
#68812 = DIRECTION ( 'NONE',  ( -1.000000000000000000, -0.000000000000000000, -0.000000000000000000 ) ) ;
#68814 = DIRECTION ( 'NONE',  ( 1.000000000000000000, 0.000000000000000000, 0.000000000000000000 ) ) ;
#68815 = COLOUR_RGB ( '', 0.40784314, 0.44705882, 0.49803922) ;
#68816 = CARTESIAN_POINT ( 'NONE',  ( -143.1549999999999727, 7.632228543268600340, 2.479861379858949277 ) ) ;
#68817 = CARTESIAN_POINT ( 'NONE',  ( -158.9950000000000045, -6.826472737025115478, 4.959722759717900331 ) ) ;
#68818 = CARTESIAN_POINT ( 'NONE',  ( -142.3449999999999989, 7.632228543268599452, -2.479861379858951942 ) ) ;
#68819 = VERTEX_POINT ( 'NONE', #6157 ) ;
#68820 =( BOUNDED_CURVE ( )  B_SPLINE_CURVE ( 2, ( #36412, #4685, #14929, #63445, #68736, #57829, #20165, #36756, #68045, #68373, #19830 ),
 .UNSPECIFIED., .F., .F. ) 
 B_SPLINE_CURVE_WITH_KNOTS ( ( 3, 2, 2, 2, 2, 3 ),
 ( 0.5108695652173793622, 0.5130434782608576105, 0.5152173913043357478, 0.5173913043478139961, 0.5195652173912921334, 0.5217391304347703818 ),
 .UNSPECIFIED. ) 
 CURVE ( )  GEOMETRIC_REPRESENTATION_ITEM ( )  RATIONAL_B_SPLINE_CURVE ( ( 1.000000000000270006, 0.9510565162948835249, 1.000000000000000000, 0.9510565162951535312, 1.000000000000000000, 0.9510565162951535312, 1.000000000000000000, 0.9510565162951535312, 1.000000000000000000, 0.9510565162954285334, 0.9999999999997249978 ) ) 
 REPRESENTATION_ITEM ( '' )  );
#68821 = CARTESIAN_POINT ( 'NONE',  ( 27.00000000000001776, 14.00000000000000000, -60.00402776293827145 ) ) ;
#68822 = CARTESIAN_POINT ( 'NONE',  ( 0.000000000000000000, 111.9999999999999858, -8.025000000000000355 ) ) ;
#68823 = LINE ( 'NONE', #46713, #23726 ) ;
#68824 = CARTESIAN_POINT ( 'NONE',  ( -50.00499999999998835, 6.826472737025116366, 4.959722759717898555 ) ) ;
#68825 = PRESENTATION_STYLE_ASSIGNMENT (( #21294 ) ) ;
#68826 = AXIS2_PLACEMENT_3D ( 'NONE', #16713, #38178, #765 ) ;
#68827 = CARTESIAN_POINT ( 'NONE',  ( -9.058813317711338797, 156.4549999999999841, 2.943386871421373563 ) ) ;
#68828 = FACE_OUTER_BOUND ( 'NONE', #25044, .T. ) ;
#68829 = CARTESIAN_POINT ( 'NONE',  ( -143.1570736234662036, -9.058813317711329915, -2.943386871421370898 ) ) ;
#68830 = EDGE_CURVE ( 'NONE', #9977, #51271, #17898, .T. ) ;
#68831 = SURFACE_STYLE_USAGE ( .BOTH. , #13006 ) ;
#68832 = AXIS2_PLACEMENT_3D ( 'NONE', #32674, #49925, #33710 ) ;
#68833 = DIRECTION ( 'NONE',  ( -0.000000000000000000, -0.000000000000000000, 1.000000000000000000 ) ) ;
#68834 = PRESENTATION_STYLE_ASSIGNMENT (( #3356 ) ) ;
#68835 = PRESENTATION_LAYER_ASSIGNMENT (  '', '', ( #12665 ) ) ;
#68836 = CYLINDRICAL_SURFACE ( 'NONE', #30442, 0.5000000000000004441 ) ;
#68837 = AXIS2_PLACEMENT_3D ( 'NONE', #6708, #7070, #18329 ) ;
#68838 = FILL_AREA_STYLE_COLOUR ( '', #47678 ) ;
#68839 = CARTESIAN_POINT ( 'NONE',  ( 179.4361977533490347, 13.00000000000000178, 103.7004518695263044 ) ) ;
#68840 = CARTESIAN_POINT ( 'NONE',  ( 74.65811388300841145, 19.88603796100278487, -6.000000000000000000 ) ) ;
#68841 = ORIENTED_EDGE ( 'NONE', *, *, #43019, .F. ) ;
#68842 = ORIENTED_EDGE ( 'NONE', *, *, #1693, .T. ) ;
#68843 = SURFACE_SIDE_STYLE ('',( #47062 ) ) ;
#68844 = VECTOR ( 'NONE', #49318, 1000.000000000000000 ) ;
#68845 = CARTESIAN_POINT ( 'NONE',  ( -6.826472737025120807, 116.1070736234661496, 4.959722759717906548 ) ) ;
#68846 = DIRECTION ( 'NONE',  ( 0.000000000000000000, 0.000000000000000000, -1.000000000000000000 ) ) ;
#68847 = DIRECTION ( 'NONE',  ( 0.000000000000000000, 1.000000000000000000, 0.000000000000000000 ) ) ;
#68848 = VERTEX_POINT ( 'NONE', #55384 ) ;
#68849 = ORIENTED_EDGE ( 'NONE', *, *, #59014, .F. ) ;
#68850 = CIRCLE ( 'NONE', #27231, 0.2500000000000002220 ) ;
#68851 = DIRECTION ( 'NONE',  ( -1.000000000000000000, 0.000000000000000000, 0.000000000000000000 ) ) ;
#68852 = FILL_AREA_STYLE ('',( #15403 ) ) ;
#68853 = STYLED_ITEM ( 'NONE', ( #60545 ), #28952 ) ;
#68854 = CARTESIAN_POINT ( 'NONE',  ( -20.94636006565341191, 149.9999999999999716, 9.500000000000000000 ) ) ;
#68855 = ORIENTED_EDGE ( 'NONE', *, *, #68145, .T. ) ;
#68856 = CARTESIAN_POINT ( 'NONE',  ( -8.102448949553181734, 117.0049999999999670, -5.886773742842749790 ) ) ;
#68857 = DIRECTION ( 'NONE',  ( -1.000000000000000000, 0.000000000000000000, 0.000000000000000000 ) ) ;
#68858 = FACE_OUTER_BOUND ( 'NONE', #22395, .T. ) ;
#68859 = EDGE_CURVE ( 'NONE', #24108, #55259, #19049, .T. ) ;
#68860 = CARTESIAN_POINT ( 'NONE',  ( 32.00000000000000711, 15.00000000000000000, -36.50000000000000000 ) ) ;
#68861 = CARTESIAN_POINT ( 'NONE',  ( -101.2449999999999903, -4.716976649647093289, -6.492361379858945902 ) ) ;
#68862 = ORIENTED_EDGE ( 'NONE', *, *, #65365, .T. ) ;
#68863 = B_SPLINE_CURVE_WITH_KNOTS ( 'NONE', 3,
 ( #63660, #26689, #36969, #11225, #63995, #4555, #32329, #53781, #42591, #59392 ),
 .UNSPECIFIED., .F., .F.,
 ( 4, 2, 2, 2, 4 ),
 ( -6.387773809479085465E-06, 0.0006440562338507882902, 0.0009692782376809175489, 0.001131889239595995677, 0.001294500241511073804 ),
 .UNSPECIFIED. ) ;
#68864 = AXIS2_PLACEMENT_3D ( 'NONE', #53808, #67142, #65765 ) ;
#68865 = CARTESIAN_POINT ( 'NONE',  ( -9.064020486552543332, 110.4999999999999858, 2.960432884595932901 ) ) ;
#68866 =( NAMED_UNIT ( * ) PLANE_ANGLE_UNIT ( ) SI_UNIT ( $, .RADIAN. ) );
#68867 = EDGE_CURVE ( 'NONE', #20480, #19090, #44190, .T. ) ;
#68868 = DIRECTION ( 'NONE',  ( 1.000000000000000000, 0.000000000000000000, 0.000000000000000000 ) ) ;
#68869 = ORIENTED_EDGE ( 'NONE', *, *, #40707, .T. ) ;
#68870 = CARTESIAN_POINT ( 'NONE',  ( -8.437984349512095861, 150.6929263765338192, -5.166775262442723748E-16 ) ) ;
#68871 = CARTESIAN_POINT ( 'NONE',  ( 0.000000000000000000, 42.00000000000000000, 79.00402776293826435 ) ) ;
#68872 = CARTESIAN_POINT ( 'NONE',  ( 6.999798566743344885, 7.519018533394457353E-16, 12.50000000000000000 ) ) ;
#68873 = EDGE_CURVE ( 'NONE', #22128, #49325, #8913, .T. ) ;
#68874 = CARTESIAN_POINT ( 'NONE',  ( -20.71231517720797299, 149.6390813561872619, -10.00000000000000000 ) ) ;
#68875 = CARTESIAN_POINT ( 'NONE',  ( 20.77797364267480518, 115.1388508835393907, -10.00000000000000000 ) ) ;
#68876 = EDGE_LOOP ( 'NONE', ( #59210, #21492, #46498, #51297 ) ) ;
#68877 = FACE_OUTER_BOUND ( 'NONE', #7579, .T. ) ;
#68878 = CARTESIAN_POINT ( 'NONE',  ( -195.0000000000000000, 0.000000000000000000, 0.000000000000000000 ) ) ;
#68879 =( GEOMETRIC_REPRESENTATION_CONTEXT ( 3 ) GLOBAL_UNCERTAINTY_ASSIGNED_CONTEXT ( ( #20618 ) ) GLOBAL_UNIT_ASSIGNED_CONTEXT ( ( #47102, #63586, #31913 ) ) REPRESENTATION_CONTEXT ( 'NONE', 'WORKASPACE' ) );
#68880 = TOROIDAL_SURFACE ( 'NONE', #26167, 1.000000000000000000, 0.5000000000000000000 ) ;
#68881 = CARTESIAN_POINT ( 'NONE',  ( -15.48999599679679662, 118.4999999999999716, 9.500000000000000000 ) ) ;
#68882 = DIRECTION ( 'NONE',  ( 1.000000000000000000, 0.000000000000000000, 0.000000000000000000 ) ) ;
#68883 = AXIS2_PLACEMENT_3D ( 'NONE', #45013, #4104, #52690 ) ;
#68884 = CARTESIAN_POINT ( 'NONE',  ( -74.08452722063037754, 9.430195807687216103, 6.000000000000000888 ) ) ;
#68885 = DIRECTION ( 'NONE',  ( -0.000000000000000000, 0.000000000000000000, -1.000000000000000000 ) ) ;
#68886 = DIRECTION ( 'NONE',  ( -1.189524669241239115E-16, -1.000000000000000000, -0.000000000000000000 ) ) ;
#68887 = CARTESIAN_POINT ( 'NONE',  ( 21.75000000000001066, 22.24999999999998224, -3.750000000000000000 ) ) ;
#68888 = VERTEX_POINT ( 'NONE', #57108 ) ;
#68889 = ORIENTED_EDGE ( 'NONE', *, *, #65931, .T. ) ;
#68890 = DIRECTION ( 'NONE',  ( -0.5000000000000001110, -0.8660254037844385966, 0.000000000000000000 ) ) ;
#68891 = EDGE_CURVE ( 'NONE', #49984, #56901, #52217, .T. ) ;
#68892 = CARTESIAN_POINT ( 'NONE',  ( 0.000000000000000000, 114.9999999999999574, 0.000000000000000000 ) ) ;
#68893 = CARTESIAN_POINT ( 'NONE',  ( 2.607480562269098634, 113.7070736234661723, 8.024999999999984368 ) ) ;
#68894 = ORIENTED_EDGE ( 'NONE', *, *, #39135, .F. ) ;
#68895 = PRESENTATION_STYLE_ASSIGNMENT (( #19972 ) ) ;
#68896 = CARTESIAN_POINT ( 'NONE',  ( -167.4549999999999841, 7.632228543268599452, -2.479861379858951942 ) ) ;
#68897 = DIRECTION ( 'NONE',  ( -1.000000000000000000, 0.000000000000000000, 0.000000000000000000 ) ) ;
#68898 = DIRECTION ( 'NONE',  ( 0.000000000000000000, 1.000000000000000000, 0.000000000000000000 ) ) ;
#68899 = CARTESIAN_POINT ( 'NONE',  ( -49.25707362346617657, 5.598654528085800663, -7.705886871421367523 ) ) ;
#68900 = VECTOR ( 'NONE', #34509, 1000.000000000000000 ) ;
#68901 = CARTESIAN_POINT ( 'NONE',  ( -178.7949999999999875, 2.607480562269069324, -8.024999999999993250 ) ) ;
#68902 = VERTEX_POINT ( 'NONE', #46254 ) ;
#68903 = VECTOR ( 'NONE', #58384, 1000.000000000000000 ) ;
#68904 = CARTESIAN_POINT ( 'NONE',  ( 60.00000000000000000, -2.024042244987997205E-14, -9.500000000000000000 ) ) ;
#68905 = CARTESIAN_POINT ( 'NONE',  ( -10.51142403643257239, 11.79550216340572000, -2.227010390538998408 ) ) ;
#68906 = CIRCLE ( 'NONE', #37509, 0.5000000000000004441 ) ;
#68907 = CARTESIAN_POINT ( 'NONE',  ( -92.45499999999998408, 7.632228543268599452, -2.479861379858951942 ) ) ;
#68908 =( NAMED_UNIT ( * ) PLANE_ANGLE_UNIT ( ) SI_UNIT ( $, .RADIAN. ) );
#68909 = CARTESIAN_POINT ( 'NONE',  ( -74.91404241719055790, 35.67552983406591949, -9.789663199941575300 ) ) ;
#68910 = COLOUR_RGB ( '', 0.66274510, 0.83137255, 0.94901961) ;
#68911 = CIRCLE ( 'NONE', #7128, 0.5000000000000004441 ) ;
#68912 = CARTESIAN_POINT ( 'NONE',  ( -91.79499999999998749, 2.607480562269069324, -8.024999999999993250 ) ) ;
#68913 = CARTESIAN_POINT ( 'NONE',  ( -9.058813317711337021, 129.1550000000000011, -2.943386871421374895 ) ) ;
#68914 = DIRECTION ( 'NONE',  ( 0.000000000000000000, 0.000000000000000000, 1.000000000000000000 ) ) ;
#68915 = CARTESIAN_POINT ( 'NONE',  ( -169.9429263765337907, 0.000000000000000000, 9.524999999999991473 ) ) ;
#68916 = LINE ( 'NONE', #42228, #63045 ) ;
#68917 = EDGE_CURVE ( 'NONE', #23846, #6192, #2812, .T. ) ;
#68918 = TOROIDAL_SURFACE ( 'NONE', #37524, 29.50000000000000000, 0.5000000000000000000 ) ;
#68919 = VERTEX_POINT ( 'NONE', #56780 ) ;
#68920 = LINE ( 'NONE', #64308, #59490 ) ;
#68921 = DIRECTION ( 'NONE',  ( -0.000000000000000000, 1.000000000000000000, -0.000000000000000000 ) ) ;
#68922 = CARTESIAN_POINT ( 'NONE',  ( 23.71231517720798010, 112.9999999999999858, -7.000000000000000000 ) ) ;
#68923 = CARTESIAN_POINT ( 'NONE',  ( -87.50000000000000000, -3.500000000000000000, 24.00000000000000000 ) ) ;
#68924 = ORIENTED_EDGE ( 'NONE', *, *, #44143, .F. ) ;
#68926 = ORIENTED_EDGE ( 'NONE', *, *, #48692, .F. ) ;
#68925 = AXIS2_PLACEMENT_3D ( 'NONE', #34350, #17830, #55454 ) ;
#68927 = COLOUR_RGB ( '', 0.08235294, 0.09019608, 0.10196078) ;
#68928 = CARTESIAN_POINT ( 'NONE',  ( -45.91158282012835201, 9.415467456214855702, -6.077850184675973821 ) ) ;
#68929 = CARTESIAN_POINT ( 'NONE',  ( 31.00000000000002132, 15.00000000000000000, 80.00402776293826435 ) ) ;
#68930 = COLOUR_RGB ( '', 0.08235294, 0.09019608, 0.10196078) ;
#68931 = DIRECTION ( 'NONE',  ( -1.239088197126290817E-16, 0.000000000000000000, -1.000000000000000000 ) ) ;
#68932 = DIRECTION ( 'NONE',  ( 1.000000000000000000, 0.000000000000000000, 0.000000000000000000 ) ) ;
#68933 = DIRECTION ( 'NONE',  ( -0.000000000000000000, -0.000000000000000000, -1.000000000000000000 ) ) ;
#68934 = ORIENTED_EDGE ( 'NONE', *, *, #26963, .F. ) ;
#68935 = CARTESIAN_POINT ( 'NONE',  ( -125.3050000000000068, 8.437984349512086979, -1.550032578732815448E-15 ) ) ;
#68936 = ORIENTED_EDGE ( 'NONE', *, *, #22174, .T. ) ;
#68937 = DIRECTION ( 'NONE',  ( -1.000000000000000000, 0.000000000000000000, 1.734723475976805517E-15 ) ) ;
#68938 = ORIENTED_EDGE ( 'NONE', *, *, #29440, .T. ) ;
#68939 = ORIENTED_EDGE ( 'NONE', *, *, #69425, .T. ) ;
#68940 = EDGE_CURVE ( 'NONE', #62763, #30128, #57199, .T. ) ;
#68941 =( GEOMETRIC_REPRESENTATION_CONTEXT ( 3 ) GLOBAL_UNCERTAINTY_ASSIGNED_CONTEXT ( ( #60874 ) ) GLOBAL_UNIT_ASSIGNED_CONTEXT ( ( #9791, #62866, #14344 ) ) REPRESENTATION_CONTEXT ( 'NONE', 'WORKASPACE' ) );
#68942 = CARTESIAN_POINT ( 'NONE',  ( 179.4361977533518484, 5.000000000000000000, 103.7004518695275550 ) ) ;
#68943 = CARTESIAN_POINT ( 'NONE',  ( 0.000000000000000000, 151.4449999999999932, -9.525000000000000355 ) ) ;
#68944 = DIRECTION ( 'NONE',  ( -0.000000000000000000, 0.000000000000000000, -1.000000000000000000 ) ) ;
#68945 = VECTOR ( 'NONE', #8727, 1000.000000000000000 ) ;
#68946 = ORIENTED_EDGE ( 'NONE', *, *, #3691, .F. ) ;
#68947 = CARTESIAN_POINT ( 'NONE',  ( 3.094860106618431583, 148.2049999999999841, 9.525000000000000355 ) ) ;
#68948 =( NAMED_UNIT ( * ) PLANE_ANGLE_UNIT ( ) SI_UNIT ( $, .RADIAN. ) );
#68949 = CARTESIAN_POINT ( 'NONE',  ( -129.5929263765345070, -3.094860106630128449, -9.524999999991493382 ) ) ;
#68950 = AXIS2_PLACEMENT_3D ( 'NONE', #66043, #44984, #17872 ) ;
#68951 = EDGE_LOOP ( 'NONE', ( #39811, #16860, #14259, #10482 ) ) ;
#68952 = CARTESIAN_POINT ( 'NONE',  ( 2.607480562269076430, 122.7929263765338135, -8.025000000000000355 ) ) ;
#68953 = DIRECTION ( 'NONE',  ( -0.000000000000000000, 0.000000000000000000, -1.000000000000000000 ) ) ;
#68954 = DIRECTION ( 'NONE',  ( 0.000000000000000000, 0.000000000000000000, 1.000000000000000000 ) ) ;
#68955 = FILL_AREA_STYLE ('',( #19710 ) ) ;
#68956 = AXIS2_PLACEMENT_3D ( 'NONE', #65727, #2329, #23495 ) ;
#68957 = COLOUR_RGB ( '', 0.31764706, 0.68627451, 0.89019608) ;
#68958 = CYLINDRICAL_SURFACE ( 'NONE', #59824, 0.5000000000000004441 ) ;
#68959 = ADVANCED_FACE ( 'NONE', ( #7881 ), #35869, .T. ) ;
#68960 = SURFACE_SIDE_STYLE ('',( #10892 ) ) ;
#68961 = ORIENTED_EDGE ( 'NONE', *, *, #5524, .T. ) ;
#68962 = CARTESIAN_POINT ( 'NONE',  ( -3.000000000000000444, 0.000000000000000000, 32.50000000000000000 ) ) ;
#68963 = ORIENTED_EDGE ( 'NONE', *, *, #68381, .F. ) ;
#68964 = CARTESIAN_POINT ( 'NONE',  ( -61.34292637653379643, -9.058813317711329915, 2.943386871421371787 ) ) ;
#68965 = CARTESIAN_POINT ( 'NONE',  ( -7.766025168014158986, 0.5488498361408529203, 0.7660251680141585418 ) ) ;
#68966 = AXIS2_PLACEMENT_3D ( 'NONE', #62945, #14091, #56990 ) ;
#68967 = CARTESIAN_POINT ( 'NONE',  ( -153.3549999999999898, -4.716976649647093289, -6.492361379858945902 ) ) ;
#68969 = ORIENTED_EDGE ( 'NONE', *, *, #34759, .F. ) ;
#68968 = EDGE_CURVE ( 'NONE', #8600, #62679, #44896, .T. ) ;
#68970 = AXIS2_PLACEMENT_3D ( 'NONE', #63929, #64643, #26964 ) ;
#68971 = AXIS2_PLACEMENT_3D ( 'NONE', #15391, #58609, #27260 ) ;
#68972 = EDGE_CURVE ( 'NONE', #26540, #61448, #16814, .T. ) ;
#68973 = DIRECTION ( 'NONE',  ( 0.000000000000000000, 0.000000000000000000, 1.000000000000000000 ) ) ;
#68974 = CARTESIAN_POINT ( 'NONE',  ( 75.00000000000000000, 20.14920990499772913, 6.614546734589652033 ) ) ;
#68975 = FILL_AREA_STYLE ('',( #3498 ) ) ;
#68976 = ORIENTED_EDGE ( 'NONE', *, *, #30641, .F. ) ;
#68977 = EDGE_LOOP ( 'NONE', ( #57282, #51107, #8148, #30611 ) ) ;
#68978 = CARTESIAN_POINT ( 'NONE',  ( 22.29424117603575084, 26.17668566172280009, 27.49998957561865964 ) ) ;
#68979 = EDGE_CURVE ( 'NONE', #63620, #67437, #10365, .T. ) ;
#68981 = CARTESIAN_POINT ( 'NONE',  ( -63.05499999999998550, -9.827790563157499189E-16, -8.024999999999991473 ) ) ;
#68980 = AXIS2_PLACEMENT_3D ( 'NONE', #50307, #23227, #13339 ) ;
#68982 = EDGE_LOOP ( 'NONE', ( #35481, #55529, #33353, #34504 ) ) ;
#68983 = DIRECTION ( 'NONE',  ( -0.000000000000000000, 0.000000000000000000, -1.000000000000000000 ) ) ;
#68984 = FACE_OUTER_BOUND ( 'NONE', #37764, .T. ) ;
#68985 = CARTESIAN_POINT ( 'NONE',  ( -90.05707362346616662, 0.000000000000000000, 9.524999999999991473 ) ) ;
#68986 = CARTESIAN_POINT ( 'NONE',  ( -17.75000000000000355, -4.000000000000000000, 24.00000000000000000 ) ) ;
#68987 = ORIENTED_EDGE ( 'NONE', *, *, #41171, .F. ) ;
#68988 = CIRCLE ( 'NONE', #33014, 8.000000000000007105 ) ;
#68989 = DIRECTION ( 'NONE',  ( 1.000000000000000000, 0.000000000000000000, 0.000000000000000000 ) ) ;
#68990 = CYLINDRICAL_SURFACE ( 'NONE', #34923, 0.5000000000000004441 ) ;
#68991 = CARTESIAN_POINT ( 'NONE',  ( 33.00000000000001421, 14.00000000000000000, 36.49999999999999289 ) ) ;
#68993 = FILL_AREA_STYLE ('',( #38038 ) ) ;
#68992 = DIRECTION ( 'NONE',  ( 0.000000000000000000, 0.000000000000000000, 1.000000000000000000 ) ) ;
#68994 = CARTESIAN_POINT ( 'NONE',  ( -115.4949999999999903, 6.826472737025113702, -4.959722759717902107 ) ) ;
#68995 = CARTESIAN_POINT ( 'NONE',  ( 5.598654528085805993, 150.2449999999999761, 7.705886871421374629 ) ) ;
#68996 = CARTESIAN_POINT ( 'NONE',  ( -95.84499999999998465, -7.632228543268599452, 2.479861379858951054 ) ) ;
#68997 = CARTESIAN_POINT ( 'NONE',  ( 3.749999999999999556, 33.99999999999998579, -3.750000000000000000 ) ) ;
#68998 = COLOUR_RGB ( '', 0.72549020, 0.75294118, 0.79215686) ;
#68999 = TOROIDAL_SURFACE ( 'NONE', #47707, 13.49999999999999822, 0.5000000000000000000 ) ;
#69000 = DIRECTION ( 'NONE',  ( 0.000000000000000000, 0.000000000000000000, 1.000000000000000000 ) ) ;
#69001 = EDGE_LOOP ( 'NONE', ( #67092, #50036, #268, #13311 ) ) ;
#69002 = CARTESIAN_POINT ( 'NONE',  ( -130.1929263765337907, -10.01517768586948698, 6.132527647946031529E-16 ) ) ;
#69003 = AXIS2_PLACEMENT_3D ( 'NONE', #37028, #14476, #3533 ) ;
#69004 = CARTESIAN_POINT ( 'NONE',  ( -48.14292637653380780, 5.598654528085800663, -7.705886871421367523 ) ) ;
#69005 = CARTESIAN_POINT ( 'NONE',  ( -160.4949999999999761, 6.826472737025113702, -4.959722759717902107 ) ) ;
#69006 = FILL_AREA_STYLE_COLOUR ( '', #28427 ) ;
#69007 = SURFACE_STYLE_FILL_AREA ( #68309 ) ;
#69008 = ORIENTED_EDGE ( 'NONE', *, *, #4516, .F. ) ;
#69010 = EDGE_LOOP ( 'NONE', ( #66349, #12249, #48264, #43331 ) ) ;
#69009 = COLOUR_RGB ( '', 0.31764706, 0.68627451, 0.89019608) ;
#69011 = PRESENTATION_STYLE_ASSIGNMENT (( #59120 ) ) ;
#69012 = AXIS2_PLACEMENT_3D ( 'NONE', #38645, #33657, #55100 ) ;
#69013 = CARTESIAN_POINT ( 'NONE',  ( -6.826472737025120807, 117.3929263765338078, -4.959722759717907437 ) ) ;
#69014 = DIRECTION ( 'NONE',  ( -0.2413793103448194644, -0.9704308468600220117, 0.000000000000000000 ) ) ;
#69015 = CARTESIAN_POINT ( 'NONE',  ( -195.0000000000000000, 1.166476076187852838E-15, -9.524999999999991473 ) ) ;
#69016 = ORIENTED_EDGE ( 'NONE', *, *, #9222, .F. ) ;
#69017 = CARTESIAN_POINT ( 'NONE',  ( -149.7549999999999955, 4.716976649647091513, -6.492361379858946790 ) ) ;
#69018 = CIRCLE ( 'NONE', #49946, 0.5000000000000004441 ) ;
#69019 = ORIENTED_EDGE ( 'NONE', *, *, #64984, .F. ) ;
#69020 = DIRECTION ( 'NONE',  ( -1.000000000000000000, -0.000000000000000000, -0.000000000000000000 ) ) ;
#69021 = CARTESIAN_POINT ( 'NONE',  ( 2.816687638038912352E-15, 154.4999999999999432, 23.00000000000000000 ) ) ;
#69022 = ORIENTED_EDGE ( 'NONE', *, *, #32409, .T. ) ;
#69023 = ADVANCED_FACE ( 'NONE', ( #56416 ), #33414, .T. ) ;
#69024 = PRESENTATION_LAYER_ASSIGNMENT (  '', '', ( #3803 ) ) ;
#69025 = CYLINDRICAL_SURFACE ( 'NONE', #61873, 1.000000000000000000 ) ;
#69026 = DIRECTION ( 'NONE',  ( 1.000000000000000000, 0.000000000000000000, 0.000000000000000000 ) ) ;
#69027 = CARTESIAN_POINT ( 'NONE',  ( -9.058813317711338797, 119.3449999999999989, 2.943386871421373563 ) ) ;
#69028 = CARTESIAN_POINT ( 'NONE',  ( 0.000000000000000000, 111.9999999999999858, -8.025000000000000355 ) ) ;
#69029 = EDGE_CURVE ( 'NONE', #5601, #9272, #13151, .T. ) ;
#69030 = ORIENTED_EDGE ( 'NONE', *, *, #54170, .T. ) ;
#69031 = EDGE_CURVE ( 'NONE', #34861, #55490, #6659, .T. ) ;
#69032 = CARTESIAN_POINT ( 'NONE',  ( 9.058813317711337021, 121.6549999999999869, 2.943386871421375783 ) ) ;
#69033 = CARTESIAN_POINT ( 'NONE',  ( -65.90499999999998693, 2.607480562269069324, -8.024999999999993250 ) ) ;
#69034 = CARTESIAN_POINT ( 'NONE',  ( -80.60707362346614957, -8.102448949553174629, 5.886773742842742685 ) ) ;
#69035 = VERTEX_POINT ( 'NONE', #38397 ) ;
#69036 = CARTESIAN_POINT ( 'NONE',  ( -5.598654528085808657, 150.7549999999999955, 7.705886871421373741 ) ) ;
#69037 = EDGE_CURVE ( 'NONE', #20640, #42065, #59446, .T. ) ;
#69038 = CARTESIAN_POINT ( 'NONE',  ( 5.710692600061823221, 2.500000000000000000, -4.108790270285303414 ) ) ;
#69039 = MECHANICAL_DESIGN_GEOMETRIC_PRESENTATION_REPRESENTATION (  '', ( #9492 ), #56682 ) ;
#69040 = ADVANCED_FACE ( 'NONE', ( #38740 ), #43343, .F. ) ;
#69041 = DIRECTION ( 'NONE',  ( -0.000000000000000000, -1.000000000000000000, -0.000000000000000000 ) ) ;
#69042 = ADVANCED_FACE ( 'NONE', ( #64737 ), #11956, .F. ) ;
#69043 = ORIENTED_EDGE ( 'NONE', *, *, #43353, .T. ) ;
#69044 = COLOUR_RGB ( '', 0.40784314, 0.44705882, 0.49803922) ;
#69045 = CARTESIAN_POINT ( 'NONE',  ( -74.99999999999998579, 119.9999999999997726, 9.500000000000000000 ) ) ;
#69046 = CARTESIAN_POINT ( 'NONE',  ( -46.94499999999998607, -9.827790563157499189E-16, -8.024999999999991473 ) ) ;
#69047 = ORIENTED_EDGE ( 'NONE', *, *, #56359, .T. ) ;
#69048 = CARTESIAN_POINT ( 'NONE',  ( 5.015307210679814887, 111.7971308996410045, -6.528277465523999901 ) ) ;
#69049 = STYLED_ITEM ( 'NONE', ( #67941 ), #56173 ) ;
#69050 = DIRECTION ( 'NONE',  ( -0.000000000000000000, 1.000000000000000000, -0.000000000000000000 ) ) ;
#69051 = EDGE_CURVE ( 'NONE', #56670, #68565, #43668, .T. ) ;
#69052 = CIRCLE ( 'NONE', #38753, 0.5000000000000004441 ) ;
#69053 = DIRECTION ( 'NONE',  ( 1.000000000000000000, -1.156482317317866302E-16, 0.000000000000000000 ) ) ;
#69054 = VERTEX_POINT ( 'NONE', #68731 ) ;
#69055 = CARTESIAN_POINT ( 'NONE',  ( -9.000000000000003553, 24.99999999999998579, 4.000000000000000000 ) ) ;
#69056 = DIRECTION ( 'NONE',  ( 0.000000000000000000, 0.000000000000000000, 1.000000000000000000 ) ) ;
#69057 = EDGE_LOOP ( 'NONE', ( #38605, #16934, #12921, #46461 ) ) ;
#69058 = CARTESIAN_POINT ( 'NONE',  ( -1.744870598150811469, -7.000000000000001776, 0.2069669095365348765 ) ) ;
#69059 = PRESENTATION_LAYER_ASSIGNMENT (  '', '', ( #29722 ) ) ;
#69060 = CARTESIAN_POINT ( 'NONE',  ( -94.55499999999999261, 0.000000000000000000, 8.024999999999991473 ) ) ;
#69061 = EDGE_LOOP ( 'NONE', ( #33618, #25821, #62046, #16765 ) ) ;
#69062 = LINE ( 'NONE', #36006, #31689 ) ;
#69063 = FACE_OUTER_BOUND ( 'NONE', #21555, .T. ) ;
#69064 = CARTESIAN_POINT ( 'NONE',  ( -130.7070736234661581, -3.094860106618431139, -9.524999999999991473 ) ) ;
#69065 = FILL_AREA_STYLE ('',( #15610 ) ) ;
#69066 = CARTESIAN_POINT ( 'NONE',  ( -9.058813317711337021, 149.0449999999999875, -2.943386871421374895 ) ) ;
#69067 = CARTESIAN_POINT ( 'NONE',  ( -66.95707362346617231, 9.058813317711329915, -2.943386871421373119 ) ) ;
#69068 = AXIS2_PLACEMENT_3D ( 'NONE', #17091, #38905, #39589 ) ;
#69069 = COLOUR_RGB ( '', 0.09019608, 0.27058824, 0.51372549) ;
#69070 = CARTESIAN_POINT ( 'NONE',  ( -81.29292637653378506, 3.094860106618428031, -9.524999999999993250 ) ) ;
#69071 = VERTEX_POINT ( 'NONE', #31403 ) ;
#69072 = DIRECTION ( 'NONE',  ( -1.000000000000000000, 0.000000000000000000, 0.000000000000000000 ) ) ;
#69073 = SURFACE_STYLE_USAGE ( .BOTH. , #66096 ) ;
#69074 = FILL_AREA_STYLE_COLOUR ( '', #33541 ) ;
#69075 =( GEOMETRIC_REPRESENTATION_CONTEXT ( 3 ) GLOBAL_UNCERTAINTY_ASSIGNED_CONTEXT ( ( #25619 ) ) GLOBAL_UNIT_ASSIGNED_CONTEXT ( ( #36213, #58942, #30528 ) ) REPRESENTATION_CONTEXT ( 'NONE', 'WORKASPACE' ) );
#69076 = CARTESIAN_POINT ( 'NONE',  ( -113.0049999999999812, 6.826472737025116366, 4.959722759717898555 ) ) ;
#69077 = CARTESIAN_POINT ( 'NONE',  ( -5.598654528085806881, 115.7449999999999903, -7.705886871421374629 ) ) ;
#69078 = CARTESIAN_POINT ( 'NONE',  ( -124.4949999999999761, 6.826472737025113702, -4.959722759717902107 ) ) ;
#69079 = CIRCLE ( 'NONE', #7253, 0.2500000000000002220 ) ;
#69080 = CIRCLE ( 'NONE', #38774, 5.000000000000000000 ) ;
#69081 = SPHERICAL_SURFACE ( 'NONE', #62825, 0.2500000000000000000 ) ;
#69082 = EDGE_CURVE ( 'NONE', #62231, #17220, #52897, .T. ) ;
#69083 = CARTESIAN_POINT ( 'NONE',  ( -130.9429263765338192, 0.000000000000000000, 9.524999999999991473 ) ) ;
#69084 = ORIENTED_EDGE ( 'NONE', *, *, #21472, .F. ) ;
#69085 = CARTESIAN_POINT ( 'NONE',  ( -162.7429263765338021, -5.598654528085803328, -7.705886871421366635 ) ) ;
#69086 =( LENGTH_UNIT ( ) NAMED_UNIT ( * ) SI_UNIT ( .MILLI., .METRE. ) );
#69087 = AXIS2_PLACEMENT_3D ( 'NONE', #66223, #28213, #60265 ) ;
#69088 = CONICAL_SURFACE ( 'NONE', #8433, 3.600000000000005862, 0.7853981633974447263 ) ;
#69089 = CARTESIAN_POINT ( 'NONE',  ( -60.00000000000000000, -2.024042244987997205E-14, -11.50000000000000000 ) ) ;
#69090 = DIRECTION ( 'NONE',  ( -0.000000000000000000, -0.000000000000000000, 1.000000000000000000 ) ) ;
#69091 = CARTESIAN_POINT ( 'NONE',  ( 10.00000000000000533, 43.00000000000000000, -45.61250543006183733 ) ) ;
#69092 =( LENGTH_UNIT ( ) NAMED_UNIT ( * ) SI_UNIT ( .MILLI., .METRE. ) );
#69093 = EDGE_LOOP ( 'NONE', ( #1092, #41363, #51472, #4286 ) ) ;
#69094 = CARTESIAN_POINT ( 'NONE',  ( -75.14292637653380780, 5.598654528085800663, -7.705886871421367523 ) ) ;
#69095 = CIRCLE ( 'NONE', #57850, 0.9999999999999986677 ) ;
#69096 = CARTESIAN_POINT ( 'NONE',  ( 60.00000000000000000, 1.797044900979284448E-15, 6.500000000000000000 ) ) ;
#69097 = SURFACE_STYLE_USAGE ( .BOTH. , #42746 ) ;
#69098 = CIRCLE ( 'NONE', #41048, 1.000000000000000888 ) ;
#69099 = CARTESIAN_POINT ( 'NONE',  ( 2.607480562269118174, 152.7929263765338135, -8.024999999999970157 ) ) ;
#69101 =( BOUNDED_SURFACE ( )  B_SPLINE_SURFACE ( 3, 2, ( 
 ( #36118, #63180, #26225 ),
 ( #47764, #55023, #27928 ),
 ( #49439, #59256, #117 ),
 ( #58947, #64897, #16747 ),
 ( #27241, #69491, #38911 ),
 ( #54344, #21646, #5798 ),
 ( #64571, #6850, #32912 ),
 ( #65247, #48428, #64206 ),
 ( #32530, #49115, #43163 ),
 ( #800, #48085, #43510 ) ),
 .UNSPECIFIED., .F., .F., .F. ) 
 B_SPLINE_SURFACE_WITH_KNOTS ( ( 4, 2, 2, 2, 4 ),
 ( 3, 3 ),
 ( 4.181938019525841099, 4.707249841439277382, 5.232561663352713666, 5.757873485266149949, 6.283185307179586232 ),
 ( 0.000000000000000000, 1.000000000000000000 ),
 .UNSPECIFIED. ) 
 GEOMETRIC_REPRESENTATION_ITEM ( )  RATIONAL_B_SPLINE_SURFACE ( (
 ( 1.000000000000000000, 0.7615729461579494597, 1.000000000000000000),
 ( 1.000000000000000000, 0.7459210345859041968, 1.000000000000000000),
 ( 1.000000000000000000, 0.7272421848981694970, 1.000000000000000000),
 ( 1.000000000000000000, 0.6881200523220029064, 1.000000000000000000),
 ( 1.000000000000000000, 0.6676671612971883940, 1.000000000000000000),
 ( 1.000000000000000000, 0.6306589281295537086, 1.000000000000000000),
 ( 1.000000000000000000, 0.6141839381258914488, 1.000000000000000000),
 ( 1.000000000000000000, 0.5911458751171522197, 1.000000000000000000),
 ( 1.000000000000000000, 0.5846320934540327752, 1.000000000000000000),
 ( 1.000000000000000000, 0.5847102846637711737, 1.000000000000000000) ) ) 
 REPRESENTATION_ITEM ( '' )  SURFACE ( )  );
#69100 = CARTESIAN_POINT ( 'NONE',  ( 9.250000000000003553, 27.74999999999998934, -3.750000000000000000 ) ) ;
#69102 = DIRECTION ( 'NONE',  ( 0.000000000000000000, 1.000000000000000000, 0.000000000000000000 ) ) ;
#69103 = CARTESIAN_POINT ( 'NONE',  ( -177.9550000000000125, -7.632228543268599452, 2.479861379858951054 ) ) ;
#69104 = EDGE_CURVE ( 'NONE', #26743, #52121, #48316, .T. ) ;
#69105 = ORIENTED_EDGE ( 'NONE', *, *, #47959, .T. ) ;
#69106 = LINE ( 'NONE', #52925, #43772 ) ;
#69107 = VERTEX_POINT ( 'NONE', #968 ) ;
#69108 = FACE_OUTER_BOUND ( 'NONE', #66227, .T. ) ;
#69109 = CARTESIAN_POINT ( 'NONE',  ( 8.437984349512095861, 147.3070736234662093, 1.550032578732817026E-15 ) ) ;
#69110 = EDGE_CURVE ( 'NONE', #39296, #20493, #54842, .T. ) ;
#69111 = CIRCLE ( 'NONE', #38816, 0.5000000000000004441 ) ;
#69112 = VERTEX_POINT ( 'NONE', #20527 ) ;
#69113 = CARTESIAN_POINT ( 'NONE',  ( -101.7570736234661695, -5.598654528085801552, 7.705886871421367523 ) ) ;
#69114 = CARTESIAN_POINT ( 'NONE',  ( -97.70499999999996987, 2.607480562269072433, 8.024999999999991473 ) ) ;
#69115 = CARTESIAN_POINT ( 'NONE',  ( -9.827790563157511022E-16, 131.5570736234661524, 8.025000000000000355 ) ) ;
#69116 = ORIENTED_EDGE ( 'NONE', *, *, #17200, .F. ) ;
#69117 = DIRECTION ( 'NONE',  ( 0.000000000000000000, -1.000000000000000000, 0.000000000000000000 ) ) ;
#69118 = DIRECTION ( 'NONE',  ( -0.7681514953298218540, 0.000000000000000000, 0.6402681315062924705 ) ) ;
#69119 = LINE ( 'NONE', #20928, #20934 ) ;
#69120 = CARTESIAN_POINT ( 'NONE',  ( -84.49999999999997158, 50.00000000000000000, -9.999999999999998224 ) ) ;
#69121 = EDGE_CURVE ( 'NONE', #47549, #65448, #63441, .T. ) ;
#69122 = AXIS2_PLACEMENT_3D ( 'NONE', #51978, #56180, #67438 ) ;
#69123 = ORIENTED_EDGE ( 'NONE', *, *, #55798, .F. ) ;
#69124 = AXIS2_PLACEMENT_3D ( 'NONE', #65663, #49167, #6230 ) ;
#69125 = CARTESIAN_POINT ( 'NONE',  ( -70.34499999999998465, 7.632228543268599452, -2.479861379858951942 ) ) ;
#69126 = ORIENTED_EDGE ( 'NONE', *, *, #25177, .T. ) ;
#69127 = CARTESIAN_POINT ( 'NONE',  ( 62.10000000000000142, 11.99999999999999822, 3.499999999999992895 ) ) ;
#69128 = DIRECTION ( 'NONE',  ( 1.000000000000000000, 0.000000000000000000, 0.000000000000000000 ) ) ;
#69129 = EDGE_CURVE ( 'NONE', #48775, #53539, #3327, .T. ) ;
#69130 = EDGE_LOOP ( 'NONE', ( #64154, #56017, #27091, #41444 ) ) ;
#69131 = DIRECTION ( 'NONE',  ( -0.000000000000000000, -0.000000000000000000, 1.000000000000000000 ) ) ;
#69132 = DIRECTION ( 'NONE',  ( 0.000000000000000000, 0.000000000000000000, -1.000000000000000000 ) ) ;
#69133 = FACE_OUTER_BOUND ( 'NONE', #35777, .T. ) ;
#69134 = AXIS2_PLACEMENT_3D ( 'NONE', #9240, #30663, #62669 ) ;
#69135 = CARTESIAN_POINT ( 'NONE',  ( -74.08452723581622479, 9.430195785006297626, 6.025268399887226067 ) ) ;
#69136 = ORIENTED_EDGE ( 'NONE', *, *, #58370, .F. ) ;
#69137 = CARTESIAN_POINT ( 'NONE',  ( -8.690363669209109077, 2.361802048420726496, -2.947848588679145454 ) ) ;
#69138 = ORIENTED_EDGE ( 'NONE', *, *, #33979, .T. ) ;
#69139 = CYLINDRICAL_SURFACE ( 'NONE', #57223, 0.5000000000000004441 ) ;
#69140 =( LENGTH_UNIT ( ) NAMED_UNIT ( * ) SI_UNIT ( .MILLI., .METRE. ) );
#69141 = CARTESIAN_POINT ( 'NONE',  ( -161.7570736234661695, -5.598654528085801552, 7.705886871421367523 ) ) ;
#69142 = CARTESIAN_POINT ( 'NONE',  ( -3.094860106618432471, 118.5949999999999847, -9.525000000000000355 ) ) ;
#69143 = CIRCLE ( 'NONE', #50067, 7.500000000000000000 ) ;
#69144 = CARTESIAN_POINT ( 'NONE',  ( -108.3570736234661780, 5.598654528085804216, 7.705886871421366635 ) ) ;
#69145 = MECHANICAL_DESIGN_GEOMETRIC_PRESENTATION_REPRESENTATION (  '', ( #41089 ), #17489 ) ;
#69146 = CARTESIAN_POINT ( 'NONE',  ( 5.196152422706629359, 9.000000000000008882, 7.500000000000000000 ) ) ;
#69147 = ORIENTED_EDGE ( 'NONE', *, *, #64252, .T. ) ;
#69148 = CARTESIAN_POINT ( 'NONE',  ( 31.00000000000001421, 42.00000000000000000, 36.50000000000000000 ) ) ;
#69150 = CARTESIAN_POINT ( 'NONE',  ( 2.999999999999997335, 5.000000000000000000, 72.00402776293822171 ) ) ;
#69149 = CARTESIAN_POINT ( 'NONE',  ( 21.24999999999998579, -2.457524924300472510E-14, 3.750000000000000000 ) ) ;
#69151 = PRESENTATION_STYLE_ASSIGNMENT (( #22000 ) ) ;
#69152 = CARTESIAN_POINT ( 'NONE',  ( -138.9549999999999841, -7.632228543268599452, 2.479861379858951054 ) ) ;
#69153 = CARTESIAN_POINT ( 'NONE',  ( -85.70707362346617231, -3.094860106618431139, -9.524999999999991473 ) ) ;
#69154 = CARTESIAN_POINT ( 'NONE',  ( -71.50000000000000000, 35.92875272052971525, 9.500000000000000000 ) ) ;
#69155 = CARTESIAN_POINT ( 'NONE',  ( -154.7950000000000159, 2.607480562269068880, -8.024999999999993250 ) ) ;
#69156 = CARTESIAN_POINT ( 'NONE',  ( -139.4949999999999761, 6.826472737025113702, -4.959722759717902107 ) ) ;
#69157 = VERTEX_POINT ( 'NONE', #48604 ) ;
#69158 = ADVANCED_FACE ( 'NONE', ( #12993 ), #69599, .F. ) ;
#69159 = CARTESIAN_POINT ( 'NONE',  ( 70.87837837837835764, 13.70805908423323949, 9.500000000000000000 ) ) ;
#69160 = AXIS2_PLACEMENT_3D ( 'NONE', #63251, #35486, #14729 ) ;
#69161 = CARTESIAN_POINT ( 'NONE',  ( 20.71231517720798365, 149.5697028012963301, -10.00000000000000000 ) ) ;
#69162 = UNCERTAINTY_MEASURE_WITH_UNIT (LENGTH_MEASURE( 1.000000000000000082E-05 ), #47899, 'distance_accuracy_value', 'NONE');
#69163 = CARTESIAN_POINT ( 'NONE',  ( -54.35499999999998977, -4.716976649647093289, -6.492361379858945902 ) ) ;
#69164 =( NAMED_UNIT ( * ) PLANE_ANGLE_UNIT ( ) SI_UNIT ( $, .RADIAN. ) );
#69165 = AXIS2_PLACEMENT_3D ( 'NONE', #49232, #44342, #43986 ) ;
#69166 = DIRECTION ( 'NONE',  ( -0.000000000000000000, 1.000000000000000000, -0.000000000000000000 ) ) ;
#69167 =( NAMED_UNIT ( * ) SI_UNIT ( $, .STERADIAN. ) SOLID_ANGLE_UNIT ( ) );
#69168 = FACE_OUTER_BOUND ( 'NONE', #48329, .T. ) ;
#69169 = MECHANICAL_DESIGN_GEOMETRIC_PRESENTATION_REPRESENTATION (  '', ( #551 ), #38868 ) ;
#69170 = CIRCLE ( 'NONE', #24260, 0.5000000000000004441 ) ;
#69171 = FILL_AREA_STYLE ('',( #15386 ) ) ;
#69172 = UNCERTAINTY_MEASURE_WITH_UNIT (LENGTH_MEASURE( 1.000000000000000082E-05 ), #20524, 'distance_accuracy_value', 'NONE');
#69173 = DIRECTION ( 'NONE',  ( -1.000000000000000000, -1.010476424756490132E-16, -2.775557561562891351E-17 ) ) ;
#69174 = DIRECTION ( 'NONE',  ( 0.000000000000000000, 0.000000000000000000, -1.000000000000000000 ) ) ;
#69175 = CARTESIAN_POINT ( 'NONE',  ( -178.3429263765338249, -9.058813317711329915, 2.943386871421371787 ) ) ;
#69176 = EDGE_CURVE ( 'NONE', #6055, #47666, #5557, .T. ) ;
#69177 = CARTESIAN_POINT ( 'NONE',  ( 29.00000000000002842, 34.36176364315826248, 80.00402776293826435 ) ) ;
#69178 = ADVANCED_FACE ( 'NONE', ( #29149 ), #14582, .T. ) ;
#69179 = CARTESIAN_POINT ( 'NONE',  ( -7.632228543268608334, 138.8429263765337964, 2.479861379858952830 ) ) ;
#69180 = CIRCLE ( 'NONE', #5133, 0.5000000000000004441 ) ;
#69181 = CARTESIAN_POINT ( 'NONE',  ( -12.72792206135785165, 1.797044900979284448E-15, 10.00000000000000000 ) ) ;
#69182 = CARTESIAN_POINT ( 'NONE',  ( 10.57623092156537936, 58.31681314173471975, -6.349999999999996092 ) ) ;
#69183 = VECTOR ( 'NONE', #1765, 1000.000000000000227 ) ;
#69184 = ORIENTED_EDGE ( 'NONE', *, *, #53607, .F. ) ;
#69186 = CARTESIAN_POINT ( 'NONE',  ( -2.607480562269073765, 112.2070736234661581, -8.025000000000000355 ) ) ;
#69185 = CIRCLE ( 'NONE', #11880, 12.50000000000001066 ) ;
#69187 = ADVANCED_FACE ( 'NONE', ( #18280 ), #67155, .T. ) ;
#69188 = CARTESIAN_POINT ( 'NONE',  ( -20.42980746818723503, 114.8194254430358399, 10.32394991351191571 ) ) ;
#69189 = CARTESIAN_POINT ( 'NONE',  ( 22.41861097278089332, 25.30861756478646996, -27.43527847615431625 ) ) ;
#69190 = FACE_OUTER_BOUND ( 'NONE', #9433, .T. ) ;
#69191 = EDGE_CURVE ( 'NONE', #23204, #46742, #11203, .T. ) ;
#69192 = VERTEX_POINT ( 'NONE', #44368 ) ;
#69193 = EDGE_LOOP ( 'NONE', ( #6357, #3537, #63922 ) ) ;
#69194 = CARTESIAN_POINT ( 'NONE',  ( 29.00000000000000000, 42.00000000000000000, -89.00000000000000000 ) ) ;
#69195 =( LENGTH_UNIT ( ) NAMED_UNIT ( * ) SI_UNIT ( .MILLI., .METRE. ) );
#69196 = ORIENTED_EDGE ( 'NONE', *, *, #69336, .F. ) ;
#69197 = CARTESIAN_POINT ( 'NONE',  ( 3.094860106618435136, 119.4049999999999727, -9.525000000000000355 ) ) ;
#69198 = CARTESIAN_POINT ( 'NONE',  ( -115.9429263765338050, 0.000000000000000000, 9.524999999999991473 ) ) ;
#69199 = FACE_OUTER_BOUND ( 'NONE', #16518, .T. ) ;
#69200 = EDGE_CURVE ( 'NONE', #67546, #19997, #2142, .T. ) ;
#69201 = CARTESIAN_POINT ( 'NONE',  ( -51.50000000000000000, -2.024042244987997205E-14, -9.999999999999998224 ) ) ;
#69202 = CARTESIAN_POINT ( 'NONE',  ( -102.2949999999999733, -2.607480562269069768, 8.024999999999991473 ) ) ;
#69203 = ORIENTED_EDGE ( 'NONE', *, *, #6261, .F. ) ;
#69204 = PRESENTATION_LAYER_ASSIGNMENT (  '', '', ( #27594 ) ) ;
#69205 = CARTESIAN_POINT ( 'NONE',  ( 66.74999999999998579, 36.75000000000000000, 4.000000000000000000 ) ) ;
#69206 = EDGE_CURVE ( 'NONE', #69671, #23279, #23215, .T. ) ;
#69207 = ORIENTED_EDGE ( 'NONE', *, *, #4944, .T. ) ;
#69208 = CARTESIAN_POINT ( 'NONE',  ( -6.826472737025120807, 156.3929263765337794, -4.959722759717907437 ) ) ;
#69209 = CARTESIAN_POINT ( 'NONE',  ( -195.0000000000000000, 0.000000000000000000, 11.99999999999999645 ) ) ;
#69210 = AXIS2_PLACEMENT_3D ( 'NONE', #21019, #42512, #10127 ) ;
#69211 = FACE_OUTER_BOUND ( 'NONE', #7492, .T. ) ;
#69212 = CARTESIAN_POINT ( 'NONE',  ( -15.98999599679679839, 117.4999999999999716, 9.500000000000000000 ) ) ;
#69213 = CARTESIAN_POINT ( 'NONE',  ( 20.71462257042821520, 114.4999999999999574, -10.00000000000000355 ) ) ;
#69214 = EDGE_LOOP ( 'NONE', ( #62062, #18042, #68694, #58045 ) ) ;
#69215 = CARTESIAN_POINT ( 'NONE',  ( 6.826472737025119919, 127.8929263765338220, 4.959722759717908325 ) ) ;
#69216 = STYLED_ITEM ( 'NONE', ( #16703 ), #49805 ) ;
#69217 =( GEOMETRIC_REPRESENTATION_CONTEXT ( 3 ) GLOBAL_UNCERTAINTY_ASSIGNED_CONTEXT ( ( #60017 ) ) GLOBAL_UNIT_ASSIGNED_CONTEXT ( ( #69621, #52780, #64707 ) ) REPRESENTATION_CONTEXT ( 'NONE', 'WORKASPACE' ) );
#69218 =( NAMED_UNIT ( * ) SI_UNIT ( $, .STERADIAN. ) SOLID_ANGLE_UNIT ( ) );
#69219 =( NAMED_UNIT ( * ) SI_UNIT ( $, .STERADIAN. ) SOLID_ANGLE_UNIT ( ) );
#69220 = LINE ( 'NONE', #20679, #22052 ) ;
#69221 = DIRECTION ( 'NONE',  ( 1.000000000000000000, -0.000000000000000000, -0.000000000000000000 ) ) ;
#69222 = DIRECTION ( 'NONE',  ( -1.000000000000000000, 0.000000000000000000, 0.000000000000000000 ) ) ;
#69223 =( BOUNDED_CURVE ( )  B_SPLINE_CURVE ( 2, ( #2948, #45262, #19519, #29738, #1894, #41020, #67034, #45615, #23762, #62440, #14254 ),
 .UNSPECIFIED., .F., .F. ) 
 B_SPLINE_CURVE_WITH_KNOTS ( ( 3, 2, 2, 2, 2, 3 ),
 ( 0.7941176470588233727, 0.7999999999999999334, 0.8058823529411763831, 0.8117647058823528328, 0.8176470588235292825, 0.8235294117647057321 ),
 .UNSPECIFIED. ) 
 CURVE ( )  GEOMETRIC_REPRESENTATION_ITEM ( )  RATIONAL_B_SPLINE_CURVE ( ( 1.000000000000000888, 0.9510565162951526430, 1.000000000000000000, 0.9510565162951535312, 1.000000000000000000, 0.9510565162951535312, 1.000000000000000000, 0.9510565162951535312, 1.000000000000000000, 0.9510565162951544194, 0.9999999999999991118 ) ) 
 REPRESENTATION_ITEM ( '' )  );
#69224 = DIRECTION ( 'NONE',  ( 0.000000000000000000, 0.000000000000000000, -1.000000000000000000 ) ) ;
#69225 = CARTESIAN_POINT ( 'NONE',  ( 30.25000000000002842, 3.498359009886561184E-14, 4.000000000000000000 ) ) ;
#69226 = CARTESIAN_POINT ( 'NONE',  ( 24.00000000000000000, 0.000000000000000000, 4.000000000000000000 ) ) ;
#69227 = EDGE_LOOP ( 'NONE', ( #39033, #40814, #30664, #2003 ) ) ;
#69228 = ORIENTED_EDGE ( 'NONE', *, *, #24142, .F. ) ;
#69229 = CARTESIAN_POINT ( 'NONE',  ( -10.74999999999999645, 4.336808689942018722E-16, 20.00000000000000000 ) ) ;
#69230 = DIRECTION ( 'NONE',  ( 1.000000000000000000, 0.000000000000000000, 0.000000000000000000 ) ) ;
#69231 = CARTESIAN_POINT ( 'NONE',  ( -170.4570736234661865, -9.058813317711329915, 2.943386871421371787 ) ) ;
#69232 = CARTESIAN_POINT ( 'NONE',  ( 2.607480562269034241, 114.9070736234661467, -8.025000000000032330 ) ) ;
#69234 = ORIENTED_EDGE ( 'NONE', *, *, #46357, .F. ) ;
#69233 = AXIS2_PLACEMENT_3D ( 'NONE', #16532, #37994, #59377 ) ;
#69235 = CARTESIAN_POINT ( 'NONE',  ( -170.1550000000000011, 7.632228543268600340, 2.479861379858949277 ) ) ;
#69236 = CYLINDRICAL_SURFACE ( 'NONE', #21748, 9.524999999999991473 ) ;
#69237 = CARTESIAN_POINT ( 'NONE',  ( 21.25000000000001066, 24.74999999999998224, 3.750000000000000000 ) ) ;
#69238 = CARTESIAN_POINT ( 'NONE',  ( -181.7949999999999875, 2.607480562269068880, -8.024999999999993250 ) ) ;
#69239 = VECTOR ( 'NONE', #24378, 1000.000000000000000 ) ;
#69240 = CARTESIAN_POINT ( 'NONE',  ( -170.8449999999999989, -7.632228543268599452, 2.479861379858951054 ) ) ;
#69241 = AXIS2_PLACEMENT_3D ( 'NONE', #8213, #29659, #2146 ) ;
#69242 = EDGE_LOOP ( 'NONE', ( #16853, #67396, #37305, #9587 ) ) ;
#69243 = DIRECTION ( 'NONE',  ( 0.000000000000000000, 1.000000000000000000, 0.000000000000000000 ) ) ;
#69244 = DIRECTION ( 'NONE',  ( 0.000000000000000000, -0.000000000000000000, -1.000000000000000000 ) ) ;
#69245 = CARTESIAN_POINT ( 'NONE',  ( -10.16325816446478569, 11.93274896293544884, 1.310308443953213997 ) ) ;
#69246 = CARTESIAN_POINT ( 'NONE',  ( -80.45499999999998408, 7.632228543268599452, -2.479861379858951942 ) ) ;
#69247 = CARTESIAN_POINT ( 'NONE',  ( 72.00000000000000000, 14.49137674618942562, 7.500000000000000000 ) ) ;
#69248 = DIRECTION ( 'NONE',  ( 1.000000000000000000, -0.000000000000000000, -0.000000000000000000 ) ) ;
#69249 = CARTESIAN_POINT ( 'NONE',  ( -81.59499999999997044, 2.607480562269072433, 8.024999999999991473 ) ) ;
#69250 = CARTESIAN_POINT ( 'NONE',  ( 0.000000000000000000, 131.5549999999999784, -9.525000000000000355 ) ) ;
#69251 = LINE ( 'NONE', #30902, #12838 ) ;
#69252 = CARTESIAN_POINT ( 'NONE',  ( -171.2929263765339556, 3.094860106615688888, -9.525000000001982770 ) ) ;
#69253 = UNCERTAINTY_MEASURE_WITH_UNIT (LENGTH_MEASURE( 1.000000000000000082E-05 ), #40089, 'distance_accuracy_value', 'NONE');
#69254 = CARTESIAN_POINT ( 'NONE',  ( -41.49999999999998579, 99.99999999999998579, -3.500000000000000000 ) ) ;
#69255 = PRESENTATION_STYLE_ASSIGNMENT (( #48873 ) ) ;
#69256 = ORIENTED_EDGE ( 'NONE', *, *, #65764, .T. ) ;
#69257 = ADVANCED_FACE ( 'NONE', ( #55561 ), #8763, .T. ) ;
#69258 = CARTESIAN_POINT ( 'NONE',  ( 72.00000000000000000, 14.49137674618942562, -7.000000000000000000 ) ) ;
#69259 = EDGE_CURVE ( 'NONE', #62684, #14708, #46802, .T. ) ;
#69260 =( GEOMETRIC_REPRESENTATION_CONTEXT ( 3 ) GLOBAL_UNCERTAINTY_ASSIGNED_CONTEXT ( ( #22094 ) ) GLOBAL_UNIT_ASSIGNED_CONTEXT ( ( #13215, #13563, #30087 ) ) REPRESENTATION_CONTEXT ( 'NONE', 'WORKASPACE' ) );
#69261 = ADVANCED_FACE ( 'NONE', ( #19296 ), #9820, .F. ) ;
#69262 = DIRECTION ( 'NONE',  ( 2.168404344971007882E-16, 0.000000000000000000, 1.000000000000000000 ) ) ;
#69263 = EDGE_CURVE ( 'NONE', #56915, #13621, #26938, .T. ) ;
#69265 = LINE ( 'NONE', #47506, #1074 ) ;
#69264 = DIRECTION ( 'NONE',  ( -0.000000000000000000, -0.000000000000000000, 1.000000000000000000 ) ) ;
#69266 = AXIS2_PLACEMENT_3D ( 'NONE', #57788, #10971, #12006 ) ;
#69267 = CARTESIAN_POINT ( 'NONE',  ( -7.632228543268607446, 136.6570736234661467, -2.479861379858953718 ) ) ;
#69268 = ORIENTED_EDGE ( 'NONE', *, *, #25502, .F. ) ;
#69269 = VERTEX_POINT ( 'NONE', #19658 ) ;
#69270 = FACE_OUTER_BOUND ( 'NONE', #32749, .T. ) ;
#69271 = LINE ( 'NONE', #36938, #29707 ) ;
#69272 = SURFACE_STYLE_USAGE ( .BOTH. , #53097 ) ;
#69273 = LINE ( 'NONE', #47517, #14986 ) ;
#69274 = CARTESIAN_POINT ( 'NONE',  ( -8.252730563585672030, -2.464278740834326520, 3.705851362693083573 ) ) ;
#69275 = EDGE_CURVE ( 'NONE', #41197, #52602, #20243, .T. ) ;
#69276 = ORIENTED_EDGE ( 'NONE', *, *, #36740, .F. ) ;
#69277 = CARTESIAN_POINT ( 'NONE',  ( -123.8049999999999784, -8.437984349512086979, 5.166775262442717831E-16 ) ) ;
#69278 = ORIENTED_EDGE ( 'NONE', *, *, #18275, .T. ) ;
#69279 = AXIS2_PLACEMENT_3D ( 'NONE', #33619, #838, #33289 ) ;
#69280 =( LENGTH_UNIT ( ) NAMED_UNIT ( * ) SI_UNIT ( .MILLI., .METRE. ) );
#69281 = ORIENTED_EDGE ( 'NONE', *, *, #28702, .F. ) ;
#69282 = DIRECTION ( 'NONE',  ( -1.000000000000000000, -0.000000000000000000, -0.000000000000000000 ) ) ;
#69283 = SURFACE_STYLE_USAGE ( .BOTH. , #68587 ) ;
#69284 = VERTEX_POINT ( 'NONE', #41154 ) ;
#69285 = DIRECTION ( 'NONE',  ( 0.000000000000000000, 0.000000000000000000, 1.000000000000000000 ) ) ;
#69286 = B_SPLINE_CURVE_WITH_KNOTS ( 'NONE', 3,
 ( #51796, #24340, #24675, #41264, #63378, #8871, #41603, #13801 ),
 .UNSPECIFIED., .F., .F.,
 ( 4, 2, 2, 4 ),
 ( 0.000000000000000000, 0.0001769990489079868224, 0.0003539980978159736448, 0.0007079961956319273404 ),
 .UNSPECIFIED. ) ;
#69287 = CARTESIAN_POINT ( 'NONE',  ( 10.01517768586949231, 150.6949999999999648, 1.839758294383810543E-15 ) ) ;
#69288 = DIRECTION ( 'NONE',  ( 0.000000000000000000, -1.000000000000000000, 0.000000000000000000 ) ) ;
#69289 = VERTEX_POINT ( 'NONE', #47485 ) ;
#69290 = DIRECTION ( 'NONE',  ( 1.000000000000000000, 0.000000000000000000, -0.000000000000000000 ) ) ;
#69291 = CARTESIAN_POINT ( 'NONE',  ( 9.058813317711338797, 151.9550000000000125, -2.943386871421372675 ) ) ;
#69292 = CARTESIAN_POINT ( 'NONE',  ( -9.827790563157511022E-16, 131.5570736234661524, 8.025000000000000355 ) ) ;
#69293 = CARTESIAN_POINT ( 'NONE',  ( 5.705565085145809512, 2.472216779103305395, 4.117671386636410524 ) ) ;
#69294 = ORIENTED_EDGE ( 'NONE', *, *, #11023, .F. ) ;
#69295 = CARTESIAN_POINT ( 'NONE',  ( 4.716976649647099507, 128.6429263765338362, -6.492361379858953008 ) ) ;
#69296 = CARTESIAN_POINT ( 'NONE',  ( 45.65811388300841855, 10.21937129433612235, -4.000000000000000000 ) ) ;
#69297 = UNCERTAINTY_MEASURE_WITH_UNIT (LENGTH_MEASURE( 1.000000000000000082E-05 ), #28097, 'distance_accuracy_value', 'NONE');
#69298 = VECTOR ( 'NONE', #49074, 1000.000000000000000 ) ;
#69299 = PRESENTATION_STYLE_ASSIGNMENT (( #34162 ) ) ;
#69300 = EDGE_CURVE ( 'NONE', #66633, #16901, #33457, .T. ) ;
#69301 = ORIENTED_EDGE ( 'NONE', *, *, #23410, .T. ) ;
#69302 = DIRECTION ( 'NONE',  ( 1.000000000000000000, 0.000000000000000000, 0.000000000000000000 ) ) ;
#69303 = ORIENTED_EDGE ( 'NONE', *, *, #21282, .F. ) ;
#69304 = CARTESIAN_POINT ( 'NONE',  ( -61.64292637653380780, -5.598654528085801552, 7.705886871421367523 ) ) ;
#69305 = FACE_OUTER_BOUND ( 'NONE', #34443, .T. ) ;
#69306 = CARTESIAN_POINT ( 'NONE',  ( -156.5050000000000239, -6.826472737025115478, -4.959722759717899443 ) ) ;
#69307 = CARTESIAN_POINT ( 'NONE',  ( -24.21231517720798010, 117.4999999999999716, -7.000000000000000000 ) ) ;
#69308 = EDGE_CURVE ( 'NONE', #1270, #19619, #59028, .T. ) ;
#69309 = UNCERTAINTY_MEASURE_WITH_UNIT (LENGTH_MEASURE( 1.000000000000000082E-05 ), #59714, 'distance_accuracy_value', 'NONE');
#69310 = CARTESIAN_POINT ( 'NONE',  ( 48.74999999999999289, 24.99999999999998579, 3.750000000000000000 ) ) ;
#69311 = CARTESIAN_POINT ( 'NONE',  ( 0.000000000000000000, 154.9999999999999716, 0.000000000000000000 ) ) ;
#69312 = CARTESIAN_POINT ( 'NONE',  ( 40.95866658621363854, 108.0312444614856986, 3.562488397567471932 ) ) ;
#69313 =( LENGTH_UNIT ( ) NAMED_UNIT ( * ) SI_UNIT ( .MILLI., .METRE. ) );
#69314 = EDGE_LOOP ( 'NONE', ( #32737, #11904, #65283, #66996, #2307, #61791, #33300, #3506, #13305, #32107, #18758, #35308, #45764, #39098, #23080, #30075, #6988, #42760, #17832 ) ) ;
#69315 = ORIENTED_EDGE ( 'NONE', *, *, #3028, .F. ) ;
#69316 = CARTESIAN_POINT ( 'NONE',  ( 23.49527607712185073, 27.44009427658185984, 27.19000446309344809 ) ) ;
#69317 = STYLED_ITEM ( 'NONE', ( #12440 ), #65354 ) ;
#69318 = DIRECTION ( 'NONE',  ( -0.000000000000000000, 0.000000000000000000, -1.000000000000000000 ) ) ;
#69319 = CARTESIAN_POINT ( 'NONE',  ( -66.35499999999998977, -4.716976649647093289, -6.492361379858945902 ) ) ;
#69320 = EDGE_LOOP ( 'NONE', ( #41908, #13834 ) ) ;
#69321 = FILL_AREA_STYLE ('',( #63682 ) ) ;
#69322 = DIRECTION ( 'NONE',  ( 0.000000000000000000, 0.000000000000000000, -1.000000000000000000 ) ) ;
#69323 = AXIS2_PLACEMENT_3D ( 'NONE', #2442, #56300, #13053 ) ;
#69324 = DIRECTION ( 'NONE',  ( 7.080503983578803083E-17, 1.000000000000000000, -0.000000000000000000 ) ) ;
#69325 = VECTOR ( 'NONE', #61046, 1000.000000000000000 ) ;
#69326 = DIRECTION ( 'NONE',  ( -1.000000000000000000, -2.168404344971008868E-16, 0.000000000000000000 ) ) ;
#69327 = ORIENTED_EDGE ( 'NONE', *, *, #64085, .F. ) ;
#69328 =( NAMED_UNIT ( * ) PLANE_ANGLE_UNIT ( ) SI_UNIT ( $, .RADIAN. ) );
#69329 = CARTESIAN_POINT ( 'NONE',  ( -45.00000000000000000, 10.49999999999998224, -4.000000000000000000 ) ) ;
#69330 = LINE ( 'NONE', #26399, #62262 ) ;
#69331 = CARTESIAN_POINT ( 'NONE',  ( 4.716976649647099507, 126.7570736234661695, -6.492361379858953008 ) ) ;
#69332 = VECTOR ( 'NONE', #43396, 1000.000000000000000 ) ;
#69333 = CARTESIAN_POINT ( 'NONE',  ( -121.3449999999999989, 7.632228543268599452, -2.479861379858951942 ) ) ;
#69334 = CARTESIAN_POINT ( 'NONE',  ( -8.102448949553181734, 152.4949999999999477, 5.886773742842747126 ) ) ;
#69335 = CARTESIAN_POINT ( 'NONE',  ( -89.69499999999999318, -8.437984349512085203, 5.166775262442717831E-16 ) ) ;
#69336 = EDGE_CURVE ( 'NONE', #49467, #5853, #9055, .T. ) ;
#69337 = DIRECTION ( 'NONE',  ( -1.000000000000000000, 0.000000000000000000, 0.000000000000000000 ) ) ;
#69338 = CARTESIAN_POINT ( 'NONE',  ( 12.75000000000000533, 28.24999999999998224, -3.750000000000000000 ) ) ;
#69339 = UNCERTAINTY_MEASURE_WITH_UNIT (LENGTH_MEASURE( 1.000000000000000082E-05 ), #27121, 'distance_accuracy_value', 'NONE');
#69340 = SURFACE_SIDE_STYLE ('',( #43356 ) ) ;
#69341 = VERTEX_POINT ( 'NONE', #21378 ) ;
#69342 = CARTESIAN_POINT ( 'NONE',  ( -129.5929263765338249, -3.094860106618431139, -9.524999999999991473 ) ) ;
#69343 = DIRECTION ( 'NONE',  ( -0.000000000000000000, 1.000000000000000000, -0.000000000000000000 ) ) ;
#69344 = CARTESIAN_POINT ( 'NONE',  ( -147.1450000000000102, -4.716976649647092401, 6.492361379858946790 ) ) ;
#69345 = DIRECTION ( 'NONE',  ( 0.000000000000000000, 0.000000000000000000, 1.000000000000000000 ) ) ;
#69346 = EDGE_CURVE ( 'NONE', #24587, #41886, #21738, .T. ) ;
#69347 = SURFACE_SIDE_STYLE ('',( #25040 ) ) ;
#69348 = DIRECTION ( 'NONE',  ( 0.000000000000000000, 0.000000000000000000, -1.000000000000000000 ) ) ;
#69349 = EDGE_LOOP ( 'NONE', ( #11293, #36860, #36703, #41368 ) ) ;
#69350 = ORIENTED_EDGE ( 'NONE', *, *, #26651, .T. ) ;
#69351 = FACE_OUTER_BOUND ( 'NONE', #62342, .T. ) ;
#69352 = CARTESIAN_POINT ( 'NONE',  ( -75.00000000000000000, -2.215169945516535778E-14, 10.00000000000000000 ) ) ;
#69353 = DIRECTION ( 'NONE',  ( -1.000000000000000000, -0.000000000000000000, -0.000000000000000000 ) ) ;
#69354 = CARTESIAN_POINT ( 'NONE',  ( -129.8070736234661240, 10.01517768586948698, -1.839758294383808966E-15 ) ) ;
#69355 = CIRCLE ( 'NONE', #39061, 0.2500000000000002220 ) ;
#69356 = CARTESIAN_POINT ( 'NONE',  ( 44.99999999999977973, 149.9999999999999716, 10.00000000000000000 ) ) ;
#69357 = AXIS2_PLACEMENT_3D ( 'NONE', #36203, #62881, #19274 ) ;
#69358 = EDGE_CURVE ( 'NONE', #44514, #23604, #59705, .T. ) ;
#69359 = ORIENTED_EDGE ( 'NONE', *, *, #63228, .T. ) ;
#69360 = CARTESIAN_POINT ( 'NONE',  ( -149.9050000000000011, 2.607480562269069324, -8.024999999999993250 ) ) ;
#69361 = VECTOR ( 'NONE', #31999, 1000.000000000000000 ) ;
#69362 = VERTEX_POINT ( 'NONE', #59342 ) ;
#69363 = DIRECTION ( 'NONE',  ( 0.000000000000000000, 0.000000000000000000, -1.000000000000000000 ) ) ;
#69364 = FACE_OUTER_BOUND ( 'NONE', #38381, .T. ) ;
#69365 = VERTEX_POINT ( 'NONE', #10840 ) ;
#69366 = FILL_AREA_STYLE ('',( #26433 ) ) ;
#69367 = CARTESIAN_POINT ( 'NONE',  ( -55.00000000000000000, -2.024042244987997205E-14, -12.00000000000000000 ) ) ;
#69368 = CARTESIAN_POINT ( 'NONE',  ( 8.102448949553181734, 123.3949999999999676, 5.886773742842750679 ) ) ;
#69369 = DIRECTION ( 'NONE',  ( -1.000000000000000000, 0.000000000000000000, 0.000000000000000000 ) ) ;
#69370 = ORIENTED_EDGE ( 'NONE', *, *, #19140, .F. ) ;
#69371 = DIRECTION ( 'NONE',  ( -0.000000000000000000, -0.000000000000000000, -1.000000000000000000 ) ) ;
#69372 = CARTESIAN_POINT ( 'NONE',  ( 0.000000000000000000, 125.5550000000000068, -9.525000000000000355 ) ) ;
#69373 = CARTESIAN_POINT ( 'NONE',  ( -61.40499999999998693, -2.607480562269069768, 8.024999999999991473 ) ) ;
#69374 = CARTESIAN_POINT ( 'NONE',  ( -123.1449999999999960, -4.716976649647092401, 6.492361379858946790 ) ) ;
#69375 = CARTESIAN_POINT ( 'NONE',  ( -75.00000000000000000, -2.215169945516535778E-14, -6.500000000000000888 ) ) ;
#69376 = VERTEX_POINT ( 'NONE', #5199 ) ;
#69377 = CARTESIAN_POINT ( 'NONE',  ( 8.102448949553183510, 152.1049999999999613, -5.886773742842746238 ) ) ;
#69378 = UNCERTAINTY_MEASURE_WITH_UNIT (LENGTH_MEASURE( 1.000000000000000082E-05 ), #7476, 'distance_accuracy_value', 'NONE');
#69379 = COLOUR_RGB ( '', 0.31764706, 0.68627451, 0.89019608) ;
#69380 = DIRECTION ( 'NONE',  ( -1.189524669241239115E-16, -1.000000000000000000, -0.000000000000000000 ) ) ;
#69381 = AXIS2_PLACEMENT_3D ( 'NONE', #27029, #10888, #58379 ) ;
#69382 = CARTESIAN_POINT ( 'NONE',  ( 6.062177826491068622, 2.500000000000000000, -3.500000000000001332 ) ) ;
#69383 = DIRECTION ( 'NONE',  ( -0.000000000000000000, 0.000000000000000000, 1.000000000000000000 ) ) ;
#69384 = DIRECTION ( 'NONE',  ( 1.000000000000000000, 0.000000000000000000, 0.000000000000000000 ) ) ;
#69385 = ORIENTED_EDGE ( 'NONE', *, *, #31051, .F. ) ;
#69386 = CARTESIAN_POINT ( 'NONE',  ( -180.0550000000000068, -9.827790563157499189E-16, -8.024999999999991473 ) ) ;
#69387 = EDGE_LOOP ( 'NONE', ( #47250, #5409, #540, #7072 ) ) ;
#69388 = FACE_OUTER_BOUND ( 'NONE', #8402, .T. ) ;
#69389 =( REPRESENTATION_RELATIONSHIP ('NONE','NONE', #5102, #22166 ) REPRESENTATION_RELATIONSHIP_WITH_TRANSFORMATION ( #19844 )SHAPE_REPRESENTATION_RELATIONSHIP( ) );
#69390 = SURFACE_STYLE_FILL_AREA ( #36382 ) ;
#69391 = EDGE_LOOP ( 'NONE', ( #24210, #25993, #51388, #4300 ) ) ;
#69392 = LINE ( 'NONE', #43410, #14069 ) ;
#69393 = SURFACE_STYLE_USAGE ( .BOTH. , #58150 ) ;
#69394 = ORIENTED_EDGE ( 'NONE', *, *, #41920, .T. ) ;
#69395 = CARTESIAN_POINT ( 'NONE',  ( -128.9070736234668857, -3.094860106607204120, 9.525000000008148504 ) ) ;
#69396 = CARTESIAN_POINT ( 'NONE',  ( -90.50499999999999545, -6.826472737025115478, -4.959722759717899443 ) ) ;
#69397 = VERTEX_POINT ( 'NONE', #5527 ) ;
#69398 = SURFACE_STYLE_USAGE ( .BOTH. , #31054 ) ;
#69399 =( NAMED_UNIT ( * ) SI_UNIT ( $, .STERADIAN. ) SOLID_ANGLE_UNIT ( ) );
#69400 = CARTESIAN_POINT ( 'NONE',  ( -131.9070736234661751, -3.094860106618429807, 9.524999999999991473 ) ) ;
#69401 = FILL_AREA_STYLE ('',( #26475 ) ) ;
#69402 = DIRECTION ( 'NONE',  ( 0.000000000000000000, 0.000000000000000000, 1.000000000000000000 ) ) ;
#69403 = CARTESIAN_POINT ( 'NONE',  ( -68.00707362346616947, -8.102448949553172852, -5.886773742842741797 ) ) ;
#69404 = AXIS2_PLACEMENT_3D ( 'NONE', #50894, #36120, #19203 ) ;
#69405 = ORIENTED_EDGE ( 'NONE', *, *, #47226, .T. ) ;
#69406 = SURFACE_STYLE_FILL_AREA ( #53243 ) ;
#69407 = AXIS2_PLACEMENT_3D ( 'NONE', #56388, #30329, #51832 ) ;
#69409 = SURFACE_STYLE_FILL_AREA ( #11001 ) ;
#69408 = CARTESIAN_POINT ( 'NONE',  ( 6.123233995736766282E-16, 2.299999999999999822, 5.000000000000000000 ) ) ;
#69410 = VECTOR ( 'NONE', #29044, 1000.000000000000000 ) ;
#69411 = CARTESIAN_POINT ( 'NONE',  ( -116.1550000000000011, 7.632228543268600340, 2.479861379858949277 ) ) ;
#69412 = CARTESIAN_POINT ( 'NONE',  ( -9.058813317711338797, 122.3449999999999847, 2.943386871421373563 ) ) ;
#69413 = CARTESIAN_POINT ( 'NONE',  ( -120.5949999999999704, 2.607480562269073321, 8.024999999999991473 ) ) ;
#69414 = ADVANCED_FACE ( 'NONE', ( #15790 ), #31587, .F. ) ;
#69415 = DIRECTION ( 'NONE',  ( -1.000000000000000000, 0.000000000000000000, 0.000000000000000000 ) ) ;
#69416 =( BOUNDED_SURFACE ( )  B_SPLINE_SURFACE ( 1, 2, ( 
 ( #45572, #40617, #40979, #61665, #29694, #8933, #30353, #3604, #62397, #61342, #56781, #8596, #35327, #3250, #68042, #25108, #62721, #24738, #8252, #55736, #2908, #50460, #46624, #14214, #18457, #29330, #24400, #34607, #45894, #2188, #30030, #23718, #19828, #45216, #39940, #41318, #13152, #7882, #50809, #63442, #58169, #9291, #69077, #15289, #20879, #21563, #48336, #4683, #30711, #31760, #26136, #25791, #9985, #42037, #41668, #3979, #68371, #36024, #36753, #47306, #47673, #10330, #42383, #68732, #63773, #25450, #57824, #20528, #9652, #31404, #32121, #26485, #52898, #15621, #37096, #53249, #52218, #63086, #58506, #46964, #64122, #5035, #14925, #57466, #4308, #48010, #69412, #37456, #21201, #42724, #43075, #15974, #58860, #36410, #53574, #10667, #20162, #31067, #5361, #14550, #26802, #52563, #28, #6753, #59176, #28183, #39161, #54928, #54252, #27507, #38489, #50048, #49694, #44110, #22607, #27841, #12370, #6073, #1063, #1428, #32813, #59881, #60552, #33833, #55295, #22957, #21922, #17358, #38824, #65506, #12036, #28546, #7117, #23294, #44459, #49034, #64481, #723, #11003, #1784, #33496, #48687, #59524, #33169, #64817, #54604, #32441, #22255, #16325, #37801, #53902, #5708, #16997, #49343, #65863, #393, #43433, #43751, #27157, #60237, #65152, #16664, #38129, #11699, #17693, #11344, #6409, #61953, #34200, #39503, #14135, #3518, #2832, #44791, #30272, #56697, #60911, #8517, #19394, #35237, #34530, #7796, #18713, #51770, #29952, #24325, #45817, #8164, #62313, #55989, #51079, #51417, #13077, #40186, #40891, #35595, #57033, #3161, #2105, #67241, #19027, #40539, #13779, #8852, #66189, #18012, #24652, #29243, #12728, #50725, #55651, #7467, #46169, #28892, #39863, #13417, #45136, #34881, #50377, #2470, #23628, #66554, #18377, #61267, #66911, #29605, #67596, #23981, #45495, #61587, #56328, #52820, #25700, #37365, #57385, #4224, #14461, #41240, #58421, #47221, #68639, #19744, #9906, #20444, #31322, #32037, #58771, #15207, #62639, #42308, #36674, #36315, #41946, #52486, #52136, #35940, #9210, #46534, #63352, #57739, #58095, #20801, #4595, #9570, #26054, #30628, #68290, #30988, #20076, #47588, #42632, #37013, #68995, #63696, #15540, #10247, #3891, #25367, #31684, #46889, #4954, #53160, #41576, #67959, #14838, #26402, #47933, #69334, #21128, #64037, #15881, #62997, #10588, #53498, #25024, #65431, #44374, #6329, #54846, #65779, #59432, #42987, #11263, #21835, #17280, #59804, #38744, #16918, #64391, #17615, #10926, #54519, #33754, #33082, #60151, #39081, #48248, #11615, #65064, #22874, #69663, #59107, #5281, #32361, #26726, #32718, #648, #27760, #60475, #11960, #28105, #43347, #27422, #22523, #6665, #21477, #49264, #44021, #973, #49610, #5621 ),
 ( #48950, #38401, #33417, #1344, #12283, #16239, #37717, #22176, #53822, #43671, #27073, #48608, #301, #54173, #64742, #16585, #38040, #5983, #23543, #55911, #12996, #49965, #66829, #18637, #2377, #7386, #45053, #45743, #34792, #8435, #23896, #3078, #56605, #2018, #1702, #7027, #44713, #34451, #40117, #17932, #23219, #56244, #28817, #67160, #61505, #29521, #61187, #13333, #67501, #28454, #18946, #29152, #8069, #50985, #66463, #40449, #7713, #66103, #29868, #61865, #39422, #2750, #40806, #50638, #24242, #35150, #62221, #19301, #45409, #60823, #13691, #51333, #18287, #24569, #46082, #12643, #34107, #55565, #50299, #14047, #39772, #55204, #31233, #41852, #68211, #63273, #62904, #35847, #46443, #30541, #57650, #53073, #47490, #14748, #15118, #36223, #4496, #51682, #62558, #19987, #3428, #15458, #41488, #14376, #56950, #25284, #25614, #36595, #58333, #52398, #4144, #42546, #46806, #52728, #57291, #4867, #25961, #24931, #30189, #26310, #63946, #58013, #35507, #21050, #68913, #67868, #20711, #10158, #42224, #9477, #30900, #47127, #8768, #63615, #9823, #36921, #68553, #47855, #20350, #31591, #69250, #3798, #19661, #41157, #9123, #52043, #49186, #42905, #38307, #59711, #64980, #32995, #49527, #6573, #44288, #6250, #212, #15793, #21743, #31945, #33338, #54430, #69577, #10843, #54085, #16150, #5893, #53422, #43254, #37277, #54760, #58675, #5201, #37970, #565, #27675, #21382, #64298, #64660, #28018, #43592, #16504, #1256, #48170, #59346, #26645, #37628, #888, #11176, #32624, #10507, #22090, #27336, #16836, #22429, #48866, #59032, #43930, #11524, #32287, #65340, #17190, #38662, #60060, #11875, #22787, #53738, #5532, #26982, #48515, #7984, #39677, #18191, #50218, #2662, #6941, #28367, #45314, #34018, #66370, #23457, #60395, #7628, #29062, #12909, #17853, #55479, #56157, #66736, #18863, #34374, #13595, #67078, #12552, #12198, #17532, #55114, #44963, #50560, #49874, #33672, #18551, #39331, #29428, #2283, #40036, #1940, #23812, #8347, #39002, #50899, #61099, #61425, #13246, #7301, #24157, #55823, #1613, #40357, #45662, #23139, #34701, #51252, #61766, #35062, #56509, #28730, #60734, #29792, #24483, #2993, #65684, #44629, #66026, #25882, #15382, #30451, #13957, #51952, #62482, #36503, #30817, #57926, #57562, #35425, #58251, #51591, #25533, #4779, #4069, #9746, #10075, #19210, #52316, #36127, #63529, #40720, #30113, #45990, #3346, #67415, #3709, #41415, #47047, #36837, #52647, #68827, #14301, #68133, #63188, #47399, #62130, #20262, #15029, #41767, #20621, #56875, #8686, #31499, #19912, #24840, #46355, #25203, #67775, #19575, #31153, #46720, #62818, #41068, #68466, #14658, #4406, #52986, #35765, #9394, #57201, #42134, #9033, #37552, #126, #53660 ) ),
 .UNSPECIFIED., .F., .F., .F. ) 
 B_SPLINE_SURFACE_WITH_KNOTS ( ( 2, 2 ),
 ( 3, 2, 2, 2, 2, 2, 2, 2, 2, 2, 2, 2, 2, 2, 2, 2, 2, 2, 2, 2, 2, 2, 2, 2, 2, 2, 2, 2, 2, 2, 2, 2, 2, 2, 2, 2, 2, 2, 2, 2, 2, 2, 2, 2, 2, 2, 2, 2, 2, 2, 2, 2, 2, 2, 2, 2, 2, 2, 2, 2, 2, 2, 2, 2, 2, 2, 2, 2, 2, 2, 2, 2, 2, 2, 2, 2, 2, 2, 2, 2, 2, 2, 2, 2, 2, 2, 2, 2, 2, 2, 2, 2, 2, 2, 2, 2, 2, 2, 2, 2, 2, 2, 2, 2, 2, 2, 2, 2, 2, 2, 2, 2, 2, 2, 2, 2, 2, 2, 2, 2, 2, 2, 2, 2, 2, 2, 2, 2, 2, 2, 2, 2, 2, 2, 2, 2, 2, 2, 2, 2, 2, 2, 2, 2, 2, 2, 2, 2, 2, 2, 2, 2, 2, 2, 2, 2, 2, 2, 2, 2, 2, 2, 2, 2, 2, 2, 2, 2, 2, 2, 3 ),
 ( 0.000000000000000000, 1.000000000000000000 ),
 ( 0.000000000000000000, 0.005882352941176470507, 0.01176470588235294101, 0.01764705882352941152, 0.02352941176470588203, 0.02941176470588235253, 0.03529411764705882304, 0.04117647058823529355, 0.04705882352941176405, 0.05294117647058823456, 0.05882352941176470507, 0.06470588235294118251, 0.07058823529411764608, 0.07647058823529412352, 0.08235294117647058709, 0.08823529411764706454, 0.09411764705882352811, 0.1000000000000000056, 0.1058823529411764691, 0.1117647058823529466, 0.1176470588235294101, 0.1235294117647058876, 0.1294117647058823650, 0.1352941176470588147, 0.1411764705882352922, 0.1470588235294117696, 0.1529411764705882470, 0.1588235294117646967, 0.1647058823529411742, 0.1705882352941176516, 0.1764705882352941291, 0.1823529411764705788, 0.1882352941176470562, 0.1941176470588235337, 0.2000000000000000111, 0.2058823529411764608, 0.2117647058823529382, 0.2176470588235294157, 0.2235294117647058931, 0.2294117647058823428, 0.2352941176470588203, 0.2411764705882352977, 0.2470588235294117752, 0.2529411764705882248, 0.2588235294117647300, 0.2647058823529411797, 0.2705882352941176294, 0.2764705882352941346, 0.2823529411764705843, 0.2882352941176470340, 0.2941176470588235392, 0.2999999999999999889, 0.3058823529411764941, 0.3117647058823529438, 0.3176470588235293935, 0.3235294117647058987, 0.3294117647058823484, 0.3352941176470587981, 0.3411764705882353033, 0.3470588235294117530, 0.3529411764705882582, 0.3588235294117647078, 0.3647058823529411575, 0.3705882352941176627, 0.3764705882352941124, 0.3823529411764705621, 0.3882352941176470673, 0.3941176470588235170, 0.4000000000000000222, 0.4058823529411764719, 0.4117647058823529216, 0.4176470588235294268, 0.4235294117647058765, 0.4294117647058823262, 0.4352941176470588314, 0.4411764705882352811, 0.4470588235294117863, 0.4529411764705882359, 0.4588235294117646856, 0.4647058823529411908, 0.4705882352941176405, 0.4764705882352940902, 0.4823529411764705954, 0.4882352941176470451, 0.4941176470588235503, 0.5000000000000000000, 0.5058823529411764497, 0.5117647058823528994, 0.5176470588235294601, 0.5235294117647059098, 0.5294117647058823595, 0.5352941176470588092, 0.5411764705882352589, 0.5470588235294118196, 0.5529411764705882693, 0.5588235294117647189, 0.5647058823529411686, 0.5705882352941176183, 0.5764705882352940680, 0.5823529411764706287, 0.5882352941176470784, 0.5941176470588235281, 0.5999999999999999778, 0.6058823529411764275, 0.6117647058823529882, 0.6176470588235294379, 0.6235294117647058876, 0.6294117647058823373, 0.6352941176470587870, 0.6411764705882353477, 0.6470588235294117974, 0.6529411764705882470, 0.6588235294117646967, 0.6647058823529411464, 0.6705882352941175961, 0.6764705882352941568, 0.6823529411764706065, 0.6882352941176470562, 0.6941176470588235059, 0.6999999999999999556, 0.7058823529411765163, 0.7117647058823529660, 0.7176470588235294157, 0.7235294117647058654, 0.7294117647058823151, 0.7352941176470588758, 0.7411764705882353255, 0.7470588235294117752, 0.7529411764705882248, 0.7588235294117646745, 0.7647058823529411242, 0.7705882352941176849, 0.7764705882352941346, 0.7823529411764705843, 0.7882352941176470340, 0.7941176470588234837, 0.8000000000000000444, 0.8058823529411764941, 0.8117647058823529438, 0.8176470588235293935, 0.8235294117647058432, 0.8294117647058824039, 0.8352941176470588536, 0.8411764705882353033, 0.8470588235294117530, 0.8529411764705882026, 0.8588235294117646523, 0.8647058823529412130, 0.8705882352941176627, 0.8764705882352941124, 0.8823529411764705621, 0.8882352941176470118, 0.8941176470588235725, 0.9000000000000000222, 0.9058823529411764719, 0.9117647058823529216, 0.9176470588235293713, 0.9235294117647059320, 0.9294117647058823817, 0.9352941176470588314, 0.9411764705882352811, 0.9470588235294117307, 0.9529411764705881804, 0.9588235294117647411, 0.9647058823529411908, 0.9705882352941176405, 0.9764705882352940902, 0.9823529411764705399, 0.9882352941176471006, 0.9941176470588235503, 1.000000000000000000 ),
 .UNSPECIFIED. ) 
 GEOMETRIC_REPRESENTATION_ITEM ( )  RATIONAL_B_SPLINE_SURFACE ( (
 ( 1.000000000000000000, 0.9510565162951535312, 1.000000000000000000, 0.9510565162951535312, 1.000000000000000000, 0.9510565162951535312, 1.000000000000000000, 0.9510565162951535312, 1.000000000000000000, 0.9510565162951535312, 1.000000000000000000, 0.9510565162951535312, 1.000000000000000000, 0.9510565162951535312, 1.000000000000000000, 0.9510565162951535312, 1.000000000000000000, 0.9510565162951535312, 1.000000000000000000, 0.9510565162951535312, 1.000000000000000000, 0.9510565162951535312, 1.000000000000000000, 0.9510565162951535312, 1.000000000000000000, 0.9510565162951535312, 1.000000000000000000, 0.9510565162951535312, 1.000000000000000000, 0.9510565162951535312, 1.000000000000000000, 0.9510565162951535312, 1.000000000000000000, 0.9510565162951535312, 1.000000000000000000, 0.9510565162951535312, 1.000000000000000000, 0.9510565162951535312, 1.000000000000000000, 0.9510565162951535312, 1.000000000000000000, 0.9510565162951535312, 1.000000000000000000, 0.9510565162951535312, 1.000000000000000000, 0.9510565162951535312, 1.000000000000000000, 0.9510565162951535312, 1.000000000000000000, 0.9510565162951535312, 1.000000000000000000, 0.9510565162951535312, 1.000000000000000000, 0.9510565162951535312, 1.000000000000000000, 0.9510565162951535312, 1.000000000000000000, 0.9510565162951535312, 1.000000000000000000, 0.9510565162951535312, 1.000000000000000000, 0.9510565162951535312, 1.000000000000000000, 0.9510565162951535312, 1.000000000000000000, 0.9510565162951535312, 1.000000000000000000, 0.9510565162951535312, 1.000000000000000000, 0.9510565162951535312, 1.000000000000000000, 0.9510565162951535312, 1.000000000000000000, 0.9510565162951535312, 1.000000000000000000, 0.9510565162951535312, 1.000000000000000000, 0.9510565162951535312, 1.000000000000000000, 0.9510565162951535312, 1.000000000000000000, 0.9510565162951535312, 1.000000000000000000, 0.9510565162951535312, 1.000000000000000000, 0.9510565162951535312, 1.000000000000000000, 0.9510565162951535312, 1.000000000000000000, 0.9510565162951535312, 1.000000000000000000, 0.9510565162951535312, 1.000000000000000000, 0.9510565162951535312, 1.000000000000000000, 0.9510565162951535312, 1.000000000000000000, 0.9510565162951535312, 1.000000000000000000, 0.9510565162951535312, 1.000000000000000000, 0.9510565162951535312, 1.000000000000000000, 0.9510565162951535312, 1.000000000000000000, 0.9510565162951535312, 1.000000000000000000, 0.9510565162951535312, 1.000000000000000000, 0.9510565162951535312, 1.000000000000000000, 0.9510565162951535312, 1.000000000000000000, 0.9510565162951535312, 1.000000000000000000, 0.9510565162951535312, 1.000000000000000000, 0.9510565162951535312, 1.000000000000000000, 0.9510565162951535312, 1.000000000000000000, 0.9510565162951535312, 1.000000000000000000, 0.9510565162951535312, 1.000000000000000000, 0.9510565162951535312, 1.000000000000000000, 0.9510565162951535312, 1.000000000000000000, 0.9510565162951535312, 1.000000000000000000, 0.9510565162951535312, 1.000000000000000000, 0.9510565162951535312, 1.000000000000000000, 0.9510565162951535312, 1.000000000000000000, 0.9510565162951535312, 1.000000000000000000, 0.9510565162951535312, 1.000000000000000000, 0.9510565162951535312, 1.000000000000000000, 0.9510565162951535312, 1.000000000000000000, 0.9510565162951535312, 1.000000000000000000, 0.9510565162951535312, 1.000000000000000000, 0.9510565162951535312, 1.000000000000000000, 0.9510565162951535312, 1.000000000000000000, 0.9510565162951535312, 1.000000000000000000, 0.9510565162951535312, 1.000000000000000000, 0.9510565162951535312, 1.000000000000000000, 0.9510565162951535312, 1.000000000000000000, 0.9510565162951535312, 1.000000000000000000, 0.9510565162951535312, 1.000000000000000000, 0.9510565162951535312, 1.000000000000000000, 0.9510565162951535312, 1.000000000000000000, 0.9510565162951535312, 1.000000000000000000, 0.9510565162951535312, 1.000000000000000000, 0.9510565162951535312, 1.000000000000000000, 0.9510565162951535312, 1.000000000000000000, 0.9510565162951535312, 1.000000000000000000, 0.9510565162951535312, 1.000000000000000000, 0.9510565162951535312, 1.000000000000000000, 0.9510565162951535312, 1.000000000000000000, 0.9510565162951535312, 1.000000000000000000, 0.9510565162951535312, 1.000000000000000000, 0.9510565162951535312, 1.000000000000000000, 0.9510565162951535312, 1.000000000000000000, 0.9510565162951535312, 1.000000000000000000, 0.9510565162951535312, 1.000000000000000000, 0.9510565162951535312, 1.000000000000000000, 0.9510565162951535312, 1.000000000000000000, 0.9510565162951535312, 1.000000000000000000, 0.9510565162951535312, 1.000000000000000000, 0.9510565162951535312, 1.000000000000000000, 0.9510565162951535312, 1.000000000000000000, 0.9510565162951535312, 1.000000000000000000, 0.9510565162951535312, 1.000000000000000000, 0.9510565162951535312, 1.000000000000000000, 0.9510565162951535312, 1.000000000000000000, 0.9510565162951535312, 1.000000000000000000, 0.9510565162951535312, 1.000000000000000000, 0.9510565162951535312, 1.000000000000000000, 0.9510565162951535312, 1.000000000000000000, 0.9510565162951535312, 1.000000000000000000, 0.9510565162951535312, 1.000000000000000000, 0.9510565162951535312, 1.000000000000000000, 0.9510565162951535312, 1.000000000000000000, 0.9510565162951535312, 1.000000000000000000, 0.9510565162951535312, 1.000000000000000000, 0.9510565162951535312, 1.000000000000000000, 0.9510565162951535312, 1.000000000000000000, 0.9510565162951535312, 1.000000000000000000, 0.9510565162951535312, 1.000000000000000000, 0.9510565162951535312, 1.000000000000000000, 0.9510565162951535312, 1.000000000000000000, 0.9510565162951535312, 1.000000000000000000, 0.9510565162951535312, 1.000000000000000000, 0.9510565162951535312, 1.000000000000000000, 0.9510565162951535312, 1.000000000000000000, 0.9510565162951535312, 1.000000000000000000, 0.9510565162951535312, 1.000000000000000000, 0.9510565162951535312, 1.000000000000000000, 0.9510565162951535312, 1.000000000000000000, 0.9510565162951535312, 1.000000000000000000, 0.9510565162951535312, 1.000000000000000000, 0.9510565162951535312, 1.000000000000000000, 0.9510565162951535312, 1.000000000000000000, 0.9510565162951535312, 1.000000000000000000, 0.9510565162951535312, 1.000000000000000000, 0.9510565162951535312, 1.000000000000000000, 0.9510565162951535312, 1.000000000000000000, 0.9510565162951535312, 1.000000000000000000, 0.9510565162951535312, 1.000000000000000000, 0.9510565162951535312, 1.000000000000000000, 0.9510565162951535312, 1.000000000000000000, 0.9510565162951535312, 1.000000000000000000, 0.9510565162951535312, 1.000000000000000000, 0.9510565162951535312, 1.000000000000000000, 0.9510565162951535312, 1.000000000000000000, 0.9510565162951535312, 1.000000000000000000, 0.9510565162951535312, 1.000000000000000000, 0.9510565162951535312, 1.000000000000000000, 0.9510565162951535312, 1.000000000000000000, 0.9510565162951535312, 1.000000000000000000, 0.9510565162951535312, 1.000000000000000000, 0.9510565162951535312, 1.000000000000000000, 0.9510565162951535312, 1.000000000000000000, 0.9510565162951535312, 1.000000000000000000, 0.9510565162951535312, 1.000000000000000000, 0.9510565162951535312, 1.000000000000000000, 0.9510565162951535312, 1.000000000000000000, 0.9510565162951535312, 1.000000000000000000, 0.9510565162951535312, 1.000000000000000000, 0.9510565162951535312, 1.000000000000000000, 0.9510565162951535312, 1.000000000000000000, 0.9510565162951535312, 1.000000000000000000, 0.9510565162951535312, 1.000000000000000000, 0.9510565162951535312, 1.000000000000000000, 0.9510565162951535312, 1.000000000000000000, 0.9510565162951535312, 1.000000000000000000, 0.9510565162951535312, 1.000000000000000000),
 ( 1.000000000000000000, 0.9510565162951535312, 1.000000000000000000, 0.9510565162951535312, 1.000000000000000000, 0.9510565162951535312, 1.000000000000000000, 0.9510565162951535312, 1.000000000000000000, 0.9510565162951535312, 1.000000000000000000, 0.9510565162951535312, 1.000000000000000000, 0.9510565162951535312, 1.000000000000000000, 0.9510565162951535312, 1.000000000000000000, 0.9510565162951535312, 1.000000000000000000, 0.9510565162951535312, 1.000000000000000000, 0.9510565162951535312, 1.000000000000000000, 0.9510565162951535312, 1.000000000000000000, 0.9510565162951535312, 1.000000000000000000, 0.9510565162951535312, 1.000000000000000000, 0.9510565162951535312, 1.000000000000000000, 0.9510565162951535312, 1.000000000000000000, 0.9510565162951535312, 1.000000000000000000, 0.9510565162951535312, 1.000000000000000000, 0.9510565162951535312, 1.000000000000000000, 0.9510565162951535312, 1.000000000000000000, 0.9510565162951535312, 1.000000000000000000, 0.9510565162951535312, 1.000000000000000000, 0.9510565162951535312, 1.000000000000000000, 0.9510565162951535312, 1.000000000000000000, 0.9510565162951535312, 1.000000000000000000, 0.9510565162951535312, 1.000000000000000000, 0.9510565162951535312, 1.000000000000000000, 0.9510565162951535312, 1.000000000000000000, 0.9510565162951535312, 1.000000000000000000, 0.9510565162951535312, 1.000000000000000000, 0.9510565162951535312, 1.000000000000000000, 0.9510565162951535312, 1.000000000000000000, 0.9510565162951535312, 1.000000000000000000, 0.9510565162951535312, 1.000000000000000000, 0.9510565162951535312, 1.000000000000000000, 0.9510565162951535312, 1.000000000000000000, 0.9510565162951535312, 1.000000000000000000, 0.9510565162951535312, 1.000000000000000000, 0.9510565162951535312, 1.000000000000000000, 0.9510565162951535312, 1.000000000000000000, 0.9510565162951535312, 1.000000000000000000, 0.9510565162951535312, 1.000000000000000000, 0.9510565162951535312, 1.000000000000000000, 0.9510565162951535312, 1.000000000000000000, 0.9510565162951535312, 1.000000000000000000, 0.9510565162951535312, 1.000000000000000000, 0.9510565162951535312, 1.000000000000000000, 0.9510565162951535312, 1.000000000000000000, 0.9510565162951535312, 1.000000000000000000, 0.9510565162951535312, 1.000000000000000000, 0.9510565162951535312, 1.000000000000000000, 0.9510565162951535312, 1.000000000000000000, 0.9510565162951535312, 1.000000000000000000, 0.9510565162951535312, 1.000000000000000000, 0.9510565162951535312, 1.000000000000000000, 0.9510565162951535312, 1.000000000000000000, 0.9510565162951535312, 1.000000000000000000, 0.9510565162951535312, 1.000000000000000000, 0.9510565162951535312, 1.000000000000000000, 0.9510565162951535312, 1.000000000000000000, 0.9510565162951535312, 1.000000000000000000, 0.9510565162951535312, 1.000000000000000000, 0.9510565162951535312, 1.000000000000000000, 0.9510565162951535312, 1.000000000000000000, 0.9510565162951535312, 1.000000000000000000, 0.9510565162951535312, 1.000000000000000000, 0.9510565162951535312, 1.000000000000000000, 0.9510565162951535312, 1.000000000000000000, 0.9510565162951535312, 1.000000000000000000, 0.9510565162951535312, 1.000000000000000000, 0.9510565162951535312, 1.000000000000000000, 0.9510565162951535312, 1.000000000000000000, 0.9510565162951535312, 1.000000000000000000, 0.9510565162951535312, 1.000000000000000000, 0.9510565162951535312, 1.000000000000000000, 0.9510565162951535312, 1.000000000000000000, 0.9510565162951535312, 1.000000000000000000, 0.9510565162951535312, 1.000000000000000000, 0.9510565162951535312, 1.000000000000000000, 0.9510565162951535312, 1.000000000000000000, 0.9510565162951535312, 1.000000000000000000, 0.9510565162951535312, 1.000000000000000000, 0.9510565162951535312, 1.000000000000000000, 0.9510565162951535312, 1.000000000000000000, 0.9510565162951535312, 1.000000000000000000, 0.9510565162951535312, 1.000000000000000000, 0.9510565162951535312, 1.000000000000000000, 0.9510565162951535312, 1.000000000000000000, 0.9510565162951535312, 1.000000000000000000, 0.9510565162951535312, 1.000000000000000000, 0.9510565162951535312, 1.000000000000000000, 0.9510565162951535312, 1.000000000000000000, 0.9510565162951535312, 1.000000000000000000, 0.9510565162951535312, 1.000000000000000000, 0.9510565162951535312, 1.000000000000000000, 0.9510565162951535312, 1.000000000000000000, 0.9510565162951535312, 1.000000000000000000, 0.9510565162951535312, 1.000000000000000000, 0.9510565162951535312, 1.000000000000000000, 0.9510565162951535312, 1.000000000000000000, 0.9510565162951535312, 1.000000000000000000, 0.9510565162951535312, 1.000000000000000000, 0.9510565162951535312, 1.000000000000000000, 0.9510565162951535312, 1.000000000000000000, 0.9510565162951535312, 1.000000000000000000, 0.9510565162951535312, 1.000000000000000000, 0.9510565162951535312, 1.000000000000000000, 0.9510565162951535312, 1.000000000000000000, 0.9510565162951535312, 1.000000000000000000, 0.9510565162951535312, 1.000000000000000000, 0.9510565162951535312, 1.000000000000000000, 0.9510565162951535312, 1.000000000000000000, 0.9510565162951535312, 1.000000000000000000, 0.9510565162951535312, 1.000000000000000000, 0.9510565162951535312, 1.000000000000000000, 0.9510565162951535312, 1.000000000000000000, 0.9510565162951535312, 1.000000000000000000, 0.9510565162951535312, 1.000000000000000000, 0.9510565162951535312, 1.000000000000000000, 0.9510565162951535312, 1.000000000000000000, 0.9510565162951535312, 1.000000000000000000, 0.9510565162951535312, 1.000000000000000000, 0.9510565162951535312, 1.000000000000000000, 0.9510565162951535312, 1.000000000000000000, 0.9510565162951535312, 1.000000000000000000, 0.9510565162951535312, 1.000000000000000000, 0.9510565162951535312, 1.000000000000000000, 0.9510565162951535312, 1.000000000000000000, 0.9510565162951535312, 1.000000000000000000, 0.9510565162951535312, 1.000000000000000000, 0.9510565162951535312, 1.000000000000000000, 0.9510565162951535312, 1.000000000000000000, 0.9510565162951535312, 1.000000000000000000, 0.9510565162951535312, 1.000000000000000000, 0.9510565162951535312, 1.000000000000000000, 0.9510565162951535312, 1.000000000000000000, 0.9510565162951535312, 1.000000000000000000, 0.9510565162951535312, 1.000000000000000000, 0.9510565162951535312, 1.000000000000000000, 0.9510565162951535312, 1.000000000000000000, 0.9510565162951535312, 1.000000000000000000, 0.9510565162951535312, 1.000000000000000000, 0.9510565162951535312, 1.000000000000000000, 0.9510565162951535312, 1.000000000000000000, 0.9510565162951535312, 1.000000000000000000, 0.9510565162951535312, 1.000000000000000000, 0.9510565162951535312, 1.000000000000000000, 0.9510565162951535312, 1.000000000000000000, 0.9510565162951535312, 1.000000000000000000, 0.9510565162951535312, 1.000000000000000000, 0.9510565162951535312, 1.000000000000000000, 0.9510565162951535312, 1.000000000000000000, 0.9510565162951535312, 1.000000000000000000, 0.9510565162951535312, 1.000000000000000000, 0.9510565162951535312, 1.000000000000000000, 0.9510565162951535312, 1.000000000000000000, 0.9510565162951535312, 1.000000000000000000, 0.9510565162951535312, 1.000000000000000000, 0.9510565162951535312, 1.000000000000000000, 0.9510565162951535312, 1.000000000000000000, 0.9510565162951535312, 1.000000000000000000, 0.9510565162951535312, 1.000000000000000000, 0.9510565162951535312, 1.000000000000000000, 0.9510565162951535312, 1.000000000000000000, 0.9510565162951535312, 1.000000000000000000, 0.9510565162951535312, 1.000000000000000000, 0.9510565162951535312, 1.000000000000000000, 0.9510565162951535312, 1.000000000000000000, 0.9510565162951535312, 1.000000000000000000, 0.9510565162951535312, 1.000000000000000000) ) ) 
 REPRESENTATION_ITEM ( '' )  SURFACE ( )  );
#69417 = DIRECTION ( 'NONE',  ( 1.000000000000000000, 0.000000000000000000, 0.000000000000000000 ) ) ;
#69418 =( GEOMETRIC_REPRESENTATION_CONTEXT ( 3 ) GLOBAL_UNCERTAINTY_ASSIGNED_CONTEXT ( ( #54389 ) ) GLOBAL_UNIT_ASSIGNED_CONTEXT ( ( #3847, #46853, #24982 ) ) REPRESENTATION_CONTEXT ( 'NONE', 'WORKASPACE' ) );
#69419 = ORIENTED_EDGE ( 'NONE', *, *, #47656, .F. ) ;
#69420 = CARTESIAN_POINT ( 'NONE',  ( -159.7429263765338021, -5.598654528085803328, -7.705886871421366635 ) ) ;
#69421 =( NAMED_UNIT ( * ) PLANE_ANGLE_UNIT ( ) SI_UNIT ( $, .RADIAN. ) );
#69422 = FILL_AREA_STYLE ('',( #57836 ) ) ;
#69423 = EDGE_CURVE ( 'NONE', #11461, #69157, #26979, .T. ) ;
#69424 = DIRECTION ( 'NONE',  ( 0.000000000000000000, 0.000000000000000000, 1.000000000000000000 ) ) ;
#69425 = EDGE_CURVE ( 'NONE', #4771, #15447, #65652, .T. ) ;
#69426 = DIRECTION ( 'NONE',  ( -1.000000000000000000, 0.000000000000000000, 0.000000000000000000 ) ) ;
#69427 = EDGE_LOOP ( 'NONE', ( #33192, #29308, #40934, #63499 ) ) ;
#69428 = ADVANCED_FACE ( 'NONE', ( #7624 ), #7297, .T. ) ;
#69429 = CARTESIAN_POINT ( 'NONE',  ( -79.79292637653381348, -3.094860106618429807, 9.524999999999991473 ) ) ;
#69430 = CARTESIAN_POINT ( 'NONE',  ( 16.75000000000000711, 0.000000000000000000, 4.000000000000000000 ) ) ;
#69431 = FACE_OUTER_BOUND ( 'NONE', #23610, .T. ) ;
#69432 = EDGE_CURVE ( 'NONE', #51828, #40202, #29226, .T. ) ;
#69433 = CARTESIAN_POINT ( 'NONE',  ( 22.99999999999999645, 0.000000000000000000, 24.00402776293825013 ) ) ;
#69434 = CARTESIAN_POINT ( 'NONE',  ( 23.71231517720798010, 112.9999999999999858, 7.000000000000000000 ) ) ;
#69435 = CARTESIAN_POINT ( 'NONE',  ( -182.1549999999999727, 7.632228543268600340, 2.479861379858949277 ) ) ;
#69436 = ORIENTED_EDGE ( 'NONE', *, *, #37926, .T. ) ;
#69437 = CARTESIAN_POINT ( 'NONE',  ( 71.50000000000000000, 35.92875272052971525, -10.00000000000000000 ) ) ;
#69438 = FACE_OUTER_BOUND ( 'NONE', #20042, .T. ) ;
#69439 = CARTESIAN_POINT ( 'NONE',  ( -73.85707362346617799, -5.598654528085803328, -7.705886871421366635 ) ) ;
#69440 = CARTESIAN_POINT ( 'NONE',  ( 9.250000000000003553, 27.99999999999998934, 3.750000000000000000 ) ) ;
#69441 = CYLINDRICAL_SURFACE ( 'NONE', #64570, 0.2500000000000002220 ) ;
#69442 = CARTESIAN_POINT ( 'NONE',  ( 2.607480562269076430, 138.9070736234661467, -8.025000000000000355 ) ) ;
#69443 = VERTEX_POINT ( 'NONE', #39672 ) ;
#69444 = CARTESIAN_POINT ( 'NONE',  ( -32.02582413434465991, -8.774267863477543727, -1.283165077963180023 ) ) ;
#69445 = CARTESIAN_POINT ( 'NONE',  ( -95.45499999999998408, 7.632228543268599452, -2.479861379858951942 ) ) ;
#69446 = UNCERTAINTY_MEASURE_WITH_UNIT (LENGTH_MEASURE( 1.000000000000000082E-05 ), #45447, 'distance_accuracy_value', 'NONE');
#69447 = CARTESIAN_POINT ( 'NONE',  ( 32.00000000000002132, 42.00000000000000000, 80.00402776293826435 ) ) ;
#69448 = COLOUR_RGB ( '', 0.40784314, 0.44705882, 0.49803922) ;
#69449 = ORIENTED_EDGE ( 'NONE', *, *, #37100, .F. ) ;
#69450 = AXIS2_PLACEMENT_3D ( 'NONE', #23793, #39656, #45296 ) ;
#69451 = CARTESIAN_POINT ( 'NONE',  ( -40.04190075645215785, -13.49999999999999822, 0.8979962945199000401 ) ) ;
#69452 = CARTESIAN_POINT ( 'NONE',  ( 71.50000000000000000, 14.49137674618942739, -7.500000000000000000 ) ) ;
#69453 = LINE ( 'NONE', #32858, #65700 ) ;
#69454 = CARTESIAN_POINT ( 'NONE',  ( -76.75000000000000000, 4.336808689942018722E-16, 20.00000000000000000 ) ) ;
#69455 = DIRECTION ( 'NONE',  ( -0.000000000000000000, -0.000000000000000000, -1.000000000000000000 ) ) ;
#69456 = EDGE_LOOP ( 'NONE', ( #43897, #7569, #5960, #36002 ) ) ;
#69457 = DIRECTION ( 'NONE',  ( 1.000000000000000000, 0.000000000000000000, 0.000000000000000000 ) ) ;
#69458 = CARTESIAN_POINT ( 'NONE',  ( -72.89499999999999602, 6.826472737025116366, 4.959722759717898555 ) ) ;
#69459 = ORIENTED_EDGE ( 'NONE', *, *, #21851, .T. ) ;
#69460 = CARTESIAN_POINT ( 'NONE',  ( 0.000000000000000000, 116.9429263765338192, -8.025000000000000355 ) ) ;
#69461 = DIRECTION ( 'NONE',  ( 0.000000000000000000, 1.000000000000000000, 0.000000000000000000 ) ) ;
#69462 = ORIENTED_EDGE ( 'NONE', *, *, #2368, .F. ) ;
#69463 = FACE_OUTER_BOUND ( 'NONE', #8630, .T. ) ;
#69464 =( NAMED_UNIT ( * ) PLANE_ANGLE_UNIT ( ) SI_UNIT ( $, .RADIAN. ) );
#69465 =( GEOMETRIC_REPRESENTATION_CONTEXT ( 3 ) GLOBAL_UNCERTAINTY_ASSIGNED_CONTEXT ( ( #23460 ) ) GLOBAL_UNIT_ASSIGNED_CONTEXT ( ( #45731, #9458, #47116 ) ) REPRESENTATION_CONTEXT ( 'NONE', 'WORKASPACE' ) );
#69466 = DIRECTION ( 'NONE',  ( 0.000000000000000000, 0.000000000000000000, 1.000000000000000000 ) ) ;
#69467 = CARTESIAN_POINT ( 'NONE',  ( 40.78947368421051323, 108.1536491499103363, 10.00000000000000000 ) ) ;
#69468 = ORIENTED_EDGE ( 'NONE', *, *, #31429, .T. ) ;
#69469 = ORIENTED_EDGE ( 'NONE', *, *, #65117, .F. ) ;
#69470 = CARTESIAN_POINT ( 'NONE',  ( -160.1929263765337907, -10.01517768586948698, 6.132527647946031529E-16 ) ) ;
#69471 = DIRECTION ( 'NONE',  ( 0.000000000000000000, 1.000000000000000000, -0.000000000000000000 ) ) ;
#69472 = CARTESIAN_POINT ( 'NONE',  ( -157.4070736234661751, 3.094860106618428031, -9.524999999999993250 ) ) ;
#69473 = CARTESIAN_POINT ( 'NONE',  ( -3.094860106618432471, 124.5949999999999704, -9.525000000000000355 ) ) ;
#69474 = CARTESIAN_POINT ( 'NONE',  ( -96.20707362346614389, 3.094860106618433360, 9.524999999999991473 ) ) ;
#69475 = AXIS2_PLACEMENT_3D ( 'NONE', #22517, #17926, #66455 ) ;
#69476 = CARTESIAN_POINT ( 'NONE',  ( -60.00000000000000000, -2.024042244987997205E-14, 10.50000000000000000 ) ) ;
#69477 = VERTEX_POINT ( 'NONE', #23808 ) ;
#69479 = PRESENTATION_STYLE_ASSIGNMENT (( #38562 ) ) ;
#69478 = DIRECTION ( 'NONE',  ( 0.000000000000000000, 0.000000000000000000, 1.000000000000000000 ) ) ;
#69480 =( GEOMETRIC_REPRESENTATION_CONTEXT ( 3 ) GLOBAL_UNCERTAINTY_ASSIGNED_CONTEXT ( ( #52445 ) ) GLOBAL_UNIT_ASSIGNED_CONTEXT ( ( #68711, #27495, #48674 ) ) REPRESENTATION_CONTEXT ( 'NONE', 'WORKASPACE' ) );
#69481 = CARTESIAN_POINT ( 'NONE',  ( -7.632228543268608334, 130.9570736234661581, 2.479861379858952830 ) ) ;
#69482 = CARTESIAN_POINT ( 'NONE',  ( -138.2049999999999272, -2.607480562269071545, -8.024999999999991473 ) ) ;
#69483 = LINE ( 'NONE', #11072, #31875 ) ;
#69484 = CARTESIAN_POINT ( 'NONE',  ( -147.7449999999999761, 4.716976649647094177, 6.492361379858945902 ) ) ;
#69485 = EDGE_CURVE ( 'NONE', #66860, #44068, #2657, .T. ) ;
#69486 = MECHANICAL_DESIGN_GEOMETRIC_PRESENTATION_REPRESENTATION (  '', ( #14391 ), #28986 ) ;
#69487 = CARTESIAN_POINT ( 'NONE',  ( -141.7450000000000045, 4.716976649647094177, 6.492361379858945902 ) ) ;
#69488 = ORIENTED_EDGE ( 'NONE', *, *, #56861, .T. ) ;
#69489 = CIRCLE ( 'NONE', #24518, 0.5000000000000004441 ) ;
#69490 = EDGE_CURVE ( 'NONE', #41057, #64160, #56176, .T. ) ;
#69491 = CARTESIAN_POINT ( 'NONE',  ( 44.83562443654410146, 9.945208145514939702, -3.584089800672845882 ) ) ;
#69492 = LINE ( 'NONE', #68822, #52573 ) ;
#69493 = SURFACE_SIDE_STYLE ('',( #10423 ) ) ;
#69494 = CARTESIAN_POINT ( 'NONE',  ( -55.55499999999999261, 0.000000000000000000, 8.024999999999991473 ) ) ;
#69495 =( BOUNDED_CURVE ( )  B_SPLINE_CURVE ( 2, ( #10076, #9034, #40721, #35426, #15384, #45991, #68829, #68468, #30452, #62132, #36839 ),
 .UNSPECIFIED., .F., .F. ) 
 B_SPLINE_CURVE_WITH_KNOTS ( ( 3, 2, 2, 2, 2, 3 ),
 ( 0.2826086956521673410, 0.2847826086956455893, 0.2869565217391237821, 0.2891304347826019194, 0.2913043478260801122, 0.2934782608695583606 ),
 .UNSPECIFIED. ) 
 CURVE ( )  GEOMETRIC_REPRESENTATION_ITEM ( )  RATIONAL_B_SPLINE_CURVE ( ( 1.000000000000147438, 0.9510565162950060936, 1.000000000000000000, 0.9510565162951535312, 1.000000000000000000, 0.9510565162951535312, 1.000000000000000000, 0.9510565162951535312, 1.000000000000000000, 0.9510565162953085183, 0.9999999999998450129 ) ) 
 REPRESENTATION_ITEM ( '' )  );
#69496 = DIRECTION ( 'NONE',  ( -0.000000000000000000, -0.000000000000000000, 1.000000000000000000 ) ) ;
#69497 = CIRCLE ( 'NONE', #42569, 1.000000000000000888 ) ;
#69498 = VECTOR ( 'NONE', #36105, 1000.000000000000000 ) ;
#69499 = CARTESIAN_POINT ( 'NONE',  ( -41.49999999999997868, 10.49999999999998224, -3.000000000000000444 ) ) ;
#69500 = EDGE_CURVE ( 'NONE', #67044, #49461, #28724, .T. ) ;
#69501 = FACE_OUTER_BOUND ( 'NONE', #60258, .T. ) ;
#69502 = EDGE_CURVE ( 'NONE', #60615, #360, #43387, .T. ) ;
#69503 = CARTESIAN_POINT ( 'NONE',  ( -32.76851741822840580, -9.107254030101904263, -2.000000000000000000 ) ) ;
#69504 = FACE_OUTER_BOUND ( 'NONE', #63715, .T. ) ;
#69505 = STYLED_ITEM ( 'NONE', ( #41841 ), #68252 ) ;
#69506 = CARTESIAN_POINT ( 'NONE',  ( 20.71231517720797655, 149.4999999999999716, 10.00000000000000000 ) ) ;
#69507 =( NAMED_UNIT ( * ) SI_UNIT ( $, .STERADIAN. ) SOLID_ANGLE_UNIT ( ) );
#69508 = ORIENTED_EDGE ( 'NONE', *, *, #48477, .T. ) ;
#69509 =( LENGTH_UNIT ( ) NAMED_UNIT ( * ) SI_UNIT ( .MILLI., .METRE. ) );
#69510 =( BOUNDED_CURVE ( )  B_SPLINE_CURVE ( 2, ( #15926, #53534, #38082, #65104, #27110, #22214, #54213, #38444, #11654, #682, #6711 ),
 .UNSPECIFIED., .F., .F. ) 
 B_SPLINE_CURVE_WITH_KNOTS ( ( 3, 2, 2, 2, 2, 3 ),
 ( 0.6304347826086809103, 0.6326086956521591587, 0.6347826086956372960, 0.6369565217391155443, 0.6391304347825936816, 0.6413043478260719299 ),
 .UNSPECIFIED. ) 
 CURVE ( )  GEOMETRIC_REPRESENTATION_ITEM ( )  RATIONAL_B_SPLINE_CURVE ( ( 1.000000000000332401, 0.9510565162948211304, 1.000000000000000000, 0.9510565162951535312, 1.000000000000000000, 0.9510565162951535312, 1.000000000000000000, 0.9510565162951535312, 1.000000000000000000, 0.9510565162954909280, 0.9999999999996626032 ) ) 
 REPRESENTATION_ITEM ( '' )  );
#69511 = CARTESIAN_POINT ( 'NONE',  ( -4.716976649647098618, 113.2570736234661553, 6.492361379858953008 ) ) ;
#69512 = CIRCLE ( 'NONE', #57158, 0.5000000000000004441 ) ;
#69513 = CARTESIAN_POINT ( 'NONE',  ( 3.851859888774471706E-31, -8.500000000000000000, 23.00000000000000000 ) ) ;
#69514 = EDGE_CURVE ( 'NONE', #1442, #2941, #6780, .T. ) ;
#69515 = ORIENTED_EDGE ( 'NONE', *, *, #14156, .F. ) ;
#69517 = VERTEX_POINT ( 'NONE', #65680 ) ;
#69516 = VECTOR ( 'NONE', #47029, 1000.000000000000000 ) ;
#69518 = DIRECTION ( 'NONE',  ( 0.000000000000000000, 0.000000000000000000, 1.000000000000000000 ) ) ;
#69519 = DIRECTION ( 'NONE',  ( -1.000000000000000000, 0.000000000000000000, 0.000000000000000000 ) ) ;
#69520 =( NAMED_UNIT ( * ) PLANE_ANGLE_UNIT ( ) SI_UNIT ( $, .RADIAN. ) );
#69521 = ORIENTED_EDGE ( 'NONE', *, *, #22287, .T. ) ;
#69522 = CARTESIAN_POINT ( 'NONE',  ( 8.102448949553183510, 122.1049999999999898, -5.886773742842746238 ) ) ;
#69523 = SURFACE_STYLE_USAGE ( .BOTH. , #15407 ) ;
#69524 = FILL_AREA_STYLE_COLOUR ( '', #29959 ) ;
#69525 = AXIS2_PLACEMENT_3D ( 'NONE', #10835, #555, #23133 ) ;
#69526 = CIRCLE ( 'NONE', #39243, 0.5000000000000004441 ) ;
#69527 = CARTESIAN_POINT ( 'NONE',  ( -74.99999999999998579, 50.00000000000000000, -11.50000000000001066 ) ) ;
#69528 = CARTESIAN_POINT ( 'NONE',  ( -99.59499999999999886, 2.607480562269073321, 8.024999999999991473 ) ) ;
#69529 = ORIENTED_EDGE ( 'NONE', *, *, #6364, .T. ) ;
#69530 =( GEOMETRIC_REPRESENTATION_CONTEXT ( 3 ) GLOBAL_UNCERTAINTY_ASSIGNED_CONTEXT ( ( #41723 ) ) GLOBAL_UNIT_ASSIGNED_CONTEXT ( ( #18517, #7951, #50870 ) ) REPRESENTATION_CONTEXT ( 'NONE', 'WORKASPACE' ) );
#69531 = ADVANCED_FACE ( 'NONE', ( #11871 ), #29337, .T. ) ;
#69532 = CARTESIAN_POINT ( 'NONE',  ( 45.50000000000000000, 10.69371294336137979, -4.000000000000000000 ) ) ;
#69533 = FILL_AREA_STYLE_COLOUR ( '', #223 ) ;
#69534 = ORIENTED_EDGE ( 'NONE', *, *, #58678, .T. ) ;
#69535 = CARTESIAN_POINT ( 'NONE',  ( 7.632228543268607446, 152.0429263765338135, 2.479861379858954606 ) ) ;
#69536 = ADVANCED_FACE ( 'NONE', ( #45987 ), #7895, .T. ) ;
#69537 =( GEOMETRIC_REPRESENTATION_CONTEXT ( 3 ) GLOBAL_UNCERTAINTY_ASSIGNED_CONTEXT ( ( #46724 ) ) GLOBAL_UNIT_ASSIGNED_CONTEXT ( ( #25445, #42380, #52895 ) ) REPRESENTATION_CONTEXT ( 'NONE', 'WORKASPACE' ) );
#69538 = CARTESIAN_POINT ( 'NONE',  ( 0.000000000000000000, 0.000000000000000000, 0.000000000000000000 ) ) ;
#69539 = SURFACE_STYLE_FILL_AREA ( #54046 ) ;
#69540 = CARTESIAN_POINT ( 'NONE',  ( 20.44134218812435932, 115.3860596766049440, -10.00000000000000000 ) ) ;
#69541 = ORIENTED_EDGE ( 'NONE', *, *, #23485, .T. ) ;
#69542 = LINE ( 'NONE', #21346, #27873 ) ;
#69543 = CARTESIAN_POINT ( 'NONE',  ( -45.50000000000000000, 1.797044900979284448E-15, -10.00000000000000000 ) ) ;
#69545 = VECTOR ( 'NONE', #5032, 1000.000000000000000 ) ;
#69544 = CARTESIAN_POINT ( 'NONE',  ( -32.33125961450744512, -8.628515624790757954, 6.699332285579864710 ) ) ;
#69546 = DIRECTION ( 'NONE',  ( 0.000000000000000000, 0.000000000000000000, -1.000000000000000000 ) ) ;
#69547 = CARTESIAN_POINT ( 'NONE',  ( 13.75000000000000533, 30.74999999999999289, -4.000000000000000000 ) ) ;
#69548 = DIRECTION ( 'NONE',  ( 0.000000000000000000, 0.000000000000000000, 1.000000000000000000 ) ) ;
#69549 = DIRECTION ( 'NONE',  ( 0.000000000000000000, 0.000000000000000000, 1.000000000000000000 ) ) ;
#69550 = CARTESIAN_POINT ( 'NONE',  ( -8.586026971066690550, 153.5450349297233572, -0.1239747060112212501 ) ) ;
#69551 = EDGE_LOOP ( 'NONE', ( #26677, #64137, #47567 ) ) ;
#69552 =( GEOMETRIC_REPRESENTATION_CONTEXT ( 3 ) GLOBAL_UNCERTAINTY_ASSIGNED_CONTEXT ( ( #19916 ) ) GLOBAL_UNIT_ASSIGNED_CONTEXT ( ( #35677, #9290, #51857 ) ) REPRESENTATION_CONTEXT ( 'NONE', 'WORKASPACE' ) );
#69553 = ORIENTED_EDGE ( 'NONE', *, *, #36160, .F. ) ;
#69554 = CARTESIAN_POINT ( 'NONE',  ( -161.8429263765337964, 9.058813317711329915, -2.943386871421373119 ) ) ;
#69555 = LINE ( 'NONE', #867, #16373 ) ;
#69556 = DIRECTION ( 'NONE',  ( 1.000000000000000000, -0.000000000000000000, 0.000000000000000000 ) ) ;
#69557 = EDGE_CURVE ( 'NONE', #5051, #56763, #8343, .T. ) ;
#69558 = EDGE_LOOP ( 'NONE', ( #6060, #66281, #31886, #58275 ) ) ;
#69559 = CARTESIAN_POINT ( 'NONE',  ( -57.99999999999997868, 50.00000000000000000, -6.500000000000000000 ) ) ;
#69560 = CARTESIAN_POINT ( 'NONE',  ( -168.3550000000000182, -4.716976649647093289, -6.492361379858945902 ) ) ;
#69561 = EDGE_CURVE ( 'NONE', #31194, #36960, #47267, .T. ) ;
#69562 = DIRECTION ( 'NONE',  ( -0.000000000000000000, -1.000000000000000000, -0.000000000000000000 ) ) ;
#69563 = DIRECTION ( 'NONE',  ( 0.000000000000000000, 1.000000000000000000, -0.000000000000000000 ) ) ;
#69564 = CARTESIAN_POINT ( 'NONE',  ( -179.2449999999999761, -4.716976649647093289, -6.492361379858945902 ) ) ;
#69565 = CARTESIAN_POINT ( 'NONE',  ( -164.3949999999999818, -6.826472737025113702, -4.959722759717900331 ) ) ;
#69566 = ORIENTED_EDGE ( 'NONE', *, *, #579, .T. ) ;
#69567 = SURFACE_STYLE_USAGE ( .BOTH. , #36583 ) ;
#69568 = EDGE_CURVE ( 'NONE', #60568, #69365, #24749, .T. ) ;
#69569 = CARTESIAN_POINT ( 'NONE',  ( -39.78460846725723599, -11.70376609979392946, 3.331841550777793870 ) ) ;
#69570 = FILL_AREA_STYLE_COLOUR ( '', #19186 ) ;
#69571 = CARTESIAN_POINT ( 'NONE',  ( -85.85499999999998977, 4.716976649647094177, 6.492361379858945902 ) ) ;
#69572 = CARTESIAN_POINT ( 'NONE',  ( -41.49999999999998579, 106.9282032302754999, 3.500000000000000000 ) ) ;
#69573 = DIRECTION ( 'NONE',  ( -1.000000000000000000, 0.000000000000000000, 0.000000000000000000 ) ) ;
#69574 = CARTESIAN_POINT ( 'NONE',  ( -75.48275862068965125, 36.00832590023089352, -9.500000000000000000 ) ) ;
#69575 = COLOUR_RGB ( '', 0.40784314, 0.44705882, 0.49803922) ;
#69576 = CARTESIAN_POINT ( 'NONE',  ( -77.99499999999996191, -6.826472737025113702, 4.959722759717902107 ) ) ;
#69577 = CARTESIAN_POINT ( 'NONE',  ( -5.598654528085806881, 134.8549999999999898, -7.705886871421374629 ) ) ;
#69578 = DIRECTION ( 'NONE',  ( 0.8660254037844385966, 0.5000000000000002220, -0.000000000000000000 ) ) ;
#69579 = VECTOR ( 'NONE', #38575, 1000.000000000000000 ) ;
#69580 = EDGE_CURVE ( 'NONE', #38790, #2677, #14639, .T. ) ;
#69581 = VECTOR ( 'NONE', #31115, 1000.000000000000000 ) ;
#69582 = CARTESIAN_POINT ( 'NONE',  ( -171.6570736234661751, 9.058813317711329915, 2.943386871421369566 ) ) ;
#69583 = PRESENTATION_LAYER_ASSIGNMENT (  '', '', ( #51605 ) ) ;
#69584 = DIRECTION ( 'NONE',  ( 0.000000000000000000, 1.000000000000000000, -0.000000000000000000 ) ) ;
#69585 = STYLED_ITEM ( 'NONE', ( #58532 ), #9331 ) ;
#69586 = SURFACE_SIDE_STYLE ('',( #33000 ) ) ;
#69587 = ORIENTED_EDGE ( 'NONE', *, *, #47313, .T. ) ;
#69589 = EDGE_CURVE ( 'NONE', #58700, #55021, #36498, .T. ) ;
#69588 = STYLED_ITEM ( 'NONE', ( #21903 ), #41836 ) ;
#69590 =( NAMED_UNIT ( * ) PLANE_ANGLE_UNIT ( ) SI_UNIT ( $, .RADIAN. ) );
#69591 = CIRCLE ( 'NONE', #12331, 8.499999999999992895 ) ;
#69592 = DIRECTION ( 'NONE',  ( 1.000000000000000000, 0.000000000000000000, -1.300977106640434891E-16 ) ) ;
#69593 = CYLINDRICAL_SURFACE ( 'NONE', #43184, 8.999999999999994671 ) ;
#69594 = ORIENTED_EDGE ( 'NONE', *, *, #11274, .F. ) ;
#69595 = ORIENTED_EDGE ( 'NONE', *, *, #38732, .T. ) ;
#69596 = DIRECTION ( 'NONE',  ( 0.000000000000000000, 0.000000000000000000, 1.000000000000000000 ) ) ;
#69597 = CARTESIAN_POINT ( 'NONE',  ( -174.3570736234661638, 5.598654528085804216, 7.705886871421366635 ) ) ;
#69598 = AXIS2_PLACEMENT_3D ( 'NONE', #29612, #51087, #67248 ) ;
#69599 = CONICAL_SURFACE ( 'NONE', #49446, 5.000000000000000000, 0.7853981633974482790 ) ;
#69600 = CARTESIAN_POINT ( 'NONE',  ( 53.24999999999999289, 27.74999999999998579, -4.000000000000000000 ) ) ;
#69601 = ORIENTED_EDGE ( 'NONE', *, *, #55026, .F. ) ;
#69602 = CARTESIAN_POINT ( 'NONE',  ( -121.7049999999999841, 2.607480562269072433, 8.024999999999991473 ) ) ;
#69603 = ORIENTED_EDGE ( 'NONE', *, *, #33203, .T. ) ;
#69604 = CARTESIAN_POINT ( 'NONE',  ( 57.00000000000000000, 0.000000000000000000, 60.00402776293827145 ) ) ;
#69605 = SURFACE_SIDE_STYLE ('',( #5919 ) ) ;
#69606 = ORIENTED_EDGE ( 'NONE', *, *, #18189, .F. ) ;
#69607 = CARTESIAN_POINT ( 'NONE',  ( 6.413663052920311358, 2.499999999999998668, 2.891209729714698806 ) ) ;
#69608 = ORIENTED_EDGE ( 'NONE', *, *, #36180, .F. ) ;
#69609 = VECTOR ( 'NONE', #31817, 1000.000000000000000 ) ;
#69610 = SURFACE_SIDE_STYLE ('',( #52433 ) ) ;
#69611 = CARTESIAN_POINT ( 'NONE',  ( -3.094860106618432471, 145.5949999999999136, -9.525000000000000355 ) ) ;
#69612 = DIRECTION ( 'NONE',  ( -0.000000000000000000, 0.000000000000000000, 1.000000000000000000 ) ) ;
#69613 = ADVANCED_FACE ( 'NONE', ( #62813 ), #24834, .F. ) ;
#69614 = ORIENTED_EDGE ( 'NONE', *, *, #12199, .T. ) ;
#69615 = FILL_AREA_STYLE_COLOUR ( '', #41807 ) ;
#69616 = VECTOR ( 'NONE', #52140, 1000.000000000000000 ) ;
#69617 = DIRECTION ( 'NONE',  ( 0.000000000000000000, 0.000000000000000000, 1.000000000000000000 ) ) ;
#69618 = ORIENTED_EDGE ( 'NONE', *, *, #31868, .F. ) ;
#69619 = CARTESIAN_POINT ( 'NONE',  ( -4.716976649647098618, 124.1429263765338220, 6.492361379858953008 ) ) ;
#69620 = CARTESIAN_POINT ( 'NONE',  ( 8.319377385370872346, -3.000000000000000888, 2.000000000000000000 ) ) ;
#69621 =( LENGTH_UNIT ( ) NAMED_UNIT ( * ) SI_UNIT ( .MILLI., .METRE. ) );
#69622 = DIRECTION ( 'NONE',  ( -0.000000000000000000, 1.000000000000000000, -0.000000000000000000 ) ) ;
#69623 = CARTESIAN_POINT ( 'NONE',  ( 3.249999999999998668, 36.99999999999999289, -3.750000000000000000 ) ) ;
#69624 = VERTEX_POINT ( 'NONE', #3343 ) ;
#69625 = AXIS2_PLACEMENT_3D ( 'NONE', #8086, #34467, #24948 ) ;
#69626 = DIRECTION ( 'NONE',  ( -1.000000000000000000, 0.000000000000000000, 0.000000000000000000 ) ) ;
#69627 = ORIENTED_EDGE ( 'NONE', *, *, #54408, .T. ) ;
#69628 = FACE_OUTER_BOUND ( 'NONE', #59322, .T. ) ;
#69629 = DIRECTION ( 'NONE',  ( -0.000000000000000000, -0.000000000000000000, 1.000000000000000000 ) ) ;
#69630 = CARTESIAN_POINT ( 'NONE',  ( -146.1549999999999727, 7.632228543268600340, 2.479861379858949277 ) ) ;
#69631 = SURFACE_STYLE_FILL_AREA ( #10216 ) ;
#69632 = AXIS2_PLACEMENT_3D ( 'NONE', #67892, #46830, #52421 ) ;
#69633 = CARTESIAN_POINT ( 'NONE',  ( 6.516641522221523708, 43.00000000000000000, -28.13388297856903719 ) ) ;
#69634 = EDGE_CURVE ( 'NONE', #35727, #15634, #34862, .T. ) ;
#69635 = DIRECTION ( 'NONE',  ( 0.000000000000000000, 0.000000000000000000, -1.000000000000000000 ) ) ;
#69636 = DIRECTION ( 'NONE',  ( 1.000000000000000000, 0.000000000000000000, -0.000000000000000000 ) ) ;
#69637 = SURFACE_SIDE_STYLE ('',( #32691 ) ) ;
#69638 = CYLINDRICAL_SURFACE ( 'NONE', #58973, 5.499999999999985789 ) ;
#69639 = ORIENTED_EDGE ( 'NONE', *, *, #54481, .T. ) ;
#69640 = CIRCLE ( 'NONE', #4493, 5.000000000000004441 ) ;
#69641 = VERTEX_POINT ( 'NONE', #20259 ) ;
#69642 = DIRECTION ( 'NONE',  ( -1.000000000000000000, 0.000000000000000000, 0.000000000000000000 ) ) ;
#69643 = CARTESIAN_POINT ( 'NONE',  ( 43.75000000000000000, 19.24999999999998224, -3.750000000000000000 ) ) ;
#69644 = EDGE_CURVE ( 'NONE', #54309, #6097, #25880, .T. ) ;
#69645 = CARTESIAN_POINT ( 'NONE',  ( -59.60499999999998977, 6.826472737025113702, -4.959722759717902107 ) ) ;
#69646 = VERTEX_POINT ( 'NONE', #19206 ) ;
#69647 = DIRECTION ( 'NONE',  ( 0.000000000000000000, 0.000000000000000000, 1.000000000000000000 ) ) ;
#69648 = FACE_OUTER_BOUND ( 'NONE', #25685, .T. ) ;
#69649 = EDGE_CURVE ( 'NONE', #38116, #50390, #33748, .T. ) ;
#69650 = CARTESIAN_POINT ( 'NONE',  ( 57.49999999999999289, 27.74999999999998934, -3.750000000000000000 ) ) ;
#69651 = FACE_OUTER_BOUND ( 'NONE', #53618, .T. ) ;
#69652 = MECHANICAL_DESIGN_GEOMETRIC_PRESENTATION_REPRESENTATION (  '', ( #28090 ), #6768 ) ;
#69653 = CARTESIAN_POINT ( 'NONE',  ( -74.99999999999998579, 50.00000000000000000, -12.00000000000000000 ) ) ;
#69654 = CARTESIAN_POINT ( 'NONE',  ( -97.04292637653379927, -9.058813317711329915, -2.943386871421370898 ) ) ;
#69655 = PRESENTATION_LAYER_ASSIGNMENT (  '', '', ( #42744 ) ) ;
#69656 = ORIENTED_EDGE ( 'NONE', *, *, #31260, .T. ) ;
#69657 = EDGE_CURVE ( 'NONE', #66646, #27816, #21394, .T. ) ;
#69658 = LINE ( 'NONE', #21829, #4695 ) ;
#69659 = CARTESIAN_POINT ( 'NONE',  ( 31.00000000000000000, 15.00000000000000000, -80.00402776293826435 ) ) ;
#69660 = PRESENTATION_STYLE_ASSIGNMENT (( #59430 ) ) ;
#69661 = EDGE_CURVE ( 'NONE', #54990, #33026, #59621, .T. ) ;
#69662 = CARTESIAN_POINT ( 'NONE',  ( -110.6949999999999932, -8.437984349512086979, 5.166775262442717831E-16 ) ) ;
#69663 = CARTESIAN_POINT ( 'NONE',  ( 0.000000000000000000, 157.4449999999999932, -9.525000000000000355 ) ) ;
#69664 = CARTESIAN_POINT ( 'NONE',  ( -91.94499999999997897, -9.827790563157499189E-16, -8.024999999999991473 ) ) ;
#69665 = CARTESIAN_POINT ( 'NONE',  ( -7.632228543268607446, 112.6570736234661609, -2.479861379858953718 ) ) ;
#69666 = DIRECTION ( 'NONE',  ( 1.000000000000000000, 2.312964634635740689E-15, -0.000000000000000000 ) ) ;
#69667 = AXIS2_PLACEMENT_3D ( 'NONE', #13661, #15093, #36196 ) ;
#69668 = DIRECTION ( 'NONE',  ( 0.000000000000000000, 0.000000000000000000, 1.000000000000000000 ) ) ;
#69669 = DIRECTION ( 'NONE',  ( 0.000000000000000000, 0.000000000000000000, -1.000000000000000000 ) ) ;
#69671 = VERTEX_POINT ( 'NONE', #5443 ) ;
#69670 = AXIS2_PLACEMENT_3D ( 'NONE', #4502, #63617, #21385 ) ;
#69672 = CARTESIAN_POINT ( 'NONE',  ( -137.2429263765338021, 5.598654528085804216, 7.705886871421366635 ) ) ;
#69673 =( NAMED_UNIT ( * ) SI_UNIT ( $, .STERADIAN. ) SOLID_ANGLE_UNIT ( ) );
#69674 = CARTESIAN_POINT ( 'NONE',  ( -151.1950000000000216, 8.437984349512085203, -1.550032578732815448E-15 ) ) ;
#69675 = DIRECTION ( 'NONE',  ( -1.000000000000000000, 0.000000000000000000, -0.000000000000000000 ) ) ;
#69676 = ADVANCED_FACE ( 'NONE', ( #6167 ), #16750, .T. ) ;
#69677 = AXIS2_PLACEMENT_3D ( 'NONE', #48182, #69592, #69262 ) ;
#69678 = DIRECTION ( 'NONE',  ( 0.000000000000000000, 0.000000000000000000, 1.000000000000000000 ) ) ;
#69679 = VECTOR ( 'NONE', #8052, 1000.000000000000000 ) ;
#69680 = LINE ( 'NONE', #43365, #34972 ) ;
#69681 = VERTEX_POINT ( 'NONE', #122 ) ;
#69682 = EDGE_LOOP ( 'NONE', ( #16282, #23325, #13619, #17685 ) ) ;
#69683 = EDGE_CURVE ( 'NONE', #14317, #22460, #6836, .T. ) ;
#69684 = AXIS2_PLACEMENT_3D ( 'NONE', #18967, #30214, #41181 ) ;
#69685 = CARTESIAN_POINT ( 'NONE',  ( 0.000000000000000000, 2.299999999999999822, 0.000000000000000000 ) ) ;
#69686 = AXIS2_PLACEMENT_3D ( 'NONE', #30463, #31512, #25890 ) ;
#69687 = CARTESIAN_POINT ( 'NONE',  ( -45.00000000000000711, 8.062885798612171584, 5.903555993538923019 ) ) ;
#69688 = CARTESIAN_POINT ( 'NONE',  ( -4.500000000000002665, 24.74999999999998579, 4.000000000000000000 ) ) ;
#69689 = COLOUR_RGB ( '', 0.09019608, 0.27058824, 0.51372549) ;
#69690 = DIRECTION ( 'NONE',  ( 0.000000000000000000, 1.000000000000000000, 0.000000000000000000 ) ) ;
#69691 = ORIENTED_EDGE ( 'NONE', *, *, #67281, .F. ) ;
#69692 = CARTESIAN_POINT ( 'NONE',  ( -147.8049999999999500, -8.437984349512086979, 5.166775262442717831E-16 ) ) ;
#69693 = LINE ( 'NONE', #64094, #48621 ) ;
#69694 = NEXT_ASSEMBLY_USAGE_OCCURRENCE ( 'NAUO1', ' ', ' ', #48158, #29610, $ ) ;
#69695 = NEXT_ASSEMBLY_USAGE_OCCURRENCE ( 'NAUO2', ' ', ' ', #48158, #35663, $ ) ;
#69696 = NEXT_ASSEMBLY_USAGE_OCCURRENCE ( 'NAUO3', ' ', ' ', #48158, #59698, $ ) ;
#69697 = NEXT_ASSEMBLY_USAGE_OCCURRENCE ( 'NAUO4', ' ', ' ', #48158, #59698, $ ) ;
#69698 = NEXT_ASSEMBLY_USAGE_OCCURRENCE ( 'NAUO5', ' ', ' ', #48158, #53296, $ ) ;
#69699 = NEXT_ASSEMBLY_USAGE_OCCURRENCE ( 'NAUO6', ' ', ' ', #48158, #67906, $ ) ;
#69700 = NEXT_ASSEMBLY_USAGE_OCCURRENCE ( 'NAUO7', ' ', ' ', #48158, #67906, $ ) ;
#69701 = NEXT_ASSEMBLY_USAGE_OCCURRENCE ( 'NAUO8', ' ', ' ', #48158, #45995, $ ) ;
#69702 = NEXT_ASSEMBLY_USAGE_OCCURRENCE ( 'NAUO9', ' ', ' ', #48158, #27444, $ ) ;
#69703 = NEXT_ASSEMBLY_USAGE_OCCURRENCE ( 'NAUO10', ' ', ' ', #48158, #7683, $ ) ;
#69704 = NEXT_ASSEMBLY_USAGE_OCCURRENCE ( 'NAUO11', ' ', ' ', #48158, #52435, $ ) ;
#69705 = NEXT_ASSEMBLY_USAGE_OCCURRENCE ( 'NAUO12', ' ', ' ', #48158, #32611, $ ) ;
#69706 = NEXT_ASSEMBLY_USAGE_OCCURRENCE ( 'NAUO13', ' ', ' ', #48158, #1190, $ ) ;
#69707 = NEXT_ASSEMBLY_USAGE_OCCURRENCE ( 'NAUO14', ' ', ' ', #48158, #52435, $ ) ;
#69708 = NEXT_ASSEMBLY_USAGE_OCCURRENCE ( 'NAUO15', ' ', ' ', #48158, #1190, $ ) ;
#69709 = NEXT_ASSEMBLY_USAGE_OCCURRENCE ( 'NAUO16', ' ', ' ', #48158, #32611, $ ) ;
#69710 = NEXT_ASSEMBLY_USAGE_OCCURRENCE ( 'NAUO17', ' ', ' ', #48158, #6411, $ ) ;
#69711 = NEXT_ASSEMBLY_USAGE_OCCURRENCE ( 'NAUO18', ' ', ' ', #48158, #43868, $ ) ;
#69712 = NEXT_ASSEMBLY_USAGE_OCCURRENCE ( 'NAUO19', ' ', ' ', #48158, #64860, $ ) ;
#69713 = NEXT_ASSEMBLY_USAGE_OCCURRENCE ( 'NAUO20', ' ', ' ', #48158, #6411, $ ) ;
#69714 = NEXT_ASSEMBLY_USAGE_OCCURRENCE ( 'NAUO21', ' ', ' ', #48158, #64860, $ ) ;
#69715 = NEXT_ASSEMBLY_USAGE_OCCURRENCE ( 'NAUO22', ' ', ' ', #48158, #43868, $ ) ;
#69716 = NEXT_ASSEMBLY_USAGE_OCCURRENCE ( 'NAUO23', ' ', ' ', #48158, #43006, $ ) ;
#69717 = NEXT_ASSEMBLY_USAGE_OCCURRENCE ( 'NAUO24', ' ', ' ', #48158, #43868, $ ) ;
#69718 = NEXT_ASSEMBLY_USAGE_OCCURRENCE ( 'NAUO25', ' ', ' ', #48158, #43006, $ ) ;
#69719 = NEXT_ASSEMBLY_USAGE_OCCURRENCE ( 'NAUO26', ' ', ' ', #48158, #43868, $ ) ;
#69720 = NEXT_ASSEMBLY_USAGE_OCCURRENCE ( 'NAUO27', ' ', ' ', #48158, #52435, $ ) ;
#69721 = NEXT_ASSEMBLY_USAGE_OCCURRENCE ( 'NAUO28', ' ', ' ', #48158, #1190, $ ) ;
#69722 = NEXT_ASSEMBLY_USAGE_OCCURRENCE ( 'NAUO29', ' ', ' ', #48158, #32611, $ ) ;
ENDSEC;
END-ISO-10303-21;
